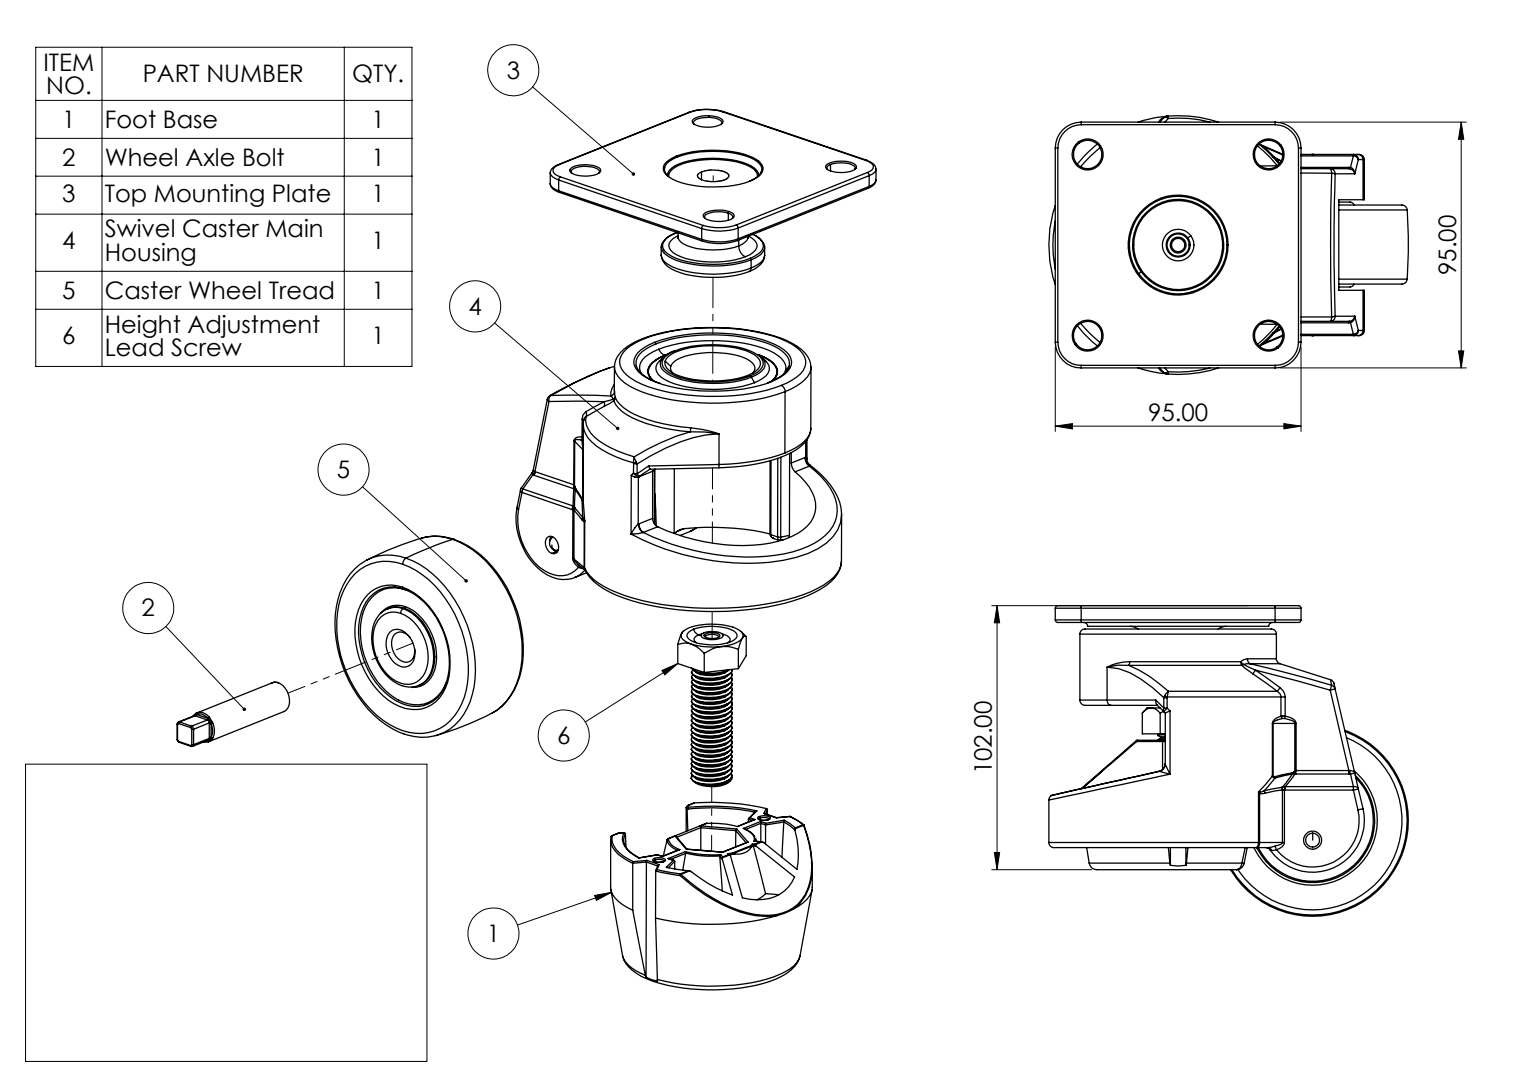
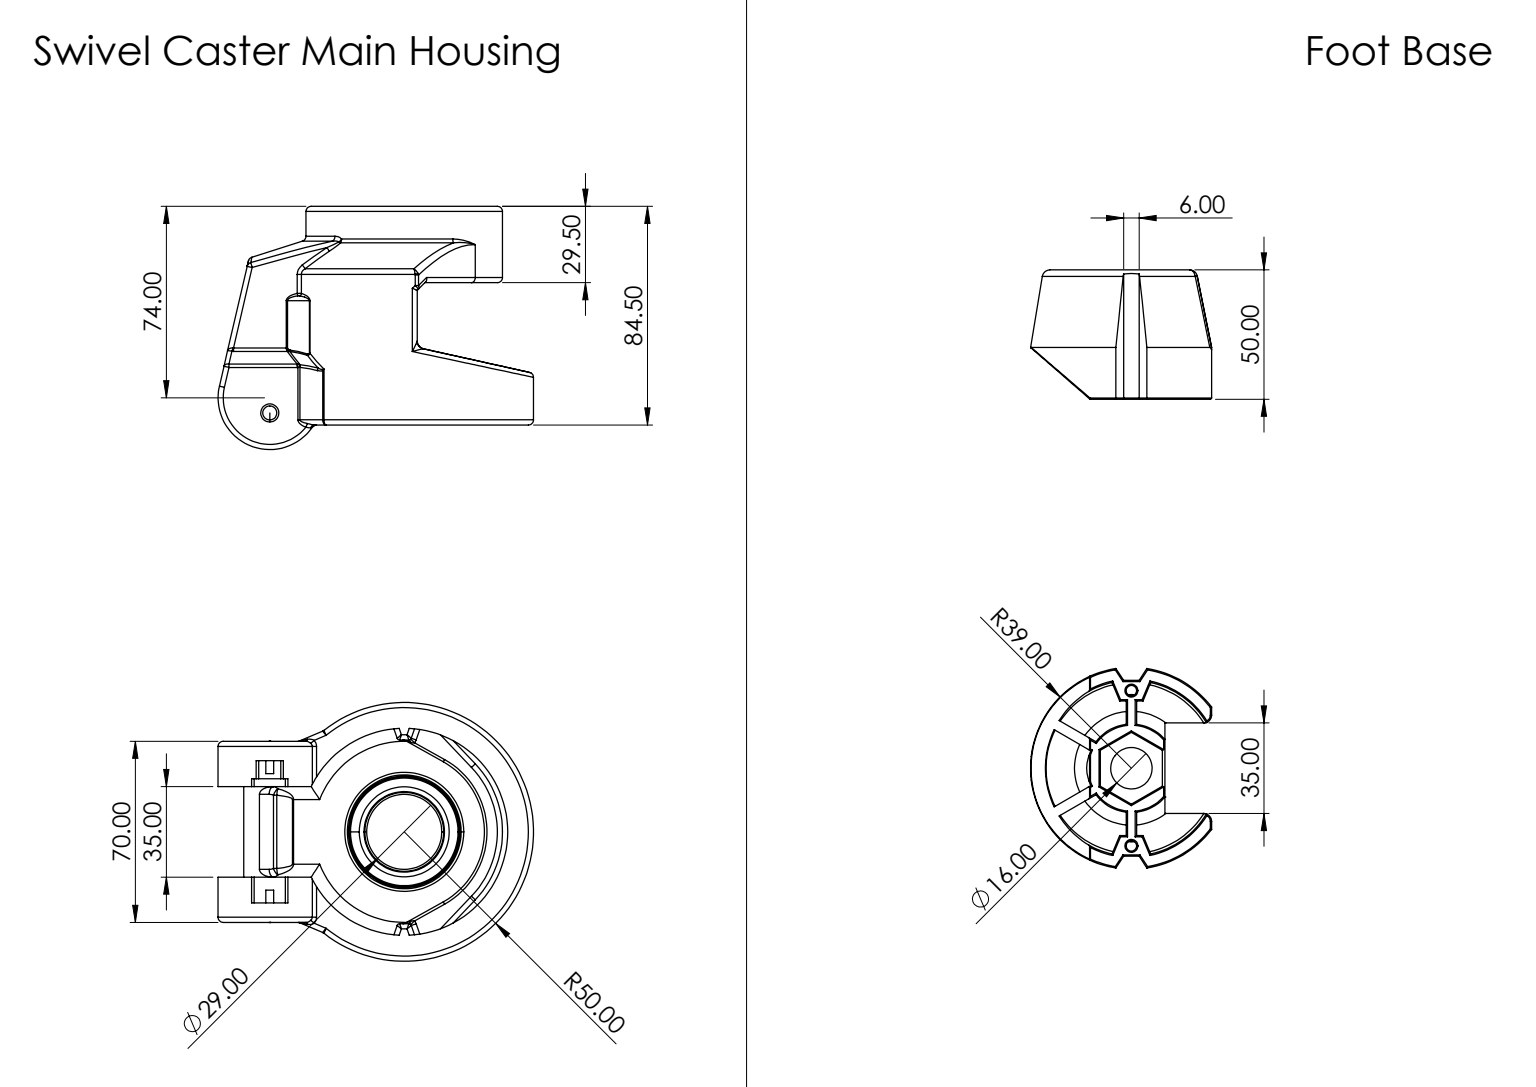
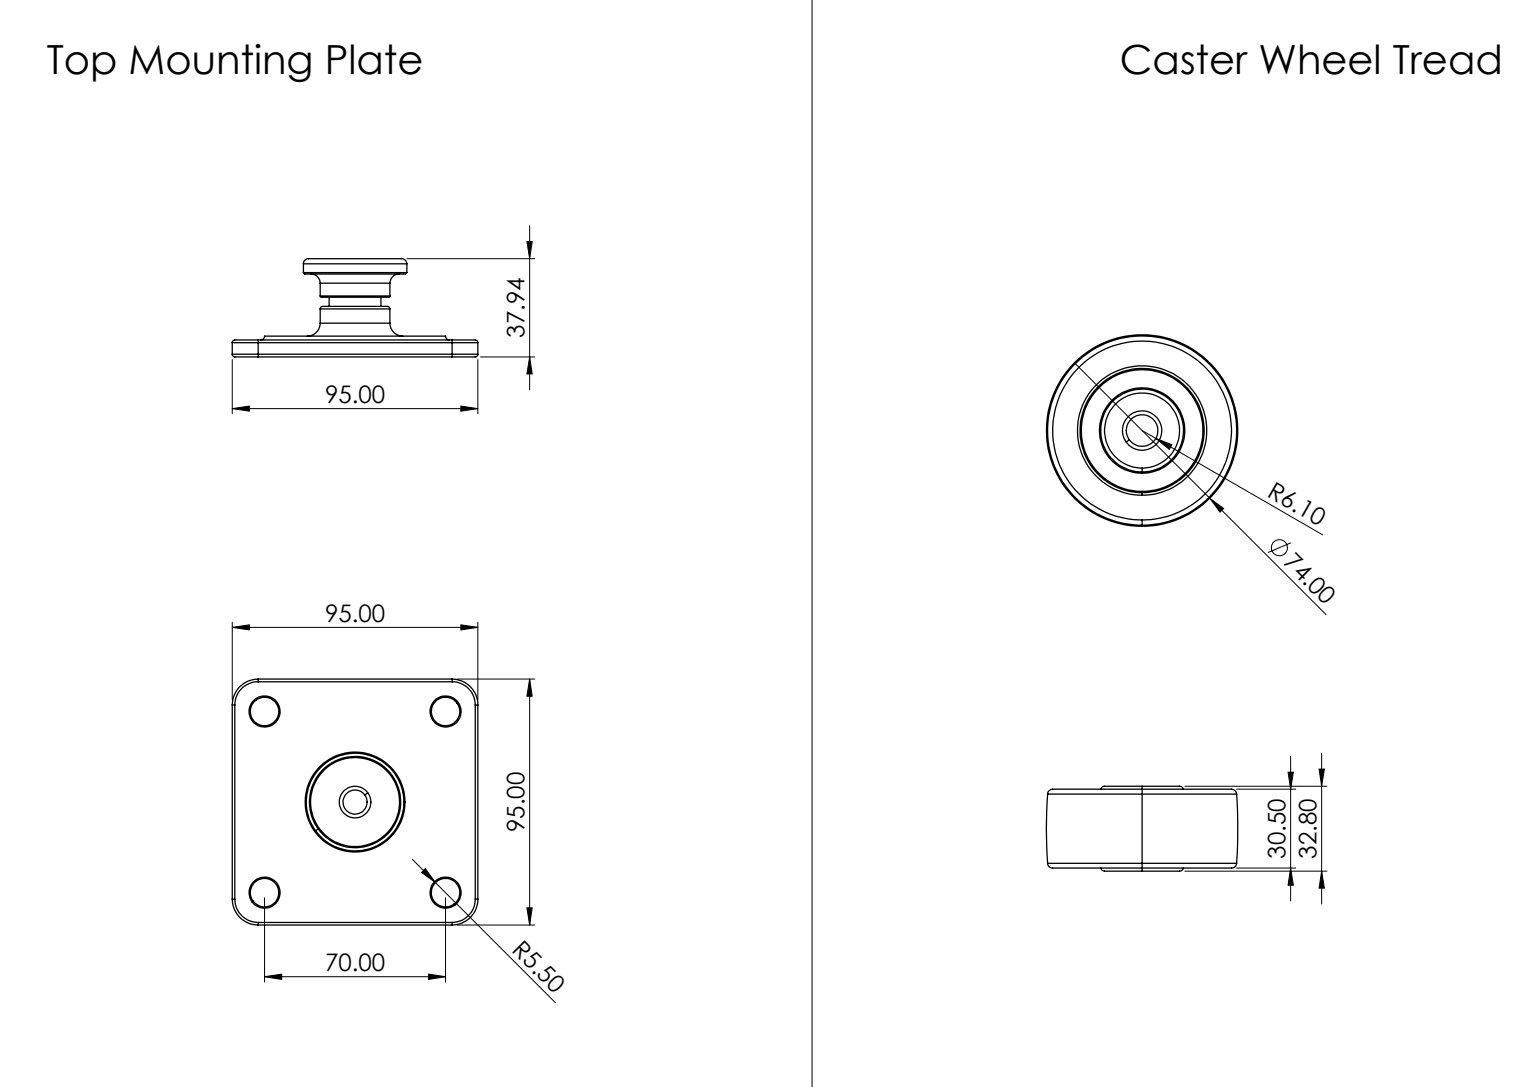
ISO-10303-21;
HEADER;
FILE_DESCRIPTION (('STEP AP214'),
    '1' );
FILE_NAME ('MAS-691',
    '2026-10-09T12:05:53',
    ( '' ),
    ( '' ),
    'SwSTEP 2.0',
    'SolidWorks 2026',
    '' );
FILE_SCHEMA (( 'AUTOMOTIVE_DESIGN' ));
ENDSEC;

DATA;
#1 = CARTESIAN_POINT ( 'NONE',  ( 24.04473007462266310, -15.61618926727986789, -75.50766188105974663 ) ) ;
#2 = CARTESIAN_POINT ( 'NONE',  ( 11.13393739769619906, -63.46281540124650178, -43.92385611378949761 ) ) ;
#3 = CARTESIAN_POINT ( 'NONE',  ( 70.83745409581372598, 17.98087126524719892, -68.79648330188406646 ) ) ;
#4 = ORIENTED_EDGE ( 'NONE', *, *, #7554, .T. ) ;
#5 = CARTESIAN_POINT ( 'NONE',  ( 23.57448381426064188, -48.85252042381474524, -34.86893418027932512 ) ) ;
#6 = CARTESIAN_POINT ( 'NONE',  ( 56.87954270074080654, 19.13328173822429790, -52.82794281668999758 ) ) ;
#7 = DIRECTION ( 'NONE',  ( 0.6933752452815363787, 0.7071067811865472397, -0.1386750490563077587 ) ) ;
#8 = CYLINDRICAL_SURFACE ( 'NONE', #48063, 2.000000000000000000 ) ;
#9 = ORIENTED_EDGE ( 'NONE', *, *, #6010, .T. ) ;
#10 = DIRECTION ( 'NONE',  ( 0.5516667872527539762, 0.8340645993220338061, 0.000000000000000000 ) ) ;
#11 = LINE ( 'NONE', #18878, #28379 ) ;
#12 = CARTESIAN_POINT ( 'NONE',  ( 9.221498779823216196, -11.63191302842313313, -56.67433499279778175 ) ) ;
#13 = CARTESIAN_POINT ( 'NONE',  ( 2.422196078461449797, -25.82482932757800143, -35.02873218748179340 ) ) ;
#14 = EDGE_CURVE ( 'NONE', #41828, #44695, #32317, .T. ) ;
#15 = CARTESIAN_POINT ( 'NONE',  ( 20.62196618598149911, -8.699519395578539260, -73.47554475576539801 ) ) ;
#16 = CYLINDRICAL_SURFACE ( 'NONE', #33863, 6.766999999999998572 ) ;
#17 = CARTESIAN_POINT ( 'NONE',  ( 46.35510799002431526, -38.18910727465775068, -58.54413787839046535 ) ) ;
#18 = SHAPE_DEFINITION_REPRESENTATION ( #45804, #4374 ) ;
#19 = VERTEX_POINT ( 'NONE', #48082 ) ;
#20 = CIRCLE ( 'NONE', #41004, 2.999999999999999112 ) ;
#21 = CIRCLE ( 'NONE', #50217, 3.400000000022779911 ) ;
#22 = CARTESIAN_POINT ( 'NONE',  ( 9.962852259819479528, -19.79044361182920042, -65.04335028194189761 ) ) ;
#23 = AXIS2_PLACEMENT_3D ( 'NONE', #28907, #44909, #49375 ) ;
#24 = CARTESIAN_POINT ( 'NONE',  ( 0.03808610503982521461, -8.381889819517736484, -34.73334895013598356 ) ) ;
#25 = CIRCLE ( 'NONE', #830, 16.00000000000000000 ) ;
#26 = CARTESIAN_POINT ( 'NONE',  ( 9.625247127302518635, -19.52582424083449908, -32.14999999999999858 ) ) ;
#27 = CARTESIAN_POINT ( 'NONE',  ( 47.24444964797500290, 23.22446773931700292, -75.11580175282739447 ) ) ;
#28 = DIRECTION ( 'NONE',  ( 0.000000000000000000, 0.000000000000000000, 1.000000000000000000 ) ) ;
#29 = CARTESIAN_POINT ( 'NONE',  ( 58.45382029077139663, 15.48193787282010092, -47.52511337483110054 ) ) ;
#30 = CARTESIAN_POINT ( 'NONE',  ( 12.20485434016749871, 33.73368687413830003, -16.27613458663830315 ) ) ;
#31 = CARTESIAN_POINT ( 'NONE',  ( 11.75558472888330108, -8.629576846066969509, -76.82947711988130379 ) ) ;
#33 = CARTESIAN_POINT ( 'NONE',  ( 11.13393739769619906, -55.30245861064819479, -43.74348518090240390 ) ) ;
#32 = DIRECTION ( 'NONE',  ( 0.05023550054956202326, 0.000000000000000000, 0.9987374001630934250 ) ) ;
#34 = CARTESIAN_POINT ( 'NONE',  ( 63.30967889250540992, 1.328674444234379859, -68.76626720283900340 ) ) ;
#35 = CARTESIAN_POINT ( 'NONE',  ( 61.45197839950609620, 13.95077426323470071, -46.74199412580669843 ) ) ;
#36 = DIRECTION ( 'NONE',  ( 0.5877852522924696954, 0.8090169943749498938, 0.000000000000000000 ) ) ;
#37 = DIRECTION ( 'NONE',  ( 0.000000000000000000, -0.7071067811865292541, 0.7071067811865656694 ) ) ;
#38 = AXIS2_PLACEMENT_3D ( 'NONE', #21905, #42103, #29767 ) ;
#39 = VERTEX_POINT ( 'NONE', #5102 ) ;
#40 = CARTESIAN_POINT ( 'NONE',  ( 52.81826494772970193, -49.66694110389089900, -48.49938242813500011 ) ) ;
#41 = CARTESIAN_POINT ( 'NONE',  ( 61.28932554653079734, -45.22069038368779559, -27.95515929525059917 ) ) ;
#42 = CARTESIAN_POINT ( 'NONE',  ( 20.99557441488136078, -21.94238693200700041, -72.08401915777523072 ) ) ;
#43 = CARTESIAN_POINT ( 'NONE',  ( 61.24946240356100446, 14.29281268270219840, -47.58806468664730005 ) ) ;
#44 = CARTESIAN_POINT ( 'NONE',  ( 22.19687809394159927, -11.28635708649630054, -78.03525497637551211 ) ) ;
#45 = CARTESIAN_POINT ( 'NONE',  ( 51.50850403090049667, 17.46583278780749993, -76.79363216376158618 ) ) ;
#46 = CARTESIAN_POINT ( 'NONE',  ( 53.43953639093020058, 18.12785922017320317, -48.94167477993919846 ) ) ;
#47 = CARTESIAN_POINT ( 'NONE',  ( 71.33582579397329937, 0.9940695285616559795, -70.71491496446259362 ) ) ;
#48 = CARTESIAN_POINT ( 'NONE',  ( -0.2431464996536397138, -45.41879842705380810, -34.97812159119441588 ) ) ;
#49 = EDGE_CURVE ( 'NONE', #3712, #26115, #46078, .T. ) ;
#50 = ORIENTED_EDGE ( 'NONE', *, *, #39346, .T. ) ;
#51 = CYLINDRICAL_SURFACE ( 'NONE', #25451, 0.9999999999999988898 ) ;
#52 = AXIS2_PLACEMENT_3D ( 'NONE', #15855, #20801, #24196 ) ;
#53 = CARTESIAN_POINT ( 'NONE',  ( 47.61264694707350031, -54.54714935536990339, -55.11842961798419793 ) ) ;
#54 = CARTESIAN_POINT ( 'NONE',  ( 22.50468263344456687, -12.72456034819510151, -68.71118389017816241 ) ) ;
#55 = CONICAL_SURFACE ( 'NONE', #5063, 44.00000000000000000, 0.8066715494215099813 ) ;
#56 = CARTESIAN_POINT ( 'NONE',  ( 10.72262792443331492, -19.77487285394900951, -71.24448753608163543 ) ) ;
#57 = CARTESIAN_POINT ( 'NONE',  ( 60.90067199252950303, -29.96820827507399798, -16.03697021813930235 ) ) ;
#58 = CARTESIAN_POINT ( 'NONE',  ( 71.48394854028050815, 1.096932441169200079, -60.71856768636379797 ) ) ;
#59 = CARTESIAN_POINT ( 'NONE',  ( 14.28038030992539476, 1.245406012443915467, -34.79644291222909658 ) ) ;
#60 = CARTESIAN_POINT ( 'NONE',  ( 72.18036885542301206, 1.274155933524790063, -61.30553710256390332 ) ) ;
#61 = AXIS2_PLACEMENT_3D ( 'NONE', #5299, #13423, #12639 ) ;
#62 = AXIS2_PLACEMENT_3D ( 'NONE', #47458, #35380, #23303 ) ;
#63 = CARTESIAN_POINT ( 'NONE',  ( 22.90087412606865058, -16.66897304226082710, -40.89671642115739303 ) ) ;
#64 = DIRECTION ( 'NONE',  ( 0.8933039976646619529, 0.3805134419105545285, 0.2392017731575520056 ) ) ;
#65 = ORIENTED_EDGE ( 'NONE', *, *, #51526, .T. ) ;
#66 = ORIENTED_EDGE ( 'NONE', *, *, #10007, .T. ) ;
#67 = LINE ( 'NONE', #19711, #13704 ) ;
#68 = CARTESIAN_POINT ( 'NONE',  ( 22.04686178097117732, -19.02415631444728561, -58.61948664697574429 ) ) ;
#69 = ORIENTED_EDGE ( 'NONE', *, *, #51815, .T. ) ;
#70 = CARTESIAN_POINT ( 'NONE',  ( 14.06316349757885042, -7.911113466102105640, -58.92429889998866344 ) ) ;
#71 = CARTESIAN_POINT ( 'NONE',  ( 55.90694558577502704, 19.65285642343416939, -74.84539568267780396 ) ) ;
#72 = ORIENTED_EDGE ( 'NONE', *, *, #36227, .F. ) ;
#73 = CARTESIAN_POINT ( 'NONE',  ( 11.04126890615173195, 33.67834000696034735, -23.14699238744169563 ) ) ;
#74 = CARTESIAN_POINT ( 'NONE',  ( 42.22422596689015251, 6.426959746402536311, -79.19854329468917342 ) ) ;
#75 = CARTESIAN_POINT ( 'NONE',  ( 23.84711268294356046, -17.41670964262949894, -65.58063247732249579 ) ) ;
#76 = EDGE_CURVE ( 'NONE', #45466, #37955, #44145, .T. ) ;
#77 = CARTESIAN_POINT ( 'NONE',  ( 21.74894416331870062, -9.578439440273777805, -43.53078881371720144 ) ) ;
#78 = CARTESIAN_POINT ( 'NONE',  ( 45.17641135619509640, 2.139553668185640412, -34.89907071124209637 ) ) ;
#79 = CARTESIAN_POINT ( 'NONE',  ( 53.63393739769619373, -53.11618894467930119, 16.35000000000000142 ) ) ;
#80 = EDGE_CURVE ( 'NONE', #28603, #19573, #33103, .T. ) ;
#81 = CARTESIAN_POINT ( 'NONE',  ( 63.96520777976849814, -30.70443757047150157, -16.53667252483340278 ) ) ;
#82 = CARTESIAN_POINT ( 'NONE',  ( 9.221484299827681141, -19.60044010530257097, -42.62566474563559638 ) ) ;
#83 = CARTESIAN_POINT ( 'NONE',  ( 9.878977750625089982, -11.56869915257929904, -35.41547006414829468 ) ) ;
#84 = CARTESIAN_POINT ( 'NONE',  ( 41.93136269540350014, 14.16859103147459997, -6.436551634680689915 ) ) ;
#85 = CARTESIAN_POINT ( 'NONE',  ( 15.05440318628110141, 21.88381105532300097, -76.14999999999999147 ) ) ;
#86 = AXIS2_PLACEMENT_3D ( 'NONE', #46178, #31434, #24593 ) ;
#87 = AXIS2_PLACEMENT_3D ( 'NONE', #9634, #13072, #16715 ) ;
#88 = CARTESIAN_POINT ( 'NONE',  ( 83.58549413295790487, -44.91149346033729728, -47.23752224019400359 ) ) ;
#89 = CARTESIAN_POINT ( 'NONE',  ( 9.633937397696209715, -15.61618894467929941, -22.64999999999999858 ) ) ;
#90 = AXIS2_PLACEMENT_3D ( 'NONE', #30342, #50541, #46365 ) ;
#91 = CARTESIAN_POINT ( 'NONE',  ( 8.278517517462621100, -18.12120375785029935, -46.40940759145149741 ) ) ;
#92 = ORIENTED_EDGE ( 'NONE', *, *, #43426, .F. ) ;
#93 = CARTESIAN_POINT ( 'NONE',  ( 54.39552376178149018, -47.99669817431590246, -26.49407277081109768 ) ) ;
#94 = CARTESIAN_POINT ( 'NONE',  ( 13.75381683890189954, -50.28652857585829850, -20.97887788433540024 ) ) ;
#95 = CARTESIAN_POINT ( 'NONE',  ( 19.30039974071021902, -22.89444622034352861, -39.87698757616706757 ) ) ;
#96 = CARTESIAN_POINT ( 'NONE',  ( 63.43393739769620510, 1.883811055320669947, -62.44999999999999574 ) ) ;
#97 = CARTESIAN_POINT ( 'NONE',  ( 22.90093739844393284, -15.61845303799943174, -56.45293168557734020 ) ) ;
#98 = DIRECTION ( 'NONE',  ( 1.681650659181820092E-11, -1.000000000000000000, -2.220771714818679968E-11 ) ) ;
#99 = ORIENTED_EDGE ( 'NONE', *, *, #38277, .T. ) ;
#100 = CARTESIAN_POINT ( 'NONE',  ( -8.352063028131979650, -44.76125978986279819, -5.675626772346689997 ) ) ;
#101 = CARTESIAN_POINT ( 'NONE',  ( 18.20467283260814639, -23.32127324669528434, -38.20900000048465017 ) ) ;
#102 = CARTESIAN_POINT ( 'NONE',  ( 52.13393739769618662, -30.49118894467929763, -65.65000000000000568 ) ) ;
#103 = CARTESIAN_POINT ( 'NONE',  ( 63.10556452593170462, 0.9234936569010840923, -62.37649816534809588 ) ) ;
#104 = CARTESIAN_POINT ( 'NONE',  ( 57.49560449525049677, -50.20980267308190292, -52.71571619239969664 ) ) ;
#105 = CARTESIAN_POINT ( 'NONE',  ( 41.47267182510199746, 13.45740503867699900, -5.287754110957130216 ) ) ;
#106 = CARTESIAN_POINT ( 'NONE',  ( 22.72481333909230017, -17.38742284364922597, -64.53615558299642885 ) ) ;
#107 = DIRECTION ( 'NONE',  ( 0.000000000000000000, 0.000000000000000000, 1.000000000000000000 ) ) ;
#108 = CARTESIAN_POINT ( 'NONE',  ( 53.43679795856239423, -49.34287432940249829, -48.83615822498679648 ) ) ;
#109 = CARTESIAN_POINT ( 'NONE',  ( 9.221334957865163773, -11.63219308205320957, -74.95902792597172493 ) ) ;
#110 = EDGE_CURVE ( 'NONE', #14338, #30215, #34341, .T. ) ;
#111 = CARTESIAN_POINT ( 'NONE',  ( 12.72590726626352975, -21.52907858405782449, -63.11948344771946040 ) ) ;
#112 = CARTESIAN_POINT ( 'NONE',  ( 17.46250221217660226, -52.82751997460400162, -76.12812327221449493 ) ) ;
#113 = LINE ( 'NONE', #8225, #22864 ) ;
#114 = CARTESIAN_POINT ( 'NONE',  ( 63.48718924516480655, 1.369286338574360107, -62.31365646596000119 ) ) ;
#115 = ORIENTED_EDGE ( 'NONE', *, *, #5512, .F. ) ;
#116 = DIRECTION ( 'NONE',  ( -0.2846079131720438693, 0.9586440088791325920, 0.000000000000000000 ) ) ;
#117 = DIRECTION ( 'NONE',  ( 0.000000000000000000, 0.000000000000000000, 1.000000000000000000 ) ) ;
#118 = CARTESIAN_POINT ( 'NONE',  ( 11.66207609259309841, -9.394545466821320190, -81.23899999999999011 ) ) ;
#119 = ORIENTED_EDGE ( 'NONE', *, *, #5990, .F. ) ;
#120 = CARTESIAN_POINT ( 'NONE',  ( 17.35323444535940141, 21.52412519331699770, -76.12563501418100032 ) ) ;
#121 = VERTEX_POINT ( 'NONE', #9296 ) ;
#122 = ORIENTED_EDGE ( 'NONE', *, *, #30558, .T. ) ;
#123 = CARTESIAN_POINT ( 'NONE',  ( 41.13393739769620083, -15.61618894467929941, -76.14999999999999147 ) ) ;
#124 = CARTESIAN_POINT ( 'NONE',  ( 23.50285504017600147, -13.84387210050659966, -81.23899999999999011 ) ) ;
#125 = AXIS2_PLACEMENT_3D ( 'NONE', #16725, #32947, #12811 ) ;
#126 = CARTESIAN_POINT ( 'NONE',  ( 61.67728155832050163, 13.96021777555640142, -46.92123163896760474 ) ) ;
#127 = ORIENTED_EDGE ( 'NONE', *, *, #25238, .T. ) ;
#128 = CARTESIAN_POINT ( 'NONE',  ( 13.00893747662790112, -65.51843693869379592, -23.32157303180050079 ) ) ;
#129 = ORIENTED_EDGE ( 'NONE', *, *, #8832, .T. ) ;
#130 = CARTESIAN_POINT ( 'NONE',  ( 11.13393741218609989, -63.52234717531779751, -24.14942545402350049 ) ) ;
#131 = EDGE_CURVE ( 'NONE', #41228, #12484, #43567, .T. ) ;
#132 = DIRECTION ( 'NONE',  ( 0.000000000000000000, 0.000000000000000000, -1.000000000000000000 ) ) ;
#133 = ORIENTED_EDGE ( 'NONE', *, *, #22274, .F. ) ;
#134 = ORIENTED_EDGE ( 'NONE', *, *, #16581, .T. ) ;
#135 = CARTESIAN_POINT ( 'NONE',  ( 68.13393739769630031, 16.88381105532069881, -71.50000000000000000 ) ) ;
#136 = CARTESIAN_POINT ( 'NONE',  ( 60.78215478534439598, 14.37029503885610104, -47.53399852477849663 ) ) ;
#137 = CARTESIAN_POINT ( 'NONE',  ( 22.18886536826886768, -12.48613193644987263, -40.30080353194567522 ) ) ;
#138 = CARTESIAN_POINT ( 'NONE',  ( 41.55663456559440050, -43.85962873145390262, -3.466044033466880059 ) ) ;
#139 = CARTESIAN_POINT ( 'NONE',  ( -7.981053360220990101, 13.77072044879260027, -5.285160133845220543 ) ) ;
#140 = DIRECTION ( 'NONE',  ( 0.000000000000000000, -1.000000000000000000, 0.000000000000000000 ) ) ;
#141 = DIRECTION ( 'NONE',  ( -1.000000000000000000, -1.007258792502662152E-15, 0.000000000000000000 ) ) ;
#142 = CARTESIAN_POINT ( 'NONE',  ( 23.87684719361660157, -16.89450661858629843, -59.33958724536129381 ) ) ;
#143 = EDGE_LOOP ( 'NONE', ( #42632, #34972, #31733, #32112, #15786, #3340, #43438, #7469 ) ) ;
#144 = CARTESIAN_POINT ( 'NONE',  ( 16.13393739769620083, -15.61618894467929941, -8.050000000000000711 ) ) ;
#145 = CARTESIAN_POINT ( 'NONE',  ( 41.69946260611190070, 14.48490530928729925, -6.580410751903029265 ) ) ;
#146 = CARTESIAN_POINT ( 'NONE',  ( 11.25398292734820060, 32.98847748127889901, -44.13762314110879714 ) ) ;
#147 = CARTESIAN_POINT ( 'NONE',  ( 72.11830705158430987, 1.407740700961940039, -69.90489258341499124 ) ) ;
#148 = CARTESIAN_POINT ( 'NONE',  ( 42.65284985753929448, -39.83221199758776976, -73.17816600590020926 ) ) ;
#149 = AXIS2_PLACEMENT_3D ( 'NONE', #32880, #41030, #5146 ) ;
#150 = AXIS2_PLACEMENT_3D ( 'NONE', #7482, #19780, #50726 ) ;
#151 = DIRECTION ( 'NONE',  ( 0.4646601886423053496, 0.000000000000000000, 0.8854890790353641128 ) ) ;
#152 = CIRCLE ( 'NONE', #47026, 15.56227766016840164 ) ;
#153 = CARTESIAN_POINT ( 'NONE',  ( 13.08915387332580060, 18.89706364897919855, -21.07935023198889724 ) ) ;
#154 = CARTESIAN_POINT ( 'NONE',  ( 47.08254214957229777, 23.29430871593149632, -75.17655545168919673 ) ) ;
#155 = CARTESIAN_POINT ( 'NONE',  ( 48.68907877926229588, -53.99330233976530025, -54.71376368574509996 ) ) ;
#156 = CARTESIAN_POINT ( 'NONE',  ( 51.77632594796870080, -32.59667852913690922, -18.40929238398544854 ) ) ;
#157 = EDGE_CURVE ( 'NONE', #32127, #27118, #5412, .T. ) ;
#158 = DIRECTION ( 'NONE',  ( -9.834501533011740460E-16, -2.054487543405499690E-16, -1.000000000000000000 ) ) ;
#159 = CARTESIAN_POINT ( 'NONE',  ( -14.41646913324137458, -47.38337005707102634, 16.85000000000000142 ) ) ;
#160 = CARTESIAN_POINT ( 'NONE',  ( 20.11809687624943521, -22.52869528883066153, -54.12566693902919468 ) ) ;
#161 = ORIENTED_EDGE ( 'NONE', *, *, #48216, .F. ) ;
#162 = CARTESIAN_POINT ( 'NONE',  ( 8.696784336233250201, -15.17409326420679960, -34.08624212660659936 ) ) ;
#163 = EDGE_CURVE ( 'NONE', #42293, #16351, #20947, .T. ) ;
#164 = CARTESIAN_POINT ( 'NONE',  ( 83.89200044194980421, -48.61618894467930119, -53.92796738110899923 ) ) ;
#165 = ORIENTED_EDGE ( 'NONE', *, *, #23269, .F. ) ;
#166 = CARTESIAN_POINT ( 'NONE',  ( 71.29447239804829906, 1.393731187554809958, -70.25064478522961053 ) ) ;
#167 = CARTESIAN_POINT ( 'NONE',  ( 60.57174147421439869, -45.61905813271650345, -47.32280480079099760 ) ) ;
#168 = CARTESIAN_POINT ( 'NONE',  ( 42.18478254462388577, 8.551920610105096188, -75.43933843070429646 ) ) ;
#169 = EDGE_CURVE ( 'NONE', #3359, #16152, #45412, .T. ) ;
#170 = CARTESIAN_POINT ( 'NONE',  ( 29.13393739769619728, 4.555383930574479656, -84.63196841427449613 ) ) ;
#171 = DIRECTION ( 'NONE',  ( 8.402539340422011355E-12, -1.000000000000000000, -1.365304166073849981E-11 ) ) ;
#172 = ORIENTED_EDGE ( 'NONE', *, *, #12898, .T. ) ;
#173 = CARTESIAN_POINT ( 'NONE',  ( 82.86439673227779679, -45.43596139653639909, -47.48719404937710209 ) ) ;
#174 = ORIENTED_EDGE ( 'NONE', *, *, #31789, .F. ) ;
#175 = ORIENTED_EDGE ( 'NONE', *, *, #21315, .T. ) ;
#176 = ORIENTED_EDGE ( 'NONE', *, *, #14775, .F. ) ;
#177 = LINE ( 'NONE', #11984, #16918 ) ;
#178 = CARTESIAN_POINT ( 'NONE',  ( 12.13393739769500357, -55.41568642894398522, -22.88367089793594999 ) ) ;
#179 = CARTESIAN_POINT ( 'NONE',  ( 76.39443566142985276, -13.50186642808351678, -12.77252636400736918 ) ) ;
#180 = CARTESIAN_POINT ( 'NONE',  ( 53.40601104668340326, -52.07939714610260040, -54.18165646226010068 ) ) ;
#181 = EDGE_LOOP ( 'NONE', ( #10169, #38470, #47423, #39238 ) ) ;
#182 = ORIENTED_EDGE ( 'NONE', *, *, #38895, .T. ) ;
#183 = CARTESIAN_POINT ( 'NONE',  ( 18.20454837585587526, -23.32130853119455693, -55.92427167932272170 ) ) ;
#184 = CARTESIAN_POINT ( 'NONE',  ( 57.10566319413430136, -45.15673104066610222, -25.30628267469290194 ) ) ;
#185 = CARTESIAN_POINT ( 'NONE',  ( 56.36581729833090293, -50.64752597117900024, -53.07181749496119494 ) ) ;
#186 = DIRECTION ( 'NONE',  ( 0.000000000000000000, 1.000000000000000000, 0.000000000000000000 ) ) ;
#187 = CARTESIAN_POINT ( 'NONE',  ( 58.91901068275170417, -2.751350989218700249, -15.64940685286009980 ) ) ;
#188 = EDGE_CURVE ( 'NONE', #6898, #18473, #14502, .T. ) ;
#189 = CARTESIAN_POINT ( 'NONE',  ( 9.367050196127319595, -15.61601677469269944, -55.84717978380999881 ) ) ;
#190 = AXIS2_PLACEMENT_3D ( 'NONE', #21830, #26535, #49643 ) ;
#191 = ORIENTED_EDGE ( 'NONE', *, *, #12053, .T. ) ;
#192 = CARTESIAN_POINT ( 'NONE',  ( 64.43393739769619799, 11.38381105532079829, -62.44999999999999574 ) ) ;
#194 = CARTESIAN_POINT ( 'NONE',  ( 53.11717557676140444, -50.37380613066250135, -77.21703359256949284 ) ) ;
#193 = AXIS2_PLACEMENT_3D ( 'NONE', #44707, #32884, #28448 ) ;
#195 = CARTESIAN_POINT ( 'NONE',  ( 60.26025110216912850, 14.55536647234954906, -47.43140372362420010 ) ) ;
#196 = CARTESIAN_POINT ( 'NONE',  ( 12.16981617636240109, -50.04926268091029584, -21.14999999999999858 ) ) ;
#197 = CARTESIAN_POINT ( 'NONE',  ( 18.24071347613679706, -23.17583458100989802, -56.42598068654729104 ) ) ;
#198 = CARTESIAN_POINT ( 'NONE',  ( 13.05744206701320209, -50.32199602849929931, -21.18087822640150364 ) ) ;
#199 = CARTESIAN_POINT ( 'NONE',  ( 18.48744068327825829, -51.29015062620795362, -15.70679445625363257 ) ) ;
#200 = CARTESIAN_POINT ( 'NONE',  ( 10.91611746120075743, -65.09563545678379626, -18.17421237897874065 ) ) ;
#201 = CARTESIAN_POINT ( 'NONE',  ( 61.22433221214529908, -45.66722181782489542, -47.75777089857670177 ) ) ;
#202 = CARTESIAN_POINT ( 'NONE',  ( 68.13393739769618662, -1.166188944679350081, -90.65000000000000568 ) ) ;
#203 = EDGE_CURVE ( 'NONE', #41459, #2348, #29936, .T. ) ;
#204 = CARTESIAN_POINT ( 'NONE',  ( 12.63580666350229897, -21.74037383255939915, -53.51237412773319591 ) ) ;
#205 = ORIENTED_EDGE ( 'NONE', *, *, #35909, .F. ) ;
#206 = CARTESIAN_POINT ( 'NONE',  ( 14.27557618103930004, -51.11617952483079108, -74.35192203308750436 ) ) ;
#207 = CARTESIAN_POINT ( 'NONE',  ( 47.38398407523909839, -54.66303005604620324, -54.71474001952109489 ) ) ;
#208 = DIRECTION ( 'NONE',  ( 1.000000000000000000, 0.000000000000000000, 0.000000000000000000 ) ) ;
#209 = CARTESIAN_POINT ( 'NONE',  ( 9.807775352051226747, -10.75450683567505550, -36.71600244428209692 ) ) ;
#210 = CARTESIAN_POINT ( 'NONE',  ( 14.48969159609045931, -51.52597369351618539, -75.36997958377637019 ) ) ;
#211 = CARTESIAN_POINT ( 'NONE',  ( 24.04447781939626338, -15.52406317847051120, -55.50396621545129250 ) ) ;
#212 = CARTESIAN_POINT ( 'NONE',  ( 10.72251451727398397, -11.45765055134171284, -75.66113898378057456 ) ) ;
#213 = CARTESIAN_POINT ( 'NONE',  ( 14.63393739769620083, -23.61618894467940066, -35.14999999999999858 ) ) ;
#215 = CARTESIAN_POINT ( 'NONE',  ( 11.13393739769619906, 32.28996931002959769, -24.14942631645369886 ) ) ;
#214 = CARTESIAN_POINT ( 'NONE',  ( 0.5774960717374295616, -8.799493537124943643, -34.81767276520690757 ) ) ;
#216 = DIRECTION ( 'NONE',  ( 1.000000000000000000, 1.435277183835595142E-25, -2.812429781167509836E-09 ) ) ;
#217 = CARTESIAN_POINT ( 'NONE',  ( 48.63544209855220402, 22.87909972998859587, -55.27856191273439634 ) ) ;
#218 = VERTEX_POINT ( 'NONE', #20999 ) ;
#219 = AXIS2_PLACEMENT_3D ( 'NONE', #32252, #16823, #17087 ) ;
#220 = CARTESIAN_POINT ( 'NONE',  ( 53.03258586660929552, -49.57550701127339465, -48.98438927054080239 ) ) ;
#221 = VECTOR ( 'NONE', #20603, 1000.000000000000000 ) ;
#222 = ORIENTED_EDGE ( 'NONE', *, *, #47182, .T. ) ;
#223 = CARTESIAN_POINT ( 'NONE',  ( 45.74232523797041239, 6.648894618224240105, -61.55666661952047036 ) ) ;
#224 = LINE ( 'NONE', #43991, #1797 ) ;
#225 = CARTESIAN_POINT ( 'NONE',  ( 16.13393739769620083, -15.61618894467929941, -10.44999999999999929 ) ) ;
#227 = CARTESIAN_POINT ( 'NONE',  ( 55.09561028961779527, 15.74612775871969994, -25.81326377834329833 ) ) ;
#226 = CARTESIAN_POINT ( 'NONE',  ( 84.44784216359251161, 11.88381105532070059, -47.47585302082339354 ) ) ;
#228 = CARTESIAN_POINT ( 'NONE',  ( 18.41697451332290214, -22.28929168817850126, -66.84789180586540169 ) ) ;
#230 = EDGE_CURVE ( 'NONE', #16151, #14500, #48277, .T. ) ;
#229 = CARTESIAN_POINT ( 'NONE',  ( 52.88388581274700329, 18.44024018630440409, -49.00306432449180249 ) ) ;
#231 = CARTESIAN_POINT ( 'NONE',  ( 57.24436304063220149, -45.12772278369259737, -17.93020339716479938 ) ) ;
#232 = CARTESIAN_POINT ( 'NONE',  ( 15.82997274078853067, -51.11618894467930119, -21.91305730704813115 ) ) ;
#233 = ORIENTED_EDGE ( 'NONE', *, *, #50630, .F. ) ;
#234 = CARTESIAN_POINT ( 'NONE',  ( 15.51400525636760008, -23.43938728828090134, -43.81267675689189645 ) ) ;
#235 = VERTEX_POINT ( 'NONE', #24656 ) ;
#236 = CARTESIAN_POINT ( 'NONE',  ( 11.16919192711069897, -65.09379547448669712, -17.21576935268850050 ) ) ;
#237 = CARTESIAN_POINT ( 'NONE',  ( 12.92951305397479977, 34.28108550583429803, -47.71245015580439741 ) ) ;
#238 = DIRECTION ( 'NONE',  ( 0.000000000000000000, 1.000000000000000000, 0.000000000000000000 ) ) ;
#239 = CARTESIAN_POINT ( 'NONE',  ( 48.15382033460080180, -54.02300406733139937, -53.72956514560460306 ) ) ;
#240 = CARTESIAN_POINT ( 'NONE',  ( 8.799473741179280495, 31.95986279266500318, -46.67015979934819825 ) ) ;
#241 = CARTESIAN_POINT ( 'NONE',  ( -0.007164427059776000244, -10.48291004383190028, -34.77269723891829756 ) ) ;
#242 = EDGE_LOOP ( 'NONE', ( #21413, #44958, #1944, #11021, #47868 ) ) ;
#243 = CARTESIAN_POINT ( 'NONE',  ( 24.04493741881096014, -14.58063984321919015, -75.46599062978197026 ) ) ;
#244 = CARTESIAN_POINT ( 'NONE',  ( -18.86606260230360022, -50.61618894467959962, 17.35000000000000142 ) ) ;
#245 = AXIS2_PLACEMENT_3D ( 'NONE', #20946, #48226, #25130 ) ;
#246 = CARTESIAN_POINT ( 'NONE',  ( 70.83745409581388230, 17.98087126524299606, -74.20351669811765305 ) ) ;
#247 = ORIENTED_EDGE ( 'NONE', *, *, #26711, .F. ) ;
#248 = CARTESIAN_POINT ( 'NONE',  ( 24.04493739085331683, -15.62301657200399418, -43.79259974408412859 ) ) ;
#249 = CARTESIAN_POINT ( 'NONE',  ( 50.13210307247129549, -48.90653279581949420, -76.14999999999999147 ) ) ;
#250 = CARTESIAN_POINT ( 'NONE',  ( 22.88637251419359941, -11.47525136018554370, -49.33255534741104498 ) ) ;
#251 =( BOUNDED_CURVE ( )  B_SPLINE_CURVE ( 3, ( #35430, #43565, #7666, #27816 ),
 .UNSPECIFIED., .F., .T. ) 
 B_SPLINE_CURVE_WITH_KNOTS ( ( 4, 4 ),
 ( 2.356194490192377700, 3.141592653589793116 ),
 .UNSPECIFIED. ) 
 CURVE ( )  GEOMETRIC_REPRESENTATION_ITEM ( )  RATIONAL_B_SPLINE_CURVE ( ( 1.000000000000000000, 0.9492530216741954519, 0.9492530216741954519, 1.000000000000000000 ) ) 
 REPRESENTATION_ITEM ( '' )  );
#252 = ORIENTED_EDGE ( 'NONE', *, *, #43387, .T. ) ;
#253 = CARTESIAN_POINT ( 'NONE',  ( 23.83903514183533190, -17.68687693202930333, -35.59099905439017419 ) ) ;
#254 = LINE ( 'NONE', #44274, #11685 ) ;
#255 = DIRECTION ( 'NONE',  ( 0.000000000000000000, 0.000000000000000000, -1.000000000000000000 ) ) ;
#256 = CARTESIAN_POINT ( 'NONE',  ( 22.51916824768339609, -10.39972011525970075, -71.57429041023848981 ) ) ;
#257 = CARTESIAN_POINT ( 'NONE',  ( 10.37119768687602317, -55.19981235010300935, -21.14999999999890079 ) ) ;
#258 = DIRECTION ( 'NONE',  ( 0.000000000000000000, 0.000000000000000000, -1.000000000000000000 ) ) ;
#259 = SHAPE_DEFINITION_REPRESENTATION ( #50860, #49550 ) ;
#260 = VERTEX_POINT ( 'NONE', #568 ) ;
#261 = VECTOR ( 'NONE', #32679, 1000.000000000000000 ) ;
#262 = CARTESIAN_POINT ( 'NONE',  ( 13.95200227718980024, -8.492576593136959673, -69.63804828363188903 ) ) ;
#263 = AXIS2_PLACEMENT_3D ( 'NONE', #1040, #23378, #35460 ) ;
#264 = CARTESIAN_POINT ( 'NONE',  ( 52.69422391758440227, -49.76824816101610338, -48.79572285777990004 ) ) ;
#265 = EDGE_CURVE ( 'NONE', #15142, #11807, #37468, .T. ) ;
#266 = DIRECTION ( 'NONE',  ( 0.000000000000000000, -1.000000000000000000, 0.000000000000000000 ) ) ;
#267 = DIRECTION ( 'NONE',  ( -0.04332574401194498603, 0.02501412996813599451, 0.9987478026047158508 ) ) ;
#268 = EDGE_CURVE ( 'NONE', #31144, #33328, #44340, .T. ) ;
#269 = CARTESIAN_POINT ( 'NONE',  ( 47.30322462833210295, 23.47865774688779794, -74.36100594765079563 ) ) ;
#270 = CARTESIAN_POINT ( 'NONE',  ( 71.19761362482960010, 1.388189907116970101, -61.01613942410280345 ) ) ;
#271 = EDGE_CURVE ( 'NONE', #20377, #35517, #9367, .T. ) ;
#272 = CARTESIAN_POINT ( 'NONE',  ( 59.65718820948480783, 14.85145970413650041, -47.32570903220330649 ) ) ;
#273 = CARTESIAN_POINT ( 'NONE',  ( 12.23212070002750096, 33.47637228114889751, -15.94047990888659783 ) ) ;
#274 = CARTESIAN_POINT ( 'NONE',  ( 23.75374426366189695, -12.46638513581170038, -69.38289759990109928 ) ) ;
#275 = AXIS2_PLACEMENT_3D ( 'NONE', #225, #8098, #24041 ) ;
#276 = CARTESIAN_POINT ( 'NONE',  ( 54.17120420068020081, -50.61618894747770270, -77.01278694698871163 ) ) ;
#278 = DIRECTION ( 'NONE',  ( 0.000000000000000000, 0.000000000000000000, -1.000000000000000000 ) ) ;
#277 = CARTESIAN_POINT ( 'NONE',  ( 16.13393739769620083, -15.61618894467929941, -28.45282021618999835 ) ) ;
#279 = CARTESIAN_POINT ( 'NONE',  ( 63.07039345372018602, 1.099973129953850215, -68.78515728267289830 ) ) ;
#280 = CARTESIAN_POINT ( 'NONE',  ( 61.31292087637410049, 14.04174110780009954, -47.04181882197700304 ) ) ;
#281 = CARTESIAN_POINT ( 'NONE',  ( 12.14986981628316620, -8.703629658544938863, -78.84100245546133579 ) ) ;
#282 = CARTESIAN_POINT ( 'NONE',  ( 2.558369240368460140, -6.046280207075140467, -34.64999999999999858 ) ) ;
#283 = ORIENTED_EDGE ( 'NONE', *, *, #13602, .F. ) ;
#284 = CARTESIAN_POINT ( 'NONE',  ( 52.85589391196879916, -49.64722623523429945, -48.63421165633150167 ) ) ;
#285 = CARTESIAN_POINT ( 'NONE',  ( 61.33763625571969413, -45.19708596712810333, -27.94521875216469908 ) ) ;
#286 = DIRECTION ( 'NONE',  ( 1.000000000000000000, 0.000000000000000000, -1.224646799147353207E-16 ) ) ;
#287 = CARTESIAN_POINT ( 'NONE',  ( 56.26879455738869495, 14.75277753040210094, -26.06397138246319756 ) ) ;
#288 = CARTESIAN_POINT ( 'NONE',  ( 10.21452801543910027, -20.14026745531459994, -75.02493559595789918 ) ) ;
#289 = CARTESIAN_POINT ( 'NONE',  ( 50.28917926387119763, 18.40713679194410091, -76.14999999999999147 ) ) ;
#291 = EDGE_CURVE ( 'NONE', #43185, #32513, #25957, .T. ) ;
#290 = CARTESIAN_POINT ( 'NONE',  ( 52.72266114154869854, 18.49315592538880182, -48.47378032971769812 ) ) ;
#292 = CARTESIAN_POINT ( 'NONE',  ( 71.23944111523938716, 1.270877794983130027, -70.57718306158270138 ) ) ;
#293 = CARTESIAN_POINT ( 'NONE',  ( 16.13393739769620083, -15.61618894467929941, -34.64999999999999858 ) ) ;
#294 = ORIENTED_EDGE ( 'NONE', *, *, #6376, .T. ) ;
#295 = AXIS2_PLACEMENT_3D ( 'NONE', #26378, #18789, #37943 ) ;
#296 = DIRECTION ( 'NONE',  ( 0.000000000000000000, 0.000000000000000000, 1.000000000000000000 ) ) ;
#297 = AXIS2_PLACEMENT_3D ( 'NONE', #33472, #4412, #32417 ) ;
#298 = CARTESIAN_POINT ( 'NONE',  ( 47.55572014686639903, -54.56393835125380321, -54.83404589176390687 ) ) ;
#299 = CARTESIAN_POINT ( 'NONE',  ( 0.4047412638265869833, -22.38804348994680282, -35.14999999999999858 ) ) ;
#300 = CARTESIAN_POINT ( 'NONE',  ( 33.83393739769619657, -15.61618894467939711, -6.649999999999999467 ) ) ;
#301 = CARTESIAN_POINT ( 'NONE',  ( 59.27112701105020420, 16.84091543466239926, -50.37593205019099685 ) ) ;
#302 = CARTESIAN_POINT ( 'NONE',  ( 71.36299175555980412, 1.264791438333819906, -60.78603624114159487 ) ) ;
#303 = CYLINDRICAL_SURFACE ( 'NONE', #11626, 0.9999999999999988898 ) ;
#304 = AXIS2_PLACEMENT_3D ( 'NONE', #29304, #41620, #1792 ) ;
#305 = CARTESIAN_POINT ( 'NONE',  ( 72.21022460378770802, 1.195685806282509978, -61.28382422308500566 ) ) ;
#306 = LINE ( 'NONE', #33028, #47756 ) ;
#307 = CARTESIAN_POINT ( 'NONE',  ( 64.99878011502339348, 1.099973129953850215, -70.71354394397609155 ) ) ;
#308 = ORIENTED_EDGE ( 'NONE', *, *, #24146, .F. ) ;
#309 = VERTEX_POINT ( 'NONE', #6067 ) ;
#310 = DIRECTION ( 'NONE',  ( 1.224645063448482957E-16, 1.000000000000000000, -1.376914871200490233E-11 ) ) ;
#311 = CARTESIAN_POINT ( 'NONE',  ( 22.90093739248998972, -16.50198092149558349, -58.49448661159359375 ) ) ;
#312 = ORIENTED_EDGE ( 'NONE', *, *, #15491, .T. ) ;
#313 = CARTESIAN_POINT ( 'NONE',  ( 56.04842253378700434, -45.73510956910900660, -25.30965062049470049 ) ) ;
#314 = CARTESIAN_POINT ( 'NONE',  ( 54.83367525942058052, 19.86242937399058306, -75.27593038797637348 ) ) ;
#315 = ORIENTED_EDGE ( 'NONE', *, *, #51572, .T. ) ;
#316 = CYLINDRICAL_SURFACE ( 'NONE', #61, 1.000000000000000888 ) ;
#317 = CARTESIAN_POINT ( 'NONE',  ( 10.20899662427918564, -12.23061640146900686, -71.61833297012245225 ) ) ;
#318 = CARTESIAN_POINT ( 'NONE',  ( 23.83903770539513900, -13.54551362709085538, -35.42433238772350279 ) ) ;
#319 = CARTESIAN_POINT ( 'NONE',  ( 17.19215044318390184, -7.439214858484909598, -47.33329750477089704 ) ) ;
#320 = CIRCLE ( 'NONE', #22077, 7.910999999999997812 ) ;
#321 = CARTESIAN_POINT ( 'NONE',  ( 8.428846698934018278, -17.68690243860981681, -68.42433492461131550 ) ) ;
#322 = CARTESIAN_POINT ( 'NONE',  ( 42.10929425512229329, -37.64097509248548334, -79.77316519949246754 ) ) ;
#323 = SHAPE_REPRESENTATION_RELATIONSHIP ( 'NONE' , 'NONE' ,  #19070, #24050 ) ;
#324 = ORIENTED_EDGE ( 'NONE', *, *, #5080, .T. ) ;
#325 = CARTESIAN_POINT ( 'NONE',  ( 11.84646636965089961, -64.37535564892330342, -24.61798141452300115 ) ) ;
#326 = CARTESIAN_POINT ( 'NONE',  ( 21.51457940895319965, -10.46299709236900100, -33.98952930500309577 ) ) ;
#327 = CARTESIAN_POINT ( 'NONE',  ( 41.50829725104460266, 14.07267842887970133, -6.113795638072149430 ) ) ;
#328 = EDGE_CURVE ( 'NONE', #9603, #32428, #39376, .T. ) ;
#329 = CARTESIAN_POINT ( 'NONE',  ( 14.89540806449589994, 21.53776777092619810, -76.12726769927830617 ) ) ;
#330 = EDGE_CURVE ( 'NONE', #24503, #9584, #50468, .T. ) ;
#331 = VECTOR ( 'NONE', #5456, 1000.000000000000227 ) ;
#332 = CARTESIAN_POINT ( 'NONE',  ( 52.15297977881749603, 18.44951849047100367, -77.15976221510139510 ) ) ;
#333 = CARTESIAN_POINT ( 'NONE',  ( 83.78435757737699419, -44.62302606491700629, -47.11582429421620333 ) ) ;
#334 = DIRECTION ( 'NONE',  ( 1.000000000000000000, 0.000000000000000000, 0.000000000000000000 ) ) ;
#335 = CARTESIAN_POINT ( 'NONE',  ( 8.883252294883678957, -19.54178268943019958, -44.34971538379739542 ) ) ;
#336 = VERTEX_POINT ( 'NONE', #49836 ) ;
#337 = CARTESIAN_POINT ( 'NONE',  ( 53.32987016954000126, -49.16639059516919730, -27.25060986079260061 ) ) ;
#338 = CARTESIAN_POINT ( 'NONE',  ( 12.47078628662380062, -64.90377506766920135, -16.09719858678619886 ) ) ;
#339 = FACE_OUTER_BOUND ( 'NONE', #8165, .T. ) ;
#340 = CARTESIAN_POINT ( 'NONE',  ( 2.633937397696199501, -15.61618894467929763, -1.149999999999999911 ) ) ;
#341 = CARTESIAN_POINT ( 'NONE',  ( 68.13393739769620083, -33.11618894467940066, -65.65000000000000568 ) ) ;
#342 = ORIENTED_EDGE ( 'NONE', *, *, #163, .T. ) ;
#343 = CARTESIAN_POINT ( 'NONE',  ( -5.211271184535770651, -47.35087631705189892, -5.409249467409000367 ) ) ;
#344 = CARTESIAN_POINT ( 'NONE',  ( 47.43699537176610193, 23.38932764359389793, -54.65593435207329520 ) ) ;
#345 = CARTESIAN_POINT ( 'NONE',  ( 21.54530417723247737, -19.77479742635252080, -48.66115513169237516 ) ) ;
#346 = CARTESIAN_POINT ( 'NONE',  ( 63.44018392888030178, 1.383811055320669947, -62.77287342953649585 ) ) ;
#347 = CARTESIAN_POINT ( 'NONE',  ( 12.80406157968140057, 19.41979416798140079, -21.33287590401240053 ) ) ;
#348 = PLANE ( 'NONE',  #1400 ) ;
#349 = CARTESIAN_POINT ( 'NONE',  ( 42.00047115798010111, 12.65453701896299954, -4.514521080317789981 ) ) ;
#350 = DIRECTION ( 'NONE',  ( 1.000000000000000000, 2.460964292799963328E-14, 0.000000000000000000 ) ) ;
#352 = EDGE_CURVE ( 'NONE', #42477, #4597, #41871, .T. ) ;
#351 = CARTESIAN_POINT ( 'NONE',  ( 18.13393739769620083, -41.61618894467930119, -54.64999999999999858 ) ) ;
#353 = CARTESIAN_POINT ( 'NONE',  ( 16.13393739769620083, -15.61618894467929941, -22.14999999999999858 ) ) ;
#354 = CARTESIAN_POINT ( 'NONE',  ( 58.37494088879699206, -46.85178433881189619, -47.96570233379380710 ) ) ;
#355 = CYLINDRICAL_SURFACE ( 'NONE', #16437, 7.910999999999997812 ) ;
#356 = AXIS2_PLACEMENT_3D ( 'NONE', #1615, #5303, #5043 ) ;
#357 = CARTESIAN_POINT ( 'NONE',  ( 65.02936113742819657, 1.390208944942409985, -61.02997314496759884 ) ) ;
#358 = CARTESIAN_POINT ( 'NONE',  ( 17.66259199974900085, -52.33797002293529488, -75.98739629952659413 ) ) ;
#359 = EDGE_CURVE ( 'NONE', #15227, #17198, #33478, .T. ) ;
#360 = CARTESIAN_POINT ( 'NONE',  ( 22.46012642958591599, -10.75454366414201246, -73.29933459694514397 ) ) ;
#361 = CARTESIAN_POINT ( 'NONE',  ( 63.57044994947320760, 1.402336724397559964, -62.38137791222469986 ) ) ;
#362 = VERTEX_POINT ( 'NONE', #30409 ) ;
#363 = FACE_OUTER_BOUND ( 'NONE', #31062, .T. ) ;
#364 = CARTESIAN_POINT ( 'NONE',  ( 8.803701492139829554, 31.98286322187070141, -46.67019247816079286 ) ) ;
#365 = CARTESIAN_POINT ( 'NONE',  ( 22.90093635944459649, -15.62053987609991701, -34.45302314068787553 ) ) ;
#366 = CARTESIAN_POINT ( 'NONE',  ( 11.41959527949359909, -9.607686208987979981, -81.23899999999999011 ) ) ;
#367 = VERTEX_POINT ( 'NONE', #1612 ) ;
#368 = CARTESIAN_POINT ( 'NONE',  ( 18.39143759339100015, 20.51618323985760028, -75.32473453343510528 ) ) ;
#369 = ORIENTED_EDGE ( 'NONE', *, *, #42644, .T. ) ;
#370 = ORIENTED_EDGE ( 'NONE', *, *, #29740, .F. ) ;
#371 = VERTEX_POINT ( 'NONE', #34078 ) ;
#372 = FACE_OUTER_BOUND ( 'NONE', #24038, .T. ) ;
#373 = FACE_OUTER_BOUND ( 'NONE', #2514, .T. ) ;
#374 = CARTESIAN_POINT ( 'NONE',  ( 9.807832152388833435, -10.75443395529458535, -62.71600216802090699 ) ) ;
#375 = CARTESIAN_POINT ( 'NONE',  ( 61.73752130501190294, 13.89709510481169907, -46.60858937970350269 ) ) ;
#376 = ORIENTED_EDGE ( 'NONE', *, *, #2345, .F. ) ;
#377 = CARTESIAN_POINT ( 'NONE',  ( 75.37149648727124429, 8.404366805738446189, -12.88285088340076712 ) ) ;
#378 = CARTESIAN_POINT ( 'NONE',  ( 11.93174526809839975, 34.20691394249479345, -17.93019253464870033 ) ) ;
#379 = ORIENTED_EDGE ( 'NONE', *, *, #9836, .T. ) ;
#380 = CARTESIAN_POINT ( 'NONE',  ( 11.18157709302775693, -63.96091097623292399, -24.11720355368492008 ) ) ;
#381 = LINE ( 'NONE', #40735, #27640 ) ;
#382 = ORIENTED_EDGE ( 'NONE', *, *, #47664, .T. ) ;
#383 = ORIENTED_EDGE ( 'NONE', *, *, #15032, .F. ) ;
#384 = DIRECTION ( 'NONE',  ( 0.000000000000000000, -1.000000000000000000, 0.000000000000000000 ) ) ;
#385 = CYLINDRICAL_SURFACE ( 'NONE', #20080, 0.4999999999999984457 ) ;
#386 = CARTESIAN_POINT ( 'NONE',  ( 60.90370348410529999, 14.44994567453569978, -47.72079593689969812 ) ) ;
#387 = CARTESIAN_POINT ( 'NONE',  ( 50.95711422415039493, 14.35971216196159794, -12.63805038270279901 ) ) ;
#388 = AXIS2_PLACEMENT_3D ( 'NONE', #14443, #6852, #15224 ) ;
#389 = EDGE_CURVE ( 'NONE', #27054, #15604, #37779, .T. ) ;
#390 = CARTESIAN_POINT ( 'NONE',  ( 14.34417029198830029, 20.88381105532299742, -21.14999999999999858 ) ) ;
#391 = CARTESIAN_POINT ( 'NONE',  ( -10.44638207467119884, 11.54816621806459942, -6.014155644910160525 ) ) ;
#392 = CARTESIAN_POINT ( 'NONE',  ( 38.67452568954060155, -15.61618894467929941, -81.65000000000000568 ) ) ;
#393 = CARTESIAN_POINT ( 'NONE',  ( 57.33093049919349937, 14.58258304156659868, -26.26999088063260146 ) ) ;
#394 = CARTESIAN_POINT ( 'NONE',  ( 10.01583490929099973, -20.53102059231009946, -58.07208434834350186 ) ) ;
#395 = ORIENTED_EDGE ( 'NONE', *, *, #27626, .F. ) ;
#396 = DIRECTION ( 'NONE',  ( -0.8090169943749478954, -0.5877852522924724710, 0.000000000000000000 ) ) ;
#397 = VECTOR ( 'NONE', #38374, 1000.000000000000000 ) ;
#398 = CARTESIAN_POINT ( 'NONE',  ( 22.23393739769620225, -15.61618894467929941, -8.849999999999999645 ) ) ;
#399 = CARTESIAN_POINT ( 'NONE',  ( 12.74573753497439910, 34.25580809235049884, -47.28532827175700248 ) ) ;
#400 = CARTESIAN_POINT ( 'NONE',  ( 72.40616118569840864, 1.406831506490830108, -69.61258613051629141 ) ) ;
#401 = CARTESIAN_POINT ( 'NONE',  ( 43.60315030137302728, -39.92105456565624877, -68.58134689406078621 ) ) ;
#402 = CARTESIAN_POINT ( 'NONE',  ( 12.36324357420019915, -64.54680782163349306, -15.76420532458509882 ) ) ;
#403 = CARTESIAN_POINT ( 'NONE',  ( 13.61804211761770134, 18.93546665499809833, -20.94890276653890027 ) ) ;
#404 = CARTESIAN_POINT ( 'NONE',  ( 46.95604843068529988, 23.06042629058710247, -75.52284352240690168 ) ) ;
#405 = CARTESIAN_POINT ( 'NONE',  ( 48.72504344960400147, -54.07331086023980049, -55.30415983355479881 ) ) ;
#406 = DIRECTION ( 'NONE',  ( 0.000000000000000000, 0.000000000000000000, 1.000000000000000000 ) ) ;
#407 = DIRECTION ( 'NONE',  ( 0.5720614028176879140, -0.7071067811865481278, 0.4156269377774475249 ) ) ;
#408 = EDGE_CURVE ( 'NONE', #24575, #50266, #21250, .T. ) ;
#409 = CARTESIAN_POINT ( 'NONE',  ( 16.13393739769620083, -15.61618894467929941, -23.15000000000000213 ) ) ;
#410 = ORIENTED_EDGE ( 'NONE', *, *, #13192, .T. ) ;
#411 = CARTESIAN_POINT ( 'NONE',  ( 19.99250983278150073, -9.242954828350208984, -40.74063233595069988 ) ) ;
#412 = DIRECTION ( 'NONE',  ( 0.6415444970810859626, -0.4854844151940995167, 0.5939070136550161916 ) ) ;
#413 = ORIENTED_EDGE ( 'NONE', *, *, #32309, .F. ) ;
#414 = CARTESIAN_POINT ( 'NONE',  ( 29.13393739769619728, -36.11618894467930119, -81.65000000000000568 ) ) ;
#415 = CARTESIAN_POINT ( 'NONE',  ( 60.63173930441830350, -45.57621591238160619, -47.21435140852850054 ) ) ;
#416 = LINE ( 'NONE', #12475, #13701 ) ;
#417 = CARTESIAN_POINT ( 'NONE',  ( 73.89392149341017557, -43.37877748987173732, -12.94883270627985183 ) ) ;
#419 = LINE ( 'NONE', #4352, #37390 ) ;
#418 = CARTESIAN_POINT ( 'NONE',  ( 42.16784573056604302, 8.550091971082537157, -75.52128294923836904 ) ) ;
#420 = CARTESIAN_POINT ( 'NONE',  ( 87.61621807841599718, 1.883811055320649963, -61.12885639714370001 ) ) ;
#421 = CARTESIAN_POINT ( 'NONE',  ( 68.13393739806078031, -1.166188945131049870, -65.65000000072619457 ) ) ;
#422 = ORIENTED_EDGE ( 'NONE', *, *, #26234, .F. ) ;
#423 = CARTESIAN_POINT ( 'NONE',  ( 84.44784216359251161, -43.11618894467930119, -47.47585302082339354 ) ) ;
#424 = CIRCLE ( 'NONE', #49007, 20.79999999999999716 ) ;
#425 = VERTEX_POINT ( 'NONE', #29383 ) ;
#426 = ORIENTED_EDGE ( 'NONE', *, *, #33634, .T. ) ;
#427 = B_SPLINE_CURVE_WITH_KNOTS ( 'NONE', 3,
 ( #29954, #1422, #45970, #5870, #21837, #29447, #49652, #1939, #10063, #37844, #38104, #33890, #29696, #26023, #9030, #1680, #49901, #42035, #13995, #40993, #6136, #49137, #13234, #22092, #25758, #34143, #2201, #28925, #37572, #13489, #17407, #41510, #24977, #9299, #5107 ),
 .UNSPECIFIED., .F., .F.,
 ( 4, 2, 2, 2, 2, 2, 2, 2, 2, 2, 2, 2, 2, 1, 1, 1, 1, 1, 2, 4 ),
 ( 0.000000000000000000, 0.03125022957391215134, 0.06250045914782430267, 0.09375068872173646095, 0.1250009182956486053, 0.1562511478695607636, 0.1875013774434729219, 0.2500018365912970997, 0.3125022957391213607, 0.3750027548869455107, 0.4375032140347697718, 0.4687534436086817080, 0.4843785583956377039, 0.4921911157891156186, 0.4960973944858545481, 0.4980505338342237631, 0.4990271035084085649, 0.4995153883455007993, 0.4997595307640467777, 0.5000036731825925340 ),
 .UNSPECIFIED. ) ;
#428 = ORIENTED_EDGE ( 'NONE', *, *, #30931, .T. ) ;
#429 = CARTESIAN_POINT ( 'NONE',  ( 61.51108476807580416, -45.14457241600359794, -46.37195364498460037 ) ) ;
#430 = CARTESIAN_POINT ( 'NONE',  ( 8.428856344205472695, -13.54544038257251160, -78.87566503557303577 ) ) ;
#431 = CARTESIAN_POINT ( 'NONE',  ( 76.39418201693595734, -13.59255262052404056, -12.77143339381032838 ) ) ;
#432 = CARTESIAN_POINT ( 'NONE',  ( 53.55397377960559879, -51.73583884506710717, -53.25782589811129242 ) ) ;
#433 = ORIENTED_EDGE ( 'NONE', *, *, #41777, .F. ) ;
#434 = VERTEX_POINT ( 'NONE', #14181 ) ;
#435 = CARTESIAN_POINT ( 'NONE',  ( -0.09557254528323877452, 14.34657913917513383, -34.84921897185084561 ) ) ;
#436 = CARTESIAN_POINT ( 'NONE',  ( 22.14946380439831941, -18.71488146266838370, -32.99858898373786076 ) ) ;
#437 = CARTESIAN_POINT ( 'NONE',  ( 56.50529462384820079, -50.75959910210979587, -53.84464729327209653 ) ) ;
#438 = CARTESIAN_POINT ( 'NONE',  ( 20.29260916630788714, -10.20487065087579026, -36.16115160781710358 ) ) ;
#439 = CARTESIAN_POINT ( 'NONE',  ( 24.04493740220357978, -15.60985432249296423, -59.79207070245149680 ) ) ;
#440 = ORIENTED_EDGE ( 'NONE', *, *, #16005, .F. ) ;
#441 = DIRECTION ( 'NONE',  ( 0.5897727341282541502, 0.3900873262218164661, 0.7071067811865459074 ) ) ;
#442 = CARTESIAN_POINT ( 'NONE',  ( 52.53691734465949992, -50.17408895096939858, -76.99573695420890829 ) ) ;
#443 = CARTESIAN_POINT ( 'NONE',  ( 60.24866557976250192, 14.54998834221814796, -47.36885438232269507 ) ) ;
#444 = CARTESIAN_POINT ( 'NONE',  ( 82.13853704237929776, 15.88381105532069704, -46.37203261889099792 ) ) ;
#445 = CARTESIAN_POINT ( 'NONE',  ( 19.92217479402680169, -8.743343462593710314, -51.67284482273019819 ) ) ;
#446 = FACE_OUTER_BOUND ( 'NONE', #23223, .T. ) ;
#447 = EDGE_CURVE ( 'NONE', #13016, #4886, #50086, .T. ) ;
#448 = CARTESIAN_POINT ( 'NONE',  ( -22.81805345843360655, -13.96957243270927762, -54.73201327936519789 ) ) ;
#449 = DIRECTION ( 'NONE',  ( 0.000000000000000000, 0.000000000000000000, 1.000000000000000000 ) ) ;
#450 = CARTESIAN_POINT ( 'NONE',  ( 70.83393739769717001, -48.11618894467018492, -75.95000000000109708 ) ) ;
#452 = EDGE_CURVE ( 'NONE', #19246, #15767, #46171, .T. ) ;
#451 = FACE_OUTER_BOUND ( 'NONE', #25206, .T. ) ;
#453 = EDGE_CURVE ( 'NONE', #24512, #4326, #17346, .T. ) ;
#454 = DIRECTION ( 'NONE',  ( 0.000000000000000000, 0.000000000000000000, -1.000000000000000000 ) ) ;
#455 = CARTESIAN_POINT ( 'NONE',  ( 9.307192117435908685, -13.84471835421079966, -51.92799550646089557 ) ) ;
#456 = CARTESIAN_POINT ( 'NONE',  ( -11.39236625349560050, -33.81790884424879806, -54.64999999999999858 ) ) ;
#457 = EDGE_CURVE ( 'NONE', #11026, #50723, #11770, .T. ) ;
#458 = EDGE_LOOP ( 'NONE', ( #21605, #10515, #19262, #50340, #19221 ) ) ;
#459 = VECTOR ( 'NONE', #50948, 999.9999999999998863 ) ;
#460 = CARTESIAN_POINT ( 'NONE',  ( 14.53113689391020102, -51.97808261890150305, -75.79330468503940210 ) ) ;
#461 = CARTESIAN_POINT ( 'NONE',  ( 47.30697531817629908, -54.71648428534599873, -54.76104250077580815 ) ) ;
#462 = PRESENTATION_STYLE_ASSIGNMENT (( #44492 ) ) ;
#463 = LINE ( 'NONE', #28751, #28813 ) ;
#464 = CARTESIAN_POINT ( 'NONE',  ( 24.02795760665879854, -15.08725952809635373, -55.48638191674730535 ) ) ;
#465 = DIRECTION ( 'NONE',  ( -0.8660254037844380415, 0.5000000000000012212, -1.387778780781449373E-16 ) ) ;
#466 = CARTESIAN_POINT ( 'NONE',  ( 10.77197593522630115, 33.74263483046039624, -18.02693217510839929 ) ) ;
#468 = CARTESIAN_POINT ( 'NONE',  ( -9.500613363851449833, -43.72129052405930594, -5.962761149281509354 ) ) ;
#467 = CARTESIAN_POINT ( 'NONE',  ( 83.89200044194980421, 17.38381105532069881, -53.92796738110899923 ) ) ;
#469 = DIRECTION ( 'NONE',  ( -1.000000000000000000, 0.000000000000000000, 0.000000000000000000 ) ) ;
#470 = EDGE_CURVE ( 'NONE', #16490, #36140, #45386, .T. ) ;
#471 = CARTESIAN_POINT ( 'NONE',  ( 48.42313109053679909, 22.83113193936399909, -54.61340708730690352 ) ) ;
#472 = ORIENTED_EDGE ( 'NONE', *, *, #37574, .F. ) ;
#473 = CARTESIAN_POINT ( 'NONE',  ( 52.98874192681579842, -49.59627630596699532, -48.96317220553530092 ) ) ;
#474 = ORIENTED_EDGE ( 'NONE', *, *, #40095, .T. ) ;
#475 = CARTESIAN_POINT ( 'NONE',  ( -5.366062602303798279, -15.61618894467929586, -11.05000000000000071 ) ) ;
#476 = LINE ( 'NONE', #31653, #22692 ) ;
#477 = CARTESIAN_POINT ( 'NONE',  ( 57.02861371936400303, -50.62805676435459645, -53.87746547587289569 ) ) ;
#478 = CARTESIAN_POINT ( 'NONE',  ( 84.42999065749789622, 12.06718754213130040, -47.39892822416609874 ) ) ;
#479 = CARTESIAN_POINT ( 'NONE',  ( 22.10083642963680006, -11.85604604323910038, -68.27383256501039455 ) ) ;
#480 = CARTESIAN_POINT ( 'NONE',  ( 52.97768851982059601, 18.39522800273699943, -49.05519422600419688 ) ) ;
#481 = CARTESIAN_POINT ( 'NONE',  ( 56.06159152657470202, -45.29125632613430241, -16.02375003208479853 ) ) ;
#482 = DIRECTION ( 'NONE',  ( 1.000000000000000000, -1.080128361472376380E-29, -1.260570937617230037E-11 ) ) ;
#483 = VERTEX_POINT ( 'NONE', #37512 ) ;
#484 = ORIENTED_EDGE ( 'NONE', *, *, #27774, .F. ) ;
#485 = CARTESIAN_POINT ( 'NONE',  ( 11.50291103294089901, -65.34958077267680210, -17.75618544430749779 ) ) ;
#486 = CARTESIAN_POINT ( 'NONE',  ( 11.18028273825089869, 33.73068083865630484, -46.79252262002829355 ) ) ;
#487 = CARTESIAN_POINT ( 'NONE',  ( -31.36606260230380272, -53.11618894467930119, 11.84999999999999964 ) ) ;
#488 = CARTESIAN_POINT ( 'NONE',  ( 61.75019796695539753, 13.88381105532070059, -28.15000000000000213 ) ) ;
#489 = CARTESIAN_POINT ( 'NONE',  ( 10.63867076987313176, -63.67733169492935730, -23.65473337217691352 ) ) ;
#490 = CARTESIAN_POINT ( 'NONE',  ( 0.1294298976607914931, -10.50415099917325534, -34.68804011290710321 ) ) ;
#491 = ADVANCED_FACE ( 'NONE', ( #29634 ), #45639, .T. ) ;
#492 = AXIS2_PLACEMENT_3D ( 'NONE', #43225, #42968, #30365 ) ;
#493 = ORIENTED_EDGE ( 'NONE', *, *, #30281, .F. ) ;
#494 = CARTESIAN_POINT ( 'NONE',  ( 13.06064429528559323, 19.66369995475592347, -21.55066630772461878 ) ) ;
#495 = TOROIDAL_SURFACE ( 'NONE', #15595, 9.000000000000000000, 1.000000000000000000 ) ;
#496 = CARTESIAN_POINT ( 'NONE',  ( 10.97912920880960108, -63.30540042885840535, -44.74308033447209709 ) ) ;
#497 = CARTESIAN_POINT ( 'NONE',  ( 15.09837707772988225, -23.52718739147557869, -60.04936120705558977 ) ) ;
#498 = CYLINDRICAL_SURFACE ( 'NONE', #18331, 0.4999999999999997224 ) ;
#499 = CARTESIAN_POINT ( 'NONE',  ( 50.39461351434329828, -50.13496434787850120, -76.14999999999999147 ) ) ;
#500 = CARTESIAN_POINT ( 'NONE',  ( 11.93174526809839975, -65.43929183185349530, -17.93019253464870033 ) ) ;
#501 = ORIENTED_EDGE ( 'NONE', *, *, #33687, .T. ) ;
#502 = CARTESIAN_POINT ( 'NONE',  ( 17.07096049057481935, -43.84596607001319768, -60.51477253168923909 ) ) ;
#503 = CARTESIAN_POINT ( 'NONE',  ( 68.13393739806078031, -1.166188944679350081, -41.65000000083975351 ) ) ;
#504 = CARTESIAN_POINT ( 'NONE',  ( 20.63393739769620083, -41.61618894467930119, -35.14999999999999858 ) ) ;
#505 = CARTESIAN_POINT ( 'NONE',  ( 58.35672585773610166, 17.12870549263289988, -50.48250036787379003 ) ) ;
#506 = CARTESIAN_POINT ( 'NONE',  ( 8.766479793714031743, -11.91439363571640087, -70.94053896172950147 ) ) ;
#507 = CARTESIAN_POINT ( 'NONE',  ( -21.36606260230379917, -53.11618894467930119, 10.84999999999999964 ) ) ;
#508 = CARTESIAN_POINT ( 'NONE',  ( 56.46528349507870814, 19.54388576035330161, -74.14939842031650130 ) ) ;
#509 = CONTEXT_DEPENDENT_SHAPE_REPRESENTATION ( #17419, #8056 ) ;
#510 = CARTESIAN_POINT ( 'NONE',  ( 46.98568754098660349, -53.76726209812860446, -75.86283294038038605 ) ) ;
#511 = ORIENTED_EDGE ( 'NONE', *, *, #15909, .F. ) ;
#512 = ADVANCED_FACE ( 'NONE', ( #1871 ), #3388, .F. ) ;
#513 = EDGE_CURVE ( 'NONE', #23355, #5619, #23708, .T. ) ;
#514 = CARTESIAN_POINT ( 'NONE',  ( 23.21317868976809606, -13.29432836881139934, -60.13177655599749727 ) ) ;
#515 = CARTESIAN_POINT ( 'NONE',  ( 53.23879025501499740, -49.52941110961769766, -49.17697456386299848 ) ) ;
#516 = CARTESIAN_POINT ( 'NONE',  ( 14.34417029198830029, 20.88381105532299742, -76.14999999999999147 ) ) ;
#517 = DIRECTION ( 'NONE',  ( 0.000000000000000000, 0.000000000000000000, 1.000000000000000000 ) ) ;
#518 = EDGE_CURVE ( 'NONE', #26843, #25744, #48572, .T. ) ;
#519 = VECTOR ( 'NONE', #18468, 1000.000000000000227 ) ;
#520 = CARTESIAN_POINT ( 'NONE',  ( 47.04991247857869752, 22.88708854419270011, -75.60848552117779775 ) ) ;
#521 = CARTESIAN_POINT ( 'NONE',  ( 19.04590477917927061, -52.29702409155545695, -15.95254375907780364 ) ) ;
#522 = DIRECTION ( 'NONE',  ( 1.000000000000000000, 0.000000000000000000, 0.000000000000000000 ) ) ;
#523 = DIRECTION ( 'NONE',  ( -0.5193766129849238800, 0.000000000000000000, -0.8545454545454611583 ) ) ;
#524 = AXIS2_PLACEMENT_3D ( 'NONE', #10350, #26309, #30759 ) ;
#525 = CARTESIAN_POINT ( 'NONE',  ( 19.12205772217659927, -7.931538163062599622, -71.12571408330079237 ) ) ;
#526 = AXIS2_PLACEMENT_3D ( 'NONE', #41480, #49623, #33347 ) ;
#527 = CARTESIAN_POINT ( 'NONE',  ( 54.55443780522559649, -50.61618894718989736, -76.86024425967369211 ) ) ;
#528 = CARTESIAN_POINT ( 'NONE',  ( 43.79854539025301818, -40.04024745141481390, -67.21557273064806282 ) ) ;
#529 = CARTESIAN_POINT ( 'NONE',  ( 63.47971227208819300, 1.385888765344509999, -68.65207957385619864 ) ) ;
#530 = CARTESIAN_POINT ( 'NONE',  ( 61.25020875759329897, 14.02882808903070000, -46.85262742158650440 ) ) ;
#531 = ADVANCED_FACE ( 'NONE', ( #39580 ), #38821, .T. ) ;
#532 = CARTESIAN_POINT ( 'NONE',  ( -12.80120649412780054, -56.90739261401959936, -52.53814278327499920 ) ) ;
#533 = ORIENTED_EDGE ( 'NONE', *, *, #7118, .T. ) ;
#534 = CARTESIAN_POINT ( 'NONE',  ( 52.87019085405700025, -49.63973566670129856, -48.66536726492419263 ) ) ;
#535 = CARTESIAN_POINT ( 'NONE',  ( 59.27658655098359475, -45.11618906053649880, -25.77369910084199844 ) ) ;
#536 = CARTESIAN_POINT ( 'NONE',  ( 18.13393739769639978, 10.38381105532070059, -35.14999999999999858 ) ) ;
#537 = CARTESIAN_POINT ( 'NONE',  ( 13.68344161607869935, 19.38032502360789877, -21.30676595101419935 ) ) ;
#538 = CARTESIAN_POINT ( 'NONE',  ( 57.00662312664200471, 14.67649396222829949, -26.24686926800940157 ) ) ;
#539 = CARTESIAN_POINT ( 'NONE',  ( 19.49523065122039966, -9.415844892879128736, -36.11094655318100166 ) ) ;
#540 = CARTESIAN_POINT ( 'NONE',  ( 50.91412666205799553, 17.97650990569060170, -76.31682797917909511 ) ) ;
#541 = CARTESIAN_POINT ( 'NONE',  ( 53.03884170327399517, 18.32633884920069889, -48.90887833971159893 ) ) ;
#542 = CARTESIAN_POINT ( 'NONE',  ( 71.19443613848248731, 1.370118064600909902, -70.39245762607309587 ) ) ;
#543 = DIRECTION ( 'NONE',  ( 0.000000000000000000, -1.000000000000000000, 0.000000000000000000 ) ) ;
#544 = CARTESIAN_POINT ( 'NONE',  ( 75.20701160720210510, -44.95918647008760161, -14.39058221657740155 ) ) ;
#545 = ORIENTED_EDGE ( 'NONE', *, *, #34037, .F. ) ;
#546 = CARTESIAN_POINT ( 'NONE',  ( 47.73134908716809832, -54.46630275052049086, -54.83109498023989659 ) ) ;
#547 = CARTESIAN_POINT ( 'NONE',  ( 22.90007318524572000, -14.73211321227309512, -68.80558412982628624 ) ) ;
#548 =( BOUNDED_CURVE ( )  B_SPLINE_CURVE ( 3, ( #24797, #5437, #12517, #44221 ),
 .UNSPECIFIED., .F., .T. ) 
 B_SPLINE_CURVE_WITH_KNOTS ( ( 4, 4 ),
 ( 8.754247816369622087E-15, 0.7853981633974498333 ),
 .UNSPECIFIED. ) 
 CURVE ( )  GEOMETRIC_REPRESENTATION_ITEM ( )  RATIONAL_B_SPLINE_CURVE ( ( 1.000000000000000000, 0.9492530216741921212, 0.9492530216741921212, 1.000000000000000000 ) ) 
 REPRESENTATION_ITEM ( '' )  );
#549 = CARTESIAN_POINT ( 'NONE',  ( 41.27829246776259708, 12.87545685813370078, -3.596739354799320054 ) ) ;
#550 = CARTESIAN_POINT ( 'NONE',  ( 58.09124814586559893, 17.43042520853399679, -50.80790410914660526 ) ) ;
#551 = CARTESIAN_POINT ( 'NONE',  ( 71.17905174416029013, 1.387412027389909985, -61.00994802092580471 ) ) ;
#552 = CARTESIAN_POINT ( 'NONE',  ( 61.75019796695539753, 14.88381105532069881, -28.15000000000000213 ) ) ;
#553 = CARTESIAN_POINT ( 'NONE',  ( 72.06056480500649286, 1.091560265417830022, -61.11985751463939920 ) ) ;
#554 = EDGE_CURVE ( 'NONE', #8993, #16411, #16877, .T. ) ;
#555 = CARTESIAN_POINT ( 'NONE',  ( 9.221329868776839689, -19.60017621584825775, -72.34096665405537863 ) ) ;
#556 = CARTESIAN_POINT ( 'NONE',  ( 65.07343865691001383, 1.370118064600889918, -70.39245762607309587 ) ) ;
#557 = ORIENTED_EDGE ( 'NONE', *, *, #33185, .T. ) ;
#558 = ADVANCED_FACE ( 'NONE', ( #34862 ), #38557, .T. ) ;
#559 = ORIENTED_EDGE ( 'NONE', *, *, #15390, .T. ) ;
#560 = CARTESIAN_POINT ( 'NONE',  ( 14.16335350998109988, -51.13178799506830075, -22.70850810526620123 ) ) ;
#561 = DIRECTION ( 'NONE',  ( -0.05643417272666772372, 0.04100182651872436718, -0.9975640502598241977 ) ) ;
#562 = ORIENTED_EDGE ( 'NONE', *, *, #13602, .T. ) ;
#563 = CARTESIAN_POINT ( 'NONE',  ( 33.77213399851893172, -15.61618894397937929, 14.62639320225000006 ) ) ;
#564 = CARTESIAN_POINT ( 'NONE',  ( 13.00893739761190027, -65.51843714052189682, -47.75434321210310173 ) ) ;
#565 = CARTESIAN_POINT ( 'NONE',  ( 54.70456362050531851, 19.88764045771333500, -75.31516034446933361 ) ) ;
#566 = VERTEX_POINT ( 'NONE', #15220 ) ;
#567 = CARTESIAN_POINT ( 'NONE',  ( 9.366937397696199596, -15.61618894467949836, -28.45282021618999835 ) ) ;
#568 = CARTESIAN_POINT ( 'NONE',  ( 66.72561048563109409, -33.11618894467930829, -20.64999999980150136 ) ) ;
#569 = VECTOR ( 'NONE', #35500, 1000.000000000000114 ) ;
#570 = CARTESIAN_POINT ( 'NONE',  ( 20.11810930412978138, -8.703690030208671047, -35.17433314337063877 ) ) ;
#571 = CARTESIAN_POINT ( 'NONE',  ( 9.848987560566159871, -10.27932417210969973, -47.01642178051639576 ) ) ;
#572 = CARTESIAN_POINT ( 'NONE',  ( 22.46010534431878369, -20.47786315848903271, -67.71599960382185657 ) ) ;
#573 = CARTESIAN_POINT ( 'NONE',  ( 41.62617804670394861, -37.56246594912547465, -82.18879675496150128 ) ) ;
#574 = ORIENTED_EDGE ( 'NONE', *, *, #8895, .T. ) ;
#575 = EDGE_CURVE ( 'NONE', #14719, #11008, #2482, .T. ) ;
#576 = CARTESIAN_POINT ( 'NONE',  ( 18.20469237649928118, -23.32126772162391148, -42.20899783913211678 ) ) ;
#577 = CARTESIAN_POINT ( 'NONE',  ( 9.430654476343230286, -12.36462134097749832, -39.37641661732919829 ) ) ;
#578 = CARTESIAN_POINT ( 'NONE',  ( 40.70149984973559754, 14.09668779090960022, -5.681031432320810204 ) ) ;
#579 = ADVANCED_FACE ( 'NONE', ( #43010 ), #7355, .T. ) ;
#580 = AXIS2_PLACEMENT_3D ( 'NONE', #5691, #33953, #49719 ) ;
#581 = CARTESIAN_POINT ( 'NONE',  ( 14.25117074270229978, 20.49345067490170180, -75.53710645103458887 ) ) ;
#582 = CARTESIAN_POINT ( 'NONE',  ( 52.23705703117550314, 18.52650809402000220, -77.18591267702620939 ) ) ;
#583 = CARTESIAN_POINT ( 'NONE',  ( 33.83216070239956252, -11.80875449455119686, -34.79644660940672907 ) ) ;
#584 = DIRECTION ( 'NONE',  ( -5.226026857244350872E-28, -1.000000000000000000, -1.469246684736110336E-14 ) ) ;
#585 = CARTESIAN_POINT ( 'NONE',  ( 16.51850286063059770, -7.379998677711620658, -41.02252027912539489 ) ) ;
#586 = VERTEX_POINT ( 'NONE', #35117 ) ;
#587 = CARTESIAN_POINT ( 'NONE',  ( 52.82930795109979272, -49.63909307504320623, -27.85263494685039731 ) ) ;
#588 = CARTESIAN_POINT ( 'NONE',  ( 11.66463330127890075, -65.13871550253499265, -16.69890713983809860 ) ) ;
#589 = CARTESIAN_POINT ( 'NONE',  ( 50.37629383861175825, -36.29100334579137410, -76.18004623245177243 ) ) ;
#590 = CARTESIAN_POINT ( 'NONE',  ( 14.06336117282463150, -23.32131560580253193, -64.37566576587414602 ) ) ;
#591 = CARTESIAN_POINT ( 'NONE',  ( 16.13393739769620083, -15.61618894467929941, -6.928362978644219794 ) ) ;
#592 = CARTESIAN_POINT ( 'NONE',  ( 51.83642112035360583, 14.98332062161530054, -13.79430700932419995 ) ) ;
#593 = ORIENTED_EDGE ( 'NONE', *, *, #39989, .T. ) ;
#594 = CARTESIAN_POINT ( 'NONE',  ( -10.40425463635500059, -42.83144259959529165, -6.155050416280118952 ) ) ;
#595 = CARTESIAN_POINT ( 'NONE',  ( 47.39512065225470394, 23.42572006056330025, -54.76405005057330300 ) ) ;
#596 = CIRCLE ( 'NONE', #18187, 2.999999999999999112 ) ;
#597 = LINE ( 'NONE', #27860, #18665 ) ;
#598 = CARTESIAN_POINT ( 'NONE',  ( 63.40852617131290003, 1.383411777981069957, -62.75344103383148564 ) ) ;
#599 = CARTESIAN_POINT ( 'NONE',  ( 54.84969908772705338, 16.62357410610304598, -26.66241143700859695 ) ) ;
#600 = CARTESIAN_POINT ( 'NONE',  ( 43.09344256900070036, 12.72802089279420024, -5.051331041914770559 ) ) ;
#601 = CARTESIAN_POINT ( 'NONE',  ( 11.13393739770729951, 32.24969779483610210, -22.73390400586109905 ) ) ;
#602 = CARTESIAN_POINT ( 'NONE',  ( 20.11808726905815803, -8.703676856905904202, -61.45899610695946791 ) ) ;
#603 = CYLINDRICAL_SURFACE ( 'NONE', #2404, 1.999999999999999556 ) ;
#604 = CARTESIAN_POINT ( 'NONE',  ( 55.64975804555480465, -48.32680575653600386, -48.64277601874709944 ) ) ;
#605 = CARTESIAN_POINT ( 'NONE',  ( 69.22748654599971019, -50.70395984887900909, -74.34354914830332461 ) ) ;
#606 = CARTESIAN_POINT ( 'NONE',  ( 64.89668540611299363, 1.325715844996850024, -60.88145737504000010 ) ) ;
#607 = CARTESIAN_POINT ( 'NONE',  ( 17.33798092487360165, -52.97186080988799972, -76.14999999999999147 ) ) ;
#608 = DIRECTION ( 'NONE',  ( -0.3863301728269261659, -0.9223605572461982538, 0.000000000000000000 ) ) ;
#609 = CARTESIAN_POINT ( 'NONE',  ( 10.26456537522289914, -19.52689034815859870, -81.26573725944388116 ) ) ;
#610 = CARTESIAN_POINT ( 'NONE',  ( 9.366948553292196777, -14.73030905516724509, -47.49448696612870435 ) ) ;
#611 = VERTEX_POINT ( 'NONE', #35648 ) ;
#612 = FACE_BOUND ( 'NONE', #38097, .T. ) ;
#613 = CARTESIAN_POINT ( 'NONE',  ( 9.285737161019211428, 31.96511163084949558, -46.53047815523170527 ) ) ;
#614 = CARTESIAN_POINT ( 'NONE',  ( 11.13393739769619906, -63.48206547090349972, -24.15000000000000213 ) ) ;
#615 = ADVANCED_FACE ( 'NONE', ( #51634 ), #29332, .F. ) ;
#616 = CARTESIAN_POINT ( 'NONE',  ( 13.72573378235179931, -8.165455470583809827, -81.23899999999999011 ) ) ;
#617 = EDGE_LOOP ( 'NONE', ( #818, #18947 ) ) ;
#618 = CARTESIAN_POINT ( 'NONE',  ( 17.87986931031349869, 20.00715776053360173, -74.86150924066380696 ) ) ;
#619 = ORIENTED_EDGE ( 'NONE', *, *, #38375, .T. ) ;
#620 = EDGE_CURVE ( 'NONE', #33379, #44397, #12840, .T. ) ;
#621 = VERTEX_POINT ( 'NONE', #7872 ) ;
#622 = B_SPLINE_CURVE_WITH_KNOTS ( 'NONE', 3,
 ( #47156, #27206, #3638, #27724, #11765, #210, #47411, #27973 ),
 .UNSPECIFIED., .F., .F.,
 ( 4, 2, 2, 4 ),
 ( 0.000000000000000000, 0.1882768039227099566, 0.3749999999997639666, 0.5000003605116074556 ),
 .UNSPECIFIED. ) ;
#623 = ORIENTED_EDGE ( 'NONE', *, *, #20200, .F. ) ;
#624 = CARTESIAN_POINT ( 'NONE',  ( 12.93454037390620037, -65.51377821817899871, -47.66712770179820069 ) ) ;
#625 = CARTESIAN_POINT ( 'NONE',  ( 57.29425095410220337, -45.82021646256149694, -26.26548405410519749 ) ) ;
#626 = CARTESIAN_POINT ( 'NONE',  ( 23.04658433577699839, -17.87353418447250064, -81.23899999999999011 ) ) ;
#627 = EDGE_CURVE ( 'NONE', #14961, #24006, #37678, .T. ) ;
#628 = CARTESIAN_POINT ( 'NONE',  ( 9.221464511544803955, -11.63197161253809675, -62.67433543276930408 ) ) ;
#629 = DIRECTION ( 'NONE',  ( 0.000000000000000000, 0.000000000000000000, -1.000000000000000000 ) ) ;
#630 = VERTEX_POINT ( 'NONE', #47964 ) ;
#631 = DIRECTION ( 'NONE',  ( 0.000000000000000000, -1.000000000000000000, 0.000000000000000000 ) ) ;
#632 = CARTESIAN_POINT ( 'NONE',  ( 9.367521945652839577, -16.18213243797932677, -35.82056437903438706 ) ) ;
#633 = ORIENTED_EDGE ( 'NONE', *, *, #50882, .T. ) ;
#634 = CARTESIAN_POINT ( 'NONE',  ( 11.25474628969880442, -64.20711136671845054, -24.08007506827187427 ) ) ;
#635 = CARTESIAN_POINT ( 'NONE',  ( 14.14309834359610463, -52.38391192218928438, -75.82251645567293963 ) ) ;
#636 = CARTESIAN_POINT ( 'NONE',  ( 51.96094199614199738, 2.175120467137570124, -77.41819485969911341 ) ) ;
#637 = VERTEX_POINT ( 'NONE', #4185 ) ;
#638 = ORIENTED_EDGE ( 'NONE', *, *, #46821, .F. ) ;
#639 = CARTESIAN_POINT ( 'NONE',  ( 66.72561048563099462, 1.883811055320649963, -20.64999999980150136 ) ) ;
#640 = CARTESIAN_POINT ( 'NONE',  ( 61.51122975691190220, 13.91278366405482636, -46.37203261889099792 ) ) ;
#641 = CARTESIAN_POINT ( 'NONE',  ( 70.82480173460169226, 13.72863524801690005, -13.13951160535810025 ) ) ;
#643 = CARTESIAN_POINT ( 'NONE',  ( 53.05450034938409942, -49.59539206943890122, -49.09560404125600286 ) ) ;
#642 = AXIS2_PLACEMENT_3D ( 'NONE', #26175, #25655, #45863 ) ;
#644 = ADVANCED_FACE ( 'NONE', ( #32710 ), #44798, .T. ) ;
#645 = CARTESIAN_POINT ( 'NONE',  ( 45.86983905350170687, 14.32280688279350045, -9.052205324345139914 ) ) ;
#646 = CIRCLE ( 'NONE', #34945, 1.999999999999998446 ) ;
#647 = CARTESIAN_POINT ( 'NONE',  ( -3.175079596678700433, -15.61618894467929941, 17.35000000000000142 ) ) ;
#648 = CARTESIAN_POINT ( 'NONE',  ( -7.106986607165590719, 14.44895595893859941, -4.821389471371529289 ) ) ;
#649 = CARTESIAN_POINT ( 'NONE',  ( 15.67962062535580081, -50.86266781815560023, -15.65622421709140077 ) ) ;
#650 = CARTESIAN_POINT ( 'NONE',  ( 61.35346592530439835, 13.96312120787509947, -28.05093155658810034 ) ) ;
#651 = CARTESIAN_POINT ( 'NONE',  ( 19.27421804432820096, -22.80822521013089954, -59.65646296961579509 ) ) ;
#652 = ORIENTED_EDGE ( 'NONE', *, *, #31324, .T. ) ;
#653 = FACE_OUTER_BOUND ( 'NONE', #143, .T. ) ;
#654 = FACE_OUTER_BOUND ( 'NONE', #22978, .T. ) ;
#655 = CARTESIAN_POINT ( 'NONE',  ( 11.61686812457489992, 33.60076664006019342, -45.15427369068040520 ) ) ;
#656 = CARTESIAN_POINT ( 'NONE',  ( 72.26841818567149289, 1.277726347179370059, -69.91422003724520096 ) ) ;
#657 = CARTESIAN_POINT ( 'NONE',  ( 43.14443873153287967, -39.87986852203775356, -70.80016690477312125 ) ) ;
#658 = CARTESIAN_POINT ( 'NONE',  ( 46.52115624802139848, 22.06631489729150175, -76.11314272684450088 ) ) ;
#659 = CARTESIAN_POINT ( 'NONE',  ( 48.95357505128730224, -53.97596511168260491, -55.27962234102679417 ) ) ;
#660 = DIRECTION ( 'NONE',  ( 0.000000000000000000, 0.000000000000000000, -1.000000000000000000 ) ) ;
#661 = CARTESIAN_POINT ( 'NONE',  ( 9.993740982288887409, -20.62509161583232142, -34.28983011217102472 ) ) ;
#662 = LINE ( 'NONE', #32351, #47229 ) ;
#663 = CARTESIAN_POINT ( 'NONE',  ( 9.367097141674031846, -15.61601956221279863, -71.84717978381000592 ) ) ;
#664 = ORIENTED_EDGE ( 'NONE', *, *, #24146, .T. ) ;
#665 = CARTESIAN_POINT ( 'NONE',  ( 16.48142850091230116, -8.174015587955670625, -40.58219447382339951 ) ) ;
#666 = CARTESIAN_POINT ( 'NONE',  ( 64.29895108830758943, 1.258806274519160162, -61.13074064017239806 ) ) ;
#667 = VERTEX_POINT ( 'NONE', #32194 ) ;
#668 = DIRECTION ( 'NONE',  ( 1.000000000000000000, 0.000000000000000000, 0.000000000000000000 ) ) ;
#669 = CARTESIAN_POINT ( 'NONE',  ( 60.77842532433790268, -45.71912871634670239, -47.73153708891739910 ) ) ;
#670 = FACE_OUTER_BOUND ( 'NONE', #7098, .T. ) ;
#671 = AXIS2_PLACEMENT_3D ( 'NONE', #41968, #6064, #19398 ) ;
#672 = CARTESIAN_POINT ( 'NONE',  ( 12.53549335446709989, 18.74519657356650271, -21.12176656635870131 ) ) ;
#674 = CARTESIAN_POINT ( 'NONE',  ( 8.222928424025267802, -16.65167072501185075, -78.75066471084360842 ) ) ;
#673 = CARTESIAN_POINT ( 'NONE',  ( 41.86108004392503545, 8.517095955210312042, -77.00193962239630707 ) ) ;
#675 = CARTESIAN_POINT ( 'NONE',  ( 52.32303883665399979, -51.41740952823399624, -75.90202711987829787 ) ) ;
#676 = CARTESIAN_POINT ( 'NONE',  ( 11.27226524438746047, -21.94235859059851634, -52.21600097131449303 ) ) ;
#677 = VERTEX_POINT ( 'NONE', #44536 ) ;
#678 = CARTESIAN_POINT ( 'NONE',  ( 84.44066163939218939, -43.31757366620339411, -47.44491107334449964 ) ) ;
#679 = VERTEX_POINT ( 'NONE', #1033 ) ;
#680 = EDGE_CURVE ( 'NONE', #47514, #50462, #13087, .T. ) ;
#681 = ORIENTED_EDGE ( 'NONE', *, *, #42316, .T. ) ;
#682 = ORIENTED_EDGE ( 'NONE', *, *, #11523, .T. ) ;
#683 = CARTESIAN_POINT ( 'NONE',  ( 61.55619681691449330, -45.18291742677050138, -46.87336930385270506 ) ) ;
#684 = CARTESIAN_POINT ( 'NONE',  ( 9.221442382393673753, -11.63200944172679385, -78.95899856290910179 ) ) ;
#685 = CARTESIAN_POINT ( 'NONE',  ( 76.39242090978348187, -14.36197311350646189, -12.76384447145835921 ) ) ;
#686 = CARTESIAN_POINT ( 'NONE',  ( 49.72648160330919609, -53.64673639094019819, -55.11972614036090334 ) ) ;
#687 = ORIENTED_EDGE ( 'NONE', *, *, #17798, .F. ) ;
#688 = ORIENTED_EDGE ( 'NONE', *, *, #39970, .F. ) ;
#689 = CARTESIAN_POINT ( 'NONE',  ( 49.40552051342540096, 22.26542118999089936, -54.15739458345379376 ) ) ;
#690 = CARTESIAN_POINT ( 'NONE',  ( -1.513652225697619480, 19.20845123580577862, -36.54854460006156103 ) ) ;
#691 = CARTESIAN_POINT ( 'NONE',  ( 22.84901343360919768, -14.12476282708878372, -66.77701941837864297 ) ) ;
#692 = CARTESIAN_POINT ( 'NONE',  ( 8.803322232233091071, -63.21315167929310519, -46.67017412665830278 ) ) ;
#693 = DIRECTION ( 'NONE',  ( 0.000000000000000000, 1.000000000000000000, 0.000000000000000000 ) ) ;
#694 = CARTESIAN_POINT ( 'NONE',  ( 51.88873324421900435, -49.34589961264539681, -77.07841372369080091 ) ) ;
#695 =( BOUNDED_CURVE ( )  B_SPLINE_CURVE ( 3, ( #42862, #34451, #14549, #46541 ),
 .UNSPECIFIED., .F., .T. ) 
 B_SPLINE_CURVE_WITH_KNOTS ( ( 4, 4 ),
 ( 5.229612381435808643, 5.497787143782143282 ),
 .UNSPECIFIED. ) 
 CURVE ( )  GEOMETRIC_REPRESENTATION_ITEM ( )  RATIONAL_B_SPLINE_CURVE ( ( 1.000000000000000000, 0.9940158321278117493, 0.9940158321278117493, 1.000000000000000000 ) ) 
 REPRESENTATION_ITEM ( '' )  );
#696 = ORIENTED_EDGE ( 'NONE', *, *, #45315, .F. ) ;
#697 = DIRECTION ( 'NONE',  ( 1.000000000000000000, 1.390415240674919644E-25, -1.562192859871379910E-09 ) ) ;
#698 = DIRECTION ( 'NONE',  ( 0.6888026391158329487, -0.7071067811865494601, 0.1598465650148944150 ) ) ;
#699 = DIRECTION ( 'NONE',  ( -1.000000000000000000, 9.391392475159538137E-33, -1.071169953407190059E-15 ) ) ;
#700 = CARTESIAN_POINT ( 'NONE',  ( 7.492845759203685674, -61.18022026567161475, -20.13893727953967172 ) ) ;
#701 = CARTESIAN_POINT ( 'NONE',  ( 23.59082625508080255, -13.17046693263549884, -59.91161365334649958 ) ) ;
#702 = ADVANCED_FACE ( 'NONE', ( #11811 ), #36152, .F. ) ;
#703 = DIRECTION ( 'NONE',  ( 1.000000000000000000, 0.000000000000000000, 0.000000000000000000 ) ) ;
#704 = EDGE_CURVE ( 'NONE', #47505, #49517, #4236, .T. ) ;
#705 = CARTESIAN_POINT ( 'NONE',  ( 43.17397272625170501, -43.29126248660180210, -4.721727401537160418 ) ) ;
#706 = CARTESIAN_POINT ( 'NONE',  ( 18.29473438519294604, -51.18612221100339355, -15.69049832779063536 ) ) ;
#707 = CARTESIAN_POINT ( 'NONE',  ( 57.41961387009129680, 13.88381105532070059, -17.68493601882729749 ) ) ;
#708 = DIRECTION ( 'NONE',  ( 0.000000000000000000, 0.000000000000000000, 1.000000000000000000 ) ) ;
#709 = CIRCLE ( 'NONE', #8266, 4.000000000000059508 ) ;
#710 = CARTESIAN_POINT ( 'NONE',  ( 63.77506981661740326, 1.028299550205570068, -69.77396888106839867 ) ) ;
#711 = DIRECTION ( 'NONE',  ( 4.486507500526829843E-12, 3.054623595244970244E-12, -1.000000000000000000 ) ) ;
#712 = VECTOR ( 'NONE', #37434, 1000.000000000000114 ) ;
#713 = ORIENTED_EDGE ( 'NONE', *, *, #169, .F. ) ;
#714 = CARTESIAN_POINT ( 'NONE',  ( 14.63221749635400037, -52.02998614742870132, -75.83262351151711300 ) ) ;
#715 = CARTESIAN_POINT ( 'NONE',  ( 47.23936566397109971, -54.76392035971989714, -54.65942029303390370 ) ) ;
#716 = CARTESIAN_POINT ( 'NONE',  ( 14.06325258520262267, -7.911090401242016235, -36.92433639680130142 ) ) ;
#717 = CARTESIAN_POINT ( 'NONE',  ( 56.55522355860080097, -46.21195502513410247, -26.26695352263039851 ) ) ;
#718 = CARTESIAN_POINT ( 'NONE',  ( 9.366937397696199596, -15.61618894467949836, -28.45282021618999835 ) ) ;
#719 = CARTESIAN_POINT ( 'NONE',  ( 23.19722557037290045, -14.28277357378349954, -32.14999999999999858 ) ) ;
#720 = DIRECTION ( 'NONE',  ( 0.000000000000000000, -1.000000000000000000, 0.000000000000000000 ) ) ;
#721 = CARTESIAN_POINT ( 'NONE',  ( 62.09157612670949788, 4.883811055320659733, -65.34607522167520699 ) ) ;
#722 = CARTESIAN_POINT ( 'NONE',  ( 12.16981617636240109, -50.04926268091029584, -21.14999999999999858 ) ) ;
#723 = FACE_OUTER_BOUND ( 'NONE', #48146, .T. ) ;
#724 = CARTESIAN_POINT ( 'NONE',  ( 48.40030353798399432, 22.94693014320370139, -54.96840899516890033 ) ) ;
#725 = EDGE_LOOP ( 'NONE', ( #14856, #9355, #28472, #46085, #1468 ) ) ;
#726 = CARTESIAN_POINT ( 'NONE',  ( 10.90011346693460048, -20.34373019106079994, -67.61334385705760042 ) ) ;
#727 = VERTEX_POINT ( 'NONE', #23818 ) ;
#728 = LINE ( 'NONE', #25080, #19485 ) ;
#729 = DIRECTION ( 'NONE',  ( -1.000000000000000000, 0.000000000000000000, 0.000000000000000000 ) ) ;
#730 = CYLINDRICAL_SURFACE ( 'NONE', #6163, 6.766999999999998572 ) ;
#732 = CARTESIAN_POINT ( 'NONE',  ( 52.87209705597740594, 18.30414775337619915, -27.32974920830639931 ) ) ;
#731 = CARTESIAN_POINT ( 'NONE',  ( 84.16059178761608450, 12.81961614156949913, -47.12825410637790213 ) ) ;
#733 = CARTESIAN_POINT ( 'NONE',  ( 12.44997199531479914, -9.601959350568199270, -61.77788021779369387 ) ) ;
#734 = CARTESIAN_POINT ( 'NONE',  ( 10.87995435926834631, 33.74311107132334087, -17.51161114007551944 ) ) ;
#735 = CARTESIAN_POINT ( 'NONE',  ( 55.85381426216799383, -45.42888099847450434, -16.16583135229329926 ) ) ;
#736 = CARTESIAN_POINT ( 'NONE',  ( 24.04493742152532576, -16.65172855544441788, -79.83400040593491553 ) ) ;
#737 = ORIENTED_EDGE ( 'NONE', *, *, #29270, .F. ) ;
#738 = ADVANCED_FACE ( 'NONE', ( #19903 ), #8902, .F. ) ;
#739 = EDGE_LOOP ( 'NONE', ( #14867, #33257, #22548, #39008 ) ) ;
#740 = CARTESIAN_POINT ( 'NONE',  ( 11.60439326024719975, -64.93477792032190621, -16.46429631545650096 ) ) ;
#741 = CARTESIAN_POINT ( 'NONE',  ( 9.879544118219747872, 32.17924895645339944, -46.22143104348720044 ) ) ;
#742 = CARTESIAN_POINT ( 'NONE',  ( -5.866062602303799167, -15.61618894467929586, -11.65000000000000036 ) ) ;
#743 = CARTESIAN_POINT ( 'NONE',  ( 50.02329611982750635, -52.39131470799049595, -51.61201215204189907 ) ) ;
#744 = CARTESIAN_POINT ( 'NONE',  ( 24.04493742238449627, -16.65172779011892601, -63.54933673588272569 ) ) ;
#745 = AXIS2_PLACEMENT_3D ( 'NONE', #37331, #17418, #21326 ) ;
#746 = CIRCLE ( 'NONE', #22514, 6.099999999999994316 ) ;
#747 = AXIS2_PLACEMENT_3D ( 'NONE', #6843, #22792, #38812 ) ;
#748 = ORIENTED_EDGE ( 'NONE', *, *, #1783, .T. ) ;
#749 = DIRECTION ( 'NONE',  ( -0.000000000000000000, -1.000000000000000000, -0.000000000000000000 ) ) ;
#750 = CARTESIAN_POINT ( 'NONE',  ( 57.21905121524339677, 14.60424898410619932, -26.25836237551570207 ) ) ;
#751 = CARTESIAN_POINT ( 'NONE',  ( 53.64030340482580073, 18.11865384669719603, -49.15850183287659547 ) ) ;
#752 = CARTESIAN_POINT ( 'NONE',  ( 47.40322300430459990, 23.42336669154519768, -54.88279555090589668 ) ) ;
#753 = CARTESIAN_POINT ( 'NONE',  ( 50.61164247096510138, -50.32864445627969729, -76.14999999999999147 ) ) ;
#754 = CARTESIAN_POINT ( 'NONE',  ( 13.39998208309999939, 20.55440457967890211, -74.14999999999999147 ) ) ;
#755 = ORIENTED_EDGE ( 'NONE', *, *, #1133, .T. ) ;
#756 = B_SPLINE_CURVE_WITH_KNOTS ( 'NONE', 3,
 ( #30827, #46855, #26908, #42915, #7013, #22962, #44705, #23982, #31855, #12478, #16146, #48648, #5148, #16938, #51795, #8554, #20320 ),
 .UNSPECIFIED., .F., .F.,
 ( 4, 2, 1, 1, 1, 1, 1, 1, 1, 2, 2, 4 ),
 ( 0.000000000000000000, 0.2499999999999850120, 0.3749999999999775180, 0.4374999999999742428, 0.4687499999999726330, 0.4843749999999718003, 0.4921874999999713562, 0.4960937499999711897, 0.4980468749999710787, 0.4990234374999710232, 0.4999999999999710232, 1.000000000000000000 ),
 .UNSPECIFIED. ) ;
#757 = CARTESIAN_POINT ( 'NONE',  ( 16.13393739769620083, -15.61618894467929941, -10.44999999999999929 ) ) ;
#758 = DIRECTION ( 'NONE',  ( 0.3569024281753349626, 0.000000000000000000, 0.9341416684649872515 ) ) ;
#759 = ORIENTED_EDGE ( 'NONE', *, *, #38571, .T. ) ;
#760 = CARTESIAN_POINT ( 'NONE',  ( 56.46340970796750014, -50.48601309047270291, -52.83593731299979623 ) ) ;
#761 = CARTESIAN_POINT ( 'NONE',  ( 44.13393739769620083, 1.883811055320659955, -54.35294145922169662 ) ) ;
#762 = CARTESIAN_POINT ( 'NONE',  ( 7.893181483431141565, -15.34663001334440047, -76.80273986043728485 ) ) ;
#763 = CARTESIAN_POINT ( 'NONE',  ( 13.75277754671100006, -51.30789837932719877, -22.95878748375140077 ) ) ;
#764 = CARTESIAN_POINT ( 'NONE',  ( 22.90093739769620029, -15.61618894467913243, -28.45282021618999835 ) ) ;
#765 = EDGE_CURVE ( 'NONE', #26981, #3226, #22665, .T. ) ;
#766 = CARTESIAN_POINT ( 'NONE',  ( 47.50309824425850280, -54.59962336152860019, -74.17398805956220542 ) ) ;
#767 = ORIENTED_EDGE ( 'NONE', *, *, #26058, .T. ) ;
#768 = CYLINDRICAL_SURFACE ( 'NONE', #36235, 5.000000000000000000 ) ;
#769 = CARTESIAN_POINT ( 'NONE',  ( 23.36054005697790004, -17.42806857920490060, -66.31085317895978903 ) ) ;
#770 = DIRECTION ( 'NONE',  ( -1.000000000000000000, 0.000000000000000000, 0.000000000000000000 ) ) ;
#771 = CARTESIAN_POINT ( 'NONE',  ( 9.366937397696199596, -15.61618894467949836, -28.45282021618999835 ) ) ;
#772 = CARTESIAN_POINT ( 'NONE',  ( 47.16564561314290671, 23.08780115241070163, -75.35584192875380438 ) ) ;
#773 = CARTESIAN_POINT ( 'NONE',  ( 19.66714325812582942, -54.07769960979511836, -17.19998964887385995 ) ) ;
#774 = CARTESIAN_POINT ( 'NONE',  ( 0.08375394646315241498, 19.63944928676770019, -34.70982966457259522 ) ) ;
#775 = AXIS2_PLACEMENT_3D ( 'NONE', #12372, #28335, #4501 ) ;
#776 = DIRECTION ( 'NONE',  ( 0.8545454545454587159, -1.845195999999999228E-15, -0.5193766129849277657 ) ) ;
#777 = VECTOR ( 'NONE', #14475, 1000.000000000000000 ) ;
#779 = TOROIDAL_SURFACE ( 'NONE', #18371, 23.00000000000000000, 1.000000000000000000 ) ;
#778 = FACE_OUTER_BOUND ( 'NONE', #5985, .T. ) ;
#780 = DIRECTION ( 'NONE',  ( 1.000000000000000000, 2.460964292799963328E-14, 0.000000000000000000 ) ) ;
#782 = CARTESIAN_POINT ( 'NONE',  ( 30.64062214880055635, -35.66006875884785643, -84.61512769226293074 ) ) ;
#781 = CARTESIAN_POINT ( 'NONE',  ( 64.93393739769619799, 1.883811055320669947, -68.84999999999999432 ) ) ;
#783 = AXIS2_PLACEMENT_3D ( 'NONE', #43677, #40000, #12218 ) ;
#784 = CARTESIAN_POINT ( 'NONE',  ( 63.13475262569159696, 0.9955677559369519036, -68.95442834019429768 ) ) ;
#785 = CARTESIAN_POINT ( 'NONE',  ( 61.47583438558680058, 13.93519676881970071, -46.65924605088270027 ) ) ;
#786 = CARTESIAN_POINT ( 'NONE',  ( -29.90810223010410240, -36.12363263534039248, -56.68161292995529976 ) ) ;
#787 = ORIENTED_EDGE ( 'NONE', *, *, #16197, .F. ) ;
#788 = CARTESIAN_POINT ( 'NONE',  ( 53.39264886329749515, -49.37353566164819796, -48.88676049917400235 ) ) ;
#789 = CARTESIAN_POINT ( 'NONE',  ( 52.63393739706710051, -15.61618894417471104, 10.85000000030205669 ) ) ;
#790 = CARTESIAN_POINT ( 'NONE',  ( 24.01815955786813461, -16.28851273216530871, -65.81940510519697796 ) ) ;
#791 = CARTESIAN_POINT ( 'NONE',  ( 57.43883263735640554, 14.20764915532410022, -26.07839150191840005 ) ) ;
#792 = CARTESIAN_POINT ( 'NONE',  ( 13.77087701533600139, -22.26137549781239855, -37.06157372594439181 ) ) ;
#793 = CARTESIAN_POINT ( 'NONE',  ( 50.57709982134520033, 17.50796619428020406, -76.21964822811550277 ) ) ;
#794 = CARTESIAN_POINT ( 'NONE',  ( 52.90392156722190009, 18.39178596602710059, -48.79551525360960085 ) ) ;
#795 = CARTESIAN_POINT ( 'NONE',  ( 71.07527734533519492, 1.384447124000270035, -70.32375107525380997 ) ) ;
#796 = DIRECTION ( 'NONE',  ( 1.000000000000000000, 0.000000000000000000, 0.000000000000000000 ) ) ;
#797 = CARTESIAN_POINT ( 'NONE',  ( 87.61621807841599718, 17.38381105532069881, -61.12885639714370001 ) ) ;
#798 = ORIENTED_EDGE ( 'NONE', *, *, #51697, .F. ) ;
#799 = EDGE_CURVE ( 'NONE', #15443, #35304, #28536, .T. ) ;
#800 = CARTESIAN_POINT ( 'NONE',  ( 22.90090027005575379, -15.64040245347762870, -40.45396332187905131 ) ) ;
#801 = CARTESIAN_POINT ( 'NONE',  ( 10.94036863195580089, -20.95786825121460240, -61.81286799887340067 ) ) ;
#802 = B_SPLINE_CURVE_WITH_KNOTS ( 'NONE', 3,
 ( #21670, #32685, #734, #48979, #33479, #33731, #45550, #45033, #37423, #9645, #1779, #41608, #1267, #49236, #24829, #12816, #13834, #9133 ),
 .UNSPECIFIED., .F., .F.,
 ( 4, 2, 2, 2, 2, 2, 2, 2, 4 ),
 ( 0.000000000000000000, 0.03292105691051003952, 0.2434313698576751894, 0.3750003154496525659, 0.5000002523597224524, 0.5625002208147573679, 0.6625001703428121669, 0.8225000895877013773, 1.000000000000000000 ),
 .UNSPECIFIED. ) ;
#803 = CARTESIAN_POINT ( 'NONE',  ( 72.97593009921529017, 1.263903724274369811, -68.92034810279041324 ) ) ;
#804 = CARTESIAN_POINT ( 'NONE',  ( 47.49204623235880263, -54.60559727471500224, -54.98543878004470287 ) ) ;
#805 = LINE ( 'NONE', #16806, #569 ) ;
#806 = CARTESIAN_POINT ( 'NONE',  ( 18.20779226974428511, -12.71339276770203419, -643.2998782751060389 ) ) ;
#808 = ADVANCED_FACE ( 'NONE', ( #4964 ), #20932, .T. ) ;
#807 = CARTESIAN_POINT ( 'NONE',  ( 71.22849534471220068, 1.384708701328909886, -60.99162623037230446 ) ) ;
#809 = CARTESIAN_POINT ( 'NONE',  ( 71.33393739769628894, 11.23736444591397543, -61.59644660940672622 ) ) ;
#810 = CARTESIAN_POINT ( 'NONE',  ( 71.79351670693411336, 0.9755120847784399807, -60.89440987841059894 ) ) ;
#811 = CARTESIAN_POINT ( 'NONE',  ( 24.04492190258993389, -15.63236072556031075, -71.50832317379786218 ) ) ;
#812 = EDGE_CURVE ( 'NONE', #15276, #40924, #12511, .T. ) ;
#813 = CARTESIAN_POINT ( 'NONE',  ( 64.99546124159368787, 0.9209567800143640959, -70.76376997076650355 ) ) ;
#814 = VERTEX_POINT ( 'NONE', #46105 ) ;
#815 = ORIENTED_EDGE ( 'NONE', *, *, #42486, .F. ) ;
#816 = CARTESIAN_POINT ( 'NONE',  ( 72.33393739769579156, 10.88381105532070059, -62.44999999999859597 ) ) ;
#817 = DIRECTION ( 'NONE',  ( 0.000000000000000000, 0.000000000000000000, -1.000000000000000000 ) ) ;
#818 = ORIENTED_EDGE ( 'NONE', *, *, #24467, .F. ) ;
#819 = CARTESIAN_POINT ( 'NONE',  ( 9.464122031033584292, -13.86995827888586419, -71.92931663830769651 ) ) ;
#820 = DIRECTION ( 'NONE',  ( 0.000000000000000000, -1.000000000000000000, 0.000000000000000000 ) ) ;
#821 = DIRECTION ( 'NONE',  ( 0.000000000000000000, 0.000000000000000000, -1.000000000000000000 ) ) ;
#822 = TOROIDAL_SURFACE ( 'NONE', #30097, 34.47562460986249988, 0.5000000000000000000 ) ;
#823 = CARTESIAN_POINT ( 'NONE',  ( 52.61122371366529649, 19.76723091249260023, -76.13271378951098711 ) ) ;
#824 = VECTOR ( 'NONE', #36277, 1000.000000000000000 ) ;
#825 = EDGE_LOOP ( 'NONE', ( #43165, #3802, #896, #30458 ) ) ;
#826 = DIRECTION ( 'NONE',  ( 1.430038757655089944E-15, 8.684364315601310195E-16, -1.000000000000000000 ) ) ;
#827 = CARTESIAN_POINT ( 'NONE',  ( 42.58169510332613328, 6.482798360464016696, -77.41114634390734750 ) ) ;
#828 = EDGE_CURVE ( 'NONE', #27219, #30000, #4327, .T. ) ;
#829 = CARTESIAN_POINT ( 'NONE',  ( 60.83513156569119928, 14.48683582043410034, -47.74920551991019835 ) ) ;
#830 = AXIS2_PLACEMENT_3D ( 'NONE', #20779, #32822, #5345 ) ;
#831 = B_SPLINE_SURFACE_WITH_KNOTS ( 'NONE', 3, 3, ( 
 ( #44153, #11940, #27897, #43900, #9557, #21322, #5113, #26029, #9814, #13748, #29702, #2205, #49142, #1684, #13999, #42039, #22099, #33895, #49396, #6140, #45194, #24983, #17412, #18182, #14258, #38108 ),
 ( #34148, #37327, #1427, #50161, #9035, #21067, #44935, #33113, #10068, #17924, #33381, #45713, #5630, #25508, #40998, #45456, #25766, #9306, #21579, #37067, #49906, #25253, #41514, #37850, #1165, #17162 ),
 ( #13238, #33641, #13495, #37578, #29189, #29958, #41256, #45976, #29451, #5367, #21843, #17671, #49657, #41773, #5876, #1946, #35195, #27074, #11110, #30997, #11366, #10332, #2981, #39145, #47276, #51198 ),
 ( #3502, #18437, #27329, #3238, #6657, #50934, #42826, #46764, #19471, #30742, #47023, #30483, #6920, #51453, #19213, #46504, #10851, #23131, #46245, #22360, #34675, #18697, #2726, #50675, #43082, #43335 ),
 ( #7427, #31246, #38633, #23376, #7173, #22617, #22873, #15292, #34933, #39400, #35458, #30226, #26293, #42302, #6401, #38364, #18955, #2457, #34414, #50425, #14514, #10595, #26549, #42565, #14773, #26813 ),
 ( #38893, #15030, #8642, #48478, #31505, #4706, #4970, #36663, #9164, #33250, #43588, #37453, #24594, #45062, #45326, #5241, #20674, #49010, #21193, #49266, #1299, #12845, #8908, #36405, #23636, #9431 ),
 ( #13361, #7692, #20415, #28803, #12579, #39652, #20938, #40607, #24858, #44804, #15548, #28544, #11621, #47524, #27584, #29320, #48742, #17032, #25380, #44542, #25119, #16761, #17289, #40866, #766, #32715 ),
 ( #41381, #37200, #36937, #5498, #16499, #4448, #1038, #21454, #510, #32451, #32983, #13115, #29066, #41130, #34543, #30607, #50027, #18566, #6522, #13615, #37711, #50294, #49775, #50546, #37974, #2073 ),
 ( #1552, #38490, #41905, #2326, #26156, #1810, #6005, #17790, #18052, #42166, #17540, #38234, #14637, #22225, #34017, #18300, #10714, #33763, #10459, #21703, #13868, #14120, #34271, #14382, #6266, #30347 ),
 ( #29824, #46371, #22484, #33510, #6787, #2591, #25634, #46628, #26670, #42691, #9930, #45842, #22740, #49524, #41638, #30086, #25892, #29576, #45582, #26413, #42432, #9676, #5747, #21964, #10197, #46111 ) ),
 .UNSPECIFIED., .F., .F., .F.,
 ( 4, 1, 1, 1, 1, 1, 1, 4 ),
 ( 4, 2, 2, 2, 2, 2, 2, 2, 2, 2, 2, 2, 4 ),
 ( 0.000000000000000000, 0.1428571428571430157, 0.2857142857142860315, 0.4285714285714289917, 0.5714285714285709528, 0.7142857142857139685, 0.8571428571428569843, 1.000000000000000000 ),
 ( -6.280768244545899215, -5.577335479905130455, -4.969878459065930620, -4.447679305953560203, -3.925480152841189785, -3.140384122272949607, -2.747836106988829741, -2.273209145326620106, -1.893507575996860037, -1.513806006667089976, -0.9873533102557310315, -0.1450289959975500087, 0.000000000000000000 ),
 .UNSPECIFIED. ) ;
#832 = CARTESIAN_POINT ( 'NONE',  ( 22.58857181005839720, -20.74653149256879914, -44.00610240009889651 ) ) ;
#833 = CARTESIAN_POINT ( 'NONE',  ( 22.82184556707856871, -14.56300605882913324, -56.40312229056203819 ) ) ;
#834 = AXIS2_PLACEMENT_3D ( 'NONE', #41617, #26389, #38468 ) ;
#835 = CARTESIAN_POINT ( 'NONE',  ( 42.48963204042236441, -37.70124347511775653, -77.87149162280671533 ) ) ;
#836 = EDGE_CURVE ( 'NONE', #26710, #12957, #17026, .T. ) ;
#837 = ORIENTED_EDGE ( 'NONE', *, *, #30668, .T. ) ;
#838 = CARTESIAN_POINT ( 'NONE',  ( 11.79202694837120013, -65.42741386353530686, -22.35240830876180240 ) ) ;
#839 = CARTESIAN_POINT ( 'NONE',  ( 23.56125590958530225, -15.03169469483670007, -36.20765937478449814 ) ) ;
#840 = CARTESIAN_POINT ( 'NONE',  ( 41.30042210802800184, 14.36233479846170091, -6.243946835590840294 ) ) ;
#841 = CARTESIAN_POINT ( 'NONE',  ( 14.61074770980889959, 21.25914908875220277, -76.03975947796449475 ) ) ;
#842 = CARTESIAN_POINT ( 'NONE',  ( 24.04470022272198193, -15.61619473591594698, -59.79232576333501470 ) ) ;
#843 = CARTESIAN_POINT ( 'NONE',  ( 84.22920232233470017, -43.79788717120040076, -47.02060905303799387 ) ) ;
#844 = CARTESIAN_POINT ( 'NONE',  ( 11.09249001374801580, 33.92026773320360888, -17.64371731248376918 ) ) ;
#845 = EDGE_CURVE ( 'NONE', #16471, #16095, #2067, .T. ) ;
#846 = CARTESIAN_POINT ( 'NONE',  ( 8.679101862113558497, -12.09366884588789937, -54.64817642206789827 ) ) ;
#847 = ORIENTED_EDGE ( 'NONE', *, *, #20418, .F. ) ;
#848 = CARTESIAN_POINT ( 'NONE',  ( 53.95086563731030083, -48.56598208401319994, -26.86748755849900050 ) ) ;
#849 = CARTESIAN_POINT ( 'NONE',  ( 14.59756433005749976, -51.11618894047399664, -22.39374700643829996 ) ) ;
#850 = CARTESIAN_POINT ( 'NONE',  ( 50.91427647938718337, -35.37289624976227032, -76.35606773506994216 ) ) ;
#851 = CARTESIAN_POINT ( 'NONE',  ( 49.23286883301968686, 12.27403435862436076, -6.320887061515723992 ) ) ;
#852 = CARTESIAN_POINT ( 'NONE',  ( 9.458115080269156039, -13.90150626531904976, -55.92783392174342794 ) ) ;
#853 = CARTESIAN_POINT ( 'NONE',  ( 57.55751162087899786, 17.38381105532069881, -53.92796738110899923 ) ) ;
#854 =( GEOMETRIC_REPRESENTATION_CONTEXT ( 3 ) GLOBAL_UNCERTAINTY_ASSIGNED_CONTEXT ( ( #8008 ) ) GLOBAL_UNIT_ASSIGNED_CONTEXT ( ( #10591, #23128, #47273 ) ) REPRESENTATION_CONTEXT ( 'NONE', 'WORKASPACE' ) );
#855 = ORIENTED_EDGE ( 'NONE', *, *, #20913, .T. ) ;
#856 = AXIS2_PLACEMENT_3D ( 'NONE', #22499, #6022, #38511 ) ;
#857 =( BOUNDED_CURVE ( )  B_SPLINE_CURVE ( 3, ( #37730, #33264, #1828, #49540 ),
 .UNSPECIFIED., .F., .T. ) 
 B_SPLINE_CURVE_WITH_KNOTS ( ( 4, 4 ),
 ( 3.588596993660940093, 3.993185569951394953 ),
 .UNSPECIFIED. ) 
 CURVE ( )  GEOMETRIC_REPRESENTATION_ITEM ( )  RATIONAL_B_SPLINE_CURVE ( ( 1.000000000000000000, 0.9864054627567289124, 0.9864054627567289124, 1.000000000000000000 ) ) 
 REPRESENTATION_ITEM ( '' )  );
#858 = CARTESIAN_POINT ( 'NONE',  ( -10.40801357085099887, -42.82558555462620120, -6.134105759845330574 ) ) ;
#859 = CIRCLE ( 'NONE', #38507, 14.50000000000000178 ) ;
#860 = CARTESIAN_POINT ( 'NONE',  ( 47.36460231065780135, 23.44677451268669799, -54.83710734467110370 ) ) ;
#862 = TOROIDAL_SURFACE ( 'NONE', #18448, 2.500000000000000000, 0.5000000000000000000 ) ;
#861 = DIRECTION ( 'NONE',  ( 0.000000000000000000, 0.000000000000000000, -1.000000000000000000 ) ) ;
#863 = CARTESIAN_POINT ( 'NONE',  ( 63.13551795786779053, 1.096291039689149871, -62.40636042108670267 ) ) ;
#864 = CARTESIAN_POINT ( 'NONE',  ( 13.31438294250619947, 19.11297466560260361, -21.15359004513850039 ) ) ;
#865 = CARTESIAN_POINT ( 'NONE',  ( 68.13393739769790614, -49.95860450174320277, -71.35146707679190570 ) ) ;
#866 = CARTESIAN_POINT ( 'NONE',  ( 42.48652068188589936, 13.02449556106640038, -5.094659062314931042 ) ) ;
#867 = CARTESIAN_POINT ( 'NONE',  ( 45.14832757675640096, -33.29289077328009938, -35.14999999999999858 ) ) ;
#868 = CARTESIAN_POINT ( 'NONE',  ( 24.04493739769619864, -15.61618894467929941, -32.14999999999999858 ) ) ;
#869 = CARTESIAN_POINT ( 'NONE',  ( 25.83723722998072247, -15.61618894467929941, -22.14999999999999858 ) ) ;
#870 = CARTESIAN_POINT ( 'NONE',  ( 57.81670062735999949, -47.19152184943609996, -48.15401930624599913 ) ) ;
#871 = CARTESIAN_POINT ( 'NONE',  ( 14.33494800996290586, -22.21088556678449422, -67.03786065450826470 ) ) ;
#872 = CARTESIAN_POINT ( 'NONE',  ( 64.73967613295080525, 1.000225705806889964, -60.71075825745960231 ) ) ;
#873 = CARTESIAN_POINT ( 'NONE',  ( 17.80031357392610047, -52.43578441516969946, -75.98739629952659413 ) ) ;
#874 = EDGE_CURVE ( 'NONE', #24832, #9203, #1827, .T. ) ;
#875 = CARTESIAN_POINT ( 'NONE',  ( 19.54190971727932791, -21.52911178881554477, -60.78616782307490496 ) ) ;
#876 = CARTESIAN_POINT ( 'NONE',  ( 53.38983091188899266, 13.88381105532070059, -12.71718895241959935 ) ) ;
#877 = ORIENTED_EDGE ( 'NONE', *, *, #49208, .F. ) ;
#878 = DIRECTION ( 'NONE',  ( 0.000000000000000000, 1.000000000000000000, 0.000000000000000000 ) ) ;
#879 = CARTESIAN_POINT ( 'NONE',  ( 9.290087568746971058, 31.99567791594350297, -46.53000049651490144 ) ) ;
#880 = PLANE ( 'NONE',  #44373 ) ;
#881 = DIRECTION ( 'NONE',  ( -1.000000000000000000, 0.000000000000000000, 0.000000000000000000 ) ) ;
#882 = EDGE_CURVE ( 'NONE', #6987, #19003, #21862, .T. ) ;
#883 = EDGE_LOOP ( 'NONE', ( #14827, #681, #23999, #42091, #3747, #27412 ) ) ;
#884 = CARTESIAN_POINT ( 'NONE',  ( 18.01670405268210118, 20.49345067490170180, -75.53710645103458887 ) ) ;
#885 = VERTEX_POINT ( 'NONE', #37447 ) ;
#886 = ORIENTED_EDGE ( 'NONE', *, *, #11704, .T. ) ;
#887 = EDGE_LOOP ( 'NONE', ( #17457, #46801, #27829, #39812, #47372, #27144, #12308, #24981 ) ) ;
#888 = CARTESIAN_POINT ( 'NONE',  ( 10.30800061085760078, -63.35057298049469665, -45.84700176360160384 ) ) ;
#889 = CARTESIAN_POINT ( 'NONE',  ( 63.63393739769619373, 31.88381105532059934, 17.35000000000000142 ) ) ;
#890 = CARTESIAN_POINT ( 'NONE',  ( 20.73418997509670092, -20.86103424430950071, -81.23899999999999011 ) ) ;
#891 = CARTESIAN_POINT ( 'NONE',  ( 14.06331861277063666, -7.911073306414944994, -62.92433584427882209 ) ) ;
#892 = CARTESIAN_POINT ( 'NONE',  ( 61.57064344927020016, 13.99512139804009969, -47.02885309622070054 ) ) ;
#893 = EDGE_LOOP ( 'NONE', ( #27966, #19071, #32570, #8359 ) ) ;
#894 = ORIENTED_EDGE ( 'NONE', *, *, #30363, .F. ) ;
#895 = CARTESIAN_POINT ( 'NONE',  ( -28.43713041416928178, -60.18725675654477669, 17.35000000000000142 ) ) ;
#896 = ORIENTED_EDGE ( 'NONE', *, *, #47691, .T. ) ;
#897 = FACE_OUTER_BOUND ( 'NONE', #2547, .T. ) ;
#898 = CARTESIAN_POINT ( 'NONE',  ( 14.33740833808102266, -52.54004929525823542, -75.96019247807949171 ) ) ;
#899 = DIRECTION ( 'NONE',  ( 1.000000000000000000, 0.000000000000000000, 0.000000000000000000 ) ) ;
#901 = ORIENTED_EDGE ( 'NONE', *, *, #11130, .T. ) ;
#900 = PRODUCT_DEFINITION_FORMATION_WITH_SPECIFIED_SOURCE ( 'ANY', '', #35664, .NOT_KNOWN. ) ;
#902 = CIRCLE ( 'NONE', #46115, 16.50000000000000000 ) ;
#903 = ORIENTED_EDGE ( 'NONE', *, *, #44355, .T. ) ;
#904 = SPHERICAL_SURFACE ( 'NONE', #48457, 3.000000000000000000 ) ;
#905 = CARTESIAN_POINT ( 'NONE',  ( 11.22168610241799058, -65.22927118061893736, -17.68872724077263925 ) ) ;
#906 = AXIS2_PLACEMENT_3D ( 'NONE', #10117, #42084, #27124 ) ;
#907 = CARTESIAN_POINT ( 'NONE',  ( 60.33694438359629686, 14.62750282847430050, -47.70890968787150399 ) ) ;
#908 = CIRCLE ( 'NONE', #9309, 25.00000000000000000 ) ;
#909 = CARTESIAN_POINT ( 'NONE',  ( 51.32664003060159530, 13.97355598320289971, -12.12331377635689833 ) ) ;
#910 = CARTESIAN_POINT ( 'NONE',  ( 9.807807230283941635, -20.47791195640980533, -68.58399767422770310 ) ) ;
#911 = CARTESIAN_POINT ( 'NONE',  ( -2.623662902750090176, 17.43154064403359982, -4.296538304793199536 ) ) ;
#912 = CARTESIAN_POINT ( 'NONE',  ( 59.12150967144670233, 14.27486571672459981, -26.57366796877520088 ) ) ;
#913 = EDGE_CURVE ( 'NONE', #35517, #36938, #13355, .T. ) ;
#914 = CARTESIAN_POINT ( 'NONE',  ( 20.13079160575060200, -22.36984755485060106, -63.61740952279680528 ) ) ;
#915 = ORIENTED_EDGE ( 'NONE', *, *, #39393, .F. ) ;
#917 = EDGE_CURVE ( 'NONE', #26382, #7979, #49518, .T. ) ;
#916 = CARTESIAN_POINT ( 'NONE',  ( 18.11511214869369724, 1.359379830875159900, -35.01387690002259490 ) ) ;
#918 = CARTESIAN_POINT ( 'NONE',  ( -10.84475574424750022, -41.90441115894699919, -5.029302241765080339 ) ) ;
#919 = CARTESIAN_POINT ( 'NONE',  ( 12.39013027391890098, 34.14800971689950160, -46.54379730649250035 ) ) ;
#920 = CARTESIAN_POINT ( 'NONE',  ( 72.29200328562438926, 1.409763019284750118, -69.74012879731020575 ) ) ;
#921 = EDGE_CURVE ( 'NONE', #8004, #33885, #26864, .T. ) ;
#922 = CARTESIAN_POINT ( 'NONE',  ( 41.72973598950768093, -39.73518457503501367, -77.63497562485849812 ) ) ;
#923 = FACE_OUTER_BOUND ( 'NONE', #19528, .T. ) ;
#924 = CARTESIAN_POINT ( 'NONE',  ( 8.389157129729829521, -13.77808729393154685, -64.58170620237746107 ) ) ;
#925 = CARTESIAN_POINT ( 'NONE',  ( 47.20301239504629365, 23.55868320956959749, -74.19770771953690769 ) ) ;
#926 = CARTESIAN_POINT ( 'NONE',  ( 49.02351734455730536, -53.72042385326109581, -54.35736896012630126 ) ) ;
#927 = CARTESIAN_POINT ( 'NONE',  ( 16.13393739769620083, -15.61618894467929941, -11.54999999999999893 ) ) ;
#928 = CARTESIAN_POINT ( 'NONE',  ( 24.04493440204280574, -15.62413989401176373, -33.50798514483673785 ) ) ;
#929 = CARTESIAN_POINT ( 'NONE',  ( -21.36606260230379917, -63.11618894467929408, 16.35000000000000142 ) ) ;
#930 = PLANE ( 'NONE',  #31441 ) ;
#931 = ORIENTED_EDGE ( 'NONE', *, *, #23127, .F. ) ;
#932 = VECTOR ( 'NONE', #14664, 1000.000000000000000 ) ;
#933 = CARTESIAN_POINT ( 'NONE',  ( 12.08985222827440076, -9.359027489130609112, -44.38470316487709511 ) ) ;
#934 = CARTESIAN_POINT ( 'NONE',  ( 64.34567283584411257, 1.332297898506040079, -61.16569568407510360 ) ) ;
#935 = ORIENTED_EDGE ( 'NONE', *, *, #38697, .F. ) ;
#936 = CARTESIAN_POINT ( 'NONE',  ( 55.10455769617425403, -45.21089673182738267, -14.92011165637105918 ) ) ;
#937 = CONICAL_SURFACE ( 'NONE', #46980, 0.7350000000000003197, 0.06981317007977388966 ) ;
#938 = CARTESIAN_POINT ( 'NONE',  ( 60.93213094286049625, -45.54223981210000005, -47.50418379069640196 ) ) ;
#939 = DIRECTION ( 'NONE',  ( 6.938893903907222067E-15, 0.000000000000000000, -1.000000000000000000 ) ) ;
#940 = CARTESIAN_POINT ( 'NONE',  ( 50.93003717695669508, 19.69401293973280076, -76.14999999999999147 ) ) ;
#942 = CARTESIAN_POINT ( 'NONE',  ( 82.13853704237929776, -45.64188066427789892, -47.72348187592560009 ) ) ;
#941 = CARTESIAN_POINT ( 'NONE',  ( 42.56606161249485609, 8.591259806789389941, -73.59713884681082163 ) ) ;
#943 = CARTESIAN_POINT ( 'NONE',  ( 13.39998208309999939, 20.55440457967890211, -23.15000000000000213 ) ) ;
#944 = FACE_OUTER_BOUND ( 'NONE', #51750, .T. ) ;
#945 = EDGE_CURVE ( 'NONE', #47824, #22043, #25991, .T. ) ;
#946 = EDGE_LOOP ( 'NONE', ( #10571, #40119, #3556, #2907 ) ) ;
#947 = CARTESIAN_POINT ( 'NONE',  ( 84.08245047910018855, -44.49819807295929763, -47.41523600659849791 ) ) ;
#948 = ORIENTED_EDGE ( 'NONE', *, *, #16610, .T. ) ;
#949 = ORIENTED_EDGE ( 'NONE', *, *, #24161, .T. ) ;
#950 = ORIENTED_EDGE ( 'NONE', *, *, #33591, .F. ) ;
#951 = CARTESIAN_POINT ( 'NONE',  ( 61.46275447282020110, -45.32732362765139555, -47.26394423894119257 ) ) ;
#952 = CARTESIAN_POINT ( 'NONE',  ( 8.222946371911650232, -14.58057577448233033, -78.83399827190503117 ) ) ;
#953 = CARTESIAN_POINT ( 'NONE',  ( 76.44602326054074126, -6.632694491568091877, -12.99482443176448854 ) ) ;
#954 = CARTESIAN_POINT ( 'NONE',  ( 16.13393739769620083, -15.61618894467929941, -34.64999999999999858 ) ) ;
#955 = ORIENTED_EDGE ( 'NONE', *, *, #18756, .T. ) ;
#956 = ORIENTED_EDGE ( 'NONE', *, *, #9755, .F. ) ;
#957 = CARTESIAN_POINT ( 'NONE',  ( -0.1541415209190244717, 14.27647038466169072, -34.90033495507538674 ) ) ;
#958 = CARTESIAN_POINT ( 'NONE',  ( 22.47159906988888878, -10.82927912022386252, -77.30170387646415975 ) ) ;
#959 = CARTESIAN_POINT ( 'NONE',  ( 43.91475033527959937, -43.54611815821230891, -5.093413304872340674 ) ) ;
#960 = DIRECTION ( 'NONE',  ( 1.000000000000000000, 0.000000000000000000, 0.000000000000000000 ) ) ;
#961 = CARTESIAN_POINT ( 'NONE',  ( 63.88393739769619373, 4.883811055320659733, -61.44999999999999574 ) ) ;
#962 = CARTESIAN_POINT ( 'NONE',  ( 62.11841997430489926, -0.01765245207902430002, -16.72251539323920255 ) ) ;
#963 = CARTESIAN_POINT ( 'NONE',  ( 9.366931398960248956, -14.73043463447693213, -53.49448701394783967 ) ) ;
#964 = ORIENTED_EDGE ( 'NONE', *, *, #11171, .T. ) ;
#965 = CARTESIAN_POINT ( 'NONE',  ( 6.297163323809750857, 27.24491678059309407, -10.85005457635984882 ) ) ;
#966 = CARTESIAN_POINT ( 'NONE',  ( 9.026390854479029002, -47.84168788784550230, -54.64999999999999858 ) ) ;
#967 = CARTESIAN_POINT ( 'NONE',  ( 16.14243133923272566, -22.38318395068864675, -46.95242411700758112 ) ) ;
#968 = FACE_OUTER_BOUND ( 'NONE', #35369, .T. ) ;
#969 = CARTESIAN_POINT ( 'NONE',  ( 8.323089174469110674, -16.37605579175999893, -64.98162524141820029 ) ) ;
#970 = DIRECTION ( 'NONE',  ( 0.000000000000000000, 0.000000000000000000, -1.000000000000000000 ) ) ;
#971 = CARTESIAN_POINT ( 'NONE',  ( 42.86117915456519967, -43.50499890879240183, -4.698036889839340091 ) ) ;
#972 = CARTESIAN_POINT ( 'NONE',  ( 4.133937397696209715, -8.687985714403829718, -47.64999999999999858 ) ) ;
#973 = CARTESIAN_POINT ( 'NONE',  ( 67.04038824939736685, -50.70395984888064334, -74.34354914830332461 ) ) ;
#974 = CARTESIAN_POINT ( 'NONE',  ( 61.05708829393459780, -45.70443442833619940, -47.78546717324650217 ) ) ;
#975 = VECTOR ( 'NONE', #21208, 1000.000000000000000 ) ;
#976 = CARTESIAN_POINT ( 'NONE',  ( 64.23018683434881382, 1.404169013718219894, -69.96877364398430643 ) ) ;
#977 = CARTESIAN_POINT ( 'NONE',  ( 16.13393739769620083, -15.61618894467929941, -17.93019253464870033 ) ) ;
#978 = VECTOR ( 'NONE', #20340, 1000.000000000000114 ) ;
#979 = CARTESIAN_POINT ( 'NONE',  ( 66.61546637871180110, 0.7712952386763189949, -17.88089885441980087 ) ) ;
#980 = ORIENTED_EDGE ( 'NONE', *, *, #37134, .F. ) ;
#982 = ADVANCED_FACE ( 'NONE', ( #7292 ), #46621, .T. ) ;
#981 = CARTESIAN_POINT ( 'NONE',  ( 13.54479388721200017, -51.82694627962620615, -74.93568190819630104 ) ) ;
#983 = CARTESIAN_POINT ( 'NONE',  ( 47.35896996165279660, -54.68274079166319979, -54.83032919328549326 ) ) ;
#984 = EDGE_CURVE ( 'NONE', #15604, #20784, #5928, .T. ) ;
#985 = LINE ( 'NONE', #36352, #4641 ) ;
#986 = CARTESIAN_POINT ( 'NONE',  ( 22.89998285337925310, -16.42400860516817573, -76.88518437983843512 ) ) ;
#987 = CARTESIAN_POINT ( 'NONE',  ( 20.98660220077443839, -9.290834596779705024, -55.21623050661466436 ) ) ;
#988 = CARTESIAN_POINT ( 'NONE',  ( 22.44491825635649818, -19.88650245843829723, -32.14999999999999858 ) ) ;
#989 = FACE_OUTER_BOUND ( 'NONE', #29432, .T. ) ;
#990 = CARTESIAN_POINT ( 'NONE',  ( 47.81771439681010349, -54.40006451610999960, -54.73537641861789638 ) ) ;
#992 = CARTESIAN_POINT ( 'NONE',  ( 9.807852707146459181, -20.47797030866249912, -74.29933501067056056 ) ) ;
#991 = LINE ( 'NONE', #25333, #29805 ) ;
#993 = CARTESIAN_POINT ( 'NONE',  ( 56.40268793340759856, 19.51504490916650170, -53.40073823777059658 ) ) ;
#994 = CARTESIAN_POINT ( 'NONE',  ( 43.27084646106766996, 12.63989574180925324, -5.051381113503446763 ) ) ;
#995 = CARTESIAN_POINT ( 'NONE',  ( 48.58275665155029799, 22.89281328164460305, -55.12556760934580069 ) ) ;
#996 = ORIENTED_EDGE ( 'NONE', *, *, #27776, .F. ) ;
#997 = CARTESIAN_POINT ( 'NONE',  ( 21.69971205180370077, -19.94801438831689921, -59.05769930218669828 ) ) ;
#998 = VERTEX_POINT ( 'NONE', #10970 ) ;
#999 = CARTESIAN_POINT ( 'NONE',  ( 68.13393739769620083, 11.88381105532070059, -73.64407879467491114 ) ) ;
#1000 = CYLINDRICAL_SURFACE ( 'NONE', #37757, 0.4999999999999994449 ) ;
#1001 = CARTESIAN_POINT ( 'NONE',  ( 57.24718408831279959, -50.61618894896510312, -53.91456318529609604 ) ) ;
#1003 = CARTESIAN_POINT ( 'NONE',  ( 53.07092938598290033, 18.14261795147120182, -27.35050432211490090 ) ) ;
#1002 = CARTESIAN_POINT ( 'NONE',  ( 84.37258452300260103, 12.21853262853879940, -47.24504068948059654 ) ) ;
#1004 = CARTESIAN_POINT ( 'NONE',  ( 14.06839928245249993, -8.872591166704909327, -69.85821118628280146 ) ) ;
#1005 = CARTESIAN_POINT ( 'NONE',  ( 58.92073396209919878, -15.61618894467929941, -18.64999999999999858 ) ) ;
#1006 = CARTESIAN_POINT ( 'NONE',  ( 56.21699821026070509, -45.11618894467940066, -15.04108316657150013 ) ) ;
#1007 = EDGE_CURVE ( 'NONE', #9540, #40179, #42785, .T. ) ;
#1008 = CARTESIAN_POINT ( 'NONE',  ( 12.14991563812279907, -22.52877415440609354, -80.45899895091454823 ) ) ;
#1009 = VERTEX_POINT ( 'NONE', #14633 ) ;
#1010 = ADVANCED_FACE ( 'NONE', ( #34536 ), #42685, .T. ) ;
#1011 = ORIENTED_EDGE ( 'NONE', *, *, #6265, .F. ) ;
#1012 = CARTESIAN_POINT ( 'NONE',  ( 11.73339007446299931, -65.00805721967299178, -16.50122832064900180 ) ) ;
#1013 = CARTESIAN_POINT ( 'NONE',  ( 12.68175862228480177, 34.24734278266799947, -47.36921765020689890 ) ) ;
#1014 = CARTESIAN_POINT ( 'NONE',  ( 68.13393739769618662, -29.66618894467940137, -65.65000000000000568 ) ) ;
#1015 = AXIS2_PLACEMENT_3D ( 'NONE', #38013, #45883, #2108 ) ;
#1016 =( BOUNDED_CURVE ( )  B_SPLINE_CURVE ( 3, ( #5150, #1461, #12749, #13532 ),
 .UNSPECIFIED., .F., .T. ) 
 B_SPLINE_CURVE_WITH_KNOTS ( ( 4, 4 ),
 ( 1.570796326794890341, 2.356194490192361712 ),
 .UNSPECIFIED. ) 
 CURVE ( )  GEOMETRIC_REPRESENTATION_ITEM ( )  RATIONAL_B_SPLINE_CURVE ( ( 1.000000000000000000, 0.9492530216741881244, 0.9492530216741881244, 1.000000000000000000 ) ) 
 REPRESENTATION_ITEM ( '' )  );
#1017 = CARTESIAN_POINT ( 'NONE',  ( 48.01951627911569886, -54.26780672149330087, -54.65612569015529942 ) ) ;
#1018 = B_SPLINE_CURVE_WITH_KNOTS ( 'NONE', 3,
 ( #28435, #44435, #8543, #24487 ),
 .UNSPECIFIED., .F., .F.,
 ( 4, 4 ),
 ( 0.000000000000000000, 1.000000000000000000 ),
 .UNSPECIFIED. ) ;
#1019 = DIRECTION ( 'NONE',  ( -1.000000000000000000, -5.367253113454777116E-16, 0.000000000000000000 ) ) ;
#1020 = ORIENTED_EDGE ( 'NONE', *, *, #4336, .F. ) ;
#1021 = CARTESIAN_POINT ( 'NONE',  ( 68.13393739769618662, -28.80002732851770020, -29.09832030244573176 ) ) ;
#1022 = CARTESIAN_POINT ( 'NONE',  ( 52.83862607968303848, 18.42092619350584570, -28.03263386382830191 ) ) ;
#1023 = CARTESIAN_POINT ( 'NONE',  ( 68.13393739769620083, -48.11618894467930119, -76.75000000000000000 ) ) ;
#1024 = CARTESIAN_POINT ( 'NONE',  ( 16.13393739769620083, -15.61618894467929941, 7.530187386896120216 ) ) ;
#1025 = CARTESIAN_POINT ( 'NONE',  ( 72.06663613036050720, 1.456055805561079941, -69.85592311231539497 ) ) ;
#1027 = EDGE_CURVE ( 'NONE', #630, #27600, #34293, .T. ) ;
#1026 = CARTESIAN_POINT ( 'NONE',  ( 50.57758489713300065, -49.85242741362580432, -76.16361833591838604 ) ) ;
#1028 = DIRECTION ( 'NONE',  ( 0.5193766129849327617, -1.517977999999999440E-15, 0.8545454545454557183 ) ) ;
#1029 = ORIENTED_EDGE ( 'NONE', *, *, #45351, .T. ) ;
#1030 = CARTESIAN_POINT ( 'NONE',  ( 22.72481326017360104, -13.84495465653436774, -68.36948467987761546 ) ) ;
#1031 = CARTESIAN_POINT ( 'NONE',  ( 75.13393739769618662, 4.883811055320659733, -84.38499399519520239 ) ) ;
#1032 = ORIENTED_EDGE ( 'NONE', *, *, #49842, .F. ) ;
#1033 = CARTESIAN_POINT ( 'NONE',  ( 87.04559528857578243, -50.03040250705240055, -61.26127762739950811 ) ) ;
#1034 = CARTESIAN_POINT ( 'NONE',  ( 53.39341759735100368, -46.23760979563440543, -14.95068015331019851 ) ) ;
#1035 = CARTESIAN_POINT ( 'NONE',  ( 23.97401567591719740, -15.96280768448609955, -32.02654991895260395 ) ) ;
#1036 = CARTESIAN_POINT ( 'NONE',  ( 13.89448997836719890, -51.22164804421920081, -22.84403551404049892 ) ) ;
#1037 = CARTESIAN_POINT ( 'NONE',  ( 54.78125077669279364, 19.75549256766539941, -75.45543939936278832 ) ) ;
#1038 = CARTESIAN_POINT ( 'NONE',  ( 46.84429319214610388, -53.57519873512780606, -75.98322477344710535 ) ) ;
#1039 = EDGE_LOOP ( 'NONE', ( #45803, #13275, #26617, #7920 ) ) ;
#1040 = CARTESIAN_POINT ( 'NONE',  ( 64.93393739769619799, 11.38381105532070059, -62.44999999999999574 ) ) ;
#1041 = CARTESIAN_POINT ( 'NONE',  ( 57.12444643026329771, -50.61921117834419448, -53.89324253480139504 ) ) ;
#1042 = CARTESIAN_POINT ( 'NONE',  ( 22.90571047178250197, -13.64498330036649953, -32.75701418906499640 ) ) ;
#1043 = FACE_OUTER_BOUND ( 'NONE', #5297, .T. ) ;
#1045 = EDGE_CURVE ( 'NONE', #40975, #16369, #33519, .T. ) ;
#1044 = CARTESIAN_POINT ( 'NONE',  ( 46.79390132917320244, 22.44306139706349867, -75.96020792128800281 ) ) ;
#1046 = CARTESIAN_POINT ( 'NONE',  ( 10.85466640524320070, 33.73459223951330443, -17.55961383757199812 ) ) ;
#1047 = DIRECTION ( 'NONE',  ( 1.000000000000000000, 0.000000000000000000, 0.000000000000000000 ) ) ;
#1048 = VECTOR ( 'NONE', #44595, 1000.000000000000114 ) ;
#1049 = AXIS2_PLACEMENT_3D ( 'NONE', #35049, #51057, #39260 ) ;
#1050 = CYLINDRICAL_SURFACE ( 'NONE', #23550, 0.4999999999999994449 ) ;
#1051 = CARTESIAN_POINT ( 'NONE',  ( 15.88317419833548350, -49.61618860914077089, -83.24417156247753269 ) ) ;
#1052 = DIRECTION ( 'NONE',  ( 1.000000000000000000, 0.000000000000000000, 0.000000000000000000 ) ) ;
#1054 = CARTESIAN_POINT ( 'NONE',  ( 39.92856797414579262, -39.83700212839830357, -84.94016436021760796 ) ) ;
#1053 =( NAMED_UNIT ( * ) PLANE_ANGLE_UNIT ( ) SI_UNIT ( $, .RADIAN. ) );
#1055 = PLANE ( 'NONE',  #5926 ) ;
#1056 = CARTESIAN_POINT ( 'NONE',  ( 6.354289799260980587, -65.11185414427920648, -49.17526497145230735 ) ) ;
#1057 = ORIENTED_EDGE ( 'NONE', *, *, #16426, .F. ) ;
#1058 = CARTESIAN_POINT ( 'NONE',  ( 52.76678904663840086, -49.69688782720479736, -48.54391748749920055 ) ) ;
#1059 = CARTESIAN_POINT ( 'NONE',  ( 58.00948627897130194, -45.11615097667539942, -25.49324546217139797 ) ) ;
#1060 = CARTESIAN_POINT ( 'NONE',  ( 48.95357505128730224, -53.97596511168250544, -55.27962234102679417 ) ) ;
#1061 = CARTESIAN_POINT ( 'NONE',  ( 57.20888602249090127, 14.08682267489909989, -25.90208572559579991 ) ) ;
#1062 = CARTESIAN_POINT ( 'NONE',  ( 15.91222836016400066, -22.66554379454339951, -38.96282807147130001 ) ) ;
#1063 = CARTESIAN_POINT ( 'NONE',  ( 50.57709999312739768, 17.38380754905400138, -76.21964823130210220 ) ) ;
#1064 = CARTESIAN_POINT ( 'NONE',  ( 52.65621920618569618, 18.54360875905199890, -48.47378032971769812 ) ) ;
#1065 = CARTESIAN_POINT ( 'NONE',  ( 71.03049636386479904, 1.383411777981069957, -70.37541122638330648 ) ) ;
#1066 = CARTESIAN_POINT ( 'NONE',  ( 46.90960454922193890, 22.37535576646249424, -75.96332490880217847 ) ) ;
#1067 = ORIENTED_EDGE ( 'NONE', *, *, #20321, .T. ) ;
#1068 = CARTESIAN_POINT ( 'NONE',  ( 9.533333296005068291, -19.07143420819970103, -75.91383772819759201 ) ) ;
#1069 = ORIENTED_EDGE ( 'NONE', *, *, #44169, .F. ) ;
#1070 = EDGE_CURVE ( 'NONE', #22505, #43323, #43724, .T. ) ;
#1071 = CARTESIAN_POINT ( 'NONE',  ( 73.02743803608620965, 1.099344084866040072, -69.05806188122140554 ) ) ;
#1072 = CARTESIAN_POINT ( 'NONE',  ( 47.46325745728530165, -54.62024053978399962, -54.87604833503670676 ) ) ;
#1073 = CYLINDRICAL_SURFACE ( 'NONE', #49651, 16.00000000000000000 ) ;
#1074 = CARTESIAN_POINT ( 'NONE',  ( 73.00373354607030763, 1.334812829108570131, -62.63859554625260273 ) ) ;
#1075 = CARTESIAN_POINT ( 'NONE',  ( 4.133937397696209715, -8.687985714403829718, -47.64999999999999858 ) ) ;
#1076 = CARTESIAN_POINT ( 'NONE',  ( 52.87018954733399312, 18.40735846197139836, -48.66536493865070412 ) ) ;
#1077 = DIRECTION ( 'NONE',  ( 0.000000000000000000, 1.000000000000000000, 0.000000000000000000 ) ) ;
#1078 = CARTESIAN_POINT ( 'NONE',  ( 72.23968433060379368, 1.026088617261680103, -61.27424404961239901 ) ) ;
#1079 = CARTESIAN_POINT ( 'NONE',  ( -13.39236625349559873, -30.35380722911099838, -54.64999999999999858 ) ) ;
#1080 = CARTESIAN_POINT ( 'NONE',  ( 65.07863563811220331, 1.331842543267529821, -70.50106597067950531 ) ) ;
#1081 = VERTEX_POINT ( 'NONE', #51317 ) ;
#1082 = VERTEX_POINT ( 'NONE', #15414 ) ;
#1083 = CARTESIAN_POINT ( 'NONE',  ( 8.796734227443069543, -63.17759121671350186, -46.67028841929619887 ) ) ;
#1084 = DIRECTION ( 'NONE',  ( 1.000000000000000000, 0.000000000000000000, 0.000000000000000000 ) ) ;
#1085 = EDGE_LOOP ( 'NONE', ( #33468, #22180, #43746, #6700 ) ) ;
#1086 = CARTESIAN_POINT ( 'NONE',  ( 22.27312146484720046, -12.14444901143390076, -72.68335544512909507 ) ) ;
#1087 = DIRECTION ( 'NONE',  ( 0.000000000000000000, 0.000000000000000000, 1.000000000000000000 ) ) ;
#1088 = CARTESIAN_POINT ( 'NONE',  ( 14.04940779400430984, -9.151428043508968102, -49.85362723947532970 ) ) ;
#1089 = CARTESIAN_POINT ( 'NONE',  ( 52.53869629129660268, 19.33658919202579796, -76.53474691679770103 ) ) ;
#1090 = CIRCLE ( 'NONE', #16995, 23.50000000000000000 ) ;
#1091 = ORIENTED_EDGE ( 'NONE', *, *, #23754, .F. ) ;
#1092 = AXIS2_PLACEMENT_3D ( 'NONE', #37068, #29452, #29190 ) ;
#1093 = DIRECTION ( 'NONE',  ( 1.000000000000000000, 0.000000000000000000, 0.000000000000000000 ) ) ;
#1094 = CARTESIAN_POINT ( 'NONE',  ( 17.98749448546718455, 1.245406012443906807, -34.79644291222912500 ) ) ;
#1095 = DIRECTION ( 'NONE',  ( 1.000000000000000000, 0.000000000000000000, 0.000000000000000000 ) ) ;
#1096 = CARTESIAN_POINT ( 'NONE',  ( 13.31717580901180042, -23.36529045443169750, -52.40330909284259775 ) ) ;
#1097 = CARTESIAN_POINT ( 'NONE',  ( 22.90039887029312737, -15.52396765975452908, -56.44848823407438232 ) ) ;
#1098 = CARTESIAN_POINT ( 'NONE',  ( 42.99289099728417085, -37.77664616342443082, -75.35523169207313288 ) ) ;
#1099 = ORIENTED_EDGE ( 'NONE', *, *, #24455, .T. ) ;
#1100 = CARTESIAN_POINT ( 'NONE',  ( 11.38296080374989927, -63.50148532158249282, -24.39902340605380004 ) ) ;
#1101 = CARTESIAN_POINT ( 'NONE',  ( 22.83083802998899969, -12.35110237284849966, -32.08827495947629416 ) ) ;
#1102 = CARTESIAN_POINT ( 'NONE',  ( 16.13393739769620083, -15.61618894467929941, -9.721247897589949005 ) ) ;
#1103 = AXIS2_PLACEMENT_3D ( 'NONE', #43812, #16805, #7910 ) ;
#1104 = EDGE_CURVE ( 'NONE', #41238, #12186, #39011, .T. ) ;
#1105 = CARTESIAN_POINT ( 'NONE',  ( 14.35648533949829897, 20.67521890232639947, -75.71427953954510315 ) ) ;
#1106 = EDGE_CURVE ( 'NONE', #14173, #483, #41913, .T. ) ;
#1107 = CARTESIAN_POINT ( 'NONE',  ( 23.97380802304540737, -16.70946919957393106, -59.83642518982571090 ) ) ;
#1108 = ADVANCED_FACE ( 'NONE', ( #35047, #10710 ), #26663, .T. ) ;
#1109 = CARTESIAN_POINT ( 'NONE',  ( 83.45566905280610115, -44.67438416926519551, -46.48561260377719861 ) ) ;
#1110 = EDGE_CURVE ( 'NONE', #11008, #14401, #41834, .T. ) ;
#1111 = CARTESIAN_POINT ( 'NONE',  ( 9.466508518632270608, -10.76561033469889850, -56.70786862972200026 ) ) ;
#1112 = ORIENTED_EDGE ( 'NONE', *, *, #13564, .T. ) ;
#1113 = CARTESIAN_POINT ( 'NONE',  ( 53.29233422487229888, -49.24065040618290112, -27.36763233434339782 ) ) ;
#1114 = CARTESIAN_POINT ( 'NONE',  ( 16.65429250103910164, -51.11618894347319753, -20.30769847209390022 ) ) ;
#1115 = DIRECTION ( 'NONE',  ( 1.000000000000000000, 0.000000000000000000, 0.000000000000000000 ) ) ;
#1116 = CARTESIAN_POINT ( 'NONE',  ( 9.852065557373178351, -12.47056568813226107, -69.99514707462319052 ) ) ;
#1117 = CARTESIAN_POINT ( 'NONE',  ( 83.89200044194980421, 17.38381105532069881, -53.92796738110899923 ) ) ;
#1118 = AXIS2_PLACEMENT_3D ( 'NONE', #6228, #14083, #30044 ) ;
#1119 = ORIENTED_EDGE ( 'NONE', *, *, #22600, .T. ) ;
#1120 = CARTESIAN_POINT ( 'NONE',  ( -3.322299359250789674, -48.33316442662350454, -4.794339771350640156 ) ) ;
#1121 = AXIS2_PLACEMENT_3D ( 'NONE', #26654, #30332, #31102 ) ;
#1122 = CARTESIAN_POINT ( 'NONE',  ( 47.25269221664989772, 23.52078290745969724, -54.62328044731309973 ) ) ;
#1123 = PLANE ( 'NONE',  #43774 ) ;
#1124 = CARTESIAN_POINT ( 'NONE',  ( 63.50390619396998915, 1.388715606738730068, -62.57493595107060713 ) ) ;
#1125 = DIRECTION ( 'NONE',  ( 0.000000000000000000, 0.000000000000000000, 1.000000000000000000 ) ) ;
#1126 = CARTESIAN_POINT ( 'NONE',  ( 10.86720897088950011, 33.73900725339469631, -17.53558621447849930 ) ) ;
#1127 = DIRECTION ( 'NONE',  ( -0.3863301728269291635, 0.9223605572461970326, 0.000000000000000000 ) ) ;
#1128 = CARTESIAN_POINT ( 'NONE',  ( 53.63393739769619373, -62.11618894467930119, 11.84999999999999964 ) ) ;
#1129 = CARTESIAN_POINT ( 'NONE',  ( 71.83998266832981017, 1.442158793902750036, -61.28605443723469648 ) ) ;
#1130 = CARTESIAN_POINT ( 'NONE',  ( 56.66108174125150043, -47.79774483192920087, -48.40197048052689865 ) ) ;
#1131 = CARTESIAN_POINT ( 'NONE',  ( 52.82976730393809817, 18.42853680774779690, -28.15002497595520126 ) ) ;
#1132 = CARTESIAN_POINT ( 'NONE',  ( 52.73680207265829978, 20.85125113597840141, -53.40499982253649591 ) ) ;
#1133 = EDGE_CURVE ( 'NONE', #17335, #39508, #35624, .T. ) ;
#1134 = CARTESIAN_POINT ( 'NONE',  ( 22.90093737924810569, -16.50198979217266171, -60.49448455657499579 ) ) ;
#1135 = CARTESIAN_POINT ( 'NONE',  ( 21.54529342003797154, -11.45756571115651745, -48.24448846502571087 ) ) ;
#1136 = VERTEX_POINT ( 'NONE', #44213 ) ;
#1137 = CARTESIAN_POINT ( 'NONE',  ( -0.2550193211043536579, -10.79508889112895176, -34.98823006203678432 ) ) ;
#1138 = CARTESIAN_POINT ( 'NONE',  ( 10.14269527681349992, 32.00387675655870368, -45.99343597682049989 ) ) ;
#1139 = DIRECTION ( 'NONE',  ( -1.000000000000000000, 0.000000000000000000, 0.000000000000000000 ) ) ;
#1140 = CARTESIAN_POINT ( 'NONE',  ( 67.02524171442360057, -29.91412924832570042, -17.24420288053820016 ) ) ;
#1141 = ORIENTED_EDGE ( 'NONE', *, *, #24172, .F. ) ;
#1142 = CARTESIAN_POINT ( 'NONE',  ( 17.94181465708570045, 20.01251569944690090, -74.87640169473949925 ) ) ;
#1143 = ORIENTED_EDGE ( 'NONE', *, *, #5904, .T. ) ;
#1144 = EDGE_LOOP ( 'NONE', ( #12960, #15336, #21444, #25660, #40732 ) ) ;
#1145 = CARTESIAN_POINT ( 'NONE',  ( 47.68999173674550462, 23.28182553471719984, -55.17369749140770097 ) ) ;
#1146 = VERTEX_POINT ( 'NONE', #43704 ) ;
#1147 = CARTESIAN_POINT ( 'NONE',  ( 10.51296283413299903, -64.44909923135459451, -46.46298057769340062 ) ) ;
#1148 = CARTESIAN_POINT ( 'NONE',  ( 57.12778779988809674, -45.34015298987380049, -25.89881448804210251 ) ) ;
#1149 = CARTESIAN_POINT ( 'NONE',  ( 19.95187633256550086, -21.36878654213050055, -81.23899999999999011 ) ) ;
#1150 = CARTESIAN_POINT ( 'NONE',  ( 61.57131126144769695, 13.93819913114500153, -46.80234620618990249 ) ) ;
#1151 = CARTESIAN_POINT ( 'NONE',  ( 64.83819905826869956, 1.404650034021960092, -61.09597217184949614 ) ) ;
#1152 = ORIENTED_EDGE ( 'NONE', *, *, #30983, .T. ) ;
#1153 = EDGE_CURVE ( 'NONE', #21674, #36323, #43957, .T. ) ;
#1154 = DIRECTION ( 'NONE',  ( 0.000000000000000000, -1.000000000000000000, 0.000000000000000000 ) ) ;
#1155 = DIRECTION ( 'NONE',  ( -1.000000000000000000, 0.000000000000000000, 0.000000000000000000 ) ) ;
#1156 = ORIENTED_EDGE ( 'NONE', *, *, #45674, .T. ) ;
#1157 = CARTESIAN_POINT ( 'NONE',  ( 51.67634973896889505, -45.99404415929730305, -13.53858448670719916 ) ) ;
#1158 = LINE ( 'NONE', #41768, #48093 ) ;
#1159 = AXIS2_PLACEMENT_3D ( 'NONE', #40714, #49114, #17132 ) ;
#1160 = DIRECTION ( 'NONE',  ( -2.217154000000000151E-17, -9.040936000000000316E-17, 1.000000000000000000 ) ) ;
#1161 = ORIENTED_EDGE ( 'NONE', *, *, #38814, .F. ) ;
#1162 = VERTEX_POINT ( 'NONE', #4379 ) ;
#1163 = DIRECTION ( 'NONE',  ( 0.000000000000000000, 0.000000000000000000, -1.000000000000000000 ) ) ;
#1165 = CARTESIAN_POINT ( 'NONE',  ( 47.20319696544930110, -54.79145866998830172, -74.17413012813480577 ) ) ;
#1164 = CIRCLE ( 'NONE', #51377, 1.999999999999999556 ) ;
#1166 = CARTESIAN_POINT ( 'NONE',  ( 73.28401566534610367, 12.46528443789909879, -12.81730577991920050 ) ) ;
#1167 = CARTESIAN_POINT ( 'NONE',  ( 53.12059660037449760, -49.56856005606769600, -49.12440250185819934 ) ) ;
#1168 = B_SPLINE_CURVE_WITH_KNOTS ( 'NONE', 3,
 ( #28138, #20529, #8502, #4559 ),
 .UNSPECIFIED., .F., .F.,
 ( 4, 4 ),
 ( 0.000000000000000000, 1.000000000000000000 ),
 .UNSPECIFIED. ) ;
#1169 = CARTESIAN_POINT ( 'NONE',  ( 22.90080846266944548, -15.61618871746016879, -44.84718732428002852 ) ) ;
#1170 = CARTESIAN_POINT ( 'NONE',  ( 23.04646694808121410, -19.60030851528551210, -67.95899617219959055 ) ) ;
#1171 = CARTESIAN_POINT ( 'NONE',  ( -6.895251857565479980, 14.63674971373709965, -5.069369356803940185 ) ) ;
#1172 = CARTESIAN_POINT ( 'NONE',  ( 22.90117443638819239, -15.61618876209028528, -62.84717844892357164 ) ) ;
#1173 = CARTESIAN_POINT ( 'NONE',  ( 61.34394966329610099, 13.89927047214030154, -27.35702754952210114 ) ) ;
#1174 = EDGE_CURVE ( 'NONE', #7868, #5274, #3430, .T. ) ;
#1175 = CARTESIAN_POINT ( 'NONE',  ( 10.99779310440810143, -21.54971824701760497, -72.01461621554039993 ) ) ;
#1176 = ORIENTED_EDGE ( 'NONE', *, *, #35132, .T. ) ;
#1177 = CARTESIAN_POINT ( 'NONE',  ( 53.43679795862760074, 18.11049644000969749, -48.83615822496579995 ) ) ;
#1178 = CIRCLE ( 'NONE', #11219, 5.999999999999998224 ) ;
#1179 = CARTESIAN_POINT ( 'NONE',  ( -9.920770761350539146, -43.31452625206590312, -5.970037222519819942 ) ) ;
#1180 = FACE_OUTER_BOUND ( 'NONE', #24859, .T. ) ;
#1181 = CARTESIAN_POINT ( 'NONE',  ( 72.54418616719020463, 1.434949534324099885, -69.27291511353429598 ) ) ;
#1182 = FACE_OUTER_BOUND ( 'NONE', #28159, .T. ) ;
#1183 = ADVANCED_FACE ( 'NONE', ( #23758 ), #7621, .F. ) ;
#1184 = FACE_OUTER_BOUND ( 'NONE', #22076, .T. ) ;
#1185 = CARTESIAN_POINT ( 'NONE',  ( 47.06490539288780184, 23.30732543520909772, -75.17786433282310554 ) ) ;
#1186 = CARTESIAN_POINT ( 'NONE',  ( 49.02675822138120054, -53.86209816185859722, -54.70857181914429646 ) ) ;
#1187 = CARTESIAN_POINT ( 'NONE',  ( 41.93138893772210452, -44.52284172065920131, -5.197898045262170363 ) ) ;
#1188 = AXIS2_PLACEMENT_3D ( 'NONE', #30496, #50437, #50946 ) ;
#1189 = CARTESIAN_POINT ( 'NONE',  ( 23.98466744169371978, -16.62257527342094576, -33.54825124114566393 ) ) ;
#1190 = DIRECTION ( 'NONE',  ( 0.000000000000000000, 0.000000000000000000, -1.000000000000000000 ) ) ;
#1192 = EDGE_CURVE ( 'NONE', #36035, #22605, #51866, .T. ) ;
#1191 = CARTESIAN_POINT ( 'NONE',  ( 22.90068744318051586, -15.61618870719606278, -70.84718393407784731 ) ) ;
#1193 = ORIENTED_EDGE ( 'NONE', *, *, #2776, .F. ) ;
#1194 = CARTESIAN_POINT ( 'NONE',  ( 20.37871476403569915, -21.73897911326690036, -41.37438378445959586 ) ) ;
#1195 = CARTESIAN_POINT ( 'NONE',  ( 64.45537117179310371, 1.245299373075330118, -61.01735943755249991 ) ) ;
#1196 = VERTEX_POINT ( 'NONE', #34146 ) ;
#1197 = CARTESIAN_POINT ( 'NONE',  ( 85.66799001034409855, 19.38381105532069881, -61.58097075742929860 ) ) ;
#1198 = CARTESIAN_POINT ( 'NONE',  ( 60.82911148122739320, -45.58366361498899977, -47.52550039496580325 ) ) ;
#1199 = CARTESIAN_POINT ( 'NONE',  ( 56.93701001016370356, 19.40825549114710213, -53.86363390760720193 ) ) ;
#1200 = CARTESIAN_POINT ( 'NONE',  ( 12.69621344236849936, 18.74918026471999966, -21.09935757923890165 ) ) ;
#1202 = FACE_OUTER_BOUND ( 'NONE', #23308, .T. ) ;
#1201 = CARTESIAN_POINT ( 'NONE',  ( 44.85572791398350745, 8.787869211225075361, -62.51294508393674931 ) ) ;
#1203 = CARTESIAN_POINT ( 'NONE',  ( 52.03944403422909915, -51.37790098174010467, -75.97489327030881157 ) ) ;
#1204 = FACE_OUTER_BOUND ( 'NONE', #46556, .T. ) ;
#1205 = ORIENTED_EDGE ( 'NONE', *, *, #18866, .T. ) ;
#1206 = CARTESIAN_POINT ( 'NONE',  ( 84.25371145582080601, -44.18318432820999675, -47.43624648648039965 ) ) ;
#1207 = ORIENTED_EDGE ( 'NONE', *, *, #7215, .T. ) ;
#1208 = ORIENTED_EDGE ( 'NONE', *, *, #16789, .F. ) ;
#1209 = VERTEX_POINT ( 'NONE', #46762 ) ;
#1210 = CARTESIAN_POINT ( 'NONE',  ( 61.50405222244170034, -45.37411808438429262, -47.35446793284499734 ) ) ;
#1211 = CARTESIAN_POINT ( 'NONE',  ( 52.74431155066509547, -49.74087895501130419, -48.86925626324400440 ) ) ;
#1212 = CARTESIAN_POINT ( 'NONE',  ( 61.26174344272975958, 14.35308087949198708, -47.65928943619329061 ) ) ;
#1213 = DIRECTION ( 'NONE',  ( -1.451784999999999966E-10, 6.183944999999999577E-11, 1.000000000000000000 ) ) ;
#1214 = ORIENTED_EDGE ( 'NONE', *, *, #2608, .T. ) ;
#1215 = EDGE_CURVE ( 'NONE', #43941, #37382, #5116, .T. ) ;
#1216 = VERTEX_POINT ( 'NONE', #13042 ) ;
#1217 = DIRECTION ( 'NONE',  ( -0.8090169943749487835, -0.5877852522924713607, 0.000000000000000000 ) ) ;
#1218 = ORIENTED_EDGE ( 'NONE', *, *, #7596, .F. ) ;
#1219 = CARTESIAN_POINT ( 'NONE',  ( 56.74347695815399817, 19.18629571232069964, -52.86071028956509821 ) ) ;
#1220 = CARTESIAN_POINT ( 'NONE',  ( 20.63393739769620083, -41.61618894467930119, -34.64999999999999858 ) ) ;
#1221 = EDGE_CURVE ( 'NONE', #4288, #13029, #8048, .T. ) ;
#1222 = CARTESIAN_POINT ( 'NONE',  ( 14.16187783161290170, -50.35113599914600258, -20.85710678118659800 ) ) ;
#1223 = VECTOR ( 'NONE', #46761, 1000.000000000000000 ) ;
#1224 = CARTESIAN_POINT ( 'NONE',  ( 17.92370450339619836, 19.88381105532299742, -74.14999999999999147 ) ) ;
#1225 = LINE ( 'NONE', #20861, #8389 ) ;
#1226 = EDGE_LOOP ( 'NONE', ( #51735, #40981, #47829, #33821, #877, #37585, #23815, #23897, #32974, #29371 ) ) ;
#1227 = CARTESIAN_POINT ( 'NONE',  ( 57.49008833992955658, -50.10650853560072449, -52.59398466008588002 ) ) ;
#1228 = CARTESIAN_POINT ( 'NONE',  ( 51.81517742741720411, -50.18339821138420120, -76.50774528515320583 ) ) ;
#1229 = CARTESIAN_POINT ( 'NONE',  ( 22.90086341797264780, -15.61618933298137790, -46.45282805145726002 ) ) ;
#1230 = CARTESIAN_POINT ( 'NONE',  ( 14.19338055721680014, -32.55558437065590027, -34.90839531524139971 ) ) ;
#1231 = CARTESIAN_POINT ( 'NONE',  ( 17.24545617948280096, -23.38479715910980161, -68.46725820821738751 ) ) ;
#1232 = FACE_OUTER_BOUND ( 'NONE', #36716, .T. ) ;
#1233 = CARTESIAN_POINT ( 'NONE',  ( 45.06709565917970650, 13.92152238313070178, -7.502891261494740505 ) ) ;
#1234 = CIRCLE ( 'NONE', #12959, 9.768249999999998323 ) ;
#1235 = CARTESIAN_POINT ( 'NONE',  ( 41.93138893772210452, -44.52284172065920131, -5.197898045262170363 ) ) ;
#1236 = CARTESIAN_POINT ( 'NONE',  ( 72.31745269033760337, 1.031856533264720266, -61.34884692546020091 ) ) ;
#1237 = DIRECTION ( 'NONE',  ( -1.000000000000000000, 0.000000000000000000, 0.000000000000000000 ) ) ;
#1238 = AXIS2_PLACEMENT_3D ( 'NONE', #41872, #6756, #3080 ) ;
#1239 = ADVANCED_FACE ( 'NONE', ( #41062 ), #34410, .T. ) ;
#1240 = CARTESIAN_POINT ( 'NONE',  ( 64.07670260090860381, 1.019777262794749895, -70.07076857027371375 ) ) ;
#1241 = CARTESIAN_POINT ( 'NONE',  ( -23.86606260230380272, -15.61618894467908092, -53.92777777777782688 ) ) ;
#1242 = CARTESIAN_POINT ( 'NONE',  ( 65.61836598397030684, 0.5117851582676719024, -17.32554831824890229 ) ) ;
#1243 = ADVANCED_FACE ( 'NONE', ( #14771 ), #24019, .T. ) ;
#1244 = ORIENTED_EDGE ( 'NONE', *, *, #6440, .F. ) ;
#1245 = CARTESIAN_POINT ( 'NONE',  ( 13.87305293863050082, -51.45286096150079658, -74.99552951438440118 ) ) ;
#1246 = CARTESIAN_POINT ( 'NONE',  ( 57.28958349610260115, 19.33036382309920143, -53.44848231829909935 ) ) ;
#1247 = FACE_OUTER_BOUND ( 'NONE', #46803, .T. ) ;
#1248 = CARTESIAN_POINT ( 'NONE',  ( 83.71507592998568725, 13.22434697382143298, -46.59591546942163376 ) ) ;
#1249 = CARTESIAN_POINT ( 'NONE',  ( 24.04482276282174169, -15.57017577287801124, -55.50582115160575825 ) ) ;
#1250 = CARTESIAN_POINT ( 'NONE',  ( 22.52893251407120090, -12.64281036005729852, -32.14999999999999858 ) ) ;
#1251 = CARTESIAN_POINT ( 'NONE',  ( 57.35132949813925762, 14.51266520188007902, -26.25078878154161188 ) ) ;
#1252 = CARTESIAN_POINT ( 'NONE',  ( 47.69530821581999902, -54.51124612977650230, -55.10855014336240032 ) ) ;
#1253 = VECTOR ( 'NONE', #27515, 1000.000000000000114 ) ;
#1255 = CARTESIAN_POINT ( 'NONE',  ( 9.366602974803960535, -15.61605382581650048, -49.84717978381009118 ) ) ;
#1254 = CARTESIAN_POINT ( 'NONE',  ( 38.13393739769620083, -15.61618894467929941, -13.15000000000000036 ) ) ;
#1256 = CARTESIAN_POINT ( 'NONE',  ( 56.38979760733869995, 19.45007144631160045, -53.17790575662699837 ) ) ;
#1257 = CARTESIAN_POINT ( 'NONE',  ( 48.76650864246020234, 22.82327037976499895, -55.26805329862090588 ) ) ;
#1258 = ORIENTED_EDGE ( 'NONE', *, *, #24321, .T. ) ;
#1259 = CARTESIAN_POINT ( 'NONE',  ( 9.908454316688080965, -18.93069035251320287, -59.69145075069559425 ) ) ;
#1260 = ORIENTED_EDGE ( 'NONE', *, *, #31950, .T. ) ;
#1261 = CARTESIAN_POINT ( 'NONE',  ( 2.528703657258680515, -5.910750250813970652, -34.65800258959620095 ) ) ;
#1262 = CARTESIAN_POINT ( 'NONE',  ( 65.07026117056290104, 1.388189907116970101, -61.01613942410280345 ) ) ;
#1263 = FACE_OUTER_BOUND ( 'NONE', #41665, .T. ) ;
#1265 = CARTESIAN_POINT ( 'NONE',  ( 54.74050131502779948, 16.39029591686540144, -26.36129443285850016 ) ) ;
#1264 = CARTESIAN_POINT ( 'NONE',  ( 83.43488124258610128, 13.92192429134099996, -47.39353206303620425 ) ) ;
#1266 = CARTESIAN_POINT ( 'NONE',  ( 11.13117135703519978, -20.58759625438899832, -63.20382097693880041 ) ) ;
#1267 = CARTESIAN_POINT ( 'NONE',  ( 11.74347662707552153, 33.65273995683249808, -16.31133514116600125 ) ) ;
#1268 = CARTESIAN_POINT ( 'NONE',  ( 72.72759757326660690, 1.395196698723390138, -68.83033655198650536 ) ) ;
#1269 = B_SPLINE_SURFACE_WITH_KNOTS ( 'NONE', 3, 3, ( 
 ( #40469, #20277, #44928, #28659, #44663, #8767, #16363, #12972, #40733, #12436, #24717, #4831, #16894, #9029, #10325, #14249 ),
 ( #38103, #13487, #6394, #30219, #1157, #33375, #49135, #17153, #13233, #34142, #33633, #1936, #46238, #49391, #29953, #1679 ),
 ( #9807, #29446, #45451, #1420, #26022, #5869, #9552, #2199, #13994, #25756, #33889, #22090, #42034, #9298, #17666, #21836 ),
 ( #13742, #25503, #26286, #37843, #45706, #41767, #41250, #18175, #6133, #41508, #21575, #5620, #50154, #42294, #22354, #33106 ),
 ( #17918, #21318, #29184, #17406, #37571, #49899, #45968, #10061, #45185, #49650, #25248, #29695, #5362, #37319, #14506, #22863 ),
 ( #34404, #15286, #30476, #26543, #38884, #42558, #2717, #35188, #43329, #11356, #47269, #39139, #6649, #7168, #51192, #31240 ) ),
 .UNSPECIFIED., .F., .F., .F.,
 ( 4, 1, 1, 4 ),
 ( 4, 2, 2, 2, 2, 2, 2, 4 ),
 ( -7.901482146000000741E-06, 0.3333333333333329818, 0.6666666666666670737, 1.000000000266519917 ),
 ( -7.901482146000000741E-06, 2.041349754395100025, 4.374320902275219858, 5.832427869700300249, 6.561481353412840001, 7.727966927352889925, 9.594343845656990055, 11.66486364088270022 ),
 .UNSPECIFIED. ) ;
#1270 = DIRECTION ( 'NONE',  ( 1.000000000000000000, 0.000000000000000000, 0.000000000000000000 ) ) ;
#1271 = ORIENTED_EDGE ( 'NONE', *, *, #30459, .T. ) ;
#1272 = ORIENTED_EDGE ( 'NONE', *, *, #3205, .F. ) ;
#1273 = CARTESIAN_POINT ( 'NONE',  ( 12.08205748224309950, -65.27925620804988682, -16.92411159753779870 ) ) ;
#1274 = CARTESIAN_POINT ( 'NONE',  ( 12.89154239176200001, 34.27648701824740129, -47.61655765160880094 ) ) ;
#1275 = DIRECTION ( 'NONE',  ( -0.5720614028176828070, 0.4156269377774549079, -0.7071067811865477948 ) ) ;
#1276 = FACE_OUTER_BOUND ( 'NONE', #37122, .T. ) ;
#1277 = CARTESIAN_POINT ( 'NONE',  ( 51.45476138140149658, 3.156784108801740985, -76.74519123628812167 ) ) ;
#1278 = ORIENTED_EDGE ( 'NONE', *, *, #26962, .F. ) ;
#1279 = CARTESIAN_POINT ( 'NONE',  ( -18.95254157709769771, -32.86309081617850580, -51.24642923610910117 ) ) ;
#1280 = CARTESIAN_POINT ( 'NONE',  ( 59.49262858449159808, -50.48013859002959691, -53.20292136905285929 ) ) ;
#1281 = EDGE_CURVE ( 'NONE', #4886, #6632, #5540, .T. ) ;
#1282 = CARTESIAN_POINT ( 'NONE',  ( 13.55699286802090420, 20.68057025407604499, -75.01676221294341929 ) ) ;
#1283 = CARTESIAN_POINT ( 'NONE',  ( 14.13393739769649571, 3.536827985081051562, -43.67210484879171872 ) ) ;
#1284 = CYLINDRICAL_SURFACE ( 'NONE', #28414, 0.4999999999999983347 ) ;
#1285 = EDGE_CURVE ( 'NONE', #4176, #35594, #17330, .T. ) ;
#1286 = CARTESIAN_POINT ( 'NONE',  ( 22.37268434111649995, -53.60841447722789610, -34.64999999999999858 ) ) ;
#1287 = VERTEX_POINT ( 'NONE', #25162 ) ;
#1288 = CARTESIAN_POINT ( 'NONE',  ( 54.75911359420939561, -47.36916784795560176, -25.73144026446449928 ) ) ;
#1289 = CARTESIAN_POINT ( 'NONE',  ( 10.07017945894041944, 22.77497238916370748, -34.80997524099235818 ) ) ;
#1290 = VERTEX_POINT ( 'NONE', #1075 ) ;
#1291 = CARTESIAN_POINT ( 'NONE',  ( 9.807746736123759135, -10.75454355271028639, -53.00066549702621899 ) ) ;
#1292 = FACE_OUTER_BOUND ( 'NONE', #38022, .T. ) ;
#1293 = AXIS2_PLACEMENT_3D ( 'NONE', #39345, #27526, #11829 ) ;
#1294 = CARTESIAN_POINT ( 'NONE',  ( 17.58945275769320205, -7.904624730565840807, -37.57187509340590026 ) ) ;
#1295 = CARTESIAN_POINT ( 'NONE',  ( 52.88663104391009995, -49.66786150580319514, -48.99336411538499902 ) ) ;
#1296 = AXIS2_PLACEMENT_3D ( 'NONE', #24869, #13128, #25137 ) ;
#1297 = CARTESIAN_POINT ( 'NONE',  ( 60.34379259250669492, 14.63564649040839960, -47.72732609510669732 ) ) ;
#1298 = CARTESIAN_POINT ( 'NONE',  ( 54.70440021269280351, 19.88794248854869906, -75.31486140208340885 ) ) ;
#1299 = CARTESIAN_POINT ( 'NONE',  ( 47.39174436423379433, -54.56554572047070195, -74.72285389774751252 ) ) ;
#1300 = ORIENTED_EDGE ( 'NONE', *, *, #10372, .T. ) ;
#1301 = CARTESIAN_POINT ( 'NONE',  ( 55.96902517572589630, 14.60256971682040117, -17.77637908280700429 ) ) ;
#1302 = CARTESIAN_POINT ( 'NONE',  ( 57.00264675662779723, -50.63106778522559637, -53.72993499349190216 ) ) ;
#1303 = CARTESIAN_POINT ( 'NONE',  ( 52.56369620065810011, -49.86341771588610072, -48.47378032971909789 ) ) ;
#1304 = CARTESIAN_POINT ( 'NONE',  ( 21.99623050575979732, -19.53742327708049942, -37.03483646650040129 ) ) ;
#1305 = LINE ( 'NONE', #771, #12830 ) ;
#1306 = ADVANCED_FACE ( 'NONE', ( #5017 ), #28656, .T. ) ;
#1307 = AXIS2_PLACEMENT_3D ( 'NONE', #50998, #30544, #15617 ) ;
#1308 = VERTEX_POINT ( 'NONE', #21495 ) ;
#1309 = CARTESIAN_POINT ( 'NONE',  ( 46.71512400210709615, 22.30641209017640136, -76.02645024177060407 ) ) ;
#1310 = CARTESIAN_POINT ( 'NONE',  ( 65.07261215712630076, 1.274277262446069869, -60.70118609097839624 ) ) ;
#1311 = CARTESIAN_POINT ( 'NONE',  ( 41.38327847047529673, -45.62082798267930173, -6.314269469673459589 ) ) ;
#1312 = CARTESIAN_POINT ( 'NONE',  ( 12.32961272724990032, 33.41202109490849637, -15.85993007184249848 ) ) ;
#1313 = CARTESIAN_POINT ( 'NONE',  ( 8.058121637015549510, -13.95368465620019904, -78.57229360328089740 ) ) ;
#1314 = CARTESIAN_POINT ( 'NONE',  ( 60.31639983754979539, -45.83544975381219189, -47.65366050515983432 ) ) ;
#1316 = CARTESIAN_POINT ( 'NONE',  ( 16.13393739769620083, -15.61618894467929941, -28.45282021618999835 ) ) ;
#1315 = CARTESIAN_POINT ( 'NONE',  ( 24.04462826173309153, -15.61618628916268392, -33.50766512250601181 ) ) ;
#1317 = DIRECTION ( 'NONE',  ( 0.000000000000000000, 0.000000000000000000, -1.000000000000000000 ) ) ;
#1318 = CARTESIAN_POINT ( 'NONE',  ( 8.428832403331353973, -13.54552742703515911, -68.59100208448060698 ) ) ;
#1319 = CARTESIAN_POINT ( 'NONE',  ( -26.90058206776739880, -41.85481090454489816, -56.03720707547429924 ) ) ;
#1320 = ORIENTED_EDGE ( 'NONE', *, *, #330, .T. ) ;
#1321 =( BOUNDED_CURVE ( )  B_SPLINE_CURVE ( 3, ( #30585, #50783, #14615, #35565 ),
 .UNSPECIFIED., .F., .T. ) 
 B_SPLINE_CURVE_WITH_KNOTS ( ( 4, 4 ),
 ( 5.497787143782143282, 5.746835782486941824 ),
 .UNSPECIFIED. ) 
 CURVE ( )  GEOMETRIC_REPRESENTATION_ITEM ( )  RATIONAL_B_SPLINE_CURVE ( ( 1.000000000000000000, 0.9948379068877977183, 0.9948379068877977183, 1.000000000000000000 ) ) 
 REPRESENTATION_ITEM ( '' )  );
#1322 = CARTESIAN_POINT ( 'NONE',  ( 52.78519993256289666, -49.68938364784359152, -48.68758331618039392 ) ) ;
#1323 = CARTESIAN_POINT ( 'NONE',  ( 59.21978530496789972, -45.12527060529160394, -25.93003219259560055 ) ) ;
#1324 = CIRCLE ( 'NONE', #34746, 2.000000000000000000 ) ;
#1325 = CARTESIAN_POINT ( 'NONE',  ( 48.72504344960389489, -54.07331086023990707, -55.30415983355479881 ) ) ;
#1326 = CARTESIAN_POINT ( 'NONE',  ( 56.88551911260069716, 14.51619878703609956, -26.16768187466989559 ) ) ;
#1327 = CARTESIAN_POINT ( 'NONE',  ( 14.81228562542739979, -8.688288820165540827, -33.89281648339969166 ) ) ;
#1328 = CARTESIAN_POINT ( 'NONE',  ( 50.13210307260710152, 17.67415490553439739, -76.14999999999999147 ) ) ;
#1329 = CARTESIAN_POINT ( 'NONE',  ( 52.66273062025209839, 18.53842598467419833, -48.50781030805210037 ) ) ;
#1330 = CARTESIAN_POINT ( 'NONE',  ( 71.41555540048999262, 0.9948723650351710690, -70.66407068423170301 ) ) ;
#1331 = CARTESIAN_POINT ( 'NONE',  ( -0.03447620312152044342, -8.421650097910747590, -34.79644660940672196 ) ) ;
#1332 = CARTESIAN_POINT ( 'NONE',  ( 46.52565834994577898, 21.89345249407521621, -76.13734531344884715 ) ) ;
#1333 = TOROIDAL_SURFACE ( 'NONE', #50715, 1.499999999742110068, 0.4999999999874650269 ) ;
#1334 = EDGE_LOOP ( 'NONE', ( #1354, #15466, #17577, #13098, #33374 ) ) ;
#1335 = CARTESIAN_POINT ( 'NONE',  ( 10.29322140962580079, -20.24141662394440289, -73.85414552054359660 ) ) ;
#1336 = CARTESIAN_POINT ( 'NONE',  ( 73.05279713336409486, 1.186856010528209993, -68.92285061280580294 ) ) ;
#1337 = CARTESIAN_POINT ( 'NONE',  ( 47.40218600936929505, -54.65618228108590415, -54.84992837070570459 ) ) ;
#1338 = CARTESIAN_POINT ( 'NONE',  ( 14.81467456660999993, -7.815966731016759539, -81.23899999999999011 ) ) ;
#1339 = CARTESIAN_POINT ( 'NONE',  ( 68.13393739769618662, -1.166188944679350081, -40.64999999999999858 ) ) ;
#1340 = CARTESIAN_POINT ( 'NONE',  ( 60.25958433222680100, 14.85042903512990087, -48.01680402935890157 ) ) ;
#1341 = CARTESIAN_POINT ( 'NONE',  ( -31.86606260230380627, -15.61618894467930474, -76.14999999999999147 ) ) ;
#1342 = FACE_OUTER_BOUND ( 'NONE', #34261, .T. ) ;
#1343 = CARTESIAN_POINT ( 'NONE',  ( 71.81752115780599866, 1.390572245144489960, -61.18038351632199578 ) ) ;
#1344 = CARTESIAN_POINT ( 'NONE',  ( 14.13393739769619906, -45.61618894467940066, -49.33749999999999858 ) ) ;
#1345 = CARTESIAN_POINT ( 'NONE',  ( 64.95336252238109864, 1.097895768572089814, -70.68669971647908312 ) ) ;
#1346 = EDGE_LOOP ( 'NONE', ( #33772, #30629, #30206, #50001 ) ) ;
#1347 = CARTESIAN_POINT ( 'NONE',  ( 9.293307013010640105, -63.25115262801180194, -46.52992041538980317 ) ) ;
#1348 = ADVANCED_FACE ( 'NONE', ( #6049 ), #12789, .T. ) ;
#1349 = DIRECTION ( 'NONE',  ( 1.000000000000000000, 0.000000000000000000, 0.000000000000000000 ) ) ;
#1350 = VERTEX_POINT ( 'NONE', #10501 ) ;
#1351 = CARTESIAN_POINT ( 'NONE',  ( 14.36265541187617956, -9.025324658394913158, -69.86948818930653715 ) ) ;
#1352 = DIRECTION ( 'NONE',  ( 0.000000000000000000, 0.000000000000000000, 1.000000000000000000 ) ) ;
#1353 = CARTESIAN_POINT ( 'NONE',  ( 53.91131433573680454, 19.51725069840180282, -76.32773059538270388 ) ) ;
#1354 = ORIENTED_EDGE ( 'NONE', *, *, #2281, .F. ) ;
#1355 = CARTESIAN_POINT ( 'NONE',  ( 10.47406283454438203, 31.88305279702909800, -45.62066736167659542 ) ) ;
#1357 = CARTESIAN_POINT ( 'NONE',  ( 28.13393739769619728, -8.687985714403851034, -47.64999999999999858 ) ) ;
#1356 = AXIS2_PLACEMENT_3D ( 'NONE', #51549, #3598, #31601 ) ;
#1358 = CARTESIAN_POINT ( 'NONE',  ( 23.04645231909379888, -11.63204132127529888, -43.62568514326029856 ) ) ;
#1359 = CARTESIAN_POINT ( 'NONE',  ( 8.099657082704819544, -17.46904076716189991, -52.72018481709709903 ) ) ;
#1360 = CARTESIAN_POINT ( 'NONE',  ( 0.07463975747371710823, -20.73676263863309899, -34.71188928912349780 ) ) ;
#1361 = CARTESIAN_POINT ( 'NONE',  ( 42.35187137306987637, -37.67955064941986620, -78.56033206297207983 ) ) ;
#1362 = EDGE_LOOP ( 'NONE', ( #37307, #7671, #15273, #21352 ) ) ;
#1363 = CARTESIAN_POINT ( 'NONE',  ( 59.11315108609827007, -47.49289742320240038, -49.51859781974984998 ) ) ;
#1364 = CARTESIAN_POINT ( 'NONE',  ( 23.58352022967059725, -15.51416230748120029, -42.22829813561959611 ) ) ;
#1365 = CARTESIAN_POINT ( 'NONE',  ( 52.62851868536470334, -49.80923738442960769, -48.67162951074860189 ) ) ;
#1366 = CIRCLE ( 'NONE', #21432, 1.999999999999999778 ) ;
#1367 = CARTESIAN_POINT ( 'NONE',  ( 11.01954162827919959, -11.00411938779079968, -32.14999999999999858 ) ) ;
#1368 = EDGE_CURVE ( 'NONE', #36393, #16544, #23804, .T. ) ;
#1369 = AXIS2_PLACEMENT_3D ( 'NONE', #35812, #18788, #43171 ) ;
#1370 = EDGE_CURVE ( 'NONE', #38406, #50553, #31003, .T. ) ;
#1371 = CARTESIAN_POINT ( 'NONE',  ( 13.98848244166460120, 20.97417580057960151, -75.67041253543310120 ) ) ;
#1372 = CARTESIAN_POINT ( 'NONE',  ( 51.68229386154369820, 17.53316009977629975, -77.01557736631420426 ) ) ;
#1373 = LINE ( 'NONE', #13441, #5556 ) ;
#1374 = CARTESIAN_POINT ( 'NONE',  ( 17.58032879468959919, -7.498881962947089974, -53.06379780079550557 ) ) ;
#1375 = ORIENTED_EDGE ( 'NONE', *, *, #48401, .F. ) ;
#1376 = CARTESIAN_POINT ( 'NONE',  ( 55.61276803169860017, -46.45957139663980229, -25.89158459899769582 ) ) ;
#1377 = CARTESIAN_POINT ( 'NONE',  ( 14.04279605691000121, -50.94365768270629502, -21.72007173761920029 ) ) ;
#1378 = CARTESIAN_POINT ( 'NONE',  ( 11.93454077925219892, 32.88420340368310235, -15.38530629706399999 ) ) ;
#1379 = DIRECTION ( 'NONE',  ( 0.7071067811865475727, 0.000000000000000000, 0.7071067811865475727 ) ) ;
#1380 = CARTESIAN_POINT ( 'NONE',  ( -11.00461184790416524, -51.23639054309960983, -51.06967761013345353 ) ) ;
#1381 = EDGE_LOOP ( 'NONE', ( #21922, #21116, #28793, #39356 ) ) ;
#1382 = CARTESIAN_POINT ( 'NONE',  ( -8.382319638490058011, -44.65444820222590039, -5.282248192611979754 ) ) ;
#1383 = CARTESIAN_POINT ( 'NONE',  ( 47.23442391913490468, 23.53533408100059887, -54.66895834688099853 ) ) ;
#1384 = AXIS2_PLACEMENT_3D ( 'NONE', #341, #51214, #43856 ) ;
#1385 = CARTESIAN_POINT ( 'NONE',  ( 56.48539520774843226, -50.76770210929910832, -53.84780620286824160 ) ) ;
#1386 = CARTESIAN_POINT ( 'NONE',  ( 63.23977555071240175, 1.186515949276300219, -62.33540229050490211 ) ) ;
#1387 = CARTESIAN_POINT ( 'NONE',  ( 74.17629866868290378, -33.11618894467940066, -65.34607522167520699 ) ) ;
#1388 = CARTESIAN_POINT ( 'NONE',  ( 11.82896774831129960, 34.18482258325850154, -17.62577553875959779 ) ) ;
#1389 = CARTESIAN_POINT ( 'NONE',  ( -28.43713041416927467, 28.95487886718607129, 16.35000000000000142 ) ) ;
#1390 = CARTESIAN_POINT ( 'NONE',  ( 53.05372063824089679, 18.31120138125479713, -48.79446872373849686 ) ) ;
#1391 = CARTESIAN_POINT ( 'NONE',  ( 72.04429487089811346, 1.454949836291180132, -61.42720652002459758 ) ) ;
#1392 = CARTESIAN_POINT ( 'NONE',  ( 57.22322293371580315, -47.50141109488779989, -48.27531557238859961 ) ) ;
#1393 = CARTESIAN_POINT ( 'NONE',  ( 53.20717401374850652, 18.10213357476860097, -27.47939579088139794 ) ) ;
#1394 = CARTESIAN_POINT ( 'NONE',  ( 52.21238886552460201, 21.07428037441609803, -53.50655909053360659 ) ) ;
#1395 = CARTESIAN_POINT ( 'NONE',  ( 63.33722961565180043, 1.138495159512730170, -69.18058936015049198 ) ) ;
#1396 = CARTESIAN_POINT ( 'NONE',  ( 52.88720174365979432, 13.88381105532070059, -12.35033059909330078 ) ) ;
#1397 = ORIENTED_EDGE ( 'NONE', *, *, #19551, .F. ) ;
#1398 = FACE_OUTER_BOUND ( 'NONE', #43122, .T. ) ;
#1399 = CARTESIAN_POINT ( 'NONE',  ( 9.731815933137479391, 31.93091152407239619, -46.29980776193180247 ) ) ;
#1400 = AXIS2_PLACEMENT_3D ( 'NONE', #16334, #9264, #32287 ) ;
#1401 = CARTESIAN_POINT ( 'NONE',  ( 14.47161711077219870, -7.905140794172798024, -81.23899999999999011 ) ) ;
#1402 = ORIENTED_EDGE ( 'NONE', *, *, #47573, .T. ) ;
#1403 = CARTESIAN_POINT ( 'NONE',  ( 17.96427685920679806, 20.25300558755819935, -75.29799846200430125 ) ) ;
#1404 = CIRCLE ( 'NONE', #14796, 13.50000000000000178 ) ;
#1405 = ORIENTED_EDGE ( 'NONE', *, *, #32872, .F. ) ;
#1406 = VERTEX_POINT ( 'NONE', #6830 ) ;
#1407 = CARTESIAN_POINT ( 'NONE',  ( 9.807871516326736483, -20.47799444578012285, -80.29933555240771170 ) ) ;
#1408 = EDGE_CURVE ( 'NONE', #8663, #31302, #31927, .T. ) ;
#1409 = VERTEX_POINT ( 'NONE', #22781 ) ;
#1410 = CARTESIAN_POINT ( 'NONE',  ( 11.17576989425459999, -64.81915578497500974, -46.44971693985230132 ) ) ;
#1411 = CARTESIAN_POINT ( 'NONE',  ( 57.41360129382550070, -45.61097492619999372, -26.20065532981040235 ) ) ;
#1412 = CARTESIAN_POINT ( 'NONE',  ( 19.28358208762359993, -21.69091679252559857, -81.23899999999999011 ) ) ;
#1413 = DIRECTION ( 'NONE',  ( 0.000000000000000000, 0.000000000000000000, 1.000000000000000000 ) ) ;
#1414 = ADVANCED_FACE ( 'NONE', ( #19383 ), #47187, .T. ) ;
#1415 = CARTESIAN_POINT ( 'NONE',  ( 61.71045229757179840, 13.90353478476480120, -46.65737748138349872 ) ) ;
#1416 = DIRECTION ( 'NONE',  ( 0.000000000000000000, 0.000000000000000000, 1.000000000000000000 ) ) ;
#1417 = ORIENTED_EDGE ( 'NONE', *, *, #33330, .T. ) ;
#1418 = CARTESIAN_POINT ( 'NONE',  ( 75.20566382767655966, 0.9154195451593050148, -12.07278360623682190 ) ) ;
#1419 = ORIENTED_EDGE ( 'NONE', *, *, #15135, .F. ) ;
#1420 = CARTESIAN_POINT ( 'NONE',  ( 52.47575601967660219, -45.60254204323580041, -13.75339527049669996 ) ) ;
#1421 = AXIS2_PLACEMENT_3D ( 'NONE', #4906, #5181, #37141 ) ;
#1422 = CARTESIAN_POINT ( 'NONE',  ( 8.222921933280828100, -16.32121750950448558, -34.76395294823650772 ) ) ;
#1423 = DIRECTION ( 'NONE',  ( -0.7288689868556610385, 0.6846531968814593139, 0.000000000000000000 ) ) ;
#1424 = ORIENTED_EDGE ( 'NONE', *, *, #38832, .F. ) ;
#1425 = B_SPLINE_CURVE_WITH_KNOTS ( 'NONE', 3,
 ( #31340, #10683, #43425, #42654, #2821, #23216, #31596, #30572, #47366, #46594 ),
 .UNSPECIFIED., .F., .F.,
 ( 4, 2, 2, 2, 4 ),
 ( -0.1857717838168330138, -0.1853436703574470046, -0.1652145016249799980, -0.1459149143056970022, -0.1350635247393814631 ),
 .UNSPECIFIED. ) ;
#1426 = CARTESIAN_POINT ( 'NONE',  ( 73.23379646625190276, 0.8840451408750739093, -68.81103260973570457 ) ) ;
#1427 = CARTESIAN_POINT ( 'NONE',  ( 46.45131131807830371, -53.13009906462109910, -76.13977852870850427 ) ) ;
#1428 = CARTESIAN_POINT ( 'NONE',  ( 75.20081098849910006, 13.72681413341010170, -14.38878604297190122 ) ) ;
#1429 = ADVANCED_FACE ( 'NONE', ( #23547 ), #3670, .T. ) ;
#1430 = CARTESIAN_POINT ( 'NONE',  ( 45.31002628895360118, 14.31856235321039961, -8.676032249097868743 ) ) ;
#1431 = EDGE_CURVE ( 'NONE', #22850, #15006, #38801, .T. ) ;
#1432 = CARTESIAN_POINT ( 'NONE',  ( 38.67452568954060155, -37.56081407618430035, -84.65000000000000568 ) ) ;
#1433 = LINE ( 'NONE', #34877, #17322 ) ;
#1434 = PRODUCT_DEFINITION_SHAPE ( 'NONE', 'NONE',  #51878 ) ;
#1435 = CARTESIAN_POINT ( 'NONE',  ( 11.12431739752382320, 24.06965717816936845, -21.40301502515332999 ) ) ;
#1436 = CIRCLE ( 'NONE', #12283, 2.000000000000000000 ) ;
#1437 = CARTESIAN_POINT ( 'NONE',  ( 58.35547055286580331, 14.14095518617109981, -26.20742642234660025 ) ) ;
#1438 = CARTESIAN_POINT ( 'NONE',  ( 9.431647741891751480, -19.69859773764449784, -70.11336187001349174 ) ) ;
#1439 = ORIENTED_EDGE ( 'NONE', *, *, #19864, .T. ) ;
#1440 = CARTESIAN_POINT ( 'NONE',  ( 22.90066504558609850, -15.61618132107965984, -48.84717678326153845 ) ) ;
#1441 = CARTESIAN_POINT ( 'NONE',  ( 73.04443511092439678, 0.9036513197889539661, -62.20214363597960272 ) ) ;
#1442 = CARTESIAN_POINT ( 'NONE',  ( 63.43393739769620510, 1.883811055320669947, -62.44999999999999574 ) ) ;
#1443 = CARTESIAN_POINT ( 'NONE',  ( 72.83009333885370040, 0.9561296872639739597, -69.38553930450309792 ) ) ;
#1444 = CARTESIAN_POINT ( 'NONE',  ( 11.47551314106880049, -64.97235711416220738, -16.61573023122599935 ) ) ;
#1445 = CARTESIAN_POINT ( 'NONE',  ( 24.04493700328880479, -15.41104471036569024, -65.49941472047517266 ) ) ;
#1446 = DIRECTION ( 'NONE',  ( 1.000000000000000000, 0.000000000000000000, 0.000000000000000000 ) ) ;
#1447 = CARTESIAN_POINT ( 'NONE',  ( 49.25252623552799491, -53.65403535679590163, -54.36973269069940073 ) ) ;
#1448 = CARTESIAN_POINT ( 'NONE',  ( 9.221332323800828235, -19.60018030228138741, -56.62567467500329599 ) ) ;
#1449 = CARTESIAN_POINT ( 'NONE',  ( 8.222936770565050679, -15.65019028997524586, -34.50629429565288575 ) ) ;
#1450 = DIRECTION ( 'NONE',  ( 0.000000000000000000, 0.000000000000000000, -1.000000000000000000 ) ) ;
#1451 = ORIENTED_EDGE ( 'NONE', *, *, #25769, .T. ) ;
#1452 = CARTESIAN_POINT ( 'NONE',  ( 22.05896741169510022, -11.09947402434689856, -44.86001675125889676 ) ) ;
#1453 = CARTESIAN_POINT ( 'NONE',  ( 64.52993238696269884, 1.239065815390639980, -60.96725493808969532 ) ) ;
#1454 = ORIENTED_EDGE ( 'NONE', *, *, #12920, .T. ) ;
#1455 = CARTESIAN_POINT ( 'NONE',  ( 83.67474313643315043, -44.49425646638592724, -46.57587831639807519 ) ) ;
#1456 = CARTESIAN_POINT ( 'NONE',  ( 60.85786081670519820, -45.57206638213919803, -47.51990102095140145 ) ) ;
#1457 = CARTESIAN_POINT ( 'NONE',  ( 9.366426063424411197, -15.61626247110940113, -71.45282021618990598 ) ) ;
#1458 = CARTESIAN_POINT ( 'NONE',  ( 13.50362950008909912, 18.90074601879630123, -20.96762847675789843 ) ) ;
#1460 = FACE_OUTER_BOUND ( 'NONE', #45509, .T. ) ;
#1459 = CARTESIAN_POINT ( 'NONE',  ( 42.97465247888425210, 8.631328837227204787, -71.62199823571720003 ) ) ;
#1461 = CARTESIAN_POINT ( 'NONE',  ( 11.87719327230665023, -41.98180839364705008, -34.64999999999999858 ) ) ;
#1462 = CARTESIAN_POINT ( 'NONE',  ( 60.40024892680336421, -45.69452726455055114, -47.21879065637983075 ) ) ;
#1463 = ORIENTED_EDGE ( 'NONE', *, *, #6459, .F. ) ;
#1464 = B_SPLINE_CURVE_WITH_KNOTS ( 'NONE', 3,
 ( #15475, #31173, #253, #44023, #23301, #47202, #11808, #31426, #47962, #4440, #32192, #51119, #7870, #19653, #39578, #27770, #20407, #47455 ),
 .UNSPECIFIED., .F., .F.,
 ( 4, 2, 2, 2, 2, 2, 2, 2, 4 ),
 ( 0.4999984887057566940, 0.5624986776175371350, 0.6249988665293175760, 0.6874990554410981280, 0.7499992443528785691, 0.8124994332646588990, 0.8749996221764393400, 0.9374998110882196700, 1.000000000000000000 ),
 .UNSPECIFIED. ) ;
#1465 = ORIENTED_EDGE ( 'NONE', *, *, #26717, .T. ) ;
#1466 = ORIENTED_EDGE ( 'NONE', *, *, #48803, .T. ) ;
#1467 = EDGE_CURVE ( 'NONE', #7417, #30849, #38039, .T. ) ;
#1468 = ORIENTED_EDGE ( 'NONE', *, *, #29771, .T. ) ;
#1469 = CARTESIAN_POINT ( 'NONE',  ( 61.73009793398990297, -45.11618193111070241, -46.50780714789189574 ) ) ;
#1470 = CARTESIAN_POINT ( 'NONE',  ( 47.65701684106380043, -54.43194395141289732, -54.14467735021966632 ) ) ;
#1471 = ADVANCED_FACE ( 'NONE', ( #50845 ), #29523, .T. ) ;
#1472 = CARTESIAN_POINT ( 'NONE',  ( 53.63393739769619373, 31.59091783650714547, 11.14289321881345174 ) ) ;
#1473 = EDGE_CURVE ( 'NONE', #38811, #24770, #23474, .T. ) ;
#1474 = AXIS2_PLACEMENT_3D ( 'NONE', #20240, #40428, #9254 ) ;
#1475 = ORIENTED_EDGE ( 'NONE', *, *, #32075, .T. ) ;
#1476 = VERTEX_POINT ( 'NONE', #488 ) ;
#1477 = EDGE_CURVE ( 'NONE', #34084, #28709, #47785, .T. ) ;
#1478 = ORIENTED_EDGE ( 'NONE', *, *, #24385, .T. ) ;
#1479 = CARTESIAN_POINT ( 'NONE',  ( 17.90512215027165155, -22.20707991068925935, -72.86943705533576576 ) ) ;
#1480 = CARTESIAN_POINT ( 'NONE',  ( -8.439161468533404431, 14.66851012883797267, -42.49231428658828236 ) ) ;
#1481 = DIRECTION ( 'NONE',  ( 0.000000000000000000, 0.000000000000000000, 1.000000000000000000 ) ) ;
#1483 = CARTESIAN_POINT ( 'NONE',  ( 22.90093737893454318, -16.50198540115231083, -52.49448440678582273 ) ) ;
#1482 = AXIS2_PLACEMENT_3D ( 'NONE', #21995, #42200, #6298 ) ;
#1484 = CARTESIAN_POINT ( 'NONE',  ( 29.13393739769619728, 2.762490711761015572, -83.77132034355965118 ) ) ;
#1485 = ORIENTED_EDGE ( 'NONE', *, *, #20741, .F. ) ;
#1486 = DIRECTION ( 'NONE',  ( 0.9222478369447116853, 7.578800512648213833E-13, 0.3865991816478668297 ) ) ;
#1487 = CARTESIAN_POINT ( 'NONE',  ( 52.51047230659040110, -50.98242248866299775, -76.15156771093519694 ) ) ;
#1488 = DIRECTION ( 'NONE',  ( -1.000000000000000000, -0.000000000000000000, -0.000000000000000000 ) ) ;
#1489 = CARTESIAN_POINT ( 'NONE',  ( 83.87141997220982148, -44.85900116921240510, -47.47133103328876302 ) ) ;
#1490 = EDGE_CURVE ( 'NONE', #28355, #28663, #908, .T. ) ;
#1491 = CARTESIAN_POINT ( 'NONE',  ( 19.15004480972399747, -22.86117643056869753, -60.38692723972829413 ) ) ;
#1492 = DIRECTION ( 'NONE',  ( 0.000000000000000000, -3.858025010473989332E-12, -1.000000000000000000 ) ) ;
#1493 = CARTESIAN_POINT ( 'NONE',  ( 43.82162984104279957, 13.85296797899130006, -6.692196338156839452 ) ) ;
#1494 = ADVANCED_FACE ( 'NONE', ( #1276 ), #17267, .F. ) ;
#1495 = CARTESIAN_POINT ( 'NONE',  ( 42.16203264904510206, -44.19296810100679807, -4.955231405260050792 ) ) ;
#1496 = CARTESIAN_POINT ( 'NONE',  ( 72.97999464611700660, 0.9170823515334789455, -62.11176382508629956 ) ) ;
#1497 = CARTESIAN_POINT ( 'NONE',  ( 56.61650758228095270, 14.09311236904805575, -25.29355102104276298 ) ) ;
#1498 = CARTESIAN_POINT ( 'NONE',  ( 63.95618934260088650, 1.116860928049330015, -69.95003379205579108 ) ) ;
#1499 = CARTESIAN_POINT ( 'NONE',  ( 8.633937397696200833, -15.61618894467929941, -81.65000000000000568 ) ) ;
#1500 = CARTESIAN_POINT ( 'NONE',  ( 65.88923117608129587, 0.1772000611986560004, -17.14611195593310100 ) ) ;
#1501 = ORIENTED_EDGE ( 'NONE', *, *, #1027, .F. ) ;
#1502 = CARTESIAN_POINT ( 'NONE',  ( 13.51893541109899921, -51.88241111310259868, -74.91994212301230505 ) ) ;
#1503 = CARTESIAN_POINT ( 'NONE',  ( 47.20789789792050328, -54.78773433559100425, -54.64276886469819772 ) ) ;
#1504 = DIRECTION ( 'NONE',  ( -0.9752630547974272535, -0.2208726750153868490, 0.008788366101716807433 ) ) ;
#1505 = CARTESIAN_POINT ( 'NONE',  ( 15.67962062493570130, 19.63028992856250099, -20.15000000000000213 ) ) ;
#1506 = CIRCLE ( 'NONE', #35809, 7.599999999999996092 ) ;
#1508 = ADVANCED_FACE ( 'NONE', ( #18029 ), #5983, .T. ) ;
#1507 = CARTESIAN_POINT ( 'NONE',  ( 23.29272054552549776, -14.67821866136879905, -32.14999999999999858 ) ) ;
#1509 = CARTESIAN_POINT ( 'NONE',  ( 47.79491795492819506, -54.42065591789820189, -54.76904050234069388 ) ) ;
#1511 = CARTESIAN_POINT ( 'NONE',  ( 10.17382535698764912, -11.84529732105606570, -50.02674116095206358 ) ) ;
#1510 = CARTESIAN_POINT ( 'NONE',  ( 14.25134537629159937, 19.88704348313540393, -22.60288543027370167 ) ) ;
#1512 = CARTESIAN_POINT ( 'NONE',  ( 23.24148394091340109, -47.84168788784550230, -54.64999999999999858 ) ) ;
#1513 = CARTESIAN_POINT ( 'NONE',  ( 48.02894741700589520, 23.13744333908370265, -55.28037973459740329 ) ) ;
#1514 = ORIENTED_EDGE ( 'NONE', *, *, #8021, .T. ) ;
#1515 = CARTESIAN_POINT ( 'NONE',  ( 11.21742354769409999, -20.67291226489259870, -61.59270509622239587 ) ) ;
#1516 = VERTEX_POINT ( 'NONE', #10173 ) ;
#1517 = LINE ( 'NONE', #475, #34553 ) ;
#1518 = CARTESIAN_POINT ( 'NONE',  ( 65.08882305123219680, 1.387412027389909985, -61.00994802092580471 ) ) ;
#1519 = CARTESIAN_POINT ( 'NONE',  ( 9.366956123961729830, -16.50212425713979414, -43.41115352553956086 ) ) ;
#1521 = CARTESIAN_POINT ( 'NONE',  ( 54.52192486798780635, 16.42131495964800436, -25.85211914981980286 ) ) ;
#1520 = CARTESIAN_POINT ( 'NONE',  ( 82.76927220787719364, 14.00476221583219960, -47.14638044783710313 ) ) ;
#1522 = CARTESIAN_POINT ( 'NONE',  ( 22.84952155313539990, -17.77106438141320055, -72.55165484244589891 ) ) ;
#1523 = CARTESIAN_POINT ( 'NONE',  ( 2.458146360389407370, -5.580163940743402051, -34.79644291222906105 ) ) ;
#1524 = CARTESIAN_POINT ( 'NONE',  ( 57.38548500607319625, -45.11618894467940066, -16.91114573195289950 ) ) ;
#1525 = CARTESIAN_POINT ( 'NONE',  ( 68.13393739769620083, -29.61618894467929763, -65.65000000000000568 ) ) ;
#1526 = VERTEX_POINT ( 'NONE', #9411 ) ;
#1527 = VERTEX_POINT ( 'NONE', #42145 ) ;
#1528 = CARTESIAN_POINT ( 'NONE',  ( 11.77474680306579913, -65.05674245715520954, -16.56178175561650079 ) ) ;
#1529 = CARTESIAN_POINT ( 'NONE',  ( 11.95619557619699869, 33.96145947778699536, -46.48573944864449459 ) ) ;
#1530 = PLANE ( 'NONE',  #33213 ) ;
#1531 = ADVANCED_FACE ( 'NONE', ( #37690 ), #21940, .T. ) ;
#1532 = CARTESIAN_POINT ( 'NONE',  ( 11.97534989113796478, -21.02757240557042806, -55.16115446716158033 ) ) ;
#1533 = CARTESIAN_POINT ( 'NONE',  ( 11.19961559249191474, -65.24734874261105233, -46.39999999999999858 ) ) ;
#1534 = ORIENTED_EDGE ( 'NONE', *, *, #47452, .T. ) ;
#1535 = EDGE_CURVE ( 'NONE', #21630, #5671, #42400, .T. ) ;
#1536 = CARTESIAN_POINT ( 'NONE',  ( -22.52006847887419738, -21.48129748781419934, -54.44818321674360106 ) ) ;
#1537 = CARTESIAN_POINT ( 'NONE',  ( 54.10074222690910517, 17.30990981831594766, -26.94461139255280457 ) ) ;
#1538 = CYLINDRICAL_SURFACE ( 'NONE', #19772, 0.4999999999999985012 ) ;
#1539 = CARTESIAN_POINT ( 'NONE',  ( 48.53787819235320455, 22.50666767116170064, -53.55604134326550536 ) ) ;
#1540 = CARTESIAN_POINT ( 'NONE',  ( 63.10112488574510792, -1.418970404380659911, -16.22863366573779587 ) ) ;
#1541 = CARTESIAN_POINT ( 'NONE',  ( 50.83757470097779674, -48.72856112802359263, -76.31330844465840357 ) ) ;
#1542 = CARTESIAN_POINT ( 'NONE',  ( 23.04646112206593145, -19.60031942610110178, -43.67434694693088915 ) ) ;
#1543 = EDGE_LOOP ( 'NONE', ( #23972, #20280, #24064, #34922 ) ) ;
#1544 = CARTESIAN_POINT ( 'NONE',  ( 62.63393739769619373, -53.11618894467930119, 16.35000000000000142 ) ) ;
#1545 = VERTEX_POINT ( 'NONE', #9657 ) ;
#1546 = CARTESIAN_POINT ( 'NONE',  ( 24.04493741605278956, -14.58064998728431583, -57.46600087271308865 ) ) ;
#1547 = CIRCLE ( 'NONE', #33326, 10.00000000000000355 ) ;
#1548 = CARTESIAN_POINT ( 'NONE',  ( 16.13393739769620083, -15.61618894467929941, -76.14999999999999147 ) ) ;
#1549 = CARTESIAN_POINT ( 'NONE',  ( 9.272314511663010350, -20.18801675654929895, -80.60524855149100176 ) ) ;
#1550 = CARTESIAN_POINT ( 'NONE',  ( 14.25092085129799990, -51.11945063234009723, -22.60339916836199947 ) ) ;
#1551 = CARTESIAN_POINT ( 'NONE',  ( 56.79308212940160416, 19.43544009391369798, -74.33926175450910989 ) ) ;
#1552 = CARTESIAN_POINT ( 'NONE',  ( 46.35275103504449845, -52.90993241930539881, -76.14999999999999147 ) ) ;
#1553 = ORIENTED_EDGE ( 'NONE', *, *, #3853, .T. ) ;
#1554 = CARTESIAN_POINT ( 'NONE',  ( 55.83827540872459849, 14.63062675802740031, -17.19948835330949777 ) ) ;
#1555 = CARTESIAN_POINT ( 'NONE',  ( 57.16059588472099762, -50.58286358578039454, -53.44447636780149935 ) ) ;
#1556 = CARTESIAN_POINT ( 'NONE',  ( 52.69370164499209608, -49.76876103374040383, -48.79614663361950022 ) ) ;
#1557 = CARTESIAN_POINT ( 'NONE',  ( 68.13393739769618662, -30.49118894467929763, -65.65000000000000568 ) ) ;
#1558 = CARTESIAN_POINT ( 'NONE',  ( 61.28293951594075395, 14.37135162400847577, -47.68063998569994055 ) ) ;
#1559 = ORIENTED_EDGE ( 'NONE', *, *, #50815, .T. ) ;
#1560 = CARTESIAN_POINT ( 'NONE',  ( 47.14495913819140327, 22.93959528134109860, -75.51614565245159838 ) ) ;
#1561 = CARTESIAN_POINT ( 'NONE',  ( 65.16938214696820353, 1.384887413063060180, -60.98363600610959878 ) ) ;
#1562 = B_SPLINE_CURVE_WITH_KNOTS ( 'NONE', 3,
 ( #6945, #42060, #38659, #2747, #49929, #33912, #2483, #22119, #18464, #34437, #14020 ),
 .UNSPECIFIED., .F., .F.,
 ( 4, 2, 1, 2, 2, 4 ),
 ( 0.5057982913668825908, 0.5366858981564543996, 0.5675735049460263193, 0.6293487185251679383, 0.7528991456834492890, 1.000000000000000000 ),
 .UNSPECIFIED. ) ;
#1563 = CARTESIAN_POINT ( 'NONE',  ( 60.83524288460374407, -45.71913028275803725, -47.74946701498301138 ) ) ;
#1564 = LINE ( 'NONE', #6280, #30665 ) ;
#1565 = EDGE_CURVE ( 'NONE', #48357, #10825, #38099, .T. ) ;
#1566 = CARTESIAN_POINT ( 'NONE',  ( 24.15168607019749913, -17.53938432383520052, -81.58261298369829717 ) ) ;
#1568 = EDGE_CURVE ( 'NONE', #38311, #20782, #37722, .T. ) ;
#1567 = CARTESIAN_POINT ( 'NONE',  ( 82.45640976213999807, 13.86031052324960022, -46.38984575855459980 ) ) ;
#1569 = CARTESIAN_POINT ( 'NONE',  ( 22.90114886013774864, -15.61618877916400017, -48.45281860778688809 ) ) ;
#1570 = CARTESIAN_POINT ( 'NONE',  ( 41.04642893364459866, -37.84180074923700232, -85.09326562515050796 ) ) ;
#1571 = CARTESIAN_POINT ( 'NONE',  ( 61.26297983503680200, 14.01014034993499990, -46.58707769322979431 ) ) ;
#1572 = CARTESIAN_POINT ( 'NONE',  ( 15.09837409447361978, -7.705190857215417743, -68.96600325170983581 ) ) ;
#1573 = CARTESIAN_POINT ( 'NONE',  ( 6.156981251802729815, -64.53629940273539489, -47.78905844757039745 ) ) ;
#1574 = ADVANCED_FACE ( 'NONE', ( #45821 ), #21805, .T. ) ;
#1575 = ORIENTED_EDGE ( 'NONE', *, *, #48319, .F. ) ;
#1576 = CARTESIAN_POINT ( 'NONE',  ( 52.85276835010299834, -49.64923573467969931, -48.69281397809770340 ) ) ;
#1577 = VERTEX_POINT ( 'NONE', #25868 ) ;
#1578 = CIRCLE ( 'NONE', #34180, 2.000000000000001776 ) ;
#1579 = CARTESIAN_POINT ( 'NONE',  ( 57.69121261463050132, -45.19183260204550834, -25.76919019428369850 ) ) ;
#1580 = CARTESIAN_POINT ( 'NONE',  ( 24.04483683623963941, -15.65738770392476020, -65.79398883384345709 ) ) ;
#1581 = CARTESIAN_POINT ( 'NONE',  ( 57.24727847454269636, 13.89208492953430074, -25.38222954899870132 ) ) ;
#1582 = CARTESIAN_POINT ( 'NONE',  ( 11.85511828107729926, -21.22281588510560013, -35.16031938041760441 ) ) ;
#1584 = CARTESIAN_POINT ( 'NONE',  ( 50.03007040746729928, 17.38380685021119731, -76.14999999999999147 ) ) ;
#1583 = VECTOR ( 'NONE', #1605, 1000.000000000000114 ) ;
#1585 = CARTESIAN_POINT ( 'NONE',  ( 52.79729137842230102, 18.45889402858979977, -48.80671571307529888 ) ) ;
#1586 = CARTESIAN_POINT ( 'NONE',  ( 60.23362534523650424, -45.78182602740779572, -47.26357634580359246 ) ) ;
#1587 = CARTESIAN_POINT ( 'NONE',  ( 67.05761679591040547, -45.11618894467940066, -12.74175955172660046 ) ) ;
#1588 = ORIENTED_EDGE ( 'NONE', *, *, #14854, .F. ) ;
#1589 = CIRCLE ( 'NONE', #30859, 0.5000000000000000000 ) ;
#1590 = CARTESIAN_POINT ( 'NONE',  ( 9.160088560685300862, -18.23766309806380193, -71.95289117501670262 ) ) ;
#1591 = CARTESIAN_POINT ( 'NONE',  ( 73.04558532727548936, 1.003508719580009867, -69.08444824154609876 ) ) ;
#1592 = CARTESIAN_POINT ( 'NONE',  ( 47.43684003301049756, -54.63141987875069816, -54.76595269979989666 ) ) ;
#1593 = CARTESIAN_POINT ( 'NONE',  ( 18.02367597830500756, -7.913804971115164122, -49.36890451167464278 ) ) ;
#1594 = CARTESIAN_POINT ( 'NONE',  ( 73.13312216970089708, 0.9955677559369568996, -62.34557165980569948 ) ) ;
#1595 = CARTESIAN_POINT ( 'NONE',  ( 10.74148174179099868, -64.95262810519260199, -18.12706498543029809 ) ) ;
#1596 = CARTESIAN_POINT ( 'NONE',  ( 53.05372063824079731, 18.31120138125489660, -48.79446872373860344 ) ) ;
#1597 = CARTESIAN_POINT ( 'NONE',  ( 20.09906114624694951, -22.53978528867605036, -76.12648450854941018 ) ) ;
#1598 = CARTESIAN_POINT ( 'NONE',  ( 22.67257700126428333, -13.83859173790965258, -62.36835213070619233 ) ) ;
#1599 = CARTESIAN_POINT ( 'NONE',  ( 13.79739187203479744, -23.21386632249247839, -46.10279150706872997 ) ) ;
#1600 = EDGE_CURVE ( 'NONE', #13869, #21630, #35583, .T. ) ;
#1601 = CARTESIAN_POINT ( 'NONE',  ( 65.06933737855379718, 1.383922910988889976, -70.31893907080630868 ) ) ;
#1602 = ORIENTED_EDGE ( 'NONE', *, *, #36920, .F. ) ;
#1603 = CARTESIAN_POINT ( 'NONE',  ( 9.284331854864920075, -63.18779374651679603, -46.53073416084929903 ) ) ;
#1604 = ORIENTED_EDGE ( 'NONE', *, *, #15882, .T. ) ;
#1605 = DIRECTION ( 'NONE',  ( -0.4156269377774524099, -0.5720614028176843613, -0.7071067811865480168 ) ) ;
#1606 = CARTESIAN_POINT ( 'NONE',  ( 85.17508943611196059, 18.35477988570885444, -52.74015335379900904 ) ) ;
#1607 = CARTESIAN_POINT ( 'NONE',  ( 10.13629284140139930, -19.32709435317449831, -53.67081198986049628 ) ) ;
#1608 = CARTESIAN_POINT ( 'NONE',  ( 52.02578739311559985, 19.35467404128699798, -76.37778590630358622 ) ) ;
#1610 = VERTEX_POINT ( 'NONE', #10955 ) ;
#1609 = B_SPLINE_CURVE_WITH_KNOTS ( 'NONE', 3,
 ( #39533, #4135, #51838, #51330, #51583 ),
 .UNSPECIFIED., .F., .F.,
 ( 4, 1, 4 ),
 ( 0.4999950733969018013, 0.6666633822707539458, 1.000000000000000000 ),
 .UNSPECIFIED. ) ;
#1611 = CARTESIAN_POINT ( 'NONE',  ( -11.32734370190460105, 10.64934056395049922, -19.14999999999999858 ) ) ;
#1612 = CARTESIAN_POINT ( 'NONE',  ( 9.366560669795820360, -15.61606439180730099, -33.84717978380999881 ) ) ;
#1613 = CARTESIAN_POINT ( 'NONE',  ( 8.313605784523671716, -16.98482869512226401, -66.45256872909452284 ) ) ;
#1614 = CARTESIAN_POINT ( 'NONE',  ( 15.81717235992440074, -23.85526534721260106, -54.30456343836939936 ) ) ;
#1615 = CARTESIAN_POINT ( 'NONE',  ( 8.133937397696209715, 8.337936262032100032, -43.74348518090240390 ) ) ;
#1616 = CARTESIAN_POINT ( 'NONE',  ( 43.33544367895569849, -37.82612097586055455, -73.64240385444296066 ) ) ;
#1617 = ORIENTED_EDGE ( 'NONE', *, *, #45206, .F. ) ;
#1618 = CIRCLE ( 'NONE', #33396, 18.00000000000000355 ) ;
#1619 = CARTESIAN_POINT ( 'NONE',  ( 57.20752091846340193, -45.84035874391049958, -26.25769493244969865 ) ) ;
#1620 = CARTESIAN_POINT ( 'NONE',  ( 11.79648058786079901, -9.558700832602001540, -39.53485447945649867 ) ) ;
#1622 = CARTESIAN_POINT ( 'NONE',  ( 53.50485636675099954, -49.42567878242080326, -49.20411384802949328 ) ) ;
#1621 = VECTOR ( 'NONE', #13500, 1000.000000000000000 ) ;
#1623 = CARTESIAN_POINT ( 'NONE',  ( 8.222919265141586109, -14.58077434080222545, -32.54933488526609153 ) ) ;
#1624 = CIRCLE ( 'NONE', #10003, 1.000000000000000888 ) ;
#1625 = CARTESIAN_POINT ( 'NONE',  ( 13.52746909241120044, 20.57970132932399920, -74.87640169473949925 ) ) ;
#1626 = DIRECTION ( 'NONE',  ( 1.000000000000000000, 0.000000000000000000, 0.000000000000000000 ) ) ;
#1627 =( BOUNDED_CURVE ( )  B_SPLINE_CURVE ( 3, ( #43430, #27168, #23222, #43177 ),
 .UNSPECIFIED., .F., .T. ) 
 B_SPLINE_CURVE_WITH_KNOTS ( ( 4, 4 ),
 ( 5.122516320926171041, 5.907914484323606885 ),
 .UNSPECIFIED. ) 
 CURVE ( )  GEOMETRIC_REPRESENTATION_ITEM ( )  RATIONAL_B_SPLINE_CURVE ( ( 1.000000000000000000, 0.9492530216741927873, 0.9492530216741927873, 1.000000000000000000 ) ) 
 REPRESENTATION_ITEM ( '' )  );
#1628 = CARTESIAN_POINT ( 'NONE',  ( 41.24056053114340159, -44.83149236909930124, -5.438981521421270671 ) ) ;
#1629 = CARTESIAN_POINT ( 'NONE',  ( 83.70899958829811283, -44.46275198668180195, -46.59258846095890050 ) ) ;
#1630 = CARTESIAN_POINT ( 'NONE',  ( 18.48369898198360062, -23.51943772008690203, -55.91567931908580391 ) ) ;
#1631 = ORIENTED_EDGE ( 'NONE', *, *, #47061, .F. ) ;
#1632 = CARTESIAN_POINT ( 'NONE',  ( 52.92338564704119364, -49.48118464961610385, -27.26198717260970028 ) ) ;
#1633 = EDGE_CURVE ( 'NONE', #1136, #48851, #35566, .T. ) ;
#1634 = CARTESIAN_POINT ( 'NONE',  ( 55.47560955148180284, -50.96964303883889613, -75.04526988654890829 ) ) ;
#1635 = CARTESIAN_POINT ( 'NONE',  ( 12.98154199631053274, -22.91985500418327248, -40.13723907971733951 ) ) ;
#1636 = CARTESIAN_POINT ( 'NONE',  ( 2.204417066470079956, 24.53158638618599952, -10.01932650448550000 ) ) ;
#1637 = CARTESIAN_POINT ( 'NONE',  ( 12.00938018391108919, -9.895123749747092745, -70.14834965109328380 ) ) ;
#1638 = CARTESIAN_POINT ( 'NONE',  ( -23.86606260230380272, -15.61618894467908092, -53.92777777777782688 ) ) ;
#1639 = EDGE_CURVE ( 'NONE', #21944, #32127, #11212, .T. ) ;
#1640 = ORIENTED_EDGE ( 'NONE', *, *, #24705, .T. ) ;
#1641 = CARTESIAN_POINT ( 'NONE',  ( -9.106445543791931385, -44.03001587129549677, -5.504031293643000033 ) ) ;
#1642 = CARTESIAN_POINT ( 'NONE',  ( 47.46194251081040250, 23.38593605885670001, -54.80975913085070061 ) ) ;
#1643 = DIRECTION ( 'NONE',  ( 1.000000000000000000, 0.000000000000000000, 5.637851296925361431E-15 ) ) ;
#1644 = CARTESIAN_POINT ( 'NONE',  ( 63.18291598250529262, 1.096305581841160004, -62.33061120451039727 ) ) ;
#1645 = CARTESIAN_POINT ( 'NONE',  ( 60.98478001766370227, 14.15589715924580005, -46.95039023230899744 ) ) ;
#1646 = CARTESIAN_POINT ( 'NONE',  ( 11.11465748640249984, 33.92433621588410375, -17.59315317980379945 ) ) ;
#1647 = DIRECTION ( 'NONE',  ( -1.000000000000000000, -8.935017999999999834E-14, 2.044407999999999825E-12 ) ) ;
#1648 = CARTESIAN_POINT ( 'NONE',  ( 52.86023839377149613, 18.41257215013510162, -48.64479331233690829 ) ) ;
#1649 = CARTESIAN_POINT ( 'NONE',  ( 18.06932202639800167, 24.33696219936669891, -76.14999999999999147 ) ) ;
#1650 = DIRECTION ( 'NONE',  ( 0.000000000000000000, 0.000000000000000000, -1.000000000000000000 ) ) ;
#1651 = CARTESIAN_POINT ( 'NONE',  ( 53.50528692585089630, 17.84081850706130012, -27.26091398553390022 ) ) ;
#1652 = CARTESIAN_POINT ( 'NONE',  ( 52.25041881653689302, 21.33925748481399864, -54.52050471625830141 ) ) ;
#1653 = CARTESIAN_POINT ( 'NONE',  ( 63.69560517452909920, 1.394111633877010092, -69.38462823658350942 ) ) ;
#1654 = AXIS2_PLACEMENT_3D ( 'NONE', #2847, #31113, #42939 ) ;
#1655 = CARTESIAN_POINT ( 'NONE',  ( 51.23808412292059700, 13.88381105532070059, -11.16296171957920080 ) ) ;
#1656 = ORIENTED_EDGE ( 'NONE', *, *, #8046, .F. ) ;
#1657 = DIRECTION ( 'NONE',  ( -0.5516667872527389882, -0.8340645993220435761, 8.326672684688666658E-17 ) ) ;
#1658 = CARTESIAN_POINT ( 'NONE',  ( 10.77213051274009992, 32.03892353611769295, -45.20477560231249470 ) ) ;
#1659 = DIRECTION ( 'NONE',  ( 0.000000000000000000, 0.000000000000000000, -1.000000000000000000 ) ) ;
#1660 = AXIS2_PLACEMENT_3D ( 'NONE', #44288, #32994, #47977 ) ;
#1661 = CARTESIAN_POINT ( 'NONE',  ( 14.81467456660999993, -7.815966731016759539, -81.23899999999999011 ) ) ;
#1662 = EDGE_CURVE ( 'NONE', #48498, #12296, #21120, .T. ) ;
#1663 = CARTESIAN_POINT ( 'NONE',  ( 11.55666008087221641, -9.119572623996059946, -80.81238995496710231 ) ) ;
#1664 = VERTEX_POINT ( 'NONE', #23228 ) ;
#1665 = VERTEX_POINT ( 'NONE', #31350 ) ;
#1666 = B_SPLINE_CURVE_WITH_KNOTS ( 'NONE', 3,
 ( #722, #24294, #12533, #16713, #40309, #4144, #35859, #13070, #24815, #12275 ),
 .UNSPECIFIED., .F., .F.,
 ( 4, 2, 2, 2, 4 ),
 ( 0.000000000000000000, 0.2500000000000000000, 0.5000000000000000000, 0.7500000000000000000, 1.000000000000000000 ),
 .UNSPECIFIED. ) ;
#1667 = CARTESIAN_POINT ( 'NONE',  ( 63.93393739769619089, 1.883811055320669947, -62.44999999999999574 ) ) ;
#1668 = EDGE_CURVE ( 'NONE', #28134, #25290, #15167, .T. ) ;
#1669 = ORIENTED_EDGE ( 'NONE', *, *, #47982, .T. ) ;
#1670 = CARTESIAN_POINT ( 'NONE',  ( 10.24662431634200033, -64.14781499658329267, -46.34409721753970501 ) ) ;
#1671 = CARTESIAN_POINT ( 'NONE',  ( 56.60481287756580571, -45.54075046089940315, -25.88701370651539690 ) ) ;
#1672 = CARTESIAN_POINT ( 'NONE',  ( 23.99259192901511284, -16.66193452127228625, -77.54972237907269061 ) ) ;
#1673 = CARTESIAN_POINT ( 'NONE',  ( 0.1457841021255935343, -4.451138319363987073, -34.68167779225149161 ) ) ;
#1674 = CARTESIAN_POINT ( 'NONE',  ( 61.37880515396449965, 14.09585059423469922, -47.24540677760579399 ) ) ;
#1675 = CARTESIAN_POINT ( 'NONE',  ( 63.55847417696450208, 1.399433130755639798, -62.41600958228519858 ) ) ;
#1676 = ORIENTED_EDGE ( 'NONE', *, *, #48105, .F. ) ;
#1677 = CARTESIAN_POINT ( 'NONE',  ( 46.92881658497164210, 7.010978364822217479, -55.67557228759626042 ) ) ;
#1678 = ORIENTED_EDGE ( 'NONE', *, *, #32314, .F. ) ;
#1679 = CARTESIAN_POINT ( 'NONE',  ( 45.14275739423920442, -45.91162181551540300, -8.929573315219988316 ) ) ;
#1680 = CARTESIAN_POINT ( 'NONE',  ( 19.34678433693689215, -22.91919624005971556, -34.16012075487866895 ) ) ;
#1681 = CARTESIAN_POINT ( 'NONE',  ( 22.90092006877790709, -15.63200709851992443, -50.45356305415408826 ) ) ;
#1682 = ORIENTED_EDGE ( 'NONE', *, *, #4769, .F. ) ;
#1683 = DIRECTION ( 'NONE',  ( 0.3863301728269245006, -0.9223605572461989199, -3.608224830031755305E-16 ) ) ;
#1684 = CARTESIAN_POINT ( 'NONE',  ( 47.01289497786039817, -54.42182676496869931, -75.36291177546809195 ) ) ;
#1685 = CARTESIAN_POINT ( 'NONE',  ( 75.47257744440361193, 12.45848636096840067, -13.44587694045140047 ) ) ;
#1686 = CARTESIAN_POINT ( 'NONE',  ( 51.04010994546690227, 13.88381105532070059, -11.02192607414670000 ) ) ;
#1687 = CARTESIAN_POINT ( 'NONE',  ( 50.22323044735963293, 21.91892061222964472, -53.94765380580868452 ) ) ;
#1688 = AXIS2_PLACEMENT_3D ( 'NONE', #46753, #26537, #38878 ) ;
#1689 = VECTOR ( 'NONE', #33658, 1000.000000000000000 ) ;
#1690 = AXIS2_PLACEMENT_3D ( 'NONE', #39632, #7917, #51683 ) ;
#1691 = CARTESIAN_POINT ( 'NONE',  ( 22.90147442980407888, -15.70852189567019330, -62.85151964813176306 ) ) ;
#1692 = CARTESIAN_POINT ( 'NONE',  ( 60.46851295127660109, 13.88923079682050066, -26.48073026131960006 ) ) ;
#1693 = CIRCLE ( 'NONE', #14232, 2.000000000000000000 ) ;
#1694 = CLOSED_SHELL ( 'NONE', ( #12356, #8471, #31755, #13954, #36652, #22567, #45074, #30523, #7885, #702, #2912, #45252, #37723, #9003, #46743, #8402, #4460, #20099, #15266, #34124, #28345, #49575, #27791, #22214, #15863, #26295, #9008, #37449, #17898, #38741, #43411, #42881, #8802, #12110, #8183, #36287, #47763, #3443, #45280, #22229, #29551, #19431, #12834, #5292, #24576, #26528, #15723, #18699, #6950, #13357, #2129, #42108, #44657, #24258, #4602, #2828, #26312, #45212, #9753, #26551 ) ) ;
#1695 = CARTESIAN_POINT ( 'NONE',  ( 21.65169865715700226, -21.19660639024510118, -71.53930262915869775 ) ) ;
#1696 = B_SPLINE_SURFACE_WITH_KNOTS ( 'NONE', 3, 3, ( 
 ( #23166, #39695, #31802, #15839, #35236, #50972, #20011, #11927, #7471 ),
 ( #11664, #12172, #47821, #24185, #36003, #18992, #4047, #23422, #19771 ),
 ( #3280, #39443, #19254, #19513, #7735, #34973, #3801, #120, #35760 ),
 ( #51743, #28131, #51243, #27878, #39183, #15335, #35504, #43881, #7978 ),
 ( #23930, #44137, #16094, #47063, #31287, #31548, #47319, #43121, #23678 ),
 ( #27627, #47566, #15069, #11409, #31037, #39952, #11147, #27370, #32052 ),
 ( #48074, #51493, #15594, #8233, #43632, #40206, #43376, #27117, #7212 ),
 ( #44912, #24702, #49120, #21301, #32306, #25488, #48591, #33089, #33358 ),
 ( #44647, #37045, #9282, #37305, #41236, #884, #48850, #24442, #12424 ),
 ( #8753, #13473, #20521, #9016, #25229, #36258, #9538, #5347, #28388 ),
 ( #32825, #4294, #36516, #368, #20266, #16349, #1403, #36775, #5089 ),
 ( #21043, #24960, #40976, #29429, #8495, #12955, #17392, #49376, #45436 ),
 ( #40720, #48328, #4550, #44394, #4816, #40456, #16878, #1142, #618 ),
 ( #16603, #32560, #12692, #28646, #28909, #13219, #20783, #17138, #29169 ),
 ( #45170, #26270, #49886, #22594, #2431, #13980, #46221, #22074, #14749 ),
 ( #6119, #42277, #38610, #17901, #50401, #14489, #25743, #45692, #30204 ) ),
 .UNSPECIFIED., .F., .F., .F.,
 ( 4, 2, 2, 2, 2, 2, 2, 4 ),
 ( 4, 1, 1, 1, 1, 1, 4 ),
 ( -1.570796326794899889, -1.295906969605790104, -0.9817477042468120141, -0.7853981633974489451, -0.6872233929727680213, -0.5301437602932779214, -0.2788163480060950050, 2.850064269800000171E-05 ),
 ( -2.850064267999999931E-05, 0.1666666666666670182, 0.3333333333333329818, 0.5000000000000000000, 0.6666666666666670737, 0.8333333333333330373, 1.000028500642689888 ),
 .UNSPECIFIED. ) ;
#1697 = EDGE_LOOP ( 'NONE', ( #38223, #35096, #38212, #11603 ) ) ;
#1698 = CARTESIAN_POINT ( 'NONE',  ( 18.21162691092218111, -8.876325039443173637, -48.44236253966248995 ) ) ;
#1699 = ADVANCED_FACE ( 'NONE', ( #47625 ), #46868, .F. ) ;
#1700 = CARTESIAN_POINT ( 'NONE',  ( -10.41252972610489991, -41.50076126836940205, -4.265331396025359822 ) ) ;
#1701 = CARTESIAN_POINT ( 'NONE',  ( 76.79000011994270380, -42.06488460674430030, -14.47554790092480026 ) ) ;
#1702 = CARTESIAN_POINT ( 'NONE',  ( 72.98949351566140820, 0.9150552061895700362, -69.17495778280340346 ) ) ;
#1703 = DIRECTION ( 'NONE',  ( -0.9223605572461961444, -0.3863301728269312174, 0.000000000000000000 ) ) ;
#1704 = CARTESIAN_POINT ( 'NONE',  ( -24.36606260230359666, -50.61618894467959962, 11.34999999999999964 ) ) ;
#1705 = B_SPLINE_CURVE_WITH_KNOTS ( 'NONE', 3,
 ( #16444, #24018, #44486, #33190, #48953, #32398, #40042, #32143, #41073, #48419 ),
 .UNSPECIFIED., .F., .F.,
 ( 4, 2, 2, 2, 4 ),
 ( 0.5000003605016758446, 0.5624999999907476234, 0.6624999999928627981, 0.8224999999962434583, 1.000000000000000000 ),
 .UNSPECIFIED. ) ;
#1706 = CARTESIAN_POINT ( 'NONE',  ( 64.97340239734430156, 1.393731187554809958, -70.25064478522961053 ) ) ;
#1707 = CARTESIAN_POINT ( 'NONE',  ( 49.05945480412340487, -53.75841287389920353, -54.45983108200709921 ) ) ;
#1708 = CARTESIAN_POINT ( 'NONE',  ( 43.09344256554030750, -43.96039878386999789, -5.051331041927119792 ) ) ;
#1709 = FACE_OUTER_BOUND ( 'NONE', #41195, .T. ) ;
#1710 = CARTESIAN_POINT ( 'NONE',  ( 55.52075019247980237, -50.89749466248539989, -52.96229217805840506 ) ) ;
#1711 = AXIS2_PLACEMENT_3D ( 'NONE', #40553, #24278, #48686 ) ;
#1712 = ORIENTED_EDGE ( 'NONE', *, *, #3770, .F. ) ;
#1713 = CARTESIAN_POINT ( 'NONE',  ( 11.29738606970870052, -21.28315158705520105, -55.79222923803829559 ) ) ;
#1714 = CARTESIAN_POINT ( 'NONE',  ( 64.34763627307550848, 1.432916438945960103, -61.30477097020899890 ) ) ;
#1715 = ORIENTED_EDGE ( 'NONE', *, *, #43152, .T. ) ;
#1716 = CARTESIAN_POINT ( 'NONE',  ( 10.14762331803407669, -11.88703313963010189, -34.02451708608307968 ) ) ;
#1717 = CARTESIAN_POINT ( 'NONE',  ( 61.19107041010649795, -45.55858923584479925, -47.61997709501220299 ) ) ;
#1718 = DIRECTION ( 'NONE',  ( 0.3281607301299678814, 0.6263469766835031427, 0.7071067811865485719 ) ) ;
#1719 = CARTESIAN_POINT ( 'NONE',  ( 14.19855276898620033, -55.56934008872499930, -76.14999999999999147 ) ) ;
#1721 = CARTESIAN_POINT ( 'NONE',  ( 52.26504646883520167, -49.78354544620959388, -77.19463087837650050 ) ) ;
#1720 = CARTESIAN_POINT ( 'NONE',  ( 44.14631460519247952, 8.734076427534667175, -65.95149200678194745 ) ) ;
#1722 = CARTESIAN_POINT ( 'NONE',  ( 51.84413677266599763, -51.33743803777170456, -76.02231597519390505 ) ) ;
#1723 = CARTESIAN_POINT ( 'NONE',  ( 10.12953414448040057, -54.14192202099170004, -35.04035092416999220 ) ) ;
#1724 = EDGE_LOOP ( 'NONE', ( #5035, #39103, #10123, #27654 ) ) ;
#1725 = ORIENTED_EDGE ( 'NONE', *, *, #8148, .T. ) ;
#1726 = EDGE_LOOP ( 'NONE', ( #15779, #17354, #33318, #39302 ) ) ;
#1727 = EDGE_CURVE ( 'NONE', #36299, #14841, #11730, .T. ) ;
#1728 = ORIENTED_EDGE ( 'NONE', *, *, #9218, .F. ) ;
#1729 = CARTESIAN_POINT ( 'NONE',  ( 61.28609324400200364, -45.23040860746230152, -46.44124428239370417 ) ) ;
#1730 = AXIS2_PLACEMENT_3D ( 'NONE', #22923, #38944, #3034 ) ;
#1731 = CARTESIAN_POINT ( 'NONE',  ( 14.16187783161720048, 19.11875810978959933, -20.85710678118659800 ) ) ;
#1732 = FACE_OUTER_BOUND ( 'NONE', #40043, .T. ) ;
#1733 = CONICAL_SURFACE ( 'NONE', #5065, 1.154999999999999361, 0.08090409915523018303 ) ;
#1734 = EDGE_LOOP ( 'NONE', ( #45147, #20798, #48731, #3768 ) ) ;
#1735 = VECTOR ( 'NONE', #35100, 1000.000000000000000 ) ;
#1736 = ORIENTED_EDGE ( 'NONE', *, *, #35169, .F. ) ;
#1737 = DIRECTION ( 'NONE',  ( -3.489701575733883348E-12, -0.02843704686102061993, -0.9995955854073307334 ) ) ;
#1738 = CARTESIAN_POINT ( 'NONE',  ( 64.93393739769619799, 1.383811055320669947, -62.44999999999999574 ) ) ;
#1739 = CARTESIAN_POINT ( 'NONE',  ( 45.34397758664299971, -33.92854118026809829, -34.64999999999999858 ) ) ;
#1740 = ORIENTED_EDGE ( 'NONE', *, *, #20357, .T. ) ;
#1741 = CARTESIAN_POINT ( 'NONE',  ( 44.12711257345860361, 1.883811055320659955, -54.38706558040959749 ) ) ;
#1742 = CARTESIAN_POINT ( 'NONE',  ( 52.66575370896529762, -50.80825905356590511, -76.31205015067719444 ) ) ;
#1743 = CARTESIAN_POINT ( 'NONE',  ( 15.32497155414790058, -23.42210476894710425, -60.54536510185550213 ) ) ;
#1744 = CARTESIAN_POINT ( 'NONE',  ( 2.446837772604975925, -5.526216967578156947, -34.84133294386909085 ) ) ;
#1745 = CARTESIAN_POINT ( 'NONE',  ( 45.73978377946800578, 13.90695855600979947, -7.826106078158160173 ) ) ;
#1746 = CARTESIAN_POINT ( 'NONE',  ( 41.62693577203659601, -43.81499318205119664, -3.742293455806500191 ) ) ;
#1747 = CARTESIAN_POINT ( 'NONE',  ( 67.04038824939742369, -50.70395984888145335, -73.25000000000218847 ) ) ;
#1748 = CARTESIAN_POINT ( 'NONE',  ( 16.13393739769620083, -15.61618894467929941, -32.14999999999999858 ) ) ;
#1749 = CARTESIAN_POINT ( 'NONE',  ( 64.08748592165750324, 1.274156885185230070, -69.99444499429958455 ) ) ;
#1750 = CARTESIAN_POINT ( 'NONE',  ( 68.13393739769620083, -20.61618894467929763, -65.65000000000000568 ) ) ;
#1751 = CARTESIAN_POINT ( 'NONE',  ( 17.71568204744891517, -51.70197554413384466, -75.56421372420066973 ) ) ;
#1752 = ORIENTED_EDGE ( 'NONE', *, *, #10725, .F. ) ;
#1753 = CARTESIAN_POINT ( 'NONE',  ( 14.90551652343050115, -52.98917440366089693, -76.14999999999999147 ) ) ;
#1754 = ADVANCED_FACE ( 'NONE', ( #18798 ), #34777, .T. ) ;
#1755 = CARTESIAN_POINT ( 'NONE',  ( -13.36606260230359844, -50.61618894467959962, 14.21249999999999858 ) ) ;
#1756 = FACE_OUTER_BOUND ( 'NONE', #35636, .T. ) ;
#1757 = EDGE_CURVE ( 'NONE', #20534, #18008, #24256, .T. ) ;
#1758 = CARTESIAN_POINT ( 'NONE',  ( 11.55608217430013873, 33.52247355198553436, -44.82755758702938920 ) ) ;
#1759 = ADVANCED_FACE ( 'NONE', ( #34130 ), #26032, .F. ) ;
#1760 = AXIS2_PLACEMENT_3D ( 'NONE', #42868, #3025, #27121 ) ;
#1761 = CARTESIAN_POINT ( 'NONE',  ( 23.40110066171819980, -15.35420991546000025, -32.14999999999999858 ) ) ;
#1762 = AXIS2_PLACEMENT_3D ( 'NONE', #1024, #49251, #36919 ) ;
#1763 = EDGE_CURVE ( 'NONE', #40179, #42937, #47476, .T. ) ;
#1764 = CARTESIAN_POINT ( 'NONE',  ( 63.48611918674540533, 1.385702546077159925, -68.77407799673838440 ) ) ;
#1765 = DIRECTION ( 'NONE',  ( 0.000000000000000000, 1.000000000000000000, 0.000000000000000000 ) ) ;
#1766 = CARTESIAN_POINT ( 'NONE',  ( 13.22040357262759791, -8.188698541349817006, -44.88848981900320467 ) ) ;
#1767 = CARTESIAN_POINT ( 'NONE',  ( 23.62413055734869971, -48.75525398023999912, -35.14999999999999858 ) ) ;
#1768 = CARTESIAN_POINT ( 'NONE',  ( 15.09833599464489140, -23.52718242961558914, -46.33404756934790214 ) ) ;
#1769 = CARTESIAN_POINT ( 'NONE',  ( 48.25528797735780273, 23.04103089059060139, -55.30957496453530098 ) ) ;
#1770 = ORIENTED_EDGE ( 'NONE', *, *, #27594, .T. ) ;
#1771 = CARTESIAN_POINT ( 'NONE',  ( 13.52272076457530048, -9.064539772954379515, -62.22645654473139842 ) ) ;
#1772 = ORIENTED_EDGE ( 'NONE', *, *, #29438, .T. ) ;
#1773 = DIRECTION ( 'NONE',  ( 0.000000000000000000, 0.000000000000000000, -1.000000000000000000 ) ) ;
#1774 = CARTESIAN_POINT ( 'NONE',  ( 53.59007319635684041, -49.40623578145638106, -49.22505640097209323 ) ) ;
#1775 = CARTESIAN_POINT ( 'NONE',  ( 21.54530064538955614, -19.77480226385806716, -42.66115309383150134 ) ) ;
#1777 = CARTESIAN_POINT ( 'NONE',  ( 55.88720985982159561, 14.71003042163810015, -25.33276895956559827 ) ) ;
#1776 = CARTESIAN_POINT ( 'NONE',  ( 83.77685426296399385, 13.49366907108930036, -47.23654203728539613 ) ) ;
#1778 = CARTESIAN_POINT ( 'NONE',  ( 11.42698330956450015, -20.86853526883250254, -73.18540629095488725 ) ) ;
#1779 = CARTESIAN_POINT ( 'NONE',  ( 11.60439326025533013, 33.70240003096060377, -16.46429631544720351 ) ) ;
#1780 = CARTESIAN_POINT ( 'NONE',  ( 57.48392867679269358, -45.11618894467940066, -17.43413672685039728 ) ) ;
#1781 = CARTESIAN_POINT ( 'NONE',  ( 8.693390981131763340, -48.85252042381475235, -34.86893418027933933 ) ) ;
#1782 = VERTEX_POINT ( 'NONE', #3484 ) ;
#1783 = EDGE_CURVE ( 'NONE', #20901, #45666, #28073, .T. ) ;
#1784 = ORIENTED_EDGE ( 'NONE', *, *, #12856, .F. ) ;
#1785 = CARTESIAN_POINT ( 'NONE',  ( 12.29766918195309877, -64.63049967510049498, -15.84900139482509829 ) ) ;
#1786 = CARTESIAN_POINT ( 'NONE',  ( 10.93111994017589872, 32.28751451308780673, -44.89712406839979764 ) ) ;
#1787 = CARTESIAN_POINT ( 'NONE',  ( 24.04493700143699186, -15.61325609016573779, -39.50755344202253383 ) ) ;
#1788 = CARTESIAN_POINT ( 'NONE',  ( -0.3347231778593094398, 32.07101016863870768, -50.60099389661314007 ) ) ;
#1789 = CARTESIAN_POINT ( 'NONE',  ( 17.06835202619926406, -16.29508091107710754, 36.77166666666649775 ) ) ;
#1790 = ORIENTED_EDGE ( 'NONE', *, *, #1281, .T. ) ;
#1791 = CARTESIAN_POINT ( 'NONE',  ( -19.04335822585570170, -33.05973225684409300, -51.59769406952909776 ) ) ;
#1792 = DIRECTION ( 'NONE',  ( -1.000000000000000000, 0.000000000000000000, 0.000000000000000000 ) ) ;
#1793 = CARTESIAN_POINT ( 'NONE',  ( 51.39286536822110207, 19.84796399938319666, -49.98540144959209641 ) ) ;
#1794 = CARTESIAN_POINT ( 'NONE',  ( 62.41274088580539825, -1.258673626276660018, -16.17370678346230051 ) ) ;
#1795 = CARTESIAN_POINT ( 'NONE',  ( 50.87835763800730149, -49.82993816064299608, -76.22533641326209874 ) ) ;
#1796 = CARTESIAN_POINT ( 'NONE',  ( 60.67850367109549836, -46.09186595282459820, -48.19625756050770349 ) ) ;
#1797 = VECTOR ( 'NONE', #24040, 1000.000000000000000 ) ;
#1798 = EDGE_LOOP ( 'NONE', ( #30055, #3306, #45630, #43946 ) ) ;
#1799 = CARTESIAN_POINT ( 'NONE',  ( 10.90918837189948754, -9.627391034007024118, -33.06390794336576988 ) ) ;
#1801 = DIRECTION ( 'NONE',  ( 0.000000000000000000, -1.000000000000000000, 0.000000000000000000 ) ) ;
#1800 = AXIS2_PLACEMENT_3D ( 'NONE', #28318, #47246, #4229 ) ;
#1802 = VERTEX_POINT ( 'NONE', #15531 ) ;
#1803 = CARTESIAN_POINT ( 'NONE',  ( 20.11812543827117494, -8.703699676690527909, -57.17433449590220107 ) ) ;
#1804 = DIRECTION ( 'NONE',  ( 1.000000000000000000, 0.000000000000000000, 0.000000000000000000 ) ) ;
#1805 = EDGE_CURVE ( 'NONE', #20360, #49314, #10568, .T. ) ;
#1806 = VECTOR ( 'NONE', #48834, 1000.000000000000000 ) ;
#1807 = CARTESIAN_POINT ( 'NONE',  ( 8.558321896845489718, -13.56758030102569990, -37.09656150702419808 ) ) ;
#1808 = CARTESIAN_POINT ( 'NONE',  ( 9.813195994592092575, -18.65377965825830486, -65.70430698158793348 ) ) ;
#1809 = CARTESIAN_POINT ( 'NONE',  ( 53.91121292163150258, 19.51725716617239925, -76.32774465143938869 ) ) ;
#1810 = CARTESIAN_POINT ( 'NONE',  ( 46.81166088778630296, -53.49946929133769657, -76.01705645362530106 ) ) ;
#1811 = VERTEX_POINT ( 'NONE', #23357 ) ;
#1812 = CARTESIAN_POINT ( 'NONE',  ( 55.62561308564289675, 14.67649059877530071, -16.78101652394359888 ) ) ;
#1813 = CARTESIAN_POINT ( 'NONE',  ( 9.366947176629301097, -14.73031912718973047, -77.49448675212997273 ) ) ;
#1814 = CARTESIAN_POINT ( 'NONE',  ( 57.32356178811300396, -50.41450853367899754, -53.00097362968700310 ) ) ;
#1815 = CARTESIAN_POINT ( 'NONE',  ( 14.69332040448139942, -8.712069350285601033, -32.28170060268329422 ) ) ;
#1816 = CARTESIAN_POINT ( 'NONE',  ( 13.13393739769619906, -49.61618894467939356, -35.14999999999999858 ) ) ;
#1817 = ORIENTED_EDGE ( 'NONE', *, *, #5322, .F. ) ;
#1818 = B_SPLINE_CURVE_WITH_KNOTS ( 'NONE', 3,
 ( #24431, #48580, #12681, #44636, #18852, #6300, #19112, #7331, #14671 ),
 .UNSPECIFIED., .F., .F.,
 ( 4, 1, 1, 1, 1, 1, 4 ),
 ( 0.000000000000000000, 0.08931995506724747791, 0.2031549606839579136, 0.3169899663004408508, 0.4308249719171447500, 0.5446599775336212756, 0.6416644417609895790 ),
 .UNSPECIFIED. ) ;
#1819 = CARTESIAN_POINT ( 'NONE',  ( 47.45533712166319873, 23.17465650934340360, -75.00623913050900171 ) ) ;
#1820 = CARTESIAN_POINT ( 'NONE',  ( 65.14310169846920928, 1.336371993404959824, -60.77157093307350522 ) ) ;
#1821 = CARTESIAN_POINT ( 'NONE',  ( 53.41693480158270546, -49.35328119387190071, -48.75416851881869462 ) ) ;
#1822 = CARTESIAN_POINT ( 'NONE',  ( 68.13393739769658453, -28.80002732851960445, -29.09832030244560741 ) ) ;
#1823 = TOROIDAL_SURFACE ( 'NONE', #37700, 15.56227766038949945, 0.9999999999568489617 ) ;
#1824 = DIRECTION ( 'NONE',  ( 0.8090169943749525583, 0.5877852522924661427, 0.000000000000000000 ) ) ;
#1825 = CARTESIAN_POINT ( 'NONE',  ( 18.67273062756910207, -7.771648177471909946, -81.10729939731677973 ) ) ;
#1826 = ADVANCED_FACE ( 'NONE', ( #11605 ), #6835, .T. ) ;
#1827 = B_SPLINE_CURVE_WITH_KNOTS ( 'NONE', 3,
 ( #13861, #32978, #9158, #41124, #45055, #37194, #29818, #25886, #41900, #18043, #5999 ),
 .UNSPECIFIED., .F., .F.,
 ( 4, 2, 1, 2, 2, 4 ),
 ( 0.5057982913667791181, 0.5366858981563504827, 0.5675735049459218473, 0.6293487185250745686, 0.7528991456833793450, 1.000000000000000000 ),
 .UNSPECIFIED. ) ;
#1828 = CARTESIAN_POINT ( 'NONE',  ( 60.60297408742504643, 14.35593598357043099, -47.14360528713132936 ) ) ;
#1829 = CARTESIAN_POINT ( 'NONE',  ( -5.143445851551899928, 17.08457437255530209, -39.23905930810909126 ) ) ;
#1831 = CARTESIAN_POINT ( 'NONE',  ( 41.86067813338569721, -38.82080758994548830, -81.03536039894463272 ) ) ;
#1830 = CARTESIAN_POINT ( 'NONE',  ( 16.13393739769620083, -15.61618894467929941, -19.14999999999999858 ) ) ;
#1832 = FACE_OUTER_BOUND ( 'NONE', #18083, .T. ) ;
#1833 = CARTESIAN_POINT ( 'NONE',  ( -18.46117119614969937, 21.06649955959539966, -53.76231701354929982 ) ) ;
#1834 = ORIENTED_EDGE ( 'NONE', *, *, #24084, .T. ) ;
#1835 = VECTOR ( 'NONE', #3592, 1000.000000000000000 ) ;
#1836 = CARTESIAN_POINT ( 'NONE',  ( 52.80366530508379697, -49.67681281767760026, -48.66066742733800510 ) ) ;
#1837 = CIRCLE ( 'NONE', #34479, 19.56371635397779940 ) ;
#1838 = ORIENTED_EDGE ( 'NONE', *, *, #5333, .T. ) ;
#1839 = CARTESIAN_POINT ( 'NONE',  ( 41.49481243519896623, 8.512502644196153767, -78.61658674046471162 ) ) ;
#1840 = CARTESIAN_POINT ( 'NONE',  ( 48.59292341170780105, -54.12958895873340026, -55.31326040662610666 ) ) ;
#1841 = CARTESIAN_POINT ( 'NONE',  ( 56.72616477557319570, 14.12792985703750048, -25.70465367030369919 ) ) ;
#1842 = CARTESIAN_POINT ( 'NONE',  ( 22.37652147218269860, -18.89836852075259799, -42.60689890039769523 ) ) ;
#1843 = CARTESIAN_POINT ( 'NONE',  ( 29.10094820555050177, -26.72778965252999939, -34.97139175453740023 ) ) ;
#1844 = CARTESIAN_POINT ( 'NONE',  ( 53.33276493848160271, 18.22256187676000039, -49.10545657411340414 ) ) ;
#1845 = CARTESIAN_POINT ( 'NONE',  ( 64.86358929490590697, 1.263903724274369811, -60.80800729848100161 ) ) ;
#1846 = CARTESIAN_POINT ( 'NONE',  ( 60.32811079037119839, -45.73232245539999496, -47.24891709412590046 ) ) ;
#1847 = CARTESIAN_POINT ( 'NONE',  ( 16.13393739769620083, -15.61618894467929941, -74.14999999999999147 ) ) ;
#1848 = VERTEX_POINT ( 'NONE', #47764 ) ;
#1849 = CARTESIAN_POINT ( 'NONE',  ( 20.48230527184779959, -9.566528533608519069, -78.76571924648798984 ) ) ;
#1850 = ADVANCED_FACE ( 'NONE', ( #16293, #39130, #3994 ), #48017, .T. ) ;
#1851 = CARTESIAN_POINT ( 'NONE',  ( 72.85248830348810145, 1.369535599030039963, -68.77214795431979155 ) ) ;
#1852 = CARTESIAN_POINT ( 'NONE',  ( 47.50772827459159942, -54.57838557763199816, -54.69148953378340394 ) ) ;
#1853 = CARTESIAN_POINT ( 'NONE',  ( 10.13549572879737148, -10.40084719372432254, -49.02025583064260417 ) ) ;
#1854 = CARTESIAN_POINT ( 'NONE',  ( 72.85976395805219852, 1.369613126987639928, -62.54642937019949755 ) ) ;
#1855 = CARTESIAN_POINT ( 'NONE',  ( 11.73919149117240046, -65.42291996908740259, -18.11861173573770145 ) ) ;
#1856 = CARTESIAN_POINT ( 'NONE',  ( 71.61023385683570552, 1.007912009470880221, -60.76768544528139415 ) ) ;
#1857 = CARTESIAN_POINT ( 'NONE',  ( 39.88393739769619373, 31.59091783650714547, 17.05710678118654755 ) ) ;
#1858 = CARTESIAN_POINT ( 'NONE',  ( 22.89447552609475878, -15.29690831320359656, -62.43780689980356868 ) ) ;
#1859 = CARTESIAN_POINT ( 'NONE',  ( 9.367163129351689932, -15.61602587752549809, -57.45282021618999835 ) ) ;
#1860 = CARTESIAN_POINT ( 'NONE',  ( 64.81454860220668479, 1.096305581841150012, -70.60102141519101338 ) ) ;
#1861 = ORIENTED_EDGE ( 'NONE', *, *, #23152, .F. ) ;
#1862 = CARTESIAN_POINT ( 'NONE',  ( 8.970405606519269881, -63.23339553274689706, -46.63272187348500353 ) ) ;
#1863 = CARTESIAN_POINT ( 'NONE',  ( 17.16953043169627691, -7.705195452461492067, -47.33399925743757564 ) ) ;
#1864 = ORIENTED_EDGE ( 'NONE', *, *, #31561, .F. ) ;
#1865 = DIRECTION ( 'NONE',  ( 0.000000000000000000, 1.000000000000000000, 0.000000000000000000 ) ) ;
#1866 = DIRECTION ( 'NONE',  ( 1.000000000000000000, 0.000000000000000000, 0.000000000000000000 ) ) ;
#1867 = CARTESIAN_POINT ( 'NONE',  ( 57.09195614716849576, 16.19545665448480065, -46.39999999999999858 ) ) ;
#1868 = CARTESIAN_POINT ( 'NONE',  ( 52.68970887852299967, 19.39006498537879963, -76.51771730001300398 ) ) ;
#1869 = ORIENTED_EDGE ( 'NONE', *, *, #28540, .F. ) ;
#1870 = LINE ( 'NONE', #21514, #15867 ) ;
#1871 = FACE_OUTER_BOUND ( 'NONE', #2040, .T. ) ;
#1872 = DIRECTION ( 'NONE',  ( 0.000000000000000000, 0.000000000000000000, -1.000000000000000000 ) ) ;
#1873 = EDGE_CURVE ( 'NONE', #49018, #13116, #51763, .T. ) ;
#1874 = CARTESIAN_POINT ( 'NONE',  ( 7.979399327260850328, -14.39707905883819983, -56.83956923240529591 ) ) ;
#1875 = EDGE_CURVE ( 'NONE', #6515, #29501, #26789, .T. ) ;
#1876 = CARTESIAN_POINT ( 'NONE',  ( 18.14582764655064651, -9.096175230596063699, -56.04792584441368319 ) ) ;
#1877 = CARTESIAN_POINT ( 'NONE',  ( 43.77103348427062457, -37.88684466609633006, -71.46451074123150704 ) ) ;
#1878 = ADVANCED_FACE ( 'NONE', ( #29375 ), #17083, .T. ) ;
#1879 = EDGE_LOOP ( 'NONE', ( #23046, #50505, #48861, #755 ) ) ;
#1880 = VECTOR ( 'NONE', #40014, 1000.000000000000000 ) ;
#1881 = CARTESIAN_POINT ( 'NONE',  ( 57.03837479396619869, -45.89653934241670186, -26.24811324117309752 ) ) ;
#1882 = CARTESIAN_POINT ( 'NONE',  ( 21.35513134223840126, -20.93086933004790140, -40.48548165221990303 ) ) ;
#1883 = AXIS2_PLACEMENT_3D ( 'NONE', #9159, #9670, #1804 ) ;
#1884 = CARTESIAN_POINT ( 'NONE',  ( 52.77399506770059645, -49.72485891806019964, -48.90117834109280182 ) ) ;
#1885 = CARTESIAN_POINT ( 'NONE',  ( 9.706165438393730582, -12.70257730181489997, -32.14999999999999858 ) ) ;
#1886 = CARTESIAN_POINT ( 'NONE',  ( 14.40819075579249997, 20.22256044820920096, -75.26885115310530239 ) ) ;
#1887 = CYLINDRICAL_SURFACE ( 'NONE', #44089, 1.000000000000003775 ) ;
#1888 = EDGE_CURVE ( 'NONE', #28919, #42024, #42043, .T. ) ;
#1889 = CARTESIAN_POINT ( 'NONE',  ( 41.74197467272710327, -45.06540362037719660, -5.934314133911740008 ) ) ;
#1890 = CYLINDRICAL_SURFACE ( 'NONE', #7233, 6.766999999999998572 ) ;
#1891 = CARTESIAN_POINT ( 'NONE',  ( 19.91591662378250049, -22.94280848184829935, -53.85598711143169481 ) ) ;
#1892 = ADVANCED_FACE ( 'NONE', ( #33035 ), #8441, .F. ) ;
#1893 = ORIENTED_EDGE ( 'NONE', *, *, #28364, .T. ) ;
#1894 = CARTESIAN_POINT ( 'NONE',  ( 52.64678251747500326, -49.77729224470360236, -27.84346069079800401 ) ) ;
#1895 = CARTESIAN_POINT ( 'NONE',  ( 16.36414204281640039, -51.09682298092410235, -20.27640028196719868 ) ) ;
#1897 = CARTESIAN_POINT ( 'NONE',  ( 41.51381057164023503, -39.71056979448638202, -78.67767418718656813 ) ) ;
#1896 = CARTESIAN_POINT ( 'NONE',  ( 10.97326672351239907, 33.19570593983480222, -16.07944711293080076 ) ) ;
#1898 = CARTESIAN_POINT ( 'NONE',  ( 22.49413451099558614, -12.69308235403424590, -52.70970122521629975 ) ) ;
#1899 = CARTESIAN_POINT ( 'NONE',  ( 68.13393739769618662, -1.166188944679350081, -65.65000000000000568 ) ) ;
#1900 = VERTEX_POINT ( 'NONE', #21242 ) ;
#1901 = CARTESIAN_POINT ( 'NONE',  ( -2.700142689170709875, -48.79866302901520214, -5.083883930088719971 ) ) ;
#1902 = CARTESIAN_POINT ( 'NONE',  ( 47.48638238263849587, 23.36238434565460054, -54.71109617728680519 ) ) ;
#1903 = SPHERICAL_SURFACE ( 'NONE', #11986, 1.999999999999739764 ) ;
#1904 = CARTESIAN_POINT ( 'NONE',  ( 63.16328864814500577, 1.096044978595160035, -62.36169201816110075 ) ) ;
#1905 = DIRECTION ( 'NONE',  ( -1.000000000000000000, 0.000000000000000000, 0.000000000000000000 ) ) ;
#1906 = CARTESIAN_POINT ( 'NONE',  ( 11.50001307144090035, 33.75586786865649458, -16.62227806133670072 ) ) ;
#1907 = CARTESIAN_POINT ( 'NONE',  ( 51.88873276978809912, 18.11352090822219907, -77.07841357864730014 ) ) ;
#1908 = DIRECTION ( 'NONE',  ( 0.000000000000000000, 0.000000000000000000, 1.000000000000000000 ) ) ;
#1909 = CARTESIAN_POINT ( 'NONE',  ( 19.44911581942429635, 24.24611119365071588, -75.64152464225232109 ) ) ;
#1910 = CARTESIAN_POINT ( 'NONE',  ( 56.66172278421190356, -47.79833722945330265, -48.40341972513039792 ) ) ;
#1911 = DIRECTION ( 'NONE',  ( -0.000000000000000000, 1.000000000000000000, 0.000000000000000000 ) ) ;
#1912 = CARTESIAN_POINT ( 'NONE',  ( 51.97963026116360652, 21.17322201635790080, -53.55374510773989982 ) ) ;
#1913 = CARTESIAN_POINT ( 'NONE',  ( 63.64962603492929816, 1.332297187113020032, -69.43825451126340909 ) ) ;
#1914 = CARTESIAN_POINT ( 'NONE',  ( 12.08205748224309950, -65.27925620804988682, -16.92411159753779870 ) ) ;
#1915 = CARTESIAN_POINT ( 'NONE',  ( 50.03007040746459921, -48.61618894467930119, -76.14999999999999147 ) ) ;
#1916 = ORIENTED_EDGE ( 'NONE', *, *, #17794, .T. ) ;
#1917 = DIRECTION ( 'NONE',  ( 0.000000000000000000, 0.000000000000000000, 1.000000000000000000 ) ) ;
#1918 = CARTESIAN_POINT ( 'NONE',  ( 10.77081499238640028, 31.97176150883899837, -45.20487661762840048 ) ) ;
#1919 = AXIS2_PLACEMENT_3D ( 'NONE', #24596, #39654, #51201 ) ;
#1920 = CARTESIAN_POINT ( 'NONE',  ( 72.71580530985501412, 1.395841836299609895, -62.33173032533499480 ) ) ;
#1921 = CARTESIAN_POINT ( 'NONE',  ( 67.09948588395030811, -33.06559114426190149, -20.09058981816900058 ) ) ;
#1922 = EDGE_LOOP ( 'NONE', ( #50683, #28575, #11412, #1656 ) ) ;
#1923 = LINE ( 'NONE', #49635, #18443 ) ;
#1924 = ORIENTED_EDGE ( 'NONE', *, *, #31100, .T. ) ;
#1925 = ORIENTED_EDGE ( 'NONE', *, *, #42229, .F. ) ;
#1926 = CARTESIAN_POINT ( 'NONE',  ( 11.13393739769619906, -15.61618894467929941, -46.14999999999999858 ) ) ;
#1927 = ORIENTED_EDGE ( 'NONE', *, *, #5665, .T. ) ;
#1928 = CARTESIAN_POINT ( 'NONE',  ( 11.08968279120479927, -64.22844165307741093, -45.26598027972680427 ) ) ;
#1929 = CARTESIAN_POINT ( 'NONE',  ( 57.39717139072750030, -45.73959026386049942, -26.25633027675440090 ) ) ;
#1930 = B_SPLINE_CURVE_WITH_KNOTS ( 'NONE', 3,
 ( #2424, #22588, #34384, #26519, #46216, #38605, #10302, #50396, #10562, #47044, #23150, #3783, #6944, #50954, #31019, #28115, #11132, #27610, #19752 ),
 .UNSPECIFIED., .F., .F.,
 ( 4, 3, 3, 3, 3, 3, 4 ),
 ( 8.130128712166969862, 8.744224101849910724, 18.73762479188560093, 24.98350022315790397, 28.10643793879390273, 33.10313828381179491, 38.04558972261919791 ),
 .UNSPECIFIED. ) ;
#1931 = CARTESIAN_POINT ( 'NONE',  ( 22.72480972994501869, -17.38744065826488239, -44.53615520578274101 ) ) ;
#1932 = DIRECTION ( 'NONE',  ( 0.9750030843324432039, -0.2182216942497586243, -0.04181241084878352388 ) ) ;
#1933 = ORIENTED_EDGE ( 'NONE', *, *, #37546, .T. ) ;
#1934 = CARTESIAN_POINT ( 'NONE',  ( 45.71458171117632219, 6.890963836120773678, -61.74677868268134517 ) ) ;
#1935 = ORIENTED_EDGE ( 'NONE', *, *, #9755, .T. ) ;
#1936 = CARTESIAN_POINT ( 'NONE',  ( 47.84831528495369213, -45.94688046902010115, -10.78657639741869900 ) ) ;
#1937 = EDGE_CURVE ( 'NONE', #13386, #49388, #40659, .T. ) ;
#1938 = AXIS2_PLACEMENT_3D ( 'NONE', #45067, #36160, #20420 ) ;
#1939 = CARTESIAN_POINT ( 'NONE',  ( 10.85063640367556204, -21.53850039894781432, -34.52410773689097567 ) ) ;
#1940 = CARTESIAN_POINT ( 'NONE',  ( 15.78755803686370029, 19.77187500835140099, -20.74412215666090020 ) ) ;
#1941 = CARTESIAN_POINT ( 'NONE',  ( 22.90093740079596429, -15.61855648616878689, -50.45293054938055377 ) ) ;
#1942 = EDGE_CURVE ( 'NONE', #30218, #26995, #5027, .T. ) ;
#1944 = ORIENTED_EDGE ( 'NONE', *, *, #30435, .F. ) ;
#1943 =( BOUNDED_SURFACE ( )  B_SPLINE_SURFACE ( 2, 2, ( 
 ( #3885, #44220, #36094, #24014, #36341, #450, #35840, #12006, #31885 ),
 ( #12259, #51577, #27961, #32394, #8844, #32653, #39527, #8322, #20104 ),
 ( #35589, #43964, #40037, #4128, #16179, #13554, #33187, #17479, #48950 ),
 ( #37647, #20880, #1747, #973, #13051, #25318, #29004, #41070, #21640 ),
 ( #49718, #33701, #25573, #45002, #45522, #17731, #13806, #5180, #4905 ) ),
 .UNSPECIFIED., .F., .T., .T. ) 
 B_SPLINE_SURFACE_WITH_KNOTS ( ( 3, 2, 3 ),
 ( 3, 2, 2, 2, 3 ),
 ( -0.003205554299145560102, 0.8238407534178779912, 1.650887061134900025 ),
 ( -3.141592653589790007, -1.570796326794899889, 0.000000000000000000, 1.570796326794899889, 3.141592653589790007 ),
 .UNSPECIFIED. ) 
 GEOMETRIC_REPRESENTATION_ITEM ( )  RATIONAL_B_SPLINE_SURFACE ( (
 ( 1.000000000000000000, 0.7071067811865480168, 1.000000000000000000, 0.7071067811865480168, 1.000000000000000000, 0.7071067811865480168, 1.000000000000000000, 0.7071067811865480168, 1.000000000000000000),
 ( 0.9157107718028779653, 0.6475052963473819645, 0.9157107718028779653, 0.6475052963473819645, 0.9157107718028779653, 0.6475052963473819645, 0.9157107718028779653, 0.6475052963473819645, 0.9157107718028779653),
 ( 1.000000000000000000, 0.7071067811865480168, 1.000000000000000000, 0.7071067811865480168, 1.000000000000000000, 0.7071067811865480168, 1.000000000000000000, 0.7071067811865480168, 1.000000000000000000),
 ( 0.9157107718028449916, 0.6475052963473589829, 0.9157107718028449916, 0.6475052963473589829, 0.9157107718028449916, 0.6475052963473589829, 0.9157107718028449916, 0.6475052963473589829, 0.9157107718028449916),
 ( 1.000000000000000000, 0.7071067811865480168, 1.000000000000000000, 0.7071067811865480168, 1.000000000000000000, 0.7071067811865480168, 1.000000000000000000, 0.7071067811865480168, 1.000000000000000000) ) ) 
 REPRESENTATION_ITEM ( '' )  SURFACE ( )  );
#1945 = CARTESIAN_POINT ( 'NONE',  ( 73.01385068780759013, 0.9098571636355720083, -69.14090909090960224 ) ) ;
#1946 = CARTESIAN_POINT ( 'NONE',  ( 47.11818671551210258, -54.50110806056969892, -75.17436503908771783 ) ) ;
#1947 = CARTESIAN_POINT ( 'NONE',  ( 64.87946167155979538, 12.49593138203690046, -10.46016357390099927 ) ) ;
#1948 = CARTESIAN_POINT ( 'NONE',  ( 50.20000625561069540, -49.66915949483620096, -76.14999999999999147 ) ) ;
#1949 = CARTESIAN_POINT ( 'NONE',  ( 54.69511575210409404, 20.01728140309300130, -53.07518616905519337 ) ) ;
#1950 = VECTOR ( 'NONE', #6293, 1000.000000000000227 ) ;
#1951 = CIRCLE ( 'NONE', #27081, 16.60961179679778610 ) ;
#1952 = CARTESIAN_POINT ( 'NONE',  ( 52.57481508192889663, 20.19967092288990074, -75.83555757118479335 ) ) ;
#1953 = CARTESIAN_POINT ( 'NONE',  ( 61.66984244049909591, 13.88595911880170064, -28.15148628585509982 ) ) ;
#1954 = CARTESIAN_POINT ( 'NONE',  ( 23.86772648130780183, -16.94857574789820021, -75.34181132021238625 ) ) ;
#1955 = ADVANCED_FACE ( 'NONE', ( #37251 ), #40400, .T. ) ;
#1956 = VERTEX_POINT ( 'NONE', #37504 ) ;
#1957 = CARTESIAN_POINT ( 'NONE',  ( 24.04461175216078317, -15.61617380819018663, -65.50766589912049653 ) ) ;
#1958 = CARTESIAN_POINT ( 'NONE',  ( 73.07318775143939149, 0.8986939045430389905, -62.24348040161350326 ) ) ;
#1959 = DIRECTION ( 'NONE',  ( 0.000000000000000000, 1.000000000000000000, 0.000000000000000000 ) ) ;
#1960 = EDGE_CURVE ( 'NONE', #39247, #15377, #38368, .T. ) ;
#1961 = CARTESIAN_POINT ( 'NONE',  ( 72.65863549626330098, 1.000506532484680022, -69.59146369456030357 ) ) ;
#1962 = CARTESIAN_POINT ( 'NONE',  ( 71.58179376171669617, 0.9036513197889510796, -60.73950228677190211 ) ) ;
#1963 = CARTESIAN_POINT ( 'NONE',  ( 24.04508668034977248, -15.61618904219531778, -35.79233368253564862 ) ) ;
#1964 = CARTESIAN_POINT ( 'NONE',  ( 15.09831437461540915, -7.705198071712128005, -42.96596090275411939 ) ) ;
#1965 = CARTESIAN_POINT ( 'NONE',  ( 65.19259745005730622, 1.384447124000270035, -70.32375107525380997 ) ) ;
#1966 = CARTESIAN_POINT ( 'NONE',  ( 9.976573729570910487, -53.79438198982419550, -34.67842804303189297 ) ) ;
#1967 = CARTESIAN_POINT ( 'NONE',  ( 42.70036219403750266, -44.15320494937070350, -5.071714815372149410 ) ) ;
#1968 = AXIS2_PLACEMENT_3D ( 'NONE', #43740, #16464, #32166 ) ;
#1969 = PLANE ( 'NONE',  #11684 ) ;
#1970 = CARTESIAN_POINT ( 'NONE',  ( 68.13393739769618662, -30.66618894467940137, -40.64999999999999858 ) ) ;
#1971 = EDGE_LOOP ( 'NONE', ( #47071, #17443, #38687, #7155, #20399 ) ) ;
#1972 = CARTESIAN_POINT ( 'NONE',  ( 17.44088820494859959, -8.281437829217798807, -52.62347199549359544 ) ) ;
#1973 = CARTESIAN_POINT ( 'NONE',  ( 63.71089178726140290, 1.048861872235970161, -61.59523540267399966 ) ) ;
#1974 = ORIENTED_EDGE ( 'NONE', *, *, #4701, .T. ) ;
#1975 = CARTESIAN_POINT ( 'NONE',  ( 9.944902970854920810, 32.89001708672019930, -17.55158127909980337 ) ) ;
#1976 = CARTESIAN_POINT ( 'NONE',  ( 38.67452568954050207, -36.11618894467930119, -81.65000000000000568 ) ) ;
#1977 = DIRECTION ( 'NONE',  ( 0.000000000000000000, 0.000000000000000000, 1.000000000000000000 ) ) ;
#1978 = CARTESIAN_POINT ( 'NONE',  ( 47.81335647231750130, -54.39749252970050009, -54.71582838609450050 ) ) ;
#1980 = CARTESIAN_POINT ( 'NONE',  ( 11.96950732185187327, -9.924082013335068453, -54.14612557624229794 ) ) ;
#1979 = CARTESIAN_POINT ( 'NONE',  ( 45.05458756453126767, 8.801970288391714803, -61.54777943354527281 ) ) ;
#1981 = CARTESIAN_POINT ( 'NONE',  ( 19.21265657477716005, 18.23736444591407135, -34.79644660940672907 ) ) ;
#1982 = CARTESIAN_POINT ( 'NONE',  ( 20.13393739769620083, -2.337132753317949785, -62.14999999999999858 ) ) ;
#1983 = ORIENTED_EDGE ( 'NONE', *, *, #32786, .F. ) ;
#1984 = EDGE_LOOP ( 'NONE', ( #32187, #27398, #36832, #18906 ) ) ;
#1985 = EDGE_LOOP ( 'NONE', ( #14919, #4355, #20268, #30721, #27509 ) ) ;
#1986 = VERTEX_POINT ( 'NONE', #33563 ) ;
#1987 = CARTESIAN_POINT ( 'NONE',  ( 61.14293679174719642, -45.32076580385039932, -46.99585847235690039 ) ) ;
#1988 = CARTESIAN_POINT ( 'NONE',  ( 51.35032894455923014, -51.12106501579054907, -50.03594749790474339 ) ) ;
#1989 = CIRCLE ( 'NONE', #1118, 5.499999999999998224 ) ;
#1990 = CYLINDRICAL_SURFACE ( 'NONE', #16811, 0.4999999999999980571 ) ;
#1991 = AXIS2_PLACEMENT_3D ( 'NONE', #23507, #35591, #51834 ) ;
#1992 = ORIENTED_EDGE ( 'NONE', *, *, #50752, .F. ) ;
#1993 = ORIENTED_EDGE ( 'NONE', *, *, #16301, .F. ) ;
#1994 = CARTESIAN_POINT ( 'NONE',  ( 24.04484245248367458, -15.57431735484160384, -77.50599178999226524 ) ) ;
#1995 = EDGE_CURVE ( 'NONE', #17152, #14356, #25174, .T. ) ;
#1996 = CARTESIAN_POINT ( 'NONE',  ( 68.13393739769618662, -29.66618894467940137, -65.65000000000000568 ) ) ;
#1997 = ORIENTED_EDGE ( 'NONE', *, *, #26711, .T. ) ;
#1998 = CARTESIAN_POINT ( 'NONE',  ( 23.90266814002770346, -17.16108999061242102, -49.57014705178468716 ) ) ;
#1999 = CARTESIAN_POINT ( 'NONE',  ( 53.50362398765149408, -50.77013085338330001, -76.38491628186639559 ) ) ;
#2000 = CARTESIAN_POINT ( 'NONE',  ( 60.68849784050689777, 14.37619509097770099, -47.46714534019130127 ) ) ;
#2001 = CARTESIAN_POINT ( 'NONE',  ( 23.98165953727020039, -15.61838248587350009, -74.01258338267071224 ) ) ;
#2002 = FACE_OUTER_BOUND ( 'NONE', #11935, .T. ) ;
#2003 = CONICAL_SURFACE ( 'NONE', #23749, 3.567506086244481622, 0.04995839572194331335 ) ;
#2004 = CARTESIAN_POINT ( 'NONE',  ( 41.35124225329579417, 13.74788993297780060, -5.668943192347540183 ) ) ;
#2005 = CARTESIAN_POINT ( 'NONE',  ( 42.25542674110280217, -43.34247267206160359, -3.898748443015970011 ) ) ;
#2006 = CARTESIAN_POINT ( 'NONE',  ( 72.23968433060379368, 1.026088617261680103, -61.27424404961239901 ) ) ;
#2007 = CARTESIAN_POINT ( 'NONE',  ( -7.099872940393900045, 14.68218975379929958, -5.638321079196820129 ) ) ;
#2008 = CARTESIAN_POINT ( 'NONE',  ( 64.75240447675760436, 1.412311545208970065, -70.17188921921470524 ) ) ;
#2009 = LINE ( 'NONE', #1499, #42841 ) ;
#2010 = CARTESIAN_POINT ( 'NONE',  ( 66.56329404978689013, -1.021671608844639811, -16.96526467878980071 ) ) ;
#2011 = EDGE_CURVE ( 'NONE', #27433, #50743, #51160, .T. ) ;
#2012 = ORIENTED_EDGE ( 'NONE', *, *, #5435, .T. ) ;
#2013 = CARTESIAN_POINT ( 'NONE',  ( 14.40115328186280053, -52.48721817738829287, -75.97756937697440094 ) ) ;
#2014 = CIRCLE ( 'NONE', #20434, 14.50000000000000178 ) ;
#2015 = CARTESIAN_POINT ( 'NONE',  ( 47.18324198357289845, -54.80726809202429450, -54.61058319554170026 ) ) ;
#2016 = EDGE_CURVE ( 'NONE', #11224, #26299, #45114, .T. ) ;
#2017 = B_SPLINE_CURVE_WITH_KNOTS ( 'NONE', 3,
 ( #45735, #26048, #1706, #14019, #17942, #41275, #10352, #2481, #49928, #29978, #46001, #5649, #1965, #9831, #22380, #26311 ),
 .UNSPECIFIED., .F., .F.,
 ( 4, 2, 2, 2, 2, 2, 2, 4 ),
 ( 0.000000000000000000, 0.07319275283554199651, 0.1391693187718069935, 0.1804046724819720060, 0.2061767685508260062, 0.2577209606885330073, 0.3401916681088649752, 0.4123535371016520124 ),
 .UNSPECIFIED. ) ;
#2018 = LINE ( 'NONE', #25062, #33928 ) ;
#2019 = AXIS2_PLACEMENT_3D ( 'NONE', #13002, #23970, #47863 ) ;
#2020 = DIRECTION ( 'NONE',  ( 0.5193766129849389790, 0.000000000000000000, -0.8545454545454520545 ) ) ;
#2021 = B_SPLINE_CURVE_WITH_KNOTS ( 'NONE', 3,
 ( #25618, #40850, #4951, #5226, #1537, #17524, #25364, #33493, #13851, #17775, #48726, #24841, #33233, #1022, #44788, #21688 ),
 .UNSPECIFIED., .F., .F.,
 ( 4, 2, 2, 2, 2, 2, 2, 4 ),
 ( 0.000000000000000000, 0.08300154222485658928, 0.3122511566686436146, 0.4625707003009139617, 0.6128902439331841423, 0.7672452152475061071, 0.9236669617927576459, 1.000000000000000000 ),
 .UNSPECIFIED. ) ;
#2022 = CARTESIAN_POINT ( 'NONE',  ( 46.57724752952230318, -53.42760099267549379, -76.07728942632040514 ) ) ;
#2023 = CARTESIAN_POINT ( 'NONE',  ( 63.26014808640670140, 1.265401080857980087, -68.86031185997930493 ) ) ;
#2024 = CARTESIAN_POINT ( 'NONE',  ( 48.08549546625859961, -54.25909977946169960, -54.72858777524749740 ) ) ;
#2025 = CARTESIAN_POINT ( 'NONE',  ( 8.222262383277058717, -15.61618471288229948, -44.50766849176299900 ) ) ;
#2026 = CARTESIAN_POINT ( 'NONE',  ( 56.50306386193680908, 19.52810639402949988, -53.80671218419070101 ) ) ;
#2027 = CARTESIAN_POINT ( 'NONE',  ( 47.96924620030790010, 23.16287378102880012, -55.24392577788600533 ) ) ;
#2028 = ORIENTED_EDGE ( 'NONE', *, *, #12361, .F. ) ;
#2029 = CARTESIAN_POINT ( 'NONE',  ( 22.73929038217119825, -18.08840882263159955, -76.96117772256469891 ) ) ;
#2030 = ORIENTED_EDGE ( 'NONE', *, *, #39129, .T. ) ;
#2031 = DIRECTION ( 'NONE',  ( 1.000000000000000000, 0.000000000000000000, 0.000000000000000000 ) ) ;
#2032 = DIRECTION ( 'NONE',  ( 0.8090169943749472292, -0.5877852522924734702, 0.000000000000000000 ) ) ;
#2033 = CARTESIAN_POINT ( 'NONE',  ( 12.14992638744813824, -8.703597654584235954, -40.84100140184820305 ) ) ;
#2035 = CARTESIAN_POINT ( 'NONE',  ( 52.58045726257309838, 18.61320901487979995, -28.15003661640620081 ) ) ;
#2034 = CARTESIAN_POINT ( 'NONE',  ( 84.44784216359251161, 11.88381105532070059, -47.47585302082339354 ) ) ;
#2036 = CARTESIAN_POINT ( 'NONE',  ( 20.66515000696679749, -21.02087866656289705, -78.73073146540821199 ) ) ;
#2037 = CARTESIAN_POINT ( 'NONE',  ( 19.40270147970599979, -49.11618894467930829, -34.64999999999999858 ) ) ;
#2038 = CARTESIAN_POINT ( 'NONE',  ( 55.87821755845719451, -45.11618894467940066, -14.71204629713069956 ) ) ;
#2039 = CARTESIAN_POINT ( 'NONE',  ( 16.13393739769620083, -15.61618894467929941, 7.849999999999999645 ) ) ;
#2040 = EDGE_LOOP ( 'NONE', ( #5607, #38553, #13786, #44927, #10429 ) ) ;
#2041 = CARTESIAN_POINT ( 'NONE',  ( 8.664097273252890474, -48.79579064807929711, -34.96018206680729890 ) ) ;
#2042 = AXIS2_PLACEMENT_3D ( 'NONE', #26480, #34345, #26221 ) ;
#2043 = ORIENTED_EDGE ( 'NONE', *, *, #23955, .F. ) ;
#2044 = ORIENTED_EDGE ( 'NONE', *, *, #20741, .T. ) ;
#2045 = CARTESIAN_POINT ( 'NONE',  ( 12.31509292276649958, -64.63808111159269743, -15.85496248754649962 ) ) ;
#2046 = DIRECTION ( 'NONE',  ( 0.8660254037844351549, -0.5000000000000061062, 0.000000000000000000 ) ) ;
#2047 = CARTESIAN_POINT ( 'NONE',  ( 22.90093381512099668, -15.61618921778096336, -54.45281771551935890 ) ) ;
#2048 = CARTESIAN_POINT ( 'NONE',  ( 11.71633469864940125, -65.33094175685840810, -47.42091646943509886 ) ) ;
#2049 = ORIENTED_EDGE ( 'NONE', *, *, #271, .F. ) ;
#2050 = TOROIDAL_SURFACE ( 'NONE', #31315, 14.50000000000000000, 1.500000000000000000 ) ;
#2051 = ORIENTED_EDGE ( 'NONE', *, *, #31232, .F. ) ;
#2052 = CARTESIAN_POINT ( 'NONE',  ( -20.73632584900919795, -28.65688283608509934, -52.79758657238259900 ) ) ;
#2053 = CARTESIAN_POINT ( 'NONE',  ( 56.96266348647149869, 14.69613425542049967, -26.24590930288369961 ) ) ;
#2054 = CARTESIAN_POINT ( 'NONE',  ( 53.52648000331849687, -49.40009412630509900, -49.17036629546220183 ) ) ;
#2055 = EDGE_CURVE ( 'NONE', #8993, #4830, #49318, .T. ) ;
#2056 = VECTOR ( 'NONE', #41210, 1000.000000000000114 ) ;
#2057 = CARTESIAN_POINT ( 'NONE',  ( 53.13593891953769344, 18.17654723902450087, -48.71694933965890328 ) ) ;
#2058 = CARTESIAN_POINT ( 'NONE',  ( 64.95030386029479530, -1.381558580551719873, -16.48070782218119845 ) ) ;
#2059 = CARTESIAN_POINT ( 'NONE',  ( 50.88311850207449538, -49.08192913539919289, -76.31540042335409169 ) ) ;
#2060 = EDGE_CURVE ( 'NONE', #2815, #12686, #24904, .T. ) ;
#2061 = CARTESIAN_POINT ( 'NONE',  ( 56.76964376401279821, -50.36013064195670097, -52.79151955495370174 ) ) ;
#2062 = EDGE_LOOP ( 'NONE', ( #45987, #51744 ) ) ;
#2063 = EDGE_CURVE ( 'NONE', #25175, #45766, #2640, .T. ) ;
#2064 = CARTESIAN_POINT ( 'NONE',  ( 20.97397396333849784, -9.337171417351125768, -33.50141378971362371 ) ) ;
#2065 = CARTESIAN_POINT ( 'NONE',  ( 65.43042069958039519, 17.98087126524892909, -71.50000000000090949 ) ) ;
#2066 = ORIENTED_EDGE ( 'NONE', *, *, #44781, .T. ) ;
#2067 = LINE ( 'NONE', #9425, #28497 ) ;
#2068 = CARTESIAN_POINT ( 'NONE',  ( 46.20926621405610035, -46.13066349458740234, -9.791022513314830533 ) ) ;
#2069 = EDGE_CURVE ( 'NONE', #34462, #31947, #12409, .T. ) ;
#2070 = CARTESIAN_POINT ( 'NONE',  ( 14.22007994406810027, -8.005413869907048507, -43.43407599211369075 ) ) ;
#2071 = CARTESIAN_POINT ( 'NONE',  ( 13.58337773622180045, -50.81123558615350078, -21.57342365037870024 ) ) ;
#2072 = CARTESIAN_POINT ( 'NONE',  ( 54.26191342777159576, 19.70404036202970133, -75.79539126991741682 ) ) ;
#2073 = CARTESIAN_POINT ( 'NONE',  ( 47.57154850773469690, -54.56571258662719970, -74.14999999999999147 ) ) ;
#2074 = ORIENTED_EDGE ( 'NONE', *, *, #40283, .T. ) ;
#2075 = CARTESIAN_POINT ( 'NONE',  ( 56.06575504548730038, 14.47328901277619906, -17.60699513660309989 ) ) ;
#2076 = CARTESIAN_POINT ( 'NONE',  ( 11.97534233955078165, -10.20481119701443262, -77.74448596776977638 ) ) ;
#2077 = CARTESIAN_POINT ( 'NONE',  ( 57.05931830690970230, -50.59304237665070048, -53.44572518174189923 ) ) ;
#2078 = CARTESIAN_POINT ( 'NONE',  ( 15.59821405493169877, -8.583724250529140676, -44.32297812435340489 ) ) ;
#2079 = PLANE ( 'NONE',  #31097 ) ;
#2080 = CARTESIAN_POINT ( 'NONE',  ( 47.64116069630630790, 23.30216092776590031, -74.19778950654200855 ) ) ;
#2081 = CARTESIAN_POINT ( 'NONE',  ( 65.04142308672740569, 1.102581332775300016, -60.56179621591489592 ) ) ;
#2082 = ADVANCED_FACE ( 'NONE', ( #21505 ), #11019, .F. ) ;
#2083 = CARTESIAN_POINT ( 'NONE',  ( 60.68789125469645995, -45.76122483410996011, -47.75606074947312152 ) ) ;
#2084 = CARTESIAN_POINT ( 'NONE',  ( 15.09849320450292431, -7.705176464883582099, -57.25066471183642136 ) ) ;
#2085 = FACE_OUTER_BOUND ( 'NONE', #46082, .T. ) ;
#2086 = DIRECTION ( 'NONE',  ( 0.000000000000000000, -1.000000000000000000, 0.000000000000000000 ) ) ;
#2087 = VECTOR ( 'NONE', #47340, 1000.000000000000000 ) ;
#2088 = CARTESIAN_POINT ( 'NONE',  ( 52.68908936341578908, 18.51792035577400242, -38.31189016485890875 ) ) ;
#2090 = CARTESIAN_POINT ( 'NONE',  ( 42.09738834484929271, -37.61273901578999812, -79.83211318711599347 ) ) ;
#2089 = CARTESIAN_POINT ( 'NONE',  ( 51.13393739769620083, 19.38381105532069881, 11.34999999999999964 ) ) ;
#2091 = AXIS2_PLACEMENT_3D ( 'NONE', #3053, #19287, #46833 ) ;
#2092 = LINE ( 'NONE', #8930, #22623 ) ;
#2093 = CARTESIAN_POINT ( 'NONE',  ( 8.222845792583640900, -15.61638830267690103, -48.79233150823699816 ) ) ;
#2094 = CARTESIAN_POINT ( 'NONE',  ( 6.354289799265040450, 33.87947625492100201, -49.17526497145149733 ) ) ;
#2095 = ORIENTED_EDGE ( 'NONE', *, *, #33459, .F. ) ;
#2096 = CARTESIAN_POINT ( 'NONE',  ( 52.75373701181550246, -49.71023522919640669, -48.68700931713409830 ) ) ;
#2097 = ORIENTED_EDGE ( 'NONE', *, *, #15032, .T. ) ;
#2098 = EDGE_CURVE ( 'NONE', #46021, #12521, #13664, .T. ) ;
#2099 = AXIS2_PLACEMENT_3D ( 'NONE', #41942, #26976, #21999 ) ;
#2100 = DIRECTION ( 'NONE',  ( 0.6888026391158399431, 0.7071067811865427988, 0.1598465650148944706 ) ) ;
#2101 = CARTESIAN_POINT ( 'NONE',  ( 57.05854516459380221, 13.92570298991769917, -25.37276671555040153 ) ) ;
#2102 = CARTESIAN_POINT ( 'NONE',  ( 17.88832476977960084, -8.785033577883739397, -44.03283965954289414 ) ) ;
#2103 = CARTESIAN_POINT ( 'NONE',  ( 29.10811623682189975, -26.73044074004180004, -34.99013415954840411 ) ) ;
#2104 = CARTESIAN_POINT ( 'NONE',  ( 52.92824256686530049, 18.39304521719179775, -48.92669088499940244 ) ) ;
#2105 = DIRECTION ( 'NONE',  ( 0.000000000000000000, 0.000000000000000000, 1.000000000000000000 ) ) ;
#2106 = ORIENTED_EDGE ( 'NONE', *, *, #45125, .F. ) ;
#2107 = CARTESIAN_POINT ( 'NONE',  ( 19.88348325370240133, -22.05417008143080082, -79.39947069499689292 ) ) ;
#2108 = DIRECTION ( 'NONE',  ( 1.000000000000000000, 0.000000000000000000, 0.000000000000000000 ) ) ;
#2109 = FACE_OUTER_BOUND ( 'NONE', #17396, .T. ) ;
#2110 = CARTESIAN_POINT ( 'NONE',  ( 73.01149271009099095, 1.265664290790580182, -62.44691083073610116 ) ) ;
#2111 = CARTESIAN_POINT ( 'NONE',  ( 10.78192289011060012, -64.93864051461240194, -17.70651626566360193 ) ) ;
#2112 = CARTESIAN_POINT ( 'NONE',  ( 71.56253747416560884, 1.100585178972000033, -60.77016257896750062 ) ) ;
#2113 = DIRECTION ( 'NONE',  ( 0.000000000000000000, -1.000000000000000000, 0.000000000000000000 ) ) ;
#2114 = CARTESIAN_POINT ( 'NONE',  ( 22.90083777812701982, -15.57647135431740004, -62.45096014559136677 ) ) ;
#2115 = CARTESIAN_POINT ( 'NONE',  ( 21.32685934670647043, -21.60664595198382898, -45.78044139066837204 ) ) ;
#2116 = ORIENTED_EDGE ( 'NONE', *, *, #30735, .T. ) ;
#2117 = CARTESIAN_POINT ( 'NONE',  ( 64.91481325068460251, 1.325839985408290067, -70.42711907493250578 ) ) ;
#2118 = VERTEX_POINT ( 'NONE', #10768 ) ;
#2119 = CARTESIAN_POINT ( 'NONE',  ( 9.279764201640460897, -63.15676077487329820, -46.53183983118100286 ) ) ;
#2120 = CARTESIAN_POINT ( 'NONE',  ( 16.13393739769620083, -15.61618894467929941, -1.149999999999999911 ) ) ;
#2121 = EDGE_LOOP ( 'NONE', ( #28707, #38998 ) ) ;
#2122 = CARTESIAN_POINT ( 'NONE',  ( 23.13393739769620083, -2.337132753317950229, -84.65000000000000568 ) ) ;
#2124 = B_SPLINE_CURVE_WITH_KNOTS ( 'NONE', 3,
 ( #27180, #35570, #39509, #50530, #38743, #3096, #2837, #14621, #47130, #14878, #35036, #51044, #42411, #18803, #2575, #6506 ),
 .UNSPECIFIED., .F., .F.,
 ( 4, 2, 2, 2, 2, 2, 2, 4 ),
 ( 0.1345846079508339899, 1.324410793755629978, 2.838023129476340056, 3.784030839301789850, 4.257034694214520520, 5.013840862074870230, 6.224730730651439892, 7.568061678603579701 ),
 .UNSPECIFIED. ) ;
#2123 = CARTESIAN_POINT ( 'NONE',  ( 56.92789888016839939, 19.40969084676650169, -53.72375501523509911 ) ) ;
#2125 = CARTESIAN_POINT ( 'NONE',  ( 20.99564533579582104, -21.94233031744103002, -69.79933736319598836 ) ) ;
#2126 = CARTESIAN_POINT ( 'NONE',  ( 52.63691515807389720, 19.18298782300839989, -76.75103203969149490 ) ) ;
#2127 = B_SPLINE_CURVE_WITH_KNOTS ( 'NONE', 3,
 ( #26876, #19016, #22933, #10653, #26611, #50229, #2266, #50992, #2528, #15095 ),
 .UNSPECIFIED., .F., .F.,
 ( 4, 1, 1, 1, 1, 1, 1, 4 ),
 ( 0.000000000000000000, 0.1428610187999453662, 0.2857180173656790334, 0.4285750159314126728, 0.5714320144971452020, 0.7142890130628789525, 0.8571460116286125919, 1.000000000000000000 ),
 .UNSPECIFIED. ) ;
#2128 = ORIENTED_EDGE ( 'NONE', *, *, #41690, .F. ) ;
#2129 = ADVANCED_FACE ( 'NONE', ( #18871 ), #34593, .T. ) ;
#2130 = DIRECTION ( 'NONE',  ( 1.377466541413789929E-11, -1.000000000000000000, 3.637457002807960330E-11 ) ) ;
#2131 = FACE_BOUND ( 'NONE', #44388, .T. ) ;
#2132 = CARTESIAN_POINT ( 'NONE',  ( 22.90071998467804804, -15.61618839864605057, -72.45282571548244732 ) ) ;
#2133 = CARTESIAN_POINT ( 'NONE',  ( 64.93393739769619799, 1.383811055320669947, -68.84999999999999432 ) ) ;
#2134 = EDGE_CURVE ( 'NONE', #41237, #2815, #48649, .T. ) ;
#2135 = CARTESIAN_POINT ( 'NONE',  ( 23.78551980429849877, -12.54438056346319996, -53.67081198986049628 ) ) ;
#2136 = CYLINDRICAL_SURFACE ( 'NONE', #31309, 1.000000000000001332 ) ;
#2137 = CARTESIAN_POINT ( 'NONE',  ( 45.55117721137337128, -38.10517850036617205, -62.56376302709497139 ) ) ;
#2138 = EDGE_LOOP ( 'NONE', ( #696, #20214, #8362, #43316 ) ) ;
#2139 = DIRECTION ( 'NONE',  ( -1.000000000000000000, 0.000000000000000000, 0.000000000000000000 ) ) ;
#2140 = CARTESIAN_POINT ( 'NONE',  ( 16.33068269661450245, -23.06387214769610239, -48.72425048283629678 ) ) ;
#2141 = EDGE_CURVE ( 'NONE', #8577, #47254, #46985, .T. ) ;
#2142 = CARTESIAN_POINT ( 'NONE',  ( 9.524248426565812053, -13.05564950212349906, -32.14999999999999858 ) ) ;
#2143 = CARTESIAN_POINT ( 'NONE',  ( 13.76101809979590129, 20.06273926763419979, -74.14993629405250886 ) ) ;
#2144 = EDGE_CURVE ( 'NONE', #28912, #14719, #3039, .T. ) ;
#2145 = CARTESIAN_POINT ( 'NONE',  ( 17.27947978972579079, -52.93031137935258812, -76.14999999999999147 ) ) ;
#2146 = CARTESIAN_POINT ( 'NONE',  ( 45.55527100000080054, -45.23107034338350019, -8.104338965901980885 ) ) ;
#2147 = CARTESIAN_POINT ( 'NONE',  ( 23.57883367829501609, -12.85227554272108463, -61.39446357243666341 ) ) ;
#2148 = CIRCLE ( 'NONE', #28920, 38.00000000000000000 ) ;
#2149 = CARTESIAN_POINT ( 'NONE',  ( 18.93672734906450117, -23.37035487000509804, -65.89726463310188365 ) ) ;
#2150 = EDGE_LOOP ( 'NONE', ( #3023, #42729, #51132, #1559, #13182 ) ) ;
#2151 = CARTESIAN_POINT ( 'NONE',  ( 52.66971685105150414, -49.76276386869629675, -28.00590812673040020 ) ) ;
#2152 = VECTOR ( 'NONE', #27858, 1000.000000000000000 ) ;
#2153 = CARTESIAN_POINT ( 'NONE',  ( 55.05458601726860479, -50.70842107373549368, -75.94395387307670831 ) ) ;
#2155 = CARTESIAN_POINT ( 'NONE',  ( 41.51536462713278297, -39.71075051493620123, -78.67016534560366381 ) ) ;
#2154 = CARTESIAN_POINT ( 'NONE',  ( 2.889165181869819854, 24.41604209844609841, -9.165974378419068813 ) ) ;
#2156 = CARTESIAN_POINT ( 'NONE',  ( 47.77491216306469823, -54.41753965447119867, -54.70980729587230229 ) ) ;
#2157 = CARTESIAN_POINT ( 'NONE',  ( 16.13393739769620083, -15.61618894467929941, -21.14999999999999858 ) ) ;
#2158 = ORIENTED_EDGE ( 'NONE', *, *, #34472, .F. ) ;
#2159 = CARTESIAN_POINT ( 'NONE',  ( -9.084335010050759607, -44.06577152659710350, -5.655813564461040777 ) ) ;
#2160 = CARTESIAN_POINT ( 'NONE',  ( 47.45221640967909593, 23.39300712745730237, -54.83348072773369353 ) ) ;
#2161 = ADVANCED_FACE ( 'NONE', ( #14430 ), #6573, .T. ) ;
#2162 = DIRECTION ( 'NONE',  ( 0.9987374001630935361, 0.000000000000000000, -0.05023550054956103100 ) ) ;
#2163 = CARTESIAN_POINT ( 'NONE',  ( 63.21464875163319874, 1.097545367735379918, -62.28124518314879765 ) ) ;
#2164 = CARTESIAN_POINT ( 'NONE',  ( 16.13393739769620083, -15.61618894467929941, -12.13039854958090125 ) ) ;
#2165 = CARTESIAN_POINT ( 'NONE',  ( 11.98643056009569996, 34.18553739082079801, -17.50083518280339945 ) ) ;
#2166 = CARTESIAN_POINT ( 'NONE',  ( 51.85719454310479648, 18.05925402898169807, -77.06877199832730696 ) ) ;
#2167 = CARTESIAN_POINT ( 'NONE',  ( 53.20761889774500020, 18.23056977116550215, -48.79936051936330443 ) ) ;
#2168 = DIRECTION ( 'NONE',  ( 0.000000000000000000, 0.000000000000000000, -1.000000000000000000 ) ) ;
#2169 = CARTESIAN_POINT ( 'NONE',  ( 72.33393739769618946, 1.883811055320669947, -68.84999999999999432 ) ) ;
#2170 = CARTESIAN_POINT ( 'NONE',  ( 53.42450764587109546, 17.84354127545960012, -27.17986344697500201 ) ) ;
#2171 = EDGE_CURVE ( 'NONE', #34516, #48296, #25943, .T. ) ;
#2172 = CARTESIAN_POINT ( 'NONE',  ( 54.91646384901309830, 20.20362395552430002, -54.04939823774950014 ) ) ;
#2173 = CARTESIAN_POINT ( 'NONE',  ( 63.25101889642220954, 0.9479899806831150189, -69.13670813078400101 ) ) ;
#2174 = DIRECTION ( 'NONE',  ( -1.000000000000000000, 0.000000000000000000, 0.000000000000000000 ) ) ;
#2175 = CARTESIAN_POINT ( 'NONE',  ( 9.807752066895531584, -20.47784117495694645, -76.29935098731050402 ) ) ;
#2176 = CARTESIAN_POINT ( 'NONE',  ( 53.91121044660913242, 19.99510753048234335, -75.56421356237309794 ) ) ;
#2177 = CARTESIAN_POINT ( 'NONE',  ( 11.10554433198240076, 32.07361188791999496, -44.25245290781410290 ) ) ;
#2178 = CARTESIAN_POINT ( 'NONE',  ( 16.65420337942459739, 19.88381105532299742, -15.67544741556190324 ) ) ;
#2179 = CARTESIAN_POINT ( 'NONE',  ( 66.61544058241169353, -32.00365722899270082, -17.88087248512020011 ) ) ;
#2180 = AXIS2_PLACEMENT_3D ( 'NONE', #11320, #51407, #3711 ) ;
#2181 = CARTESIAN_POINT ( 'NONE',  ( 12.13393739769649926, 24.18330853958550364, -74.14999999999999147 ) ) ;
#2182 = VERTEX_POINT ( 'NONE', #41961 ) ;
#2183 = EDGE_LOOP ( 'NONE', ( #39248, #38356, #16893, #27058, #13122, #35973, #29171, #24670, #19454, #46637 ) ) ;
#2184 = CARTESIAN_POINT ( 'NONE',  ( 86.75761129539395711, -50.03040250705240055, -60.02031173921621132 ) ) ;
#2185 = CARTESIAN_POINT ( 'NONE',  ( 76.49544124310347115, -3.188935732503785925, -13.20777387361363964 ) ) ;
#2186 = ORIENTED_EDGE ( 'NONE', *, *, #29324, .F. ) ;
#2187 = CARTESIAN_POINT ( 'NONE',  ( 12.13443654887529988, -65.25725380275149234, -46.16574950220010010 ) ) ;
#2188 = CARTESIAN_POINT ( 'NONE',  ( 56.44903381556829913, -45.81280302780699998, -26.04903467481380019 ) ) ;
#2189 = DIRECTION ( 'NONE',  ( 0.8660254037844387076, 0.4999999999999998890, 0.000000000000000000 ) ) ;
#2190 = CARTESIAN_POINT ( 'NONE',  ( 20.11810193263714552, -8.703685627498805033, -63.17433625578833301 ) ) ;
#2191 = EDGE_CURVE ( 'NONE', #48341, #7094, #21775, .T. ) ;
#2192 = LINE ( 'NONE', #13737, #42701 ) ;
#2193 = EDGE_LOOP ( 'NONE', ( #5154, #18273, #39175, #11087 ) ) ;
#2194 = DIRECTION ( 'NONE',  ( 0.000000000000000000, 0.000000000000000000, -1.000000000000000000 ) ) ;
#2195 = DIRECTION ( 'NONE',  ( 0.000000000000000000, -1.000000000000000000, 0.000000000000000000 ) ) ;
#2196 = AXIS2_PLACEMENT_3D ( 'NONE', #50565, #2611, #14655 ) ;
#2197 = EDGE_CURVE ( 'NONE', #1545, #19377, #26208, .T. ) ;
#2198 = ORIENTED_EDGE ( 'NONE', *, *, #35446, .T. ) ;
#2199 = CARTESIAN_POINT ( 'NONE',  ( 49.86167560267210064, -45.58438661543760162, -11.84535681539230012 ) ) ;
#2200 = AXIS2_PLACEMENT_3D ( 'NONE', #41223, #45423, #17890 ) ;
#2201 = CARTESIAN_POINT ( 'NONE',  ( 24.04034479754921705, -15.90769644645291159, -33.80405724268722167 ) ) ;
#2202 = CARTESIAN_POINT ( 'NONE',  ( 14.50346589897350036, 19.73949337933519743, -21.59847332898520023 ) ) ;
#2203 = CARTESIAN_POINT ( 'NONE',  ( 21.43993832425762847, -20.26257607252427206, -49.07611398817140724 ) ) ;
#2204 = CARTESIAN_POINT ( 'NONE',  ( 29.99034385824719706, -15.61618894467929941, -24.14999999999999858 ) ) ;
#2205 = CARTESIAN_POINT ( 'NONE',  ( 46.95605112289660354, -54.29280230291429632, -75.52284329973289800 ) ) ;
#2206 = CARTESIAN_POINT ( 'NONE',  ( 64.89208931730020424, 12.18390113865149971, -10.41451813566090046 ) ) ;
#2207 = CARTESIAN_POINT ( 'NONE',  ( 47.03372200559340399, 13.88381105525409964, -8.530834882583718581 ) ) ;
#2208 = DIRECTION ( 'NONE',  ( 1.000000000000000000, 0.000000000000000000, 0.000000000000000000 ) ) ;
#2210 = AXIS2_PLACEMENT_3D ( 'NONE', #29549, #18022, #14093 ) ;
#2209 = CARTESIAN_POINT ( 'NONE',  ( 53.64468172387730505, 20.03465317324409867, -75.63087525020739577 ) ) ;
#2211 = CARTESIAN_POINT ( 'NONE',  ( 61.43364056055730060, 13.93410018439400133, -28.15121868926310000 ) ) ;
#2212 = CARTESIAN_POINT ( 'NONE',  ( 15.98404599893290090, -7.372388041690080662, -35.00188151829029692 ) ) ;
#2213 = VERTEX_POINT ( 'NONE', #37770 ) ;
#2214 = AXIS2_PLACEMENT_3D ( 'NONE', #10095, #29476, #45221 ) ;
#2215 = LINE ( 'NONE', #21588, #48947 ) ;
#2216 = CARTESIAN_POINT ( 'NONE',  ( 5.980931312570809233, -59.92332712615679924, -13.42879642680019892 ) ) ;
#2217 = LINE ( 'NONE', #50174, #35402 ) ;
#2218 = CARTESIAN_POINT ( 'NONE',  ( 72.78068555023349973, 1.369286338573830086, -68.98634353402660224 ) ) ;
#2219 = CARTESIAN_POINT ( 'NONE',  ( 19.57495879260927296, -55.46790799353475165, -75.52237511312991103 ) ) ;
#2220 = CARTESIAN_POINT ( 'NONE',  ( 3.633937397696210159, -22.83306730954970121, -34.64999999999999858 ) ) ;
#2221 = CONICAL_SURFACE ( 'NONE', #31492, 0.6299999999999942313, 0.7853981633974476129 ) ;
#2222 = ADVANCED_FACE ( 'NONE', ( #17842 ), #6318, .T. ) ;
#2223 = LINE ( 'NONE', #18200, #30963 ) ;
#2224 = CARTESIAN_POINT ( 'NONE',  ( 40.73531902818009343, 13.41031014730079995, -4.523453215150309958 ) ) ;
#2225 = CARTESIAN_POINT ( 'NONE',  ( 47.32200660942530845, -54.12888409431639758, -75.47293010958831871 ) ) ;
#2226 = CARTESIAN_POINT ( 'NONE',  ( 34.13393739769620083, -15.61618894467929941, -18.58999999999999986 ) ) ;
#2227 = AXIS2_PLACEMENT_3D ( 'NONE', #6594, #22558, #33324 ) ;
#2228 = DIRECTION ( 'NONE',  ( 0.000000000000000000, 0.000000000000000000, -1.000000000000000000 ) ) ;
#2229 = ADVANCED_FACE ( 'NONE', ( #2374 ), #25329, .F. ) ;
#2230 = CARTESIAN_POINT ( 'NONE',  ( 22.81411437884488791, -16.71916889329374811, -62.50490964971036334 ) ) ;
#2231 = FACE_OUTER_BOUND ( 'NONE', #31489, .T. ) ;
#2232 = ADVANCED_FACE ( 'NONE', ( #27242 ), #15719, .T. ) ;
#2233 = VERTEX_POINT ( 'NONE', #23556 ) ;
#2234 = CARTESIAN_POINT ( 'NONE',  ( 18.78540261209650097, -8.653687486498709447, -54.68316420314759796 ) ) ;
#2235 = CARTESIAN_POINT ( 'NONE',  ( 63.66985334848389044, 1.334524132314560019, -61.83332299293069667 ) ) ;
#2236 = ORIENTED_EDGE ( 'NONE', *, *, #23575, .T. ) ;
#2237 = CARTESIAN_POINT ( 'NONE',  ( 19.54194422072443516, -21.52909115720838429, -68.78615194735675686 ) ) ;
#2238 = FACE_OUTER_BOUND ( 'NONE', #30126, .T. ) ;
#2239 = DIRECTION ( 'NONE',  ( 0.000000000000000000, 0.000000000000000000, -1.000000000000000000 ) ) ;
#2240 = CARTESIAN_POINT ( 'NONE',  ( 16.14559401701608365, -23.52718254156647149, -62.00720200095474155 ) ) ;
#2242 = CARTESIAN_POINT ( 'NONE',  ( 11.27235727644277929, -9.289949671220924188, -35.08399737537874330 ) ) ;
#2241 = CARTESIAN_POINT ( 'NONE',  ( 43.63810915241377586, 8.691766788974046420, -68.41189615741917862 ) ) ;
#2243 = DIRECTION ( 'NONE',  ( -0.6047562208151069374, 0.7964106436917012255, 0.000000000000000000 ) ) ;
#2244 = DIRECTION ( 'NONE',  ( 0.000000000000000000, 1.000000000000000000, 0.000000000000000000 ) ) ;
#2245 = ORIENTED_EDGE ( 'NONE', *, *, #26707, .F. ) ;
#2246 = ORIENTED_EDGE ( 'NONE', *, *, #46970, .F. ) ;
#2247 = ORIENTED_EDGE ( 'NONE', *, *, #18614, .F. ) ;
#2248 = CARTESIAN_POINT ( 'NONE',  ( 61.28608632866890105, -45.23041223059910010, -46.37198050166980323 ) ) ;
#2249 =( BOUNDED_CURVE ( )  B_SPLINE_CURVE ( 3, ( #25269, #28685, #37085, #12995 ),
 .UNSPECIFIED., .F., .T. ) 
 B_SPLINE_CURVE_WITH_KNOTS ( ( 4, 4 ),
 ( 1.570796326794895226, 2.356194490192482505 ),
 .UNSPECIFIED. ) 
 CURVE ( )  GEOMETRIC_REPRESENTATION_ITEM ( )  RATIONAL_B_SPLINE_CURVE ( ( 1.000000000000000000, 0.9492530216741734694, 0.9492530216741734694, 1.000000000000000000 ) ) 
 REPRESENTATION_ITEM ( '' )  );
#2250 = FACE_OUTER_BOUND ( 'NONE', #33222, .T. ) ;
#2251 = AXIS2_PLACEMENT_3D ( 'NONE', #50041, #37466, #29839 ) ;
#2252 = EDGE_LOOP ( 'NONE', ( #37375, #21111 ) ) ;
#2253 = ADVANCED_FACE ( 'NONE', ( #43259 ), #39316, .T. ) ;
#2254 = ORIENTED_EDGE ( 'NONE', *, *, #29257, .T. ) ;
#2255 = CARTESIAN_POINT ( 'NONE',  ( -0.4410626023037880206, -27.49517073325580085, -35.14999999999999858 ) ) ;
#2256 = CARTESIAN_POINT ( 'NONE',  ( 58.92073396209919878, -28.11618894467929763, -15.65000000000000036 ) ) ;
#2257 = ORIENTED_EDGE ( 'NONE', *, *, #7986, .F. ) ;
#2258 = DIRECTION ( 'NONE',  ( 0.000000000000000000, 0.000000000000000000, -1.000000000000000000 ) ) ;
#2259 = CARTESIAN_POINT ( 'NONE',  ( 52.69947344156820179, -50.44413467004440577, -76.74590226450008856 ) ) ;
#2260 = CARTESIAN_POINT ( 'NONE',  ( 61.00673202071669721, 14.19811893154319904, -47.28177263109790118 ) ) ;
#2261 = AXIS2_PLACEMENT_3D ( 'NONE', #7012, #10682, #35290 ) ;
#2262 = CARTESIAN_POINT ( 'NONE',  ( 22.20860492341360271, -20.58460539698850056, -76.23071345245209329 ) ) ;
#2263 = LINE ( 'NONE', #25822, #41461 ) ;
#2264 = CARTESIAN_POINT ( 'NONE',  ( 41.54742305948139602, 13.60457115157169916, -5.527274669639810512 ) ) ;
#2265 = CARTESIAN_POINT ( 'NONE',  ( 41.89087153576700473, -43.57633437332699344, -3.657595758776970296 ) ) ;
#2266 = CARTESIAN_POINT ( 'NONE',  ( 65.36617373303984380, -0.6361151674937697287, -16.64867384814720808 ) ) ;
#2267 = CARTESIAN_POINT ( 'NONE',  ( 65.70575104159891566, 1.626048249155310099, -18.95023426183129800 ) ) ;
#2268 = CARTESIAN_POINT ( 'NONE',  ( 64.49087712817019735, 1.421946872762799963, -70.08110891980980739 ) ) ;
#2269 = CARTESIAN_POINT ( 'NONE',  ( 47.10914403122639982, 8.080609220371670176, -53.83103343289329956 ) ) ;
#2270 = CARTESIAN_POINT ( 'NONE',  ( 54.17308945005400034, -50.61618894467930119, -77.01198594373980200 ) ) ;
#2271 = ORIENTED_EDGE ( 'NONE', *, *, #43902, .T. ) ;
#2272 = CARTESIAN_POINT ( 'NONE',  ( 14.92239907274469957, -52.74444847917729362, -76.12391999848780699 ) ) ;
#2273 = AXIS2_PLACEMENT_3D ( 'NONE', #10654, #41579, #30021 ) ;
#2274 = CARTESIAN_POINT ( 'NONE',  ( 47.18324198357289845, -54.80726809202429450, -54.61058319554170026 ) ) ;
#2275 = CARTESIAN_POINT ( 'NONE',  ( 14.28038400710302724, 10.53025766472732450, -34.79644660940672907 ) ) ;
#2276 = CARTESIAN_POINT ( 'NONE',  ( 16.13393739769620083, -15.61618894467929941, -32.14999999999999858 ) ) ;
#2277 = DIRECTION ( 'NONE',  ( 0.000000000000000000, -1.000000000000000000, 0.000000000000000000 ) ) ;
#2278 = CARTESIAN_POINT ( 'NONE',  ( 63.50390619396989678, 1.388715606738730068, -68.72506404892941134 ) ) ;
#2279 = CARTESIAN_POINT ( 'NONE',  ( 48.21851895114659925, -54.27397483391509780, -55.06726167884789902 ) ) ;
#2280 = CARTESIAN_POINT ( 'NONE',  ( 22.00814659180725386, -11.71282814676025730, -50.66049260946093824 ) ) ;
#2281 = EDGE_CURVE ( 'NONE', #1516, #43574, #3420, .T. ) ;
#2282 = CARTESIAN_POINT ( 'NONE',  ( -10.89209614962082995, -42.33678087180149419, -6.195842417289838089 ) ) ;
#2283 = CARTESIAN_POINT ( 'NONE',  ( 12.14974942666175828, -22.52868013065419461, -46.45904183493432527 ) ) ;
#2284 = CARTESIAN_POINT ( 'NONE',  ( 47.83780165944460094, 23.21886414354259998, -55.23279884646720461 ) ) ;
#2285 = ORIENTED_EDGE ( 'NONE', *, *, #1888, .F. ) ;
#2286 = CARTESIAN_POINT ( 'NONE',  ( 9.148329271428000453, -14.64467554761950119, -71.89116613449289162 ) ) ;
#2287 = ORIENTED_EDGE ( 'NONE', *, *, #49546, .F. ) ;
#2288 = CARTESIAN_POINT ( 'NONE',  ( 71.42224537953511287, 1.096044978595170027, -70.62064874955129312 ) ) ;
#2289 = CARTESIAN_POINT ( 'NONE',  ( 0.3209249304026170480, -50.71887597443840434, -35.14999999999999858 ) ) ;
#2290 = CIRCLE ( 'NONE', #19013, 0.5000000000000000000 ) ;
#2291 = CARTESIAN_POINT ( 'NONE',  ( 83.69028012310354825, 13.83793465666272482, -47.49659995924119471 ) ) ;
#2292 = CARTESIAN_POINT ( 'NONE',  ( 18.20470697638991808, -7.911114290554745132, -41.09100108441210608 ) ) ;
#2294 = CARTESIAN_POINT ( 'NONE',  ( 55.86629951729040044, 14.73742367376410023, -25.42247174273690291 ) ) ;
#2293 = CARTESIAN_POINT ( 'NONE',  ( 84.43354761919439966, 12.07319023258030022, -47.41425570151039892 ) ) ;
#2295 = CARTESIAN_POINT ( 'NONE',  ( 9.350953455536869185, -17.54846419477570052, -79.36448291391718612 ) ) ;
#2296 = DIRECTION ( 'NONE',  ( 1.062456999999999985E-16, -7.719205000000000365E-17, 1.000000000000000000 ) ) ;
#2297 = CARTESIAN_POINT ( 'NONE',  ( 17.16957190133613054, -7.705201370156754770, -67.33399687314600612 ) ) ;
#2298 = DIRECTION ( 'NONE',  ( 0.000000000000000000, 0.000000000000000000, -1.000000000000000000 ) ) ;
#2299 = VERTEX_POINT ( 'NONE', #47448 ) ;
#2300 = CARTESIAN_POINT ( 'NONE',  ( 8.644451877215889368, -48.75768716228870403, -35.10565360069929852 ) ) ;
#2301 = ORIENTED_EDGE ( 'NONE', *, *, #34873, .F. ) ;
#2302 = ORIENTED_EDGE ( 'NONE', *, *, #11741, .T. ) ;
#2303 = CARTESIAN_POINT ( 'NONE',  ( 12.32961272725700219, -64.64439898424720354, -15.85993007182080028 ) ) ;
#2304 = CARTESIAN_POINT ( 'NONE',  ( 8.602773590722975428, -13.11400814803269732, -38.60984802764800605 ) ) ;
#2305 = CARTESIAN_POINT ( 'NONE',  ( 11.67619942398430055, 33.65927571709689659, -45.08494251881550241 ) ) ;
#2306 = FACE_OUTER_BOUND ( 'NONE', #27368, .T. ) ;
#2307 = ORIENTED_EDGE ( 'NONE', *, *, #27466, .F. ) ;
#2308 = ORIENTED_EDGE ( 'NONE', *, *, #15977, .F. ) ;
#2309 = EDGE_CURVE ( 'NONE', #34738, #45666, #19276, .T. ) ;
#2310 = CARTESIAN_POINT ( 'NONE',  ( -13.76835980061299836, -41.17840569159340447, -47.00285061395300090 ) ) ;
#2311 = CARTESIAN_POINT ( 'NONE',  ( 63.93393739769684458, 10.88381105532090487, -69.84999999999980957 ) ) ;
#2312 = CARTESIAN_POINT ( 'NONE',  ( 51.76793811538249912, 19.62547313263230109, -50.48796164790370256 ) ) ;
#2313 = EDGE_CURVE ( 'NONE', #8182, #45770, #41955, .T. ) ;
#2314 = CARTESIAN_POINT ( 'NONE',  ( 60.33936747781210386, -2.295495892611130184, -15.82216635100610169 ) ) ;
#2315 = CARTESIAN_POINT ( 'NONE',  ( 50.57709982134520033, -48.74034408314059874, -76.21964822811550277 ) ) ;
#2316 = CARTESIAN_POINT ( 'NONE',  ( 57.03554082408360415, -49.83830780016760542, -52.10329396591820483 ) ) ;
#2317 = ORIENTED_EDGE ( 'NONE', *, *, #20342, .F. ) ;
#2318 = CARTESIAN_POINT ( 'NONE',  ( 24.02155121257710846, -14.98319770599232470, -33.76684429329586123 ) ) ;
#2319 = CARTESIAN_POINT ( 'NONE',  ( 70.03247032090601465, 18.72622661238470343, -69.60146707679315625 ) ) ;
#2320 = EDGE_LOOP ( 'NONE', ( #40995, #36084, #19829, #17081 ) ) ;
#2321 = DIRECTION ( 'NONE',  ( 0.000000000000000000, -1.000000000000000000, 0.000000000000000000 ) ) ;
#2322 = CARTESIAN_POINT ( 'NONE',  ( 57.81609062655950027, -47.19091213400450613, -48.15256270216469403 ) ) ;
#2323 = CARTESIAN_POINT ( 'NONE',  ( 8.452546488159928373, -14.00902333825419888, -47.07814682104019255 ) ) ;
#2324 = CARTESIAN_POINT ( 'NONE',  ( 13.87200042841950065, -51.20037006225030751, -22.54888207536149736 ) ) ;
#2325 = CARTESIAN_POINT ( 'NONE',  ( 53.85265205760590135, 19.88976859782529871, -75.70177109258371217 ) ) ;
#2326 = CARTESIAN_POINT ( 'NONE',  ( 46.63703890305789912, -53.27462879060840351, -76.10201724918678678 ) ) ;
#2327 = CARTESIAN_POINT ( 'NONE',  ( 56.70268528983609713, 13.88381105532070059, -15.64847180727820053 ) ) ;
#2328 = CARTESIAN_POINT ( 'NONE',  ( 11.13393739769619906, 32.27621211514449584, -43.92731420739779225 ) ) ;
#2329 = CARTESIAN_POINT ( 'NONE',  ( 56.84210777396779690, -50.65785230063129774, -53.85131221196560602 ) ) ;
#2330 = AXIS2_PLACEMENT_3D ( 'NONE', #28657, #28400, #20275 ) ;
#2331 = CARTESIAN_POINT ( 'NONE',  ( 9.414480144562521247, -17.75895664038510091, -45.74891888349859670 ) ) ;
#2332 = PLANE ( 'NONE',  #17724 ) ;
#2333 = ORIENTED_EDGE ( 'NONE', *, *, #13311, .T. ) ;
#2334 = CARTESIAN_POINT ( 'NONE',  ( 47.61403878904570064, 23.30730827445200148, -74.36225195369628693 ) ) ;
#2335 = AXIS2_PLACEMENT_3D ( 'NONE', #23663, #107, #48060 ) ;
#2336 = CARTESIAN_POINT ( 'NONE',  ( 20.10261140139872182, -55.32589573411479478, -19.54203465799566430 ) ) ;
#2337 = CARTESIAN_POINT ( 'NONE',  ( 60.34379258661509482, -45.86802437805019395, -47.72732609191810127 ) ) ;
#2338 = CARTESIAN_POINT ( 'NONE',  ( 53.63393739769619373, -63.11618894467929408, 16.35000000000000142 ) ) ;
#2339 = CARTESIAN_POINT ( 'NONE',  ( 51.50424210664085223, -51.12586965113519710, 11.97999999999999865 ) ) ;
#2340 = DIRECTION ( 'NONE',  ( 1.000000000000000000, -4.005157696510369650E-32, -3.556943099846429769E-14 ) ) ;
#2341 = LINE ( 'NONE', #34817, #50999 ) ;
#2342 = CARTESIAN_POINT ( 'NONE',  ( -0.1635911377674279799, 19.81675348476660048, -35.29985221058469591 ) ) ;
#2344 = CARTESIAN_POINT ( 'NONE',  ( 42.32416139106639008, -38.87540147440780913, -78.75518257947804557 ) ) ;
#2343 = DIRECTION ( 'NONE',  ( 0.000000000000000000, 0.000000000000000000, 1.000000000000000000 ) ) ;
#2345 = EDGE_CURVE ( 'NONE', #17152, #35735, #24333, .T. ) ;
#2346 = FACE_OUTER_BOUND ( 'NONE', #6063, .T. ) ;
#2347 = CARTESIAN_POINT ( 'NONE',  ( 6.312816564084299920, 31.89199177866499468, -47.22137548220790393 ) ) ;
#2348 = VERTEX_POINT ( 'NONE', #48204 ) ;
#2349 = CARTESIAN_POINT ( 'NONE',  ( 52.69435697169009813, -49.74608733290399698, -48.50602906872329356 ) ) ;
#2350 = ORIENTED_EDGE ( 'NONE', *, *, #46645, .F. ) ;
#2351 = DIRECTION ( 'NONE',  ( 0.000000000000000000, 0.000000000000000000, -1.000000000000000000 ) ) ;
#2352 = CARTESIAN_POINT ( 'NONE',  ( 12.72604580451289813, -9.703220991147921026, -41.78615335765307037 ) ) ;
#2353 = CARTESIAN_POINT ( 'NONE',  ( 14.21330390444039971, 19.89053608221549752, -22.50776184251580148 ) ) ;
#2354 = CARTESIAN_POINT ( 'NONE',  ( 51.13393739769620083, 19.38381105532069881, 11.97999999999999865 ) ) ;
#2355 = CARTESIAN_POINT ( 'NONE',  ( 15.45594426927969955, -22.63636586655560023, -44.98346683230629850 ) ) ;
#2356 = DIRECTION ( 'NONE',  ( 0.000000000000000000, 0.000000000000000000, 1.000000000000000000 ) ) ;
#2357 = CARTESIAN_POINT ( 'NONE',  ( 52.80437707413480553, 18.46123689847469862, -48.85649626243960597 ) ) ;
#2358 = CARTESIAN_POINT ( 'NONE',  ( 55.34109141907249807, -45.97060569714729894, -16.40367016765270236 ) ) ;
#2359 = DIRECTION ( 'NONE',  ( 0.000000000000000000, -1.000000000000000000, 0.000000000000000000 ) ) ;
#2360 = VERTEX_POINT ( 'NONE', #13102 ) ;
#2361 = CARTESIAN_POINT ( 'NONE',  ( 18.42797611233919852, -8.527907785417399467, -80.66697359201479856 ) ) ;
#2362 = CYLINDRICAL_SURFACE ( 'NONE', #1015, 40.00000000000000711 ) ;
#2363 = CARTESIAN_POINT ( 'NONE',  ( 9.002245878291878611, 32.05387020899590311, -46.62846274566239657 ) ) ;
#2364 = CARTESIAN_POINT ( 'NONE',  ( 72.83834671619840151, 1.382830464309369844, -62.68920552647019662 ) ) ;
#2365 = CARTESIAN_POINT ( 'NONE',  ( 11.17220089305429909, -65.21595029614879024, -17.67193522364469871 ) ) ;
#2366 = CARTESIAN_POINT ( 'NONE',  ( 53.12218299101002117, -49.57312743959001722, -49.13784299743716133 ) ) ;
#2367 = CARTESIAN_POINT ( 'NONE',  ( 24.04521450903870061, -15.61618868716203501, -63.50766715510244609 ) ) ;
#2368 = CARTESIAN_POINT ( 'NONE',  ( 22.86433249997304884, -14.89035933162552539, -62.41863209491601339 ) ) ;
#2369 = CIRCLE ( 'NONE', #18252, 1.999999999999997113 ) ;
#2370 = CARTESIAN_POINT ( 'NONE',  ( 16.13393739769620083, -15.61618894467929941, -32.14999999999999858 ) ) ;
#2371 = CARTESIAN_POINT ( 'NONE',  ( 64.86108678489050305, 1.186856010528209993, -70.56885973566789971 ) ) ;
#2372 = ORIENTED_EDGE ( 'NONE', *, *, #12854, .F. ) ;
#2373 = CARTESIAN_POINT ( 'NONE',  ( 10.13886454369750112, -63.17879643090980579, -45.99496747666990615 ) ) ;
#2374 = FACE_OUTER_BOUND ( 'NONE', #43123, .T. ) ;
#2375 = ORIENTED_EDGE ( 'NONE', *, *, #11059, .T. ) ;
#2376 = ADVANCED_FACE ( 'NONE', ( #40851 ), #12307, .T. ) ;
#2377 = CARTESIAN_POINT ( 'NONE',  ( 22.60607335269574492, -20.31847096301905609, -47.64999999999999858 ) ) ;
#2378 = CARTESIAN_POINT ( 'NONE',  ( 56.93466172174790074, 19.03186587073140146, -52.70269903729370498 ) ) ;
#2379 = CARTESIAN_POINT ( 'NONE',  ( 53.03699914620550260, 19.13327433011199830, -77.13749948101029474 ) ) ;
#2380 = ORIENTED_EDGE ( 'NONE', *, *, #19648, .F. ) ;
#2381 = DIRECTION ( 'NONE',  ( 0.000000000000000000, 0.000000000000000000, -1.000000000000000000 ) ) ;
#2382 = DIRECTION ( 'NONE',  ( 0.000000000000000000, 0.000000000000000000, 1.000000000000000000 ) ) ;
#2383 = DIRECTION ( 'NONE',  ( -9.816708849317168638E-16, 1.000000000000000000, 0.000000000000000000 ) ) ;
#2384 = DIRECTION ( 'NONE',  ( 0.000000000000000000, -9.718338800990680596E-16, 1.000000000000000000 ) ) ;
#2385 = CARTESIAN_POINT ( 'NONE',  ( 20.16438269627179736, -8.423259725569389289, -67.45490599493020056 ) ) ;
#2386 = DIRECTION ( 'NONE',  ( 1.000000000000000000, 0.000000000000000000, 0.000000000000000000 ) ) ;
#2387 = CARTESIAN_POINT ( 'NONE',  ( 43.88839816904001623, -37.90263197162346387, -70.87765394619944459 ) ) ;
#2388 = ORIENTED_EDGE ( 'NONE', *, *, #27241, .F. ) ;
#2389 = CARTESIAN_POINT ( 'NONE',  ( 56.77148119808899907, -46.03634836625910509, -26.24810600973490082 ) ) ;
#2390 = CARTESIAN_POINT ( 'NONE',  ( 15.41773806569820060, -23.03196620144690243, -44.76330392965540028 ) ) ;
#2391 = DIRECTION ( 'NONE',  ( -0.000000000000000000, -1.000000000000000000, -0.000000000000000000 ) ) ;
#2392 = CARTESIAN_POINT ( 'NONE',  ( 13.50200499130249909, 20.63642445556759952, -74.86150924066380696 ) ) ;
#2393 = CARTESIAN_POINT ( 'NONE',  ( 8.222961267541252894, -14.58046671945546002, -50.83399806724860071 ) ) ;
#2394 = CARTESIAN_POINT ( 'NONE',  ( 42.70541728070560339, -45.00675845543869968, -6.147241989062049328 ) ) ;
#2395 = CARTESIAN_POINT ( 'NONE',  ( 24.04493710079389146, -15.61360612403737314, -61.50757231037331962 ) ) ;
#2396 = AXIS2_PLACEMENT_3D ( 'NONE', #6919, #2980, #7172 ) ;
#2397 = CARTESIAN_POINT ( 'NONE',  ( 19.43325479052089833, -23.17245954930830010, -59.87662587226670041 ) ) ;
#2398 = ORIENTED_EDGE ( 'NONE', *, *, #32972, .F. ) ;
#2399 = CARTESIAN_POINT ( 'NONE',  ( 53.27340400499669926, -49.09268838209659691, -26.76986176472670209 ) ) ;
#2400 = CARTESIAN_POINT ( 'NONE',  ( 55.46462020123170333, -50.75003295001909720, -75.55576601992819974 ) ) ;
#2402 = CARTESIAN_POINT ( 'NONE',  ( 46.98749101202549383, -39.23094825485602399, -34.79644638567071269 ) ) ;
#2401 = CARTESIAN_POINT ( 'NONE',  ( 11.43906257866700038, 33.09497493101680021, -15.68575602140459857 ) ) ;
#2403 = EDGE_CURVE ( 'NONE', #5979, #8568, #16842, .T. ) ;
#2404 = AXIS2_PLACEMENT_3D ( 'NONE', #33345, #24688, #49361 ) ;
#2405 = CARTESIAN_POINT ( 'NONE',  ( 47.35501076093819961, -54.67813530284840340, -54.64069690081250030 ) ) ;
#2406 = CYLINDRICAL_SURFACE ( 'NONE', #28182, 7.910999999999997812 ) ;
#2407 = VERTEX_POINT ( 'NONE', #44789 ) ;
#2408 = FACE_OUTER_BOUND ( 'NONE', #1734, .T. ) ;
#2409 = EDGE_CURVE ( 'NONE', #30947, #24819, #31893, .T. ) ;
#2410 = CARTESIAN_POINT ( 'NONE',  ( 47.55449607009450119, 23.31128263483790164, -54.66330429744959218 ) ) ;
#2411 = CARTESIAN_POINT ( 'NONE',  ( 11.65531868176484487, -9.064193434896999690, -65.10144457859644262 ) ) ;
#2412 = DIRECTION ( 'NONE',  ( -1.000000000000000000, 0.000000000000000000, 0.000000000000000000 ) ) ;
#2413 = DIRECTION ( 'NONE',  ( 0.4156269377774536866, -0.5720614028176834731, 0.7071067811865480168 ) ) ;
#2414 = CARTESIAN_POINT ( 'NONE',  ( 11.31571024077640075, 33.79537190493880416, -16.86897517425000004 ) ) ;
#2415 = ADVANCED_FACE ( 'NONE', ( #8373 ), #5482, .T. ) ;
#2416 = CARTESIAN_POINT ( 'NONE',  ( 51.67588099511389998, 17.45826125070719925, -77.01364301606231777 ) ) ;
#2417 = CARTESIAN_POINT ( 'NONE',  ( 53.27426930170610575, 18.19673474085740139, -48.84492426196599979 ) ) ;
#2418 = DIRECTION ( 'NONE',  ( 0.000000000000000000, -1.000000000000000000, 0.000000000000000000 ) ) ;
#2419 = CARTESIAN_POINT ( 'NONE',  ( 58.40646430935630207, -46.88458887768990735, -48.04310473389099911 ) ) ;
#2420 = CARTESIAN_POINT ( 'NONE',  ( 54.16532707871409968, 17.12274662488560040, -26.76512942855410060 ) ) ;
#2421 = DIRECTION ( 'NONE',  ( 0.000000000000000000, 1.000000000000000000, 0.000000000000000000 ) ) ;
#2422 = CARTESIAN_POINT ( 'NONE',  ( 63.53378487636381067, 1.392489938374319891, -68.91992234782470916 ) ) ;
#2423 = CARTESIAN_POINT ( 'NONE',  ( 53.36465014982429977, 18.25085194934079880, -49.20420490330940311 ) ) ;
#2424 = CARTESIAN_POINT ( 'NONE',  ( 46.03121886948380137, -45.11618894467940066, -7.582877905987319700 ) ) ;
#2425 = CARTESIAN_POINT ( 'NONE',  ( 9.367299438200719308, -15.61632798465739924, -73.84717978381010539 ) ) ;
#2426 = CARTESIAN_POINT ( 'NONE',  ( 10.76899899952330131, 31.88305279702909800, -45.20723331625340791 ) ) ;
#2427 = CARTESIAN_POINT ( 'NONE',  ( 72.85979347688879670, 0.9828917932958439740, -61.95210570009940199 ) ) ;
#2428 = EDGE_CURVE ( 'NONE', #32624, #4643, #25526, .T. ) ;
#2429 = DIRECTION ( 'NONE',  ( 0.6676418852214537347, -0.2329255526947816568, 0.7071067811863875896 ) ) ;
#2430 = EDGE_LOOP ( 'NONE', ( #48923, #24938, #29146, #19387 ) ) ;
#2431 = CARTESIAN_POINT ( 'NONE',  ( 18.50686101264880179, 20.06273318926150040, -74.35769860268439402 ) ) ;
#2432 = VERTEX_POINT ( 'NONE', #21179 ) ;
#2433 = ORIENTED_EDGE ( 'NONE', *, *, #28309, .F. ) ;
#2434 = CARTESIAN_POINT ( 'NONE',  ( 41.50224533218029421, 12.67611161623769966, -3.489448898335199889 ) ) ;
#2435 = CARTESIAN_POINT ( 'NONE',  ( 49.41913868843145252, -2.245867004874552819, -15.72629724680255414 ) ) ;
#2436 = ORIENTED_EDGE ( 'NONE', *, *, #33166, .T. ) ;
#2437 = ADVANCED_FACE ( 'NONE', ( #20661 ), #21573, .T. ) ;
#2438 = CARTESIAN_POINT ( 'NONE',  ( 11.15230508032369805, -64.00960885307659964, -44.57032717116720022 ) ) ;
#2439 = CARTESIAN_POINT ( 'NONE',  ( 56.21080665499489726, -45.60151275163879347, -25.51026796885810199 ) ) ;
#2440 = CARTESIAN_POINT ( 'NONE',  ( 23.61408947799745661, -18.30540000354351449, -77.61739823543270234 ) ) ;
#2441 = CARTESIAN_POINT ( 'NONE',  ( 16.13393739769620083, -15.61618894467929941, -23.15000000000000213 ) ) ;
#2442 = ORIENTED_EDGE ( 'NONE', *, *, #1408, .T. ) ;
#2443 = CARTESIAN_POINT ( 'NONE',  ( -31.36606260230380272, -63.11618894467929408, 10.84999999999999964 ) ) ;
#2444 = TOROIDAL_SURFACE ( 'NONE', #24181, 17.07000000028409659, 3.569999999987189643 ) ;
#2445 = CARTESIAN_POINT ( 'NONE',  ( 47.09446252081839646, 7.025840437962705742, -54.84737438438714463 ) ) ;
#2446 = CARTESIAN_POINT ( 'NONE',  ( 16.13393739769620083, -27.61618894467930474, -22.14999999999999858 ) ) ;
#2447 = CIRCLE ( 'NONE', #9145, 5.500000000000005329 ) ;
#2448 = CIRCLE ( 'NONE', #15836, 10.00000000000000711 ) ;
#2449 = ORIENTED_EDGE ( 'NONE', *, *, #15158, .T. ) ;
#2450 = CARTESIAN_POINT ( 'NONE',  ( 8.174661525294158793, -13.46383032146310121, -36.87639860437320038 ) ) ;
#2451 = DIRECTION ( 'NONE',  ( 0.000000000000000000, 0.000000000000000000, 1.000000000000000000 ) ) ;
#2452 = AXIS2_PLACEMENT_3D ( 'NONE', #39112, #35156, #43556 ) ;
#2453 = CARTESIAN_POINT ( 'NONE',  ( 16.22101879095299992, 19.83813843325669879, -20.26096174765840274 ) ) ;
#2454 = CARTESIAN_POINT ( 'NONE',  ( 16.59010301012261834, -22.43865132935006201, -50.93120400185586050 ) ) ;
#2455 = CARTESIAN_POINT ( 'NONE',  ( 14.36263005250068758, -22.20704640813376685, -47.03613900106096679 ) ) ;
#2456 = DIRECTION ( 'NONE',  ( -0.3918900565005491998, 0.9200120562340454722, 0.000000000000000000 ) ) ;
#2457 = CARTESIAN_POINT ( 'NONE',  ( 47.27368826427839821, -54.50755326446490301, -75.00321679105040573 ) ) ;
#2458 = CARTESIAN_POINT ( 'NONE',  ( 43.23251398108950383, 13.74603371045659905, -6.010618268419490207 ) ) ;
#2459 = EDGE_CURVE ( 'NONE', #50858, #4288, #18686, .T. ) ;
#2460 = FACE_OUTER_BOUND ( 'NONE', #41298, .T. ) ;
#2461 = CARTESIAN_POINT ( 'NONE',  ( 53.35839899967449895, 20.15050419475459975, -75.63635010498570921 ) ) ;
#2462 = CARTESIAN_POINT ( 'NONE',  ( 61.75043778037309750, 13.88381108430640154, -28.15157759350370270 ) ) ;
#2463 = CARTESIAN_POINT ( 'NONE',  ( 8.447399571967670440, -14.03382222439730143, -78.35213070062989971 ) ) ;
#2464 = ORIENTED_EDGE ( 'NONE', *, *, #10308, .F. ) ;
#2465 = DIRECTION ( 'NONE',  ( -0.5516667872527503125, 0.8340645993220362486, -1.942890293094025918E-16 ) ) ;
#2466 = CARTESIAN_POINT ( 'NONE',  ( 5.641888144657690063, -58.94988526653390437, -11.71462473494669965 ) ) ;
#2467 = CARTESIAN_POINT ( 'NONE',  ( 75.05098508634559096, -12.48077121835190084, -11.32537598484450037 ) ) ;
#2468 = DIRECTION ( 'NONE',  ( 0.000000000000000000, 0.000000000000000000, -1.000000000000000000 ) ) ;
#2469 = DIRECTION ( 'NONE',  ( 0.8529218806139627906, -0.5196445842661518988, -0.04993767728678798895 ) ) ;
#2470 = AXIS2_PLACEMENT_3D ( 'NONE', #45539, #29780, #32673 ) ;
#2471 = AXIS2_PLACEMENT_3D ( 'NONE', #48276, #29123, #1093 ) ;
#2472 = PLANE ( 'NONE',  #49858 ) ;
#2473 = AXIS2_PLACEMENT_3D ( 'NONE', #9175, #28, #16252 ) ;
#2474 = CARTESIAN_POINT ( 'NONE',  ( 8.633937397695980565, 17.54628985290149856, -34.64999999999999858 ) ) ;
#2475 = AXIS2_PLACEMENT_3D ( 'NONE', #37544, #6618, #10030 ) ;
#2476 = CARTESIAN_POINT ( 'NONE',  ( 82.50625024752521597, -45.42892848413679729, -47.45620293274949830 ) ) ;
#2477 = CARTESIAN_POINT ( 'NONE',  ( 13.65323342483580049, 20.15922856511949846, -23.15000000000000213 ) ) ;
#2478 = CONICAL_SURFACE ( 'NONE', #31749, 0.7350000000000010969, 0.06981317007977388966 ) ;
#2479 = CARTESIAN_POINT ( 'NONE',  ( 41.88234443671479568, 12.44058544459540094, -3.969549609002189783 ) ) ;
#2480 = EDGE_CURVE ( 'NONE', #40057, #16152, #2840, .T. ) ;
#2481 = CARTESIAN_POINT ( 'NONE',  ( 65.08882305123219680, 1.387412027389909985, -70.29005197907430613 ) ) ;
#2482 = B_SPLINE_CURVE_WITH_KNOTS ( 'NONE', 3,
 ( #11034, #2910, #6581, #27512, #11291, #31174, #27252, #3686, #14696, #3168, #31428, #46949, #43266, #43514, #14955, #7618, #46690, #42492 ),
 .UNSPECIFIED., .F., .F.,
 ( 4, 2, 2, 2, 2, 2, 2, 2, 4 ),
 ( 0.3486532883837264452, 0.4300716273357606534, 0.5114899662877948616, 0.5929083052398289588, 0.6743266441918631671, 0.7557449831438973753, 0.8371633220959315835, 0.9185816610479657918, 1.000000000000000000 ),
 .UNSPECIFIED. ) ;
#2483 = CARTESIAN_POINT ( 'NONE',  ( 19.86710128871024850, 24.20909934830549659, -75.14570525072024054 ) ) ;
#2484 = CARTESIAN_POINT ( 'NONE',  ( 66.23540447448814916, -49.95860450174190248, -75.14853292321149070 ) ) ;
#2485 = CIRCLE ( 'NONE', #25876, 3.000000000000003997 ) ;
#2486 = CARTESIAN_POINT ( 'NONE',  ( 22.55531972313694666, -17.79662447378222367, -62.55699137843335933 ) ) ;
#2487 = CARTESIAN_POINT ( 'NONE',  ( 18.50685669541299916, -51.29511715723860732, -74.14992839339309683 ) ) ;
#2488 = B_SPLINE_CURVE_WITH_KNOTS ( 'NONE', 3,
 ( #34929, #47272, #15026, #30993, #11106, #28086, #51450, #19723, #39649, #19965, #43331, #44091, #43836, #35963, #39141, #47520, #11359, #7937, #3755, #7424, #8192, #27070, #43076, #24135, #23373, #40160, #31754, #39395, #11616, #27581, #43584, #35715, #51699, #15792, #47774, #11880, #8974 ),
 .UNSPECIFIED., .F., .F.,
 ( 4, 2, 2, 2, 2, 2, 2, 2, 2, 2, 2, 2, 2, 2, 1, 1, 1, 1, 1, 2, 4 ),
 ( 0.000000000000000000, 0.03125019491472925265, 0.06250038982945850530, 0.09375058474418775101, 0.1250007796589170106, 0.1562509745736462563, 0.1875011694883755020, 0.2187513644031047477, 0.2500015593178340212, 0.3125019491472925681, 0.3750023389767511151, 0.4375027288062096620, 0.4687529237209391297, 0.4843780211783040301, 0.4921905699069865081, 0.4960968442713278859, 0.4980499814534985470, 0.4990265500445839053, 0.4995148343401266122, 0.4997589764878979657, 0.5000031186356694857 ),
 .UNSPECIFIED. ) ;
#2489 = LINE ( 'NONE', #9580, #519 ) ;
#2490 = VERTEX_POINT ( 'NONE', #19838 ) ;
#2491 = CARTESIAN_POINT ( 'NONE',  ( 12.43868033672440099, -22.08548331050309699, -53.73253703038420070 ) ) ;
#2492 = CARTESIAN_POINT ( 'NONE',  ( 63.47413392627220219, 1.313759828079400060, -62.14118152289400143 ) ) ;
#2493 = VERTEX_POINT ( 'NONE', #3868 ) ;
#2494 = CARTESIAN_POINT ( 'NONE',  ( -10.41130465719239950, 11.60708275212090079, -6.431269174833519564 ) ) ;
#2495 = DIRECTION ( 'NONE',  ( 0.000000000000000000, 0.000000000000000000, 1.000000000000000000 ) ) ;
#2496 = CARTESIAN_POINT ( 'NONE',  ( 16.13393739769620083, -15.61618894467929941, -47.64999999999999858 ) ) ;
#2497 = CARTESIAN_POINT ( 'NONE',  ( 23.78344371453452410, -17.69876028378456922, -61.59227590569546607 ) ) ;
#2498 = CARTESIAN_POINT ( 'NONE',  ( 46.06102096816690050, 8.864772444052823275, -56.66258995241773277 ) ) ;
#2499 = CARTESIAN_POINT ( 'NONE',  ( 9.788743069423331278, -18.35763646220170031, -81.23899999999999011 ) ) ;
#2500 = CARTESIAN_POINT ( 'NONE',  ( 16.13393739769609780, -15.61618894467929941, 8.449999999999999289 ) ) ;
#2501 = ORIENTED_EDGE ( 'NONE', *, *, #42022, .T. ) ;
#2502 = ORIENTED_EDGE ( 'NONE', *, *, #43172, .T. ) ;
#2503 = ORIENTED_EDGE ( 'NONE', *, *, #16917, .T. ) ;
#2504 = CARTESIAN_POINT ( 'NONE',  ( 26.13393739769619728, -28.89524513604070322, -39.64999999999999858 ) ) ;
#2505 = CARTESIAN_POINT ( 'NONE',  ( 61.18213688343650603, -45.28487339755239560, -46.74705100057859397 ) ) ;
#2506 = CARTESIAN_POINT ( 'NONE',  ( 53.51474650799030286, -49.43356839336680508, -49.22562654179730401 ) ) ;
#2507 = CARTESIAN_POINT ( 'NONE',  ( 82.68190288415928535, -45.40220004952831800, -47.42733033421982469 ) ) ;
#2508 = ORIENTED_EDGE ( 'NONE', *, *, #9627, .T. ) ;
#2509 = ORIENTED_EDGE ( 'NONE', *, *, #26912, .F. ) ;
#2510 = CYLINDRICAL_SURFACE ( 'NONE', #20187, 5.499999999999998224 ) ;
#2511 = CARTESIAN_POINT ( 'NONE',  ( 19.54191378771778531, -9.703268531717034406, -54.11948898031546662 ) ) ;
#2512 = AXIS2_PLACEMENT_3D ( 'NONE', #34984, #39708, #23432 ) ;
#2513 = CIRCLE ( 'NONE', #38504, 12.00000000000000000 ) ;
#2514 = EDGE_LOOP ( 'NONE', ( #23570, #6495, #48068, #50962 ) ) ;
#2515 = CARTESIAN_POINT ( 'NONE',  ( 16.79377243150814536, -23.56734767625158256, -49.98149220073255350 ) ) ;
#2516 = CARTESIAN_POINT ( 'NONE',  ( 51.93948718480190507, -51.08957512830220082, -76.10418645920529457 ) ) ;
#2517 = VECTOR ( 'NONE', #47503, 1000.000000000000227 ) ;
#2518 = CARTESIAN_POINT ( 'NONE',  ( 60.40971711783320330, 14.45930241792809845, -47.28043267387079851 ) ) ;
#2519 = EDGE_CURVE ( 'NONE', #19450, #14121, #45321, .T. ) ;
#2520 = VECTOR ( 'NONE', #19835, 1000.000000000000114 ) ;
#2521 = CARTESIAN_POINT ( 'NONE',  ( 22.21138144903229872, -10.65116916682739934, -71.79445331288948751 ) ) ;
#2522 = ITEM_DEFINED_TRANSFORMATION ( 'NONE', 'NONE', #86,  #20940 ) ;
#2523 = EDGE_CURVE ( 'NONE', #26915, #43399, #47386, .T. ) ;
#2524 = CARTESIAN_POINT ( 'NONE',  ( 23.13393739769620083, -15.61618894467929941, -82.15000000000000568 ) ) ;
#2525 = CARTESIAN_POINT ( 'NONE',  ( 45.08955516288700238, 14.59038207675800081, -8.804749820302610885 ) ) ;
#2526 = CARTESIAN_POINT ( 'NONE',  ( 40.47914112739019998, -44.80448066467319990, -4.470311448230490647 ) ) ;
#2527 = EDGE_CURVE ( 'NONE', #6481, #19827, #11887, .T. ) ;
#2528 = CARTESIAN_POINT ( 'NONE',  ( 65.44700751694060159, -1.324274634346296775, -16.55186757724361968 ) ) ;
#2529 = CARTESIAN_POINT ( 'NONE',  ( 66.50380103983820845, 1.883526056381209512, -20.28031759223009445 ) ) ;
#2530 = LINE ( 'NONE', #22936, #6989 ) ;
#2531 = CARTESIAN_POINT ( 'NONE',  ( 46.84271081672680026, 8.424848343090520331, -54.36135291155100191 ) ) ;
#2532 = CARTESIAN_POINT ( 'NONE',  ( 74.93037295002230280, 11.88381105532070059, -15.31098073120859837 ) ) ;
#2533 = CARTESIAN_POINT ( 'NONE',  ( 13.65479182716389950, -8.170345444894159925, -52.68519703601729987 ) ) ;
#2534 = ORIENTED_EDGE ( 'NONE', *, *, #34724, .T. ) ;
#2535 = CARTESIAN_POINT ( 'NONE',  ( 57.55751162087899786, 19.14609342572249773, -52.97747665988080001 ) ) ;
#2536 = CARTESIAN_POINT ( 'NONE',  ( 71.62240088300148955, 1.377110276564099900, -70.22675574799650633 ) ) ;
#2537 = CARTESIAN_POINT ( 'NONE',  ( 44.36443571826935539, -39.98382968829412221, -64.89400308598267486 ) ) ;
#2538 = DIRECTION ( 'NONE',  ( 1.000000000000000000, 0.000000000000000000, 0.000000000000000000 ) ) ;
#2539 = CARTESIAN_POINT ( 'NONE',  ( 21.88969301003089996, -11.69594164191370034, -32.14999999999999858 ) ) ;
#2540 = EDGE_CURVE ( 'NONE', #50841, #24756, #18562, .T. ) ;
#2541 = CARTESIAN_POINT ( 'NONE',  ( 63.51391054266390768, 1.390208944942409985, -68.75457626026799574 ) ) ;
#2542 = CARTESIAN_POINT ( 'NONE',  ( 48.03324057931929758, -54.36799250499229430, -55.25634970046999683 ) ) ;
#2543 = DIRECTION ( 'NONE',  ( 1.000000000000000000, 0.000000000000000000, 0.000000000000000000 ) ) ;
#2544 = CARTESIAN_POINT ( 'NONE',  ( 56.40159749620720220, 19.40038761406519896, -53.06856178888660480 ) ) ;
#2545 = CARTESIAN_POINT ( 'NONE',  ( 47.83059346947020174, 23.21195136793840064, -55.02665008976270400 ) ) ;
#2546 = AXIS2_PLACEMENT_3D ( 'NONE', #48343, #132, #24721 ) ;
#2547 = EDGE_LOOP ( 'NONE', ( #23653, #6453, #1676 ) ) ;
#2548 = AXIS2_PLACEMENT_3D ( 'NONE', #19188, #3737, #3990 ) ;
#2549 = CARTESIAN_POINT ( 'NONE',  ( 23.17868282713410011, -15.95400683938519926, -78.86243206809150763 ) ) ;
#2550 =( BOUNDED_CURVE ( )  B_SPLINE_CURVE ( 3, ( #20735, #5036, #45385, #20471 ),
 .UNSPECIFIED., .F., .T. ) 
 B_SPLINE_CURVE_WITH_KNOTS ( ( 4, 4 ),
 ( 5.769749740152300355, 6.283185307179586232 ),
 .UNSPECIFIED. ) 
 CURVE ( )  GEOMETRIC_REPRESENTATION_ITEM ( )  RATIONAL_B_SPLINE_CURVE ( ( 1.000000000000000000, 0.9781523768112219130, 0.9781523768112219130, 1.000000000000000000 ) ) 
 REPRESENTATION_ITEM ( '' )  );
#2551 = ORIENTED_EDGE ( 'NONE', *, *, #25464, .F. ) ;
#2552 = CARTESIAN_POINT ( 'NONE',  ( 71.32344782937069283, 1.326324093417220240, -70.44093178352299844 ) ) ;
#2553 = AXIS2_PLACEMENT_3D ( 'NONE', #20985, #36982, #21499 ) ;
#2554 = CARTESIAN_POINT ( 'NONE',  ( 82.64649737942757213, 14.08998960694586344, -47.29316709580923117 ) ) ;
#2555 = DIRECTION ( 'NONE',  ( 0.000000000000000000, 0.000000000000000000, 1.000000000000000000 ) ) ;
#2556 = CARTESIAN_POINT ( 'NONE',  ( 20.99563651348813664, -9.290040531262853563, -77.50066261921593025 ) ) ;
#2558 = CARTESIAN_POINT ( 'NONE',  ( 53.46882080935260007, 17.64232885596709721, -26.54419876889340202 ) ) ;
#2557 = CARTESIAN_POINT ( 'NONE',  ( 61.75019796695539753, 13.88381105532070059, -28.15000000000000213 ) ) ;
#2559 = CARTESIAN_POINT ( 'NONE',  ( 21.87115360135859987, -19.71825049090939785, -70.65040049691899071 ) ) ;
#2560 = AXIS2_PLACEMENT_3D ( 'NONE', #21515, #41440, #41189 ) ;
#2561 = CARTESIAN_POINT ( 'NONE',  ( 19.21265657477752598, -49.46974233527256359, -34.79644660940672907 ) ) ;
#2562 = CARTESIAN_POINT ( 'NONE',  ( 24.04493737600856207, -16.65173076576985878, -41.54933394159128568 ) ) ;
#2563 = CARTESIAN_POINT ( 'NONE',  ( 20.29254098389584726, -21.02756184446683463, -40.74443803683676890 ) ) ;
#2564 = B_SPLINE_SURFACE_WITH_KNOTS ( 'NONE', 3, 3, ( 
 ( #16198, #32154, #43470, #12531, #35337, #44235 ),
 ( #8337, #39792, #40052, #31902, #24547, #48429 ),
 ( #24292, #51338, #11771, #4401, #20370, #19612 ),
 ( #4142, #19865, #27976, #7577, #36358, #15436 ),
 ( #35856, #466, #31388, #27729, #43979, #47417 ),
 ( #11510, #27468, #39540, #3642, #15689, #31643 ),
 ( #8084, #47663, #51845, #47922, #32670, #4922 ),
 ( #13316, #13818, #17493, #25841, #37660, #20629 ),
 ( #9117, #21406, #45277, #37155, #37408, #17746 ),
 ( #29532, #45536, #20893, #24813, #9387, #29021 ) ),
 .UNSPECIFIED., .F., .F., .F.,
 ( 4, 2, 2, 2, 4 ),
 ( 4, 1, 1, 4 ),
 ( -0.2468266944438050059, -0.2159733576383290055, -0.1666080187495679876, -0.08762347652754901017, 1.941358000000000020E-15 ),
 ( 0.000000000000000000, 0.3333333333333329818, 0.6666666666666670737, 1.000000000000000000 ),
 .UNSPECIFIED. ) ;
#2565 = VERTEX_POINT ( 'NONE', #35828 ) ;
#2566 = CARTESIAN_POINT ( 'NONE',  ( 18.44107633810049762, 5.527441888613518373, -34.79644660940672907 ) ) ;
#2567 = ORIENTED_EDGE ( 'NONE', *, *, #6462, .T. ) ;
#2568 = EDGE_LOOP ( 'NONE', ( #17814, #45757, #35941, #44641, #4819 ) ) ;
#2569 = CARTESIAN_POINT ( 'NONE',  ( 11.98449920101150035, -64.78734946337890221, -16.08642242878890016 ) ) ;
#2570 = CARTESIAN_POINT ( 'NONE',  ( 19.60730040409203667, -8.442301474033923725, -39.15105660710381130 ) ) ;
#2571 = CARTESIAN_POINT ( 'NONE',  ( 12.72599916435775214, -21.52913051451223225, -55.11948793158605753 ) ) ;
#2572 = CARTESIAN_POINT ( 'NONE',  ( 9.886195853582540494, -64.20534592295300058, -46.62515117760860051 ) ) ;
#2573 = ORIENTED_EDGE ( 'NONE', *, *, #14370, .F. ) ;
#2574 = ORIENTED_EDGE ( 'NONE', *, *, #40111, .F. ) ;
#2575 = CARTESIAN_POINT ( 'NONE',  ( 50.12648257197400170, 22.24397334070430077, -55.01261709213260076 ) ) ;
#2576 = CARTESIAN_POINT ( 'NONE',  ( 57.50723795381379944, -45.11618894467940066, -25.33268388717609909 ) ) ;
#2577 = CARTESIAN_POINT ( 'NONE',  ( 50.12452099567399699, 21.34276116794150369, -52.77544220100040206 ) ) ;
#2578 = CARTESIAN_POINT ( 'NONE',  ( 63.13518000424760146, -1.636848992617379928, -16.22147126600509637 ) ) ;
#2579 = CARTESIAN_POINT ( 'NONE',  ( 50.97631566918259693, -50.00474991773980094, -76.22722522842570925 ) ) ;
#2580 = CARTESIAN_POINT ( 'NONE',  ( 56.64011576333900422, -50.33902915376989995, -52.69731447354050147 ) ) ;
#2581 = ORIENTED_EDGE ( 'NONE', *, *, #30396, .F. ) ;
#2582 = CARTESIAN_POINT ( 'NONE',  ( 16.13393739769620083, -15.61618894467929941, -28.45282021618999835 ) ) ;
#2583 = CARTESIAN_POINT ( 'NONE',  ( 68.13393739769814772, 19.38381105532029736, -71.50000000000200373 ) ) ;
#2584 = EDGE_LOOP ( 'NONE', ( #41859, #16154, #11938, #44412, #38669 ) ) ;
#2585 = CARTESIAN_POINT ( 'NONE',  ( 17.01980719008272658, -8.849199162639587612, -51.99448548333836584 ) ) ;
#2586 = CARTESIAN_POINT ( 'NONE',  ( 47.18077425662879421, -45.11618894467940066, -8.347046103084750257 ) ) ;
#2587 = CARTESIAN_POINT ( 'NONE',  ( 12.83474630336350053, -8.495649237981627522, -41.37438378445959586 ) ) ;
#2588 = EDGE_CURVE ( 'NONE', #12971, #36729, #32664, .T. ) ;
#2589 = CARTESIAN_POINT ( 'NONE',  ( 13.56095021366290077, -51.24259045802140378, -22.27874983821260102 ) ) ;
#2590 = CARTESIAN_POINT ( 'NONE',  ( 56.10489411446869212, 19.52080739473450066, -75.03274246618039456 ) ) ;
#2591 = CARTESIAN_POINT ( 'NONE',  ( 46.81978912889830013, -53.49478526707780190, -76.01748491306379663 ) ) ;
#2592 = EDGE_CURVE ( 'NONE', #37038, #10379, #2670, .T. ) ;
#2593 = CARTESIAN_POINT ( 'NONE',  ( 57.24436304061489977, 13.89534489433389908, -17.93020804353299980 ) ) ;
#2594 = LINE ( 'NONE', #26415, #14815 ) ;
#2595 = CARTESIAN_POINT ( 'NONE',  ( 13.63393739769619906, -45.61618894467940066, -35.14999999999999858 ) ) ;
#2596 = CIRCLE ( 'NONE', #45274, 2.999999999999999112 ) ;
#2597 = CARTESIAN_POINT ( 'NONE',  ( 9.202753043728490567, -16.92050586389959932, -41.78797233031760072 ) ) ;
#2598 = CYLINDRICAL_SURFACE ( 'NONE', #20103, 1.999999999999996225 ) ;
#2599 = AXIS2_PLACEMENT_3D ( 'NONE', #19074, #18560, #30600 ) ;
#2600 = ORIENTED_EDGE ( 'NONE', *, *, #46888, .F. ) ;
#2601 = CARTESIAN_POINT ( 'NONE',  ( 47.63737930067980386, 23.29734254719310016, -74.36261479959799203 ) ) ;
#2602 = CARTESIAN_POINT ( 'NONE',  ( 65.05077035654539941, 1.384378348444520013, -60.98758765055369935 ) ) ;
#2603 = PLANE ( 'NONE',  #15551 ) ;
#2604 = CARTESIAN_POINT ( 'NONE',  ( 30.68460988201149675, -15.41618894468000356, -65.65000000000004832 ) ) ;
#2605 = CARTESIAN_POINT ( 'NONE',  ( 45.82851118213719843, -45.11588810659969795, -7.494127385217890236 ) ) ;
#2606 = CARTESIAN_POINT ( 'NONE',  ( 63.43393739769620510, 1.383811055320669947, -62.79342862858290886 ) ) ;
#2607 = DIRECTION ( 'NONE',  ( 1.000000000000000000, -1.080128361472376380E-29, -1.260570937617230037E-11 ) ) ;
#2608 = EDGE_CURVE ( 'NONE', #50703, #22911, #42457, .T. ) ;
#2609 = CARTESIAN_POINT ( 'NONE',  ( 82.53030587998239298, 14.28927347135980064, -47.58595373936260842 ) ) ;
#2610 = CARTESIAN_POINT ( 'NONE',  ( -0.2420090942845939952, 19.37547203512649929, -34.97694517729849650 ) ) ;
#2612 = CARTESIAN_POINT ( 'NONE',  ( 45.89884848434977016, -40.22868796843931705, -56.88510789556015368 ) ) ;
#2611 = DIRECTION ( 'NONE',  ( 4.718060457820110146E-11, -8.281540456132319756E-12, 1.000000000000000000 ) ) ;
#2613 = EDGE_CURVE ( 'NONE', #6636, #14944, #35275, .T. ) ;
#2614 = CARTESIAN_POINT ( 'NONE',  ( 56.61928439928507828, -45.32411236664518839, -17.93019253464870033 ) ) ;
#2615 = CARTESIAN_POINT ( 'NONE',  ( 24.04493739244504624, -14.58064021191867887, -69.46600480801545530 ) ) ;
#2616 = CARTESIAN_POINT ( 'NONE',  ( -29.55684472351650172, 4.629324287396400450, -55.62305524083090091 ) ) ;
#2617 = ORIENTED_EDGE ( 'NONE', *, *, #37878, .F. ) ;
#2618 = CARTESIAN_POINT ( 'NONE',  ( 52.69140955423309691, -49.74818585651569691, -48.48983962412659565 ) ) ;
#2619 = ORIENTED_EDGE ( 'NONE', *, *, #42232, .F. ) ;
#2620 = CARTESIAN_POINT ( 'NONE',  ( 45.69008980065965631, 8.960831227535303256, -57.99265491320560528 ) ) ;
#2621 = LINE ( 'NONE', #42719, #20185 ) ;
#2622 = CARTESIAN_POINT ( 'NONE',  ( 13.65323342448890109, 20.15922856535879859, -23.15000001653130113 ) ) ;
#2623 = CARTESIAN_POINT ( 'NONE',  ( 83.84453551654050329, 13.09585956956080111, -46.66649649553750123 ) ) ;
#2624 = CARTESIAN_POINT ( 'NONE',  ( 16.77661224428939590, -22.63968719969309973, -42.92377462465219651 ) ) ;
#2625 = CARTESIAN_POINT ( 'NONE',  ( 28.63499203762230394, -26.55409882356909890, -34.64999999999999858 ) ) ;
#2626 = CARTESIAN_POINT ( 'NONE',  ( 52.83551389523529451, 18.45330133924599991, -48.92570522021940604 ) ) ;
#2627 = CARTESIAN_POINT ( 'NONE',  ( 55.95161226490260020, -45.83867278594010486, -17.62594177103509807 ) ) ;
#2628 = CARTESIAN_POINT ( 'NONE',  ( 13.20770907579910158, -46.26637462015160196, -23.15000000000000213 ) ) ;
#2629 = ORIENTED_EDGE ( 'NONE', *, *, #51660, .T. ) ;
#2630 = CARTESIAN_POINT ( 'NONE',  ( 18.51684932252259941, -22.35565481394259990, -81.45916290265100201 ) ) ;
#2631 = CARTESIAN_POINT ( 'NONE',  ( 10.89208540626859900, -65.00086834622119625, -17.57297890437749999 ) ) ;
#2632 = CARTESIAN_POINT ( 'NONE',  ( 9.618181907774909334, 33.17626444807680031, -46.87734673202830038 ) ) ;
#2633 = CARTESIAN_POINT ( 'NONE',  ( 73.08075677931830683, 1.188042061556800144, -62.42534911081870064 ) ) ;
#2634 = CIRCLE ( 'NONE', #10144, 2.000000000000001776 ) ;
#2635 = CARTESIAN_POINT ( 'NONE',  ( 10.98984918190470061, -65.15326276073609790, -18.13296861429880380 ) ) ;
#2636 = DIRECTION ( 'NONE',  ( 0.000000000000000000, 0.000000000000000000, 1.000000000000000000 ) ) ;
#2637 = CARTESIAN_POINT ( 'NONE',  ( 23.79010008140480892, -17.67459298788599398, -75.87594074650500886 ) ) ;
#2638 = CARTESIAN_POINT ( 'NONE',  ( 24.04493738655059687, -14.58064352360674043, -45.75066538883495326 ) ) ;
#2639 = VECTOR ( 'NONE', #19715, 1000.000000000000000 ) ;
#2640 = CIRCLE ( 'NONE', #5149, 6.000000000000005329 ) ;
#2641 = CARTESIAN_POINT ( 'NONE',  ( 9.653816277033588023, -20.24304174429426340, -46.31047858425840502 ) ) ;
#2642 = ORIENTED_EDGE ( 'NONE', *, *, #20677, .F. ) ;
#2643 = CARTESIAN_POINT ( 'NONE',  ( 64.73967613295090473, 1.000225705806889964, -70.58924174254049433 ) ) ;
#2644 = ORIENTED_EDGE ( 'NONE', *, *, #14707, .F. ) ;
#2645 = CARTESIAN_POINT ( 'NONE',  ( 10.97982788474749860, -63.40303658660428709, -44.74674020368789940 ) ) ;
#2646 = CARTESIAN_POINT ( 'NONE',  ( 21.28881342178227243, -11.15893607458650294, -32.22570542542457162 ) ) ;
#2647 = VERTEX_POINT ( 'NONE', #48142 ) ;
#2648 = CARTESIAN_POINT ( 'NONE',  ( 3.987490788289478783, -8.603434725040944642, -34.79644660940672907 ) ) ;
#2649 = CARTESIAN_POINT ( 'NONE',  ( 57.07954899399199888, 19.06789840296940142, -52.78599243482480574 ) ) ;
#2650 = CARTESIAN_POINT ( 'NONE',  ( 52.47683853037149504, 18.72915222723299777, -77.24560337738110150 ) ) ;
#2651 = VERTEX_POINT ( 'NONE', #16166 ) ;
#2652 = CARTESIAN_POINT ( 'NONE',  ( 9.127478424014915603, -63.94375969568785933, -46.75102854448083889 ) ) ;
#2653 = LINE ( 'NONE', #41698, #21680 ) ;
#2654 = CARTESIAN_POINT ( 'NONE',  ( 16.13393739769620083, -15.61618894467929941, -41.53556505950739819 ) ) ;
#2655 = LINE ( 'NONE', #14440, #44553 ) ;
#2656 = CARTESIAN_POINT ( 'NONE',  ( 8.562943635882170668, -18.88157919922900163, -66.66271668429418185 ) ) ;
#2657 = EDGE_CURVE ( 'NONE', #18765, #29187, #24260, .T. ) ;
#2658 = CARTESIAN_POINT ( 'NONE',  ( 22.90068744318051586, -15.61618870719606278, -70.84718393407784731 ) ) ;
#2659 = CARTESIAN_POINT ( 'NONE',  ( 45.04398199156845095, -38.04764848494028229, -65.09977662695574452 ) ) ;
#2660 = ORIENTED_EDGE ( 'NONE', *, *, #42944, .F. ) ;
#2661 = CARTESIAN_POINT ( 'NONE',  ( 61.55415490858686667, -1.843864237299252862, -15.99574535869863823 ) ) ;
#2662 = CARTESIAN_POINT ( 'NONE',  ( 8.689358087320488977, -15.90762109230819910, -55.22020283005320351 ) ) ;
#2663 = CARTESIAN_POINT ( 'NONE',  ( 9.375062053639432236, -18.97670595503450031, -32.14999999999999858 ) ) ;
#2664 = CARTESIAN_POINT ( 'NONE',  ( 10.13166960481762757, -12.43500837955161309, -61.60803830279134274 ) ) ;
#2665 = DIRECTION ( 'NONE',  ( 1.224647809895004774E-16, 1.000000000000000000, -3.858400438143726299E-12 ) ) ;
#2666 = CARTESIAN_POINT ( 'NONE',  ( 68.13393739769745139, -49.21324915460109395, -75.95351669811962836 ) ) ;
#2667 = CARTESIAN_POINT ( 'NONE',  ( 41.37000474207589917, -45.26882832540889723, -6.004987957165030643 ) ) ;
#2668 = CIRCLE ( 'NONE', #5183, 4.649999999999999467 ) ;
#2669 = CARTESIAN_POINT ( 'NONE',  ( 8.974883818595877472, -12.14812015699499526, -60.65116565854415143 ) ) ;
#2670 = CIRCLE ( 'NONE', #39480, 2.000000000000000000 ) ;
#2671 = CARTESIAN_POINT ( 'NONE',  ( 24.35155753959719860, -14.94280947335750120, -67.48164325437410582 ) ) ;
#2672 = ORIENTED_EDGE ( 'NONE', *, *, #13327, .F. ) ;
#2673 = CARTESIAN_POINT ( 'NONE',  ( 20.61518557697189991, -22.02660557262029783, -32.14999999999999858 ) ) ;
#2674 = CARTESIAN_POINT ( 'NONE',  ( 56.18572637789630164, -50.74534604707739760, -74.96558747352590046 ) ) ;
#2676 = CARTESIAN_POINT ( 'NONE',  ( 40.99639966443897521, -39.64985368671198529, -81.17215446963993486 ) ) ;
#2675 = CARTESIAN_POINT ( 'NONE',  ( -2.285077198058380166, 18.61977639420179642, -5.969580375927669991 ) ) ;
#2678 = EDGE_CURVE ( 'NONE', #19040, #5062, #8304, .T. ) ;
#2677 = CARTESIAN_POINT ( 'NONE',  ( 20.39068152308554716, 10.74943050428834823, -34.64999999999999858 ) ) ;
#2679 = CARTESIAN_POINT ( 'NONE',  ( 87.61621807841599718, -15.61618894467929941, -61.12885639714370001 ) ) ;
#2680 = ORIENTED_EDGE ( 'NONE', *, *, #33098, .F. ) ;
#2681 = CARTESIAN_POINT ( 'NONE',  ( 15.05440318628110141, 21.88381105532300097, -76.14999999999999147 ) ) ;
#2682 = CARTESIAN_POINT ( 'NONE',  ( 47.41723297365239631, 23.41216560487029952, -54.77931948513369775 ) ) ;
#2683 = CARTESIAN_POINT ( 'NONE',  ( 68.13393739769618662, -29.16618894467940137, -65.65000000000000568 ) ) ;
#2684 = DIRECTION ( 'NONE',  ( -0.8660254037844381525, 0.5000000000000007772, 0.000000000000000000 ) ) ;
#2685 = CARTESIAN_POINT ( 'NONE',  ( -23.72016456855330091, -54.14290045843440424, 17.35000000000000142 ) ) ;
#2686 = CARTESIAN_POINT ( 'NONE',  ( 11.99376942192360040, 34.12659637466200024, -17.21195695013489768 ) ) ;
#2687 = CARTESIAN_POINT ( 'NONE',  ( 13.41159479355771467, -22.12244823249002224, -57.47332068091731827 ) ) ;
#2688 = CARTESIAN_POINT ( 'NONE',  ( 53.13650386459389807, 18.26782892954070192, -48.81774254411430292 ) ) ;
#2689 = FACE_OUTER_BOUND ( 'NONE', #26055, .T. ) ;
#2690 = CARTESIAN_POINT ( 'NONE',  ( 60.34488827473360573, -45.86932735725469712, -47.73027270518679899 ) ) ;
#2691 = CARTESIAN_POINT ( 'NONE',  ( 52.82924303383909859, 18.40678474754740179, -27.83106633233370175 ) ) ;
#2692 = CARTESIAN_POINT ( 'NONE',  ( 20.13393739496619972, 24.18330852864180258, -20.65000000000000213 ) ) ;
#2693 = CARTESIAN_POINT ( 'NONE',  ( 52.85423108789519375, -49.63991540118476564, -27.95802159601835157 ) ) ;
#2694 = PLANE ( 'NONE',  #47024 ) ;
#2695 = CARTESIAN_POINT ( 'NONE',  ( 11.27223392903683497, -21.94233489862524067, -76.21602140441011386 ) ) ;
#2696 = CARTESIAN_POINT ( 'NONE',  ( 71.33582579397329937, 0.9940695285616559795, -60.58508503553749591 ) ) ;
#2697 = CARTESIAN_POINT ( 'NONE',  ( 10.77261237629559965, 32.06410662680400492, -45.20506416186449883 ) ) ;
#2698 = CARTESIAN_POINT ( 'NONE',  ( 72.81668245960399588, 1.239065815390979930, -62.04599498926259571 ) ) ;
#2699 = CARTESIAN_POINT ( 'NONE',  ( 68.13393739769618662, -1.666188944679350081, -65.65000000000000568 ) ) ;
#2700 = CARTESIAN_POINT ( 'NONE',  ( 12.73007005307443329, 24.23871925420958462, -75.55954122747003510 ) ) ;
#2701 = EDGE_LOOP ( 'NONE', ( #4927, #24902, #44543, #10126 ) ) ;
#2702 = VERTEX_POINT ( 'NONE', #5168 ) ;
#2703 = LINE ( 'NONE', #11345, #48828 ) ;
#2704 = CARTESIAN_POINT ( 'NONE',  ( 48.82567944589380460, -3.116188925162400203, -15.64999999106299988 ) ) ;
#2705 = EDGE_LOOP ( 'NONE', ( #35832, #27499, #29235, #30784, #22657, #33958 ) ) ;
#2706 = CARTESIAN_POINT ( 'NONE',  ( 11.66108919451019865, -64.87818593170879922, -45.24345066936370330 ) ) ;
#2707 = CARTESIAN_POINT ( 'NONE',  ( 55.89127853695700310, -45.96104820497279775, -25.54022091618979928 ) ) ;
#2708 = CARTESIAN_POINT ( 'NONE',  ( 11.19961949155312908, -65.24734059375452944, -18.17421237899869979 ) ) ;
#2709 = CARTESIAN_POINT ( 'NONE',  ( 64.93393739769619799, 10.88381105532070059, -69.84999999999999432 ) ) ;
#2710 =( BOUNDED_CURVE ( )  B_SPLINE_CURVE ( 3, ( #40308, #40054, #12274, #8338 ),
 .UNSPECIFIED., .F., .T. ) 
 B_SPLINE_CURVE_WITH_KNOTS ( ( 4, 4 ),
 ( 5.578367201137250042, 5.769749740152300355 ),
 .UNSPECIFIED. ) 
 CURVE ( )  GEOMETRIC_REPRESENTATION_ITEM ( )  RATIONAL_B_SPLINE_CURVE ( ( 1.000000000000000000, 0.9969500553618734218, 0.9969500553618734218, 1.000000000000000000 ) ) 
 REPRESENTATION_ITEM ( '' )  );
#2711 = DIRECTION ( 'NONE',  ( 0.000000000000000000, 0.000000000000000000, -1.000000000000000000 ) ) ;
#2712 = ORIENTED_EDGE ( 'NONE', *, *, #10147, .F. ) ;
#2713 = CARTESIAN_POINT ( 'NONE',  ( 11.63574103177584185, 34.14703465354016032, -22.51277960591899685 ) ) ;
#2714 = CARTESIAN_POINT ( 'NONE',  ( 43.08803616482992993, 6.558594096496958237, -74.87949594534148900 ) ) ;
#2715 = CARTESIAN_POINT ( 'NONE',  ( 12.16706694049450022, 34.22772821235970042, -22.71320579729880151 ) ) ;
#2716 = ORIENTED_EDGE ( 'NONE', *, *, #46821, .T. ) ;
#2717 = CARTESIAN_POINT ( 'NONE',  ( 51.23833940013359722, -45.11618894467940066, -11.16259862780779955 ) ) ;
#2718 = EDGE_CURVE ( 'NONE', #33931, #51003, #24364, .T. ) ;
#2719 = LINE ( 'NONE', #39394, #13757 ) ;
#2720 = CYLINDRICAL_SURFACE ( 'NONE', #29707, 0.4999999999999994449 ) ;
#2721 = CARTESIAN_POINT ( 'NONE',  ( 12.23243695589036761, -21.17135045914907820, -51.14773272228742940 ) ) ;
#2722 = EDGE_CURVE ( 'NONE', #1545, #28603, #44726, .T. ) ;
#2723 = DIRECTION ( 'NONE',  ( 0.000000000000000000, -1.000000000000000000, 0.000000000000000000 ) ) ;
#2724 = EDGE_CURVE ( 'NONE', #13650, #27748, #30261, .T. ) ;
#2725 = CARTESIAN_POINT ( 'NONE',  ( 10.22105554918047865, -12.20814692505701160, -63.61948725257905579 ) ) ;
#2726 = CARTESIAN_POINT ( 'NONE',  ( 47.30318258422299493, -54.71095611916120305, -74.36173831268348522 ) ) ;
#2727 = CARTESIAN_POINT ( 'NONE',  ( 66.82519403554060489, 13.09192299164059925, -11.25137922129169965 ) ) ;
#2728 = EDGE_CURVE ( 'NONE', #6692, #43986, #46190, .T. ) ;
#2729 = DIRECTION ( 'NONE',  ( -0.6918010270571961495, 0.3994115091971370823, -0.6015661104845201335 ) ) ;
#2730 = CARTESIAN_POINT ( 'NONE',  ( 52.75030376661270282, 20.12775360152859960, -75.83477265320939864 ) ) ;
#2731 = LINE ( 'NONE', #38642, #41516 ) ;
#2732 = CARTESIAN_POINT ( 'NONE',  ( 9.135602731787439978, -11.25659805155929938, -34.68500579403580275 ) ) ;
#2733 = EDGE_LOOP ( 'NONE', ( #29216, #33986, #12183, #24840, #4810 ) ) ;
#2734 = CARTESIAN_POINT ( 'NONE',  ( 53.91527575946920336, -48.70888914390349811, -27.03219125244680043 ) ) ;
#2735 = CARTESIAN_POINT ( 'NONE',  ( 10.35404411787279955, -63.79155264719249629, -15.51648447543499998 ) ) ;
#2736 = CARTESIAN_POINT ( 'NONE',  ( 76.39184943767510561, -18.71884955068060208, -12.76139016365400103 ) ) ;
#2738 = EDGE_CURVE ( 'NONE', #26146, #23479, #4370, .T. ) ;
#2737 = CARTESIAN_POINT ( 'NONE',  ( 75.29474438729376118, 13.39011681956304045, -14.04674746638269767 ) ) ;
#2739 = CARTESIAN_POINT ( 'NONE',  ( 61.10787018228941037, -45.48724546724425721, -47.48172069074966828 ) ) ;
#2740 = CARTESIAN_POINT ( 'NONE',  ( 14.17038268164670001, 1.343694785579800044, -34.95504743437649608 ) ) ;
#2741 = AXIS2_PLACEMENT_3D ( 'NONE', #9925, #33245, #25887 ) ;
#2742 = DIRECTION ( 'NONE',  ( -0.06672502100504953959, -0.04847856544221940817, 0.9965929962951476373 ) ) ;
#2743 = CARTESIAN_POINT ( 'NONE',  ( 82.43660516933499594, -45.21753288021749739, -47.02797074234310060 ) ) ;
#2744 = LINE ( 'NONE', #42582, #14789 ) ;
#2745 = CARTESIAN_POINT ( 'NONE',  ( 41.54582584773770293, 12.73228223202879938, -4.072799719962560516 ) ) ;
#2746 = CARTESIAN_POINT ( 'NONE',  ( 61.43325308111587901, -45.44830257304832344, -47.47808681911117645 ) ) ;
#2747 = CARTESIAN_POINT ( 'NONE',  ( 19.62692545003119449, 24.23099720707456584, -75.46694760810223102 ) ) ;
#2748 = CARTESIAN_POINT ( 'NONE',  ( 65.43042069957888884, -49.21324915460513694, -73.25000000000119371 ) ) ;
#2749 = CARTESIAN_POINT ( 'NONE',  ( 20.29256185465771267, -21.02754514162187860, -62.74448681189702626 ) ) ;
#2750 = CARTESIAN_POINT ( 'NONE',  ( 18.05183576353649855, -51.93578155835659516, -75.67800190747080080 ) ) ;
#2751 = CARTESIAN_POINT ( 'NONE',  ( 41.51083608087070331, -44.40732572871969808, -4.911476834593860197 ) ) ;
#2752 = ORIENTED_EDGE ( 'NONE', *, *, #32037, .F. ) ;
#2753 = CARTESIAN_POINT ( 'NONE',  ( 17.36723456227180051, -22.96368324152579987, -51.51440696060289781 ) ) ;
#2754 = CARTESIAN_POINT ( 'NONE',  ( 63.63571284094848579, 1.261444690199680085, -61.78778606023939091 ) ) ;
#2755 = EDGE_LOOP ( 'NONE', ( #50519, #36386, #18610, #21044 ) ) ;
#2756 = CARTESIAN_POINT ( 'NONE',  ( 2.633937397696199945, -15.61618894467930119, 17.35000000000000142 ) ) ;
#2757 = CARTESIAN_POINT ( 'NONE',  ( 61.09252571675989429, -45.64957244923589741, -47.71760867771700276 ) ) ;
#2758 = CARTESIAN_POINT ( 'NONE',  ( 73.18782247527531126, 0.8859637708054489691, -68.88406027352149863 ) ) ;
#2759 = CARTESIAN_POINT ( 'NONE',  ( 45.71596276813887272, 8.844597340974925004, -58.33858004979597922 ) ) ;
#2760 = ADVANCED_FACE ( 'NONE', ( #37126 ), #36964, .F. ) ;
#2761 = CARTESIAN_POINT ( 'NONE',  ( 9.042768892828480176, -16.06693453323889997, -81.23899999999999011 ) ) ;
#2762 = CARTESIAN_POINT ( 'NONE',  ( 40.79813849721050190, -45.21264691650740275, -5.648537283802860465 ) ) ;
#2763 = ORIENTED_EDGE ( 'NONE', *, *, #5622, .F. ) ;
#2764 = VERTEX_POINT ( 'NONE', #16958 ) ;
#2765 = VECTOR ( 'NONE', #44428, 1000.000000000000000 ) ;
#2766 = ORIENTED_EDGE ( 'NONE', *, *, #812, .F. ) ;
#2767 = FACE_OUTER_BOUND ( 'NONE', #41206, .T. ) ;
#2768 = CARTESIAN_POINT ( 'NONE',  ( 61.13177402460449628, -45.31381189176509849, -46.88387570683920558 ) ) ;
#2769 = DIRECTION ( 'NONE',  ( 0.000000000000000000, 1.000000000000000000, 0.000000000000000000 ) ) ;
#2770 = ORIENTED_EDGE ( 'NONE', *, *, #28864, .T. ) ;
#2771 = CARTESIAN_POINT ( 'NONE',  ( 16.13393739769620083, -51.11618894467930119, -15.65000000000000036 ) ) ;
#2772 = ORIENTED_EDGE ( 'NONE', *, *, #6864, .T. ) ;
#2773 = CARTESIAN_POINT ( 'NONE',  ( 14.06329792164433101, -7.911078663674788736, -63.20899909920748883 ) ) ;
#2774 = B_SPLINE_CURVE_WITH_KNOTS ( 'NONE', 3,
 ( #43181, #7274, #26647, #20331, #20849, #15908, #25028, #43944, #32372 ),
 .UNSPECIFIED., .F., .F.,
 ( 4, 1, 1, 1, 1, 1, 4 ),
 ( 0.000000000000000000, 0.1666583021584449043, 0.3333266417267553017, 0.4999949812950666983, 0.6666633208633782059, 0.8333316604316886034, 1.000000000000000000 ),
 .UNSPECIFIED. ) ;
#2775 = CARTESIAN_POINT ( 'NONE',  ( 45.16555009513719199, -33.34057249083589625, -34.94897920698430482 ) ) ;
#2776 = EDGE_CURVE ( 'NONE', #13640, #25200, #38652, .T. ) ;
#2777 = AXIS2_PLACEMENT_3D ( 'NONE', #23907, #15815, #31780 ) ;
#2778 = ORIENTED_EDGE ( 'NONE', *, *, #17160, .F. ) ;
#2779 = CARTESIAN_POINT ( 'NONE',  ( 10.83684432477319959, -19.82762902495380075, -81.23899999999999011 ) ) ;
#2781 = CARTESIAN_POINT ( 'NONE',  ( 52.03834266725660740, -51.29072892105509851, -76.00976796454538942 ) ) ;
#2780 = CIRCLE ( 'NONE', #6974, 0.5000000000000004441 ) ;
#2782 = CARTESIAN_POINT ( 'NONE',  ( 60.86852778604830405, 14.26338112473730035, -47.33036891254590728 ) ) ;
#2783 = CIRCLE ( 'NONE', #36236, 2.000000000000002220 ) ;
#2784 = ADVANCED_FACE ( 'NONE', ( #48666 ), #28568, .T. ) ;
#2785 = DIRECTION ( 'NONE',  ( 0.7071067811865475727, 0.000000000000000000, -0.7071067811865475727 ) ) ;
#2786 = CARTESIAN_POINT ( 'NONE',  ( 40.74969953824990654, -44.70763297598060149, -4.809312831994500215 ) ) ;
#2787 = CARTESIAN_POINT ( 'NONE',  ( 5.133937397696200833, -15.61618894467929763, -20.58999999999999986 ) ) ;
#2788 = CARTESIAN_POINT ( 'NONE',  ( -7.615929272822939744, 14.09493422113850158, -5.327442894417729669 ) ) ;
#2789 = CARTESIAN_POINT ( 'NONE',  ( 1.058369240368409958, -22.58802147093010149, -34.64999999999999858 ) ) ;
#2790 = CARTESIAN_POINT ( 'NONE',  ( 72.38393739769620083, 4.883811055320659733, -61.44999999999999574 ) ) ;
#2791 = CARTESIAN_POINT ( 'NONE',  ( 87.61621807841599718, -48.61618894467930119, -61.12885639714370001 ) ) ;
#2792 = CARTESIAN_POINT ( 'NONE',  ( 23.66220021668120310, -17.83249377738399843, -55.37864069218029073 ) ) ;
#2793 = ORIENTED_EDGE ( 'NONE', *, *, #38533, .T. ) ;
#2794 = CARTESIAN_POINT ( 'NONE',  ( 14.33739625361640080, -52.54005950962240235, -75.96018872839380265 ) ) ;
#2795 = CIRCLE ( 'NONE', #51356, 20.00000000000000000 ) ;
#2796 = CARTESIAN_POINT ( 'NONE',  ( 57.55751162087899786, 19.27819942682179999, -53.27961218320869818 ) ) ;
#2797 = UNCERTAINTY_MEASURE_WITH_UNIT (LENGTH_MEASURE( 1.000000000000000082E-05 ), #44346, 'distance_accuracy_value', 'NONE');
#2799 = EDGE_CURVE ( 'NONE', #7053, #39784, #13043, .T. ) ;
#2798 = CARTESIAN_POINT ( 'NONE',  ( 71.62484648860579739, 0.9098571636355720083, -70.52991329011129551 ) ) ;
#2800 = CARTESIAN_POINT ( 'NONE',  ( 45.34134074967911943, -40.05352858297872132, -60.15667676233234573 ) ) ;
#2801 = CARTESIAN_POINT ( 'NONE',  ( 15.80832228677579643, 19.69806892893299732, -20.21644471496479767 ) ) ;
#2802 = CARTESIAN_POINT ( 'NONE',  ( 18.86789271228509790, -51.78678246903520233, -74.14999999999999147 ) ) ;
#2803 = CARTESIAN_POINT ( 'NONE',  ( 8.222911085862994796, -16.64130829724042115, -40.46641358909141672 ) ) ;
#2804 = CARTESIAN_POINT ( 'NONE',  ( 63.47112272702528912, 1.372372808637209785, -68.90857576278490626 ) ) ;
#2805 = CARTESIAN_POINT ( 'NONE',  ( 47.87139909866390752, -54.42646853815559638, -55.03639171593840018 ) ) ;
#2806 = CARTESIAN_POINT ( 'NONE',  ( 6.293131413228051585, -65.09536678314599101, -49.18705164837409427 ) ) ;
#2807 = AXIS2_PLACEMENT_3D ( 'NONE', #1005, #37170, #45292 ) ;
#2808 = CARTESIAN_POINT ( 'NONE',  ( 20.49757756391890240, -10.07532225487519284, -36.55952288011872042 ) ) ;
#2809 = CARTESIAN_POINT ( 'NONE',  ( 22.46008945880927499, -20.47788497429293031, -46.00070147826757250 ) ) ;
#2810 = LINE ( 'NONE', #19037, #40669 ) ;
#2811 = VERTEX_POINT ( 'NONE', #41824 ) ;
#2812 = VECTOR ( 'NONE', #44702, 1000.000000000000000 ) ;
#2813 = CARTESIAN_POINT ( 'NONE',  ( 20.07088694243709881, -21.46793974735500043, -73.15866903151078304 ) ) ;
#2814 = TOROIDAL_SURFACE ( 'NONE', #6147, 16.60961179679779676, 0.5000000000000000000 ) ;
#2815 = VERTEX_POINT ( 'NONE', #2256 ) ;
#2816 = CARTESIAN_POINT ( 'NONE',  ( 71.44853510719140388, 1.186515949276290227, -70.54416184698391135 ) ) ;
#2817 = CARTESIAN_POINT ( 'NONE',  ( 60.72865454444709599, -45.52246636016900538, -47.10836437988919556 ) ) ;
#2818 = CARTESIAN_POINT ( 'NONE',  ( 82.57795157571968048, 13.96423584352574743, -47.00703096682629933 ) ) ;
#2819 = CARTESIAN_POINT ( 'NONE',  ( -0.007164427059776000244, -22.82436266295209748, -34.77269723891829756 ) ) ;
#2821 = CARTESIAN_POINT ( 'NONE',  ( 14.53139780415610005, 1.019008445896690151, -34.65800258959599489 ) ) ;
#2820 = CARTESIAN_POINT ( 'NONE',  ( 9.366881967297588929, -15.61636073738300112, -79.84717978380999170 ) ) ;
#2822 = EDGE_CURVE ( 'NONE', #14121, #19450, #21628, .T. ) ;
#2823 = LINE ( 'NONE', #42395, #32065 ) ;
#2824 = CARTESIAN_POINT ( 'NONE',  ( 20.99564842327679415, -21.94232784797836544, -41.79933425902736843 ) ) ;
#2825 = CARTESIAN_POINT ( 'NONE',  ( 10.72251060975740877, -19.77472240810697102, -41.24444634761481154 ) ) ;
#2826 = ORIENTED_EDGE ( 'NONE', *, *, #35749, .F. ) ;
#2827 = CARTESIAN_POINT ( 'NONE',  ( 16.13393739769620083, -15.61618894467929941, -22.14999999999999858 ) ) ;
#2828 = ADVANCED_FACE ( 'NONE', ( #9860 ), #10125, .T. ) ;
#2829 = ORIENTED_EDGE ( 'NONE', *, *, #51342, .T. ) ;
#2830 = ORIENTED_EDGE ( 'NONE', *, *, #29719, .F. ) ;
#2831 = CARTESIAN_POINT ( 'NONE',  ( 12.23389792222440065, -64.89608577200989714, -16.17187715587200003 ) ) ;
#2832 = FACE_OUTER_BOUND ( 'NONE', #24242, .T. ) ;
#2833 = DIRECTION ( 'NONE',  ( 0.000000000000000000, 0.000000000000000000, -1.000000000000000000 ) ) ;
#2834 = CARTESIAN_POINT ( 'NONE',  ( 10.60384355420380054, -64.91168656924629943, -47.04674094553849528 ) ) ;
#2835 = ORIENTED_EDGE ( 'NONE', *, *, #25274, .F. ) ;
#2836 = ORIENTED_EDGE ( 'NONE', *, *, #26536, .T. ) ;
#2837 = CARTESIAN_POINT ( 'NONE',  ( 53.42290160909190178, 20.83982452118389972, -54.29362578891399949 ) ) ;
#2838 = CARTESIAN_POINT ( 'NONE',  ( -14.86606260230379917, -15.61618894467933139, -15.65000000000000036 ) ) ;
#2839 = VECTOR ( 'NONE', #44271, 1000.000000000000114 ) ;
#2840 = LINE ( 'NONE', #35575, #50338 ) ;
#2841 = CARTESIAN_POINT ( 'NONE',  ( 62.16233645777079886, -0.1749398299712949800, -16.60655181478709963 ) ) ;
#2842 = CARTESIAN_POINT ( 'NONE',  ( 51.62358001281820208, -48.61618677531440369, -76.93789421597479361 ) ) ;
#2843 = CARTESIAN_POINT ( 'NONE',  ( 57.17297709606850020, -50.49682799391059973, -53.01978805370689685 ) ) ;
#2844 = EDGE_CURVE ( 'NONE', #29283, #50827, #32741, .T. ) ;
#2845 = ORIENTED_EDGE ( 'NONE', *, *, #17164, .T. ) ;
#2846 = CARTESIAN_POINT ( 'NONE',  ( 23.80355599767301555, -13.57222019766435039, -33.70949676018119590 ) ) ;
#2847 = CARTESIAN_POINT ( 'NONE',  ( -31.36606260230380272, -63.11618894467929408, 17.35000000000000142 ) ) ;
#2848 = ORIENTED_EDGE ( 'NONE', *, *, #1192, .F. ) ;
#2849 = CARTESIAN_POINT ( 'NONE',  ( 35.13393739769620083, -15.61618894467929941, 8.349999999999999645 ) ) ;
#2850 = CARTESIAN_POINT ( 'NONE',  ( 24.04493740689873960, -16.65173053041055695, -53.54933808698535103 ) ) ;
#2851 = EDGE_CURVE ( 'NONE', #46028, #38446, #39740, .T. ) ;
#2852 = CARTESIAN_POINT ( 'NONE',  ( 11.56509562211340025, -9.235559475632230786, -39.31469157680550097 ) ) ;
#2853 = CARTESIAN_POINT ( 'NONE',  ( 14.24102869631719948, -51.10273149057969988, -22.22788221432130129 ) ) ;
#2854 = LINE ( 'NONE', #35588, #3344 ) ;
#2855 = CARTESIAN_POINT ( 'NONE',  ( 56.82341722989219335, 13.94957864525430047, -16.89538187380119894 ) ) ;
#2856 = CARTESIAN_POINT ( 'NONE',  ( 10.72262850419906677, -11.45750429148510996, -77.66115289588985604 ) ) ;
#2857 = CARTESIAN_POINT ( 'NONE',  ( 71.13601697155240799, 1.385888765344509999, -70.30422512560809878 ) ) ;
#2858 = CARTESIAN_POINT ( 'NONE',  ( 9.135435583350210109, -14.74238603266360137, -39.88671798479069963 ) ) ;
#2859 = CARTESIAN_POINT ( 'NONE',  ( 22.90075166721855737, -15.61618922411645727, -44.45281379938008115 ) ) ;
#2860 = EDGE_LOOP ( 'NONE', ( #12695, #28886, #13030, #638 ) ) ;
#2861 = CARTESIAN_POINT ( 'NONE',  ( 47.02416321684500389, 22.58718688193119917, -75.82399966601029462 ) ) ;
#2862 = CARTESIAN_POINT ( 'NONE',  ( 64.86108678489040358, 1.186856010528209993, -60.73114026433219692 ) ) ;
#2863 = CARTESIAN_POINT ( 'NONE',  ( 20.11811289261132885, -8.703692175439130096, -51.17433320692831700 ) ) ;
#2864 = CARTESIAN_POINT ( 'NONE',  ( 68.13393739823651174, -1.166188944679350081, -49.64999999999999858 ) ) ;
#2865 = CARTESIAN_POINT ( 'NONE',  ( 71.33393739769670105, 0.9098571636355720083, -70.12325384926869276 ) ) ;
#2866 = DIRECTION ( 'NONE',  ( 2.754761277895425776E-28, -6.290312716002009228E-11, -1.000000000000000000 ) ) ;
#2867 = CARTESIAN_POINT ( 'NONE',  ( 82.48420028019749850, 13.86594486706619911, -46.54735908456930815 ) ) ;
#2868 = CONICAL_SURFACE ( 'NONE', #5419, 44.00000000000000000, 0.8066715494215099813 ) ;
#2869 = CARTESIAN_POINT ( 'NONE',  ( -18.34876765167589951, 3.165124538224290074, -50.94389406753779781 ) ) ;
#2870 = B_SPLINE_CURVE_WITH_KNOTS ( 'NONE', 3,
 ( #39553, #11003, #15187, #31148, #47173, #39295, #35618, #26699 ),
 .UNSPECIFIED., .F., .F.,
 ( 4, 2, 2, 4 ),
 ( 0.08070042245370699641, 0.09929974077558219314, 0.1184089355330240068, 0.1205773112035685712 ),
 .UNSPECIFIED. ) ;
#2872 = CARTESIAN_POINT ( 'NONE',  ( 18.20469613467166425, -23.32126666006107030, -58.20899800978780547 ) ) ;
#2871 = CARTESIAN_POINT ( 'NONE',  ( 53.31390735437268802, 19.22904354471013733, -77.17777228777733001 ) ) ;
#2873 = CARTESIAN_POINT ( 'NONE',  ( 20.73040871625291715, -9.100038570834694696, -71.20348830954932851 ) ) ;
#2874 = CARTESIAN_POINT ( 'NONE',  ( -28.69324816627959862, 4.182983592527669714, -54.99967661823389875 ) ) ;
#2875 = VERTEX_POINT ( 'NONE', #29751 ) ;
#2876 = CARTESIAN_POINT ( 'NONE',  ( 52.65621920618569618, -49.77598664841080733, -48.47378032971909789 ) ) ;
#2877 = ORIENTED_EDGE ( 'NONE', *, *, #19055, .T. ) ;
#2878 = LINE ( 'NONE', #45872, #1950 ) ;
#2879 = CARTESIAN_POINT ( 'NONE',  ( 9.543105373624433341, -13.84479165416296809, -41.53615350155577346 ) ) ;
#2880 = CARTESIAN_POINT ( 'NONE',  ( 13.77909129202510030, 19.73319454833459830, -21.81863451142220001 ) ) ;
#2881 = DIRECTION ( 'NONE',  ( 0.7071067811865473507, 0.7071067811865476838, 0.000000000000000000 ) ) ;
#2882 = CARTESIAN_POINT ( 'NONE',  ( 20.74023174533219915, -20.95703261207519930, -46.72628331570599869 ) ) ;
#2883 = CARTESIAN_POINT ( 'NONE',  ( 52.77947503461199830, 18.47416142194530053, -48.82716066735080318 ) ) ;
#2884 = CARTESIAN_POINT ( 'NONE',  ( 54.50030068701860131, -46.15578316411880166, -15.72721191834270194 ) ) ;
#2885 = DIRECTION ( 'NONE',  ( -1.000000000000000000, 0.000000000000000000, 0.000000000000000000 ) ) ;
#2886 = ADVANCED_FACE ( 'NONE', ( #41310 ), #21058, .F. ) ;
#2887 = ORIENTED_EDGE ( 'NONE', *, *, #50559, .F. ) ;
#2888 = AXIS2_PLACEMENT_3D ( 'NONE', #14526, #2468, #39416 ) ;
#2889 = CARTESIAN_POINT ( 'NONE',  ( 9.244676780691371221, -12.77985576054640049, -80.19166000563309638 ) ) ;
#2890 = ORIENTED_EDGE ( 'NONE', *, *, #5718, .T. ) ;
#2891 = EDGE_CURVE ( 'NONE', #27600, #14302, #17390, .T. ) ;
#2892 = CARTESIAN_POINT ( 'NONE',  ( 73.02919596257699197, 0.9065823421260970072, -69.11945805671248877 ) ) ;
#2893 = CARTESIAN_POINT ( 'NONE',  ( 13.00893739769619906, 34.28605925116850273, -47.75434321273180416 ) ) ;
#2894 = CARTESIAN_POINT ( 'NONE',  ( 72.93398937763220147, 1.264121749638659864, -62.30317625966389983 ) ) ;
#2895 = CARTESIAN_POINT ( 'NONE',  ( 54.13393739769620083, -15.61618894467929941, 1.600000000000000089 ) ) ;
#2896 = CARTESIAN_POINT ( 'NONE',  ( 52.82359347161857954, -49.70062430464942338, -48.95125679539614083 ) ) ;
#2897 = CARTESIAN_POINT ( 'NONE',  ( 9.366937397696199596, -15.61618894467949836, -28.45282021618999835 ) ) ;
#2898 = CARTESIAN_POINT ( 'NONE',  ( 50.51702630346309775, -53.30999449162459314, -54.91376886094779763 ) ) ;
#2899 = ORIENTED_EDGE ( 'NONE', *, *, #23030, .F. ) ;
#2900 = CARTESIAN_POINT ( 'NONE',  ( 64.91485532786460055, 1.370853092582090094, -70.32939881202800336 ) ) ;
#2901 = ORIENTED_EDGE ( 'NONE', *, *, #359, .F. ) ;
#2902 = CARTESIAN_POINT ( 'NONE',  ( 10.14269678154489895, -63.23625467025420477, -45.99342279163030156 ) ) ;
#2903 = DIRECTION ( 'NONE',  ( -1.000000000000000000, 0.000000000000000000, 0.000000000000000000 ) ) ;
#2904 = ORIENTED_EDGE ( 'NONE', *, *, #44817, .T. ) ;
#2905 = DIRECTION ( 'NONE',  ( 0.000000000000000000, -1.000000000000000000, 0.000000000000000000 ) ) ;
#2906 = CARTESIAN_POINT ( 'NONE',  ( 53.07595676737840762, 19.15211386111450054, -77.13124878406790685 ) ) ;
#2907 = ORIENTED_EDGE ( 'NONE', *, *, #3499, .T. ) ;
#2908 = CARTESIAN_POINT ( 'NONE',  ( 12.13162407143141941, -65.41884435351431648, -47.52833372959231895 ) ) ;
#2909 = CARTESIAN_POINT ( 'NONE',  ( 16.13393739769620083, -15.61618894467929941, -28.45282021618999835 ) ) ;
#2910 = CARTESIAN_POINT ( 'NONE',  ( 21.80550130585419311, -19.38323868333978695, -32.63959037186587864 ) ) ;
#2911 = CARTESIAN_POINT ( 'NONE',  ( 23.13393739769620083, -28.89524513604070322, -84.65000000000000568 ) ) ;
#2912 = ADVANCED_FACE ( 'NONE', ( #28371 ), #50372, .T. ) ;
#2913 = CARTESIAN_POINT ( 'NONE',  ( 19.30279291186920076, -23.22809243764550047, -60.16676433707729643 ) ) ;
#2914 = AXIS2_PLACEMENT_3D ( 'NONE', #17919, #50155, #13743 ) ;
#2915 = CARTESIAN_POINT ( 'NONE',  ( 61.75019796695539753, -46.11618894467930119, -46.37203261889099792 ) ) ;
#2916 = FACE_OUTER_BOUND ( 'NONE', #48205, .T. ) ;
#2917 = ORIENTED_EDGE ( 'NONE', *, *, #16683, .T. ) ;
#2918 = ORIENTED_EDGE ( 'NONE', *, *, #47019, .F. ) ;
#2919 = CARTESIAN_POINT ( 'NONE',  ( 74.17629866868290378, 1.883811055320649963, -65.34607522167520699 ) ) ;
#2920 = CARTESIAN_POINT ( 'NONE',  ( 20.88369410565369932, -9.876284326973658878, -53.95269993303519840 ) ) ;
#2921 = CARTESIAN_POINT ( 'NONE',  ( 9.015406492218581036, -14.49019859173800029, -32.14999999999999858 ) ) ;
#2922 = LINE ( 'NONE', #30420, #45089 ) ;
#2923 = VECTOR ( 'NONE', #49668, 1000.000000000000000 ) ;
#2924 = CARTESIAN_POINT ( 'NONE',  ( 0.1457839871805957643, 14.73018012514992137, -34.68167748489143776 ) ) ;
#2925 = CARTESIAN_POINT ( 'NONE',  ( 16.13393739769620083, -15.61618894467929941, -46.39999999999999858 ) ) ;
#2926 = CARTESIAN_POINT ( 'NONE',  ( 11.74706319441980007, 33.70588526301440169, -16.38446683800539816 ) ) ;
#2927 = CARTESIAN_POINT ( 'NONE',  ( 8.304045112041299248, -13.03248859362910039, -58.60912297524879477 ) ) ;
#2928 = CARTESIAN_POINT ( 'NONE',  ( 52.87639532687919797, -49.52782412333860407, -27.19604750702729845 ) ) ;
#2929 = CARTESIAN_POINT ( 'NONE',  ( 55.50491188657730390, -50.93693546367299518, -75.08273106147520082 ) ) ;
#2931 = DIRECTION ( 'NONE',  ( 0.000000000000000000, 0.000000000000000000, -1.000000000000000000 ) ) ;
#2930 = CARTESIAN_POINT ( 'NONE',  ( -5.479087955498720852, 16.54576887086220083, -6.304622368372980290 ) ) ;
#2932 = ADVANCED_BREP_SHAPE_REPRESENTATION ( '', ( #10006, #20940 ), #854 ) ;
#2933 = CARTESIAN_POINT ( 'NONE',  ( 47.51629483024640166, -54.56948809585979632, -54.66793506916069845 ) ) ;
#2934 = DIRECTION ( 'NONE',  ( 0.000000000000000000, 0.000000000000000000, -1.000000000000000000 ) ) ;
#2935 = EDGE_LOOP ( 'NONE', ( #27341, #12969, #36013, #4740 ) ) ;
#2936 = CARTESIAN_POINT ( 'NONE',  ( -9.549430425165668979, -43.62870283194010312, -5.615282516777119426 ) ) ;
#2937 = CARTESIAN_POINT ( 'NONE',  ( 47.68653297382180511, 23.26174403522189849, -54.85872168688340622 ) ) ;
#2938 = CARTESIAN_POINT ( 'NONE',  ( 16.23169237103991236, -7.684835125088456564, -65.29632762180530392 ) ) ;
#2939 = CARTESIAN_POINT ( 'NONE',  ( 63.54731047306190561, 1.396834109478120034, -62.44999999999999574 ) ) ;
#2940 = CARTESIAN_POINT ( 'NONE',  ( 13.44563218319239972, 19.36637353181840027, -21.34300943931999939 ) ) ;
#2941 = CARTESIAN_POINT ( 'NONE',  ( 61.36953742131760237, 14.18133800638229935, -47.42052028026720478 ) ) ;
#2942 = CARTESIAN_POINT ( 'NONE',  ( 11.47551314107550091, 33.73997922480180023, -16.61573023121770021 ) ) ;
#2943 = CARTESIAN_POINT ( 'NONE',  ( 52.14531965947149672, 18.65759927364149817, -76.93285152251199577 ) ) ;
#2944 = CARTESIAN_POINT ( 'NONE',  ( 53.13654529785400626, 18.26855529545099799, -48.84750850883899886 ) ) ;
#2945 = DIRECTION ( 'NONE',  ( -0.000000000000000000, 1.000000000000000000, 0.000000000000000000 ) ) ;
#2946 = LINE ( 'NONE', #19695, #33441 ) ;
#2947 = CARTESIAN_POINT ( 'NONE',  ( 52.81005473481379653, 18.43886536192449910, -28.08974515321689935 ) ) ;
#2948 = ADVANCED_FACE ( 'NONE', ( #16860 ), #32808, .F. ) ;
#2949 = CYLINDRICAL_SURFACE ( 'NONE', #22126, 6.766999999999998572 ) ;
#2950 = CARTESIAN_POINT ( 'NONE',  ( 68.13393739769618662, -15.41618894467939782, -65.65000000000000568 ) ) ;
#2951 = CARTESIAN_POINT ( 'NONE',  ( 52.67198247596510186, 18.54881933231609992, -48.75776900890529930 ) ) ;
#2952 = CARTESIAN_POINT ( 'NONE',  ( 37.13393739769620083, -15.61618894467929941, -12.65000000000000036 ) ) ;
#2953 = CARTESIAN_POINT ( 'NONE',  ( 71.27262092911099955, 0.8838110553206759423, -60.53635606803790381 ) ) ;
#2954 = CARTESIAN_POINT ( 'NONE',  ( 11.13393739769619906, 32.04700499139590164, -43.91469645497959817 ) ) ;
#2955 = CARTESIAN_POINT ( 'NONE',  ( -21.36606260230379917, 21.88381105532059934, 16.35000000000000142 ) ) ;
#2956 = CARTESIAN_POINT ( 'NONE',  ( 66.85053874715731581, -33.11604528757069943, -20.46403489035089862 ) ) ;
#2957 = CARTESIAN_POINT ( 'NONE',  ( 11.13393739769619906, 32.24968758154479787, -24.15000000000000213 ) ) ;
#2958 = EDGE_LOOP ( 'NONE', ( #3950, #45172, #15913, #20138 ) ) ;
#2959 = ORIENTED_EDGE ( 'NONE', *, *, #31324, .F. ) ;
#2960 = CARTESIAN_POINT ( 'NONE',  ( 42.62644315548489971, 11.62703185229469938, -3.197525305353829950 ) ) ;
#2961 = CARTESIAN_POINT ( 'NONE',  ( 50.03950439116019311, -1.319789489291227857, -15.98383729154298116 ) ) ;
#2962 = ORIENTED_EDGE ( 'NONE', *, *, #35366, .T. ) ;
#2963 = CARTESIAN_POINT ( 'NONE',  ( 11.89007180640820138, -65.09421494503590111, -45.69968209956180516 ) ) ;
#2964 = CARTESIAN_POINT ( 'NONE',  ( 57.65063410596479798, -45.12128949765089914, -25.41617693766169950 ) ) ;
#2965 = CARTESIAN_POINT ( 'NONE',  ( 13.58486031666897098, -23.12313378403861819, -78.11181520993953598 ) ) ;
#2966 = EDGE_CURVE ( 'NONE', #9803, #51621, #5334, .T. ) ;
#2967 = DIRECTION ( 'NONE',  ( 0.000000000000000000, 0.000000000000000000, -1.000000000000000000 ) ) ;
#2968 = ORIENTED_EDGE ( 'NONE', *, *, #2608, .F. ) ;
#2969 = CARTESIAN_POINT ( 'NONE',  ( 11.71770650845053829, 34.17304478383466204, -22.42848135754658045 ) ) ;
#2970 = CARTESIAN_POINT ( 'NONE',  ( 43.37366955983795691, 6.599305106106574392, -73.45127533249436169 ) ) ;
#2971 = CARTESIAN_POINT ( 'NONE',  ( 11.79202840372359873, 34.19503632603060339, -22.35240682345929741 ) ) ;
#2972 = ORIENTED_EDGE ( 'NONE', *, *, #46173, .T. ) ;
#2973 = EDGE_CURVE ( 'NONE', #50743, #27433, #16057, .T. ) ;
#2974 = FACE_OUTER_BOUND ( 'NONE', #13672, .T. ) ;
#2975 = CARTESIAN_POINT ( 'NONE',  ( 51.86285139979289482, 1.501691761424130522, -18.73280815860681159 ) ) ;
#2976 = CARTESIAN_POINT ( 'NONE',  ( 15.92174032690060059, 19.82163670650420073, -20.83925419535739820 ) ) ;
#2977 = EDGE_CURVE ( 'NONE', #6854, #15707, #8480, .T. ) ;
#2978 = CARTESIAN_POINT ( 'NONE',  ( 22.88218496723100159, -16.13676012226024170, -50.47731942806621674 ) ) ;
#2979 = CARTESIAN_POINT ( 'NONE',  ( 59.22431851757179544, -28.11149781888600074, -15.66519468461460107 ) ) ;
#2980 = DIRECTION ( 'NONE',  ( 0.000000000000000000, 0.000000000000000000, 1.000000000000000000 ) ) ;
#2981 = CARTESIAN_POINT ( 'NONE',  ( 47.24086420343820691, -54.75472043013769508, -74.36236381585459299 ) ) ;
#2982 = CARTESIAN_POINT ( 'NONE',  ( 45.33440053090729549, 12.30260350233129962, -5.407269074095729877 ) ) ;
#2983 = VECTOR ( 'NONE', #44297, 1000.000000000000114 ) ;
#2984 = VECTOR ( 'NONE', #43778, 1000.000000000000000 ) ;
#2985 = DIRECTION ( 'NONE',  ( -0.5110015285683598973, 0.4887508954475665024, -0.7071067811865485719 ) ) ;
#2986 = CARTESIAN_POINT ( 'NONE',  ( 65.24498301373863285, -31.35931339248442029, -16.97693345051512637 ) ) ;
#2987 = CARTESIAN_POINT ( 'NONE',  ( 10.09313298742930165, -21.22790907185699893, -36.26938441530820256 ) ) ;
#2988 = B_SPLINE_SURFACE_WITH_KNOTS ( 'NONE', 3, 3, ( 
 ( #49772, #24856, #24591, #13359, #44539, #36660, #5496, #17787, #29317, #17287, #45324, #8640, #44802, #1550, #12843, #8905 ),
 ( #21451, #40863, #49008, #763, #16759, #33247, #1036, #37451, #49264, #25632, #21701, #45579, #4968, #32713, #37709, #48739 ),
 ( #20935, #17030, #32981, #41636, #9428, #17538, #9674, #5744, #2324, #42945, #38758, #46886, #18049, #26409, #30084, #2853 ),
 ( #6263, #30858, #42688, #2589, #10713, #51059, #22739, #14891, #34799, #50544, #6784, #42429, #42164, #50804, #22223, #14636 ),
 ( #41903, #9928, #30345, #10973, #18817, #29821, #26940, #7042, #39015, #22994, #37971, #18564, #50025, #35052, #46109, #26154 ),
 ( #34269, #38230, #34015, #3110, #19078, #45839, #25890, #6003, #21962, #50292, #30606, #2071, #14118, #10195, #18298, #38488 ),
 ( #14380, #46624, #46368, #10456, #6519, #22481, #34540, #26668, #27957, #12002, #31370, #47142, #16175, #8066, #23762, #35322 ),
 ( #8317, #43961, #24012, #32133, #20101, #27193, #36090, #43206, #198, #43707, #51573, #15672, #24270, #31626, #47902, #51320 ),
 ( #15417, #48152, #11494, #3881, #28215, #40291, #12256, #47645, #44216, #40033, #4382, #4126, #3624, #20350, #36336, #15156 ),
 ( #19339, #47399, #7810, #31117, #19595, #39776, #31883, #35586, #27450, #11231, #7295, #23246, #39264, #3365, #43453, #11751 ) ),
 .UNSPECIFIED., .F., .F., .F.,
 ( 4, 1, 1, 1, 1, 1, 1, 4 ),
 ( 4, 2, 2, 2, 2, 2, 2, 4 ),
 ( -5.223814999999999915E-09, 0.1428571428571430157, 0.2857142857142860315, 0.4285714285714289917, 0.5714285714285709528, 0.7142857142857139685, 0.8571428571428569843, 1.000000005223810051 ),
 ( -5.223816000000000234E-09, 0.4421363464883489858, 0.9474350281893190173, 1.263246704252430019, 1.421152542283979914, 1.673801883134460100, 2.076007908835539872, 2.526493408654630013 ),
 .UNSPECIFIED. ) ;
#2989 = ORIENTED_EDGE ( 'NONE', *, *, #47820, .F. ) ;
#2990 = AXIS2_PLACEMENT_3D ( 'NONE', #15099, #4070, #141 ) ;
#2991 = DIRECTION ( 'NONE',  ( -0.2260571801428161165, 0.000000000000000000, 0.9741140340359943917 ) ) ;
#2992 = PRESENTATION_LAYER_ASSIGNMENT (  '', '', ( #4659 ) ) ;
#2993 = CARTESIAN_POINT ( 'NONE',  ( 0.1207629063369290018, -53.60130123069310315, -8.684987670772850166 ) ) ;
#2994 = CARTESIAN_POINT ( 'NONE',  ( 76.41176102376428503, -21.82315656738479959, -12.84719217718200035 ) ) ;
#2995 = CARTESIAN_POINT ( 'NONE',  ( 75.40794329062271117, 12.89811451530892938, -13.65441625236441325 ) ) ;
#2996 = CARTESIAN_POINT ( 'NONE',  ( 20.08285034307092687, -55.42068993749968797, -74.66535148654590159 ) ) ;
#2997 = LINE ( 'NONE', #18967, #459 ) ;
#2998 = CARTESIAN_POINT ( 'NONE',  ( 47.18324198357279897, 23.57489020266570279, -54.61058319554400242 ) ) ;
#2999 = CARTESIAN_POINT ( 'NONE',  ( 82.13853704237929776, -45.35390657427750227, -47.32252334011910477 ) ) ;
#3000 = CARTESIAN_POINT ( 'NONE',  ( 57.35806099734729457, -50.23336412204299961, -52.73965739960290477 ) ) ;
#3001 = CARTESIAN_POINT ( 'NONE',  ( 41.84726577509989909, 12.36321918212159865, -3.460729483473919732 ) ) ;
#3002 = CARTESIAN_POINT ( 'NONE',  ( 67.20199456633837087, -29.99687375860984062, -17.36203811242810957 ) ) ;
#3003 = CARTESIAN_POINT ( 'NONE',  ( -22.60072279458010058, -20.15755767129849829, -54.65015892017029842 ) ) ;
#3004 = DIRECTION ( 'NONE',  ( 0.000000000000000000, 0.000000000000000000, -1.000000000000000000 ) ) ;
#3005 = CARTESIAN_POINT ( 'NONE',  ( 67.04038824939742369, -50.70395984888145335, -73.25000000000218847 ) ) ;
#3006 = ADVANCED_FACE ( 'NONE', ( #24426 ), #9001, .T. ) ;
#3007 = CARTESIAN_POINT ( 'NONE',  ( 75.74828555535219721, -43.35025879547261951, -13.50093798269990053 ) ) ;
#3008 = CARTESIAN_POINT ( 'NONE',  ( 17.87926713331770046, -52.17875626651990473, -75.87012052777591009 ) ) ;
#3009 = CARTESIAN_POINT ( 'NONE',  ( 53.17864038894789758, -45.11618894467940066, -9.007559113946960849 ) ) ;
#3010 = CARTESIAN_POINT ( 'NONE',  ( 23.39063669964830083, -17.30349732769349913, -65.14006310354538698 ) ) ;
#3011 =( BOUNDED_CURVE ( )  B_SPLINE_CURVE ( 3, ( #22961, #38453, #19308, #2557 ),
 .UNSPECIFIED., .F., .T. ) 
 B_SPLINE_CURVE_WITH_KNOTS ( ( 4, 4 ),
 ( 5.063167621403719565, 6.283185307179586232 ),
 .UNSPECIFIED. ) 
 CURVE ( )  GEOMETRIC_REPRESENTATION_ITEM ( )  RATIONAL_B_SPLINE_CURVE ( ( 1.000000000000000000, 0.8797619680071214754, 0.8797619680071214754, 1.000000000000000000 ) ) 
 REPRESENTATION_ITEM ( '' )  );
#3012 = CARTESIAN_POINT ( 'NONE',  ( 63.62053861216700312, 1.408710407023049838, -62.16810826758219832 ) ) ;
#3013 = ORIENTED_EDGE ( 'NONE', *, *, #31196, .F. ) ;
#3014 = CARTESIAN_POINT ( 'NONE',  ( 2.774651518975000286, 25.39333629030980433, -11.69507786875200139 ) ) ;
#3015 = CARTESIAN_POINT ( 'NONE',  ( 69.73393739769620936, 10.88381105532070059, -61.94999999999999574 ) ) ;
#3016 = CARTESIAN_POINT ( 'NONE',  ( 73.03020225798630349, 1.267233196669030004, -68.81685389259939711 ) ) ;
#3017 = DIRECTION ( 'NONE',  ( 0.8660254037844387076, 0.4999999999999998890, 0.000000000000000000 ) ) ;
#3018 = AXIS2_PLACEMENT_3D ( 'NONE', #927, #12465, #4082 ) ;
#3019 = CARTESIAN_POINT ( 'NONE',  ( 16.13393739769620083, -45.61618894467940066, -35.14999999999999858 ) ) ;
#3020 = CARTESIAN_POINT ( 'NONE',  ( 45.08949527824870529, -45.82276084545720352, -8.804711001959010019 ) ) ;
#3021 = ORIENTED_EDGE ( 'NONE', *, *, #3116, .F. ) ;
#3022 = AXIS2_PLACEMENT_3D ( 'NONE', #41140, #50042, #10473 ) ;
#3023 = ORIENTED_EDGE ( 'NONE', *, *, #31311, .T. ) ;
#3024 = ORIENTED_EDGE ( 'NONE', *, *, #16197, .T. ) ;
#3025 = DIRECTION ( 'NONE',  ( 0.000000000000000000, 0.000000000000000000, 1.000000000000000000 ) ) ;
#3026 = CARTESIAN_POINT ( 'NONE',  ( 22.62424293246530382, -11.35212744648809924, -81.23899999999999011 ) ) ;
#3027 = CARTESIAN_POINT ( 'NONE',  ( 53.55386411653459788, -49.42051784504710099, -49.22808815827509932 ) ) ;
#3028 = LINE ( 'NONE', #46551, #19304 ) ;
#3029 = EDGE_LOOP ( 'NONE', ( #40475, #35569 ) ) ;
#3030 = CARTESIAN_POINT ( 'NONE',  ( 22.13393739769619728, -54.15188668067469990, -54.64999999999999858 ) ) ;
#3031 = VERTEX_POINT ( 'NONE', #17122 ) ;
#3032 = DIRECTION ( 'NONE',  ( -1.000000000000000000, 0.000000000000000000, 0.000000000000000000 ) ) ;
#3033 = ADVANCED_FACE ( 'NONE', ( #33075 ), #49103, .T. ) ;
#3034 = DIRECTION ( 'NONE',  ( 1.000000000000000000, 0.000000000000000000, 0.000000000000000000 ) ) ;
#3035 = VERTEX_POINT ( 'NONE', #29153 ) ;
#3036 = CARTESIAN_POINT ( 'NONE',  ( 9.781452946156626638, -20.36976900595904283, -50.30319433359476733 ) ) ;
#3037 = CARTESIAN_POINT ( 'NONE',  ( 52.14830239089789643, -51.14206852341889942, -76.06502807251010267 ) ) ;
#3038 = CARTESIAN_POINT ( 'NONE',  ( 60.69566241836140819, 14.32434429444830037, -47.28745234666029518 ) ) ;
#3039 = B_SPLINE_CURVE_WITH_KNOTS ( 'NONE', 3,
 ( #34854, #29875, #2646, #13919, #45895, #10249, #46422, #30401, #34328, #10510 ),
 .UNSPECIFIED., .F., .F.,
 ( 4, 2, 2, 2, 4 ),
 ( 0.000000000000000000, 0.08716332209593161129, 0.1743266441918632226, 0.2614899662877948616, 0.3486532883837264452 ),
 .UNSPECIFIED. ) ;
#3040 = CIRCLE ( 'NONE', #44899, 22.00000000000000000 ) ;
#3041 = DIRECTION ( 'NONE',  ( 0.000000000000000000, 0.000000000000000000, -1.000000000000000000 ) ) ;
#3042 = B_SPLINE_CURVE_WITH_KNOTS ( 'NONE', 3,
 ( #13509, #17175, #33906, #29464 ),
 .UNSPECIFIED., .F., .F.,
 ( 4, 4 ),
 ( 6.761997042909579925, 6.813952014709780514 ),
 .UNSPECIFIED. ) ;
#3043 = CARTESIAN_POINT ( 'NONE',  ( 42.11778985043759604, -43.34518763914169881, -3.278435071288769542 ) ) ;
#3044 = PLANE ( 'NONE',  #41262 ) ;
#3045 = CARTESIAN_POINT ( 'NONE',  ( -6.129785861383029832, 15.32157675170519973, -5.280748218974210317 ) ) ;
#3046 = CARTESIAN_POINT ( 'NONE',  ( 1.057008924473209932, -22.58759019641090049, -34.64999999999999858 ) ) ;
#3047 = CIRCLE ( 'NONE', #39905, 16.00000000000000000 ) ;
#3048 = FACE_OUTER_BOUND ( 'NONE', #4439, .T. ) ;
#3049 = DIRECTION ( 'NONE',  ( 0.000000000000000000, -1.000000000000000000, 0.000000000000000000 ) ) ;
#3050 = CARTESIAN_POINT ( 'NONE',  ( 12.31011725209880048, -8.763076682552949137, -50.62550482836309840 ) ) ;
#3051 = ORIENTED_EDGE ( 'NONE', *, *, #5133, .T. ) ;
#3052 = AXIS2_PLACEMENT_3D ( 'NONE', #26799, #47261, #6385 ) ;
#3053 = CARTESIAN_POINT ( 'NONE',  ( 61.29923170577789904, 16.44081181233369904, -45.87705507641510394 ) ) ;
#3054 = CARTESIAN_POINT ( 'NONE',  ( 57.43212237869229853, 18.98854805440929994, -52.72827966158989454 ) ) ;
#3055 = CARTESIAN_POINT ( 'NONE',  ( 71.66453485656519717, 1.138495779907619854, -70.44670231041529007 ) ) ;
#3056 = CARTESIAN_POINT ( 'NONE',  ( 44.80053834244425559, -40.01632457077029414, -62.78033700576844467 ) ) ;
#3057 = CARTESIAN_POINT ( 'NONE',  ( 15.94236692260559884, 19.75473188654670054, -20.14988694616360121 ) ) ;
#3058 = DIRECTION ( 'NONE',  ( 0.4646601886423053496, 0.000000000000000000, 0.8854890790353641128 ) ) ;
#3059 = CARTESIAN_POINT ( 'NONE',  ( 17.74966129736979781, -22.48146355349690140, -45.27360529711679504 ) ) ;
#3060 = CARTESIAN_POINT ( 'NONE',  ( 63.51397770047800861, 1.389468113695450091, -68.84985728199801258 ) ) ;
#3061 = CARTESIAN_POINT ( 'NONE',  ( 47.91340349060840254, -54.37608934015739948, -54.84711144667770810 ) ) ;
#3062 = CARTESIAN_POINT ( 'NONE',  ( 24.04493711684570201, -15.61369914127065428, -45.50757579690004206 ) ) ;
#3063 = AXIS2_PLACEMENT_3D ( 'NONE', #5647, #49672, #10086 ) ;
#3064 = ADVANCED_FACE ( 'NONE', ( #4800 ), #12937, .T. ) ;
#3065 = CARTESIAN_POINT ( 'NONE',  ( 56.41630124387919665, 19.34388386770270074, -52.96295731896090331 ) ) ;
#3066 = CARTESIAN_POINT ( 'NONE',  ( 20.11811137678875738, -22.52868662009152700, -37.84100380649100970 ) ) ;
#3067 = CARTESIAN_POINT ( 'NONE',  ( 47.75515754607199881, 23.22926032546549990, -54.87660553739110014 ) ) ;
#3068 = VERTEX_POINT ( 'NONE', #1389 ) ;
#3069 = ADVANCED_FACE ( 'NONE', ( #49358 ), #28630, .T. ) ;
#3070 = CARTESIAN_POINT ( 'NONE',  ( 17.86626912417429836, -8.779407102036641319, -74.42617192852868868 ) ) ;
#3071 = EDGE_CURVE ( 'NONE', #1664, #31547, #152, .T. ) ;
#3072 = VERTEX_POINT ( 'NONE', #32289 ) ;
#3073 = CARTESIAN_POINT ( 'NONE',  ( 71.37448966235888292, 1.264489825601020190, -70.50788383491540401 ) ) ;
#3074 = CARTESIAN_POINT ( 'NONE',  ( 13.00893739769619906, 34.28605925116850273, -47.75434321204170374 ) ) ;
#3075 = VECTOR ( 'NONE', #10209, 999.9999999999998863 ) ;
#3076 = CARTESIAN_POINT ( 'NONE',  ( 48.73678662100336823, -53.88539940205524914, -54.49010856789386281 ) ) ;
#3077 = CARTESIAN_POINT ( 'NONE',  ( 53.29384558423090112, 19.31433099946569953, -28.15000000000000213 ) ) ;
#3079 = CARTESIAN_POINT ( 'NONE',  ( 68.13393739769620083, 0.8838110553206759423, -65.65000000000000568 ) ) ;
#3078 = CARTESIAN_POINT ( 'NONE',  ( 40.85150231246245056, 8.399356969744889767, -81.87147178968719174 ) ) ;
#3081 = EDGE_CURVE ( 'NONE', #32578, #45801, #8506, .T. ) ;
#3080 = DIRECTION ( 'NONE',  ( -0.08481436951012806535, 0.9963967697281035374, 0.000000000000000000 ) ) ;
#3082 = CARTESIAN_POINT ( 'NONE',  ( 0.1457839871805957643, 14.73018012514992137, -34.68167748489143776 ) ) ;
#3083 = DIRECTION ( 'NONE',  ( 0.000000000000000000, -1.000000000000000000, 0.000000000000000000 ) ) ;
#3084 = ORIENTED_EDGE ( 'NONE', *, *, #11613, .T. ) ;
#3085 = CARTESIAN_POINT ( 'NONE',  ( 28.63393739769619728, -22.83306730954970121, -34.64999999999999858 ) ) ;
#3086 = ORIENTED_EDGE ( 'NONE', *, *, #7688, .F. ) ;
#3087 = ORIENTED_EDGE ( 'NONE', *, *, #20357, .F. ) ;
#3088 = DIRECTION ( 'NONE',  ( -0.04251717301921301151, 0.000000000000000000, 0.9990957361526743297 ) ) ;
#3089 = DIRECTION ( 'NONE',  ( 0.000000000000000000, 0.000000000000000000, 1.000000000000000000 ) ) ;
#3090 = DIRECTION ( 'NONE',  ( 0.000000000000000000, 0.000000000000000000, 1.000000000000000000 ) ) ;
#3091 = CARTESIAN_POINT ( 'NONE',  ( 11.15267625120379869, -65.14072497951910634, -47.20537807037530342 ) ) ;
#3092 = VECTOR ( 'NONE', #7022, 1000.000000000000000 ) ;
#3093 = EDGE_CURVE ( 'NONE', #20898, #15133, #12365, .T. ) ;
#3094 = ORIENTED_EDGE ( 'NONE', *, *, #49692, .F. ) ;
#3095 = ORIENTED_EDGE ( 'NONE', *, *, #32922, .F. ) ;
#3096 = CARTESIAN_POINT ( 'NONE',  ( 53.70964822437330355, 20.71768139653399743, -54.24308104583559498 ) ) ;
#3097 = VECTOR ( 'NONE', #18125, 1000.000000000000000 ) ;
#3098 = PLANE ( 'NONE',  #42125 ) ;
#3099 = FACE_OUTER_BOUND ( 'NONE', #13841, .T. ) ;
#3100 = CARTESIAN_POINT ( 'NONE',  ( 68.13393739769618662, -0.5161889446793590519, -65.65000000000000568 ) ) ;
#3101 = CARTESIAN_POINT ( 'NONE',  ( 64.80898460781330073, -0.3417096974386910624, -16.69305045354919770 ) ) ;
#3102 = ADVANCED_FACE ( 'NONE', ( #8736 ), #32539, .T. ) ;
#3103 = CARTESIAN_POINT ( 'NONE',  ( 51.64973235580259825, -49.25056687465429661, -76.82386385094510217 ) ) ;
#3104 = DIRECTION ( 'NONE',  ( 0.000000000000000000, 1.000000000000000000, 0.000000000000000000 ) ) ;
#3105 = VERTEX_POINT ( 'NONE', #867 ) ;
#3106 = CARTESIAN_POINT ( 'NONE',  ( 18.20470550922528119, -23.32126401386723202, -48.20899934070940418 ) ) ;
#3107 = CARTESIAN_POINT ( 'NONE',  ( 29.13393739769619728, -26.76363820448759867, -35.14999999999999858 ) ) ;
#3108 = CARTESIAN_POINT ( 'NONE',  ( 18.20468139625259596, -23.32127082703616949, -53.92433694102878405 ) ) ;
#3109 = CARTESIAN_POINT ( 'NONE',  ( 16.84904414660969962, -23.43126219636669916, -42.48344881935029349 ) ) ;
#3110 = CARTESIAN_POINT ( 'NONE',  ( 13.17520392672940055, -50.89446949932710851, -21.60492300268700205 ) ) ;
#3111 = CARTESIAN_POINT ( 'NONE',  ( 56.07939589478549891, 19.38381105532069881, -75.94606253248319661 ) ) ;
#3112 = FACE_OUTER_BOUND ( 'NONE', #29817, .T. ) ;
#3113 = CARTESIAN_POINT ( 'NONE',  ( 56.76189318125270233, 13.89673976699089941, -16.10745061695219960 ) ) ;
#3114 = CARTESIAN_POINT ( 'NONE',  ( 8.919738259460300966, 18.05571844226340161, -34.65024031912469837 ) ) ;
#3115 = CARTESIAN_POINT ( 'NONE',  ( 71.09849264842429761, 1.384887413063060180, -70.31636399389039127 ) ) ;
#3116 = EDGE_CURVE ( 'NONE', #11348, #17454, #51187, .T. ) ;
#3117 = CARTESIAN_POINT ( 'NONE',  ( 21.16241148139290118, -20.56159161423429893, -39.09452867415449617 ) ) ;
#3118 = DIRECTION ( 'NONE',  ( 0.000000000000000000, 0.000000000000000000, -1.000000000000000000 ) ) ;
#3119 = ORIENTED_EDGE ( 'NONE', *, *, #32389, .F. ) ;
#3120 = CARTESIAN_POINT ( 'NONE',  ( 14.33439054234879961, -51.26614876192449799, -74.93568190819630104 ) ) ;
#3121 = CARTESIAN_POINT ( 'NONE',  ( 64.89338513303370348, 1.264489825601020190, -60.79211616508469973 ) ) ;
#3122 = CARTESIAN_POINT ( 'NONE',  ( 23.62400244246320113, 17.52418497763099836, -35.12503119152809461 ) ) ;
#3123 = CARTESIAN_POINT ( 'NONE',  ( 17.71568183981793609, 20.46959823935371503, -75.56421430877649925 ) ) ;
#3124 = CARTESIAN_POINT ( 'NONE',  ( 8.830271178173081381, -49.11659379690700433, -34.68023162149790295 ) ) ;
#3125 = AXIS2_PLACEMENT_3D ( 'NONE', #49091, #44619, #21274 ) ;
#3126 = DIRECTION ( 'NONE',  ( -1.000000000000000000, -9.178581432917707304E-26, 1.529205156547310004E-10 ) ) ;
#3127 = CARTESIAN_POINT ( 'NONE',  ( 82.37381124112360453, 13.88258767056099963, -46.56085682599739783 ) ) ;
#3128 = CARTESIAN_POINT ( 'NONE',  ( 12.32273708341836915, -8.640312908610901843, -64.84861858487673203 ) ) ;
#3130 = CARTESIAN_POINT ( 'NONE',  ( 23.83903819154209458, -17.68686180718279743, -57.87566458210246623 ) ) ;
#3129 = CARTESIAN_POINT ( 'NONE',  ( 47.64143405046823432, 23.30250931194617436, -74.17387245449363320 ) ) ;
#3131 = CARTESIAN_POINT ( 'NONE',  ( 18.96081146330753597, -8.159879717317295444, -71.12286597728768811 ) ) ;
#3132 = B_SPLINE_CURVE_WITH_KNOTS ( 'NONE', 3,
 ( #37543, #7394, #3721, #3467, #14737, #51420, #47743, #35418, #51164, #15514, #23852, #50899, #23600, #34900, #14991, #15257, #31468, #47492 ),
 .UNSPECIFIED., .F., .F.,
 ( 4, 2, 2, 2, 2, 2, 2, 2, 4 ),
 ( 0.000000000000000000, 0.06249980403246548771, 0.1249996080649309754, 0.1874994120973964562, 0.2499992161298619509, 0.3124990201623274455, 0.3749988241947929124, 0.4374986282272584348, 0.4999984322597239017 ),
 .UNSPECIFIED. ) ;
#3133 = CARTESIAN_POINT ( 'NONE',  ( 68.13393739769620083, -15.61618894467929941, -65.65000000000000568 ) ) ;
#3134 = ORIENTED_EDGE ( 'NONE', *, *, #31521, .T. ) ;
#3135 = EDGE_CURVE ( 'NONE', #7519, #50005, #39973, .T. ) ;
#3136 = CARTESIAN_POINT ( 'NONE',  ( 52.93745306185230248, -49.61473117453819981, -48.89566031930959866 ) ) ;
#3137 = ORIENTED_EDGE ( 'NONE', *, *, #30281, .T. ) ;
#3138 = CARTESIAN_POINT ( 'NONE',  ( 46.99535652950729059, 8.020657431200683973, -55.88807232857796947 ) ) ;
#3139 = CARTESIAN_POINT ( 'NONE',  ( 9.367118387258660306, -15.61602127472129986, -41.45282021618999835 ) ) ;
#3140 = CARTESIAN_POINT ( 'NONE',  ( 14.05648281248510045, 19.92572429859249894, -22.83284005205619849 ) ) ;
#3141 = CARTESIAN_POINT ( 'NONE',  ( 51.99247890846820042, -49.49757107862999561, -77.11022715351130330 ) ) ;
#3142 = CARTESIAN_POINT ( 'NONE',  ( 14.55382961656019880, -22.48974829167110201, -57.02474435397660102 ) ) ;
#3144 = EDGE_CURVE ( 'NONE', #14662, #21348, #29924, .T. ) ;
#3143 = CARTESIAN_POINT ( 'NONE',  ( 53.15617284440619983, 18.31170051411429966, -49.11047172704059705 ) ) ;
#3145 = CARTESIAN_POINT ( 'NONE',  ( 54.56504510741340397, -45.97009618579260604, -15.64073160589219924 ) ) ;
#3146 = DIRECTION ( 'NONE',  ( 1.000000000000000000, 0.000000000000000000, 0.000000000000000000 ) ) ;
#3147 = ORIENTED_EDGE ( 'NONE', *, *, #22468, .F. ) ;
#3148 = CARTESIAN_POINT ( 'NONE',  ( 14.53095738391709979, -7.933948783221270951, -32.72202640798520434 ) ) ;
#3149 = EDGE_LOOP ( 'NONE', ( #47032, #20928, #29403, #20478, #18997, #6953, #32467, #41663 ) ) ;
#3150 = CARTESIAN_POINT ( 'NONE',  ( 53.59007319875249920, 18.17385789302069554, -49.22505640236219904 ) ) ;
#3151 = CARTESIAN_POINT ( 'NONE',  ( 11.74846882065989995, 34.09090366579489739, -47.38045816806030075 ) ) ;
#3152 = CARTESIAN_POINT ( 'NONE',  ( 73.01702207920239118, 1.186614556332920234, -62.31696408872340243 ) ) ;
#3153 = CARTESIAN_POINT ( 'NONE',  ( 49.98909701452470244, -52.82152540991150147, -53.22897615407840277 ) ) ;
#3154 = DIRECTION ( 'NONE',  ( 1.000000000000000000, 0.000000000000000000, 0.000000000000000000 ) ) ;
#3155 = CARTESIAN_POINT ( 'NONE',  ( 7.234750459571823278, -9.150551169462135093, -84.65000000000000568 ) ) ;
#3156 = CARTESIAN_POINT ( 'NONE',  ( 52.62939598134340002, -52.19035112265739684, -53.52988853690619919 ) ) ;
#3157 = EDGE_LOOP ( 'NONE', ( #8378, #16844, #1669, #13148, #19636, #26018 ) ) ;
#3158 = PLANE ( 'NONE',  #13451 ) ;
#3159 = CARTESIAN_POINT ( 'NONE',  ( 10.77213108896340010, -63.27130156652651038, -45.20475918482989641 ) ) ;
#3160 = CARTESIAN_POINT ( 'NONE',  ( 69.22748654599826068, 19.47158195952208004, -70.40645085170191919 ) ) ;
#3161 = ORIENTED_EDGE ( 'NONE', *, *, #11523, .F. ) ;
#3162 = CARTESIAN_POINT ( 'NONE',  ( 19.52320908822511569, -22.84352052172154401, -44.15244030110604712 ) ) ;
#3163 = DIRECTION ( 'NONE',  ( 1.000000000000000000, 0.000000000000000000, 0.000000000000000000 ) ) ;
#3164 = CARTESIAN_POINT ( 'NONE',  ( 53.36305338436599754, 19.31849222244400011, -76.89765214543919569 ) ) ;
#3165 = ORIENTED_EDGE ( 'NONE', *, *, #21582, .T. ) ;
#3166 = DIRECTION ( 'NONE',  ( 0.000000000000000000, 0.000000000000000000, 1.000000000000000000 ) ) ;
#3167 = CARTESIAN_POINT ( 'NONE',  ( 51.19516202202958510, 19.86383965925710626, -76.13919812682924260 ) ) ;
#3168 = CARTESIAN_POINT ( 'NONE',  ( 13.80921672251139931, -22.01564006803594964, -33.06388420368715941 ) ) ;
#3169 = VECTOR ( 'NONE', #37471, 1000.000000000000000 ) ;
#3170 = CARTESIAN_POINT ( 'NONE',  ( 32.63393739769630031, -15.61618894467929941, -6.649999999999999467 ) ) ;
#3171 = CARTESIAN_POINT ( 'NONE',  ( 9.618119672177739332, -20.66859821390469776, -58.58238571580489662 ) ) ;
#3172 = CARTESIAN_POINT ( 'NONE',  ( 24.04523214473702097, -15.61618869705131729, -47.50766735973101618 ) ) ;
#3173 = DIRECTION ( 'NONE',  ( -0.000000000000000000, -1.000000000000000000, -0.000000000000000000 ) ) ;
#3174 = AXIS2_PLACEMENT_3D ( 'NONE', #21807, #1647, #5591 ) ;
#3175 = VERTEX_POINT ( 'NONE', #37541 ) ;
#3176 = ORIENTED_EDGE ( 'NONE', *, *, #46926, .T. ) ;
#3177 = DIRECTION ( 'NONE',  ( 1.000000000000000000, 0.000000000000000000, 0.000000000000000000 ) ) ;
#3178 = CARTESIAN_POINT ( 'NONE',  ( 23.37302340462380457, -17.37753149780470352, -50.30862910410869659 ) ) ;
#3179 = EDGE_CURVE ( 'NONE', #3226, #41446, #4843, .T. ) ;
#3180 = CARTESIAN_POINT ( 'NONE',  ( 50.04794199436929603, 13.88381105532070059, -10.32001505388980078 ) ) ;
#3181 = DIRECTION ( 'NONE',  ( -0.05886216378138799110, 0.000000000000000000, -0.9982661196669817549 ) ) ;
#3182 = EDGE_CURVE ( 'NONE', #2875, #11745, #13280, .T. ) ;
#3183 = CARTESIAN_POINT ( 'NONE',  ( 56.61928439928508539, 14.09173447728649720, -31.98003398807230369 ) ) ;
#3184 = DIRECTION ( 'NONE',  ( 0.000000000000000000, 0.000000000000000000, -1.000000000000000000 ) ) ;
#3185 = EDGE_CURVE ( 'NONE', #30141, #12739, #17382, .T. ) ;
#3186 = FACE_OUTER_BOUND ( 'NONE', #42684, .T. ) ;
#3187 = CARTESIAN_POINT ( 'NONE',  ( 11.80495200725580140, 33.73638531772620297, -16.40176568414450031 ) ) ;
#3188 = CARTESIAN_POINT ( 'NONE',  ( 23.21148977389540136, -19.84596116917700215, -63.67913456332050259 ) ) ;
#3189 = CARTESIAN_POINT ( 'NONE',  ( 22.02707644877200011, -20.53240942572870154, -32.14999999999999858 ) ) ;
#3190 = CARTESIAN_POINT ( 'NONE',  ( 55.10512401493469525, -51.00770816830609533, -75.23756392707410612 ) ) ;
#3192 = CARTESIAN_POINT ( 'NONE',  ( 23.06214062797170072, -27.61618894467930119, -32.14999999999999858 ) ) ;
#3191 = CARTESIAN_POINT ( 'NONE',  ( -1.714040913996900173, 19.72568320566199773, -6.699893841482610135 ) ) ;
#3193 = CARTESIAN_POINT ( 'NONE',  ( 14.13393739769619906, -32.62399965035220362, -35.14999999999999858 ) ) ;
#3194 = DIRECTION ( 'NONE',  ( -1.000000000000000000, 0.000000000000000000, 0.000000000000000000 ) ) ;
#3195 = EDGE_LOOP ( 'NONE', ( #1272, #7409, #51083, #35729 ) ) ;
#3196 = CARTESIAN_POINT ( 'NONE',  ( -10.89209614968750017, -42.33678087173180415, -6.195842417017019876 ) ) ;
#3197 = CARTESIAN_POINT ( 'NONE',  ( 47.67808432772210381, 23.28069921495480088, -55.00342241055910364 ) ) ;
#3198 = AXIS2_PLACEMENT_3D ( 'NONE', #34860, #2381, #45902 ) ;
#3199 = DIRECTION ( 'NONE',  ( 0.000000000000000000, 0.000000000000000000, -1.000000000000000000 ) ) ;
#3200 = DIRECTION ( 'NONE',  ( 0.000000000000000000, 0.000000000000000000, -1.000000000000000000 ) ) ;
#3201 = CARTESIAN_POINT ( 'NONE',  ( 61.20223082393160041, 14.41488311889550111, -47.73662807001939967 ) ) ;
#3202 = CARTESIAN_POINT ( 'NONE',  ( 20.58572098376589921, -9.642218563498740735, -79.93650932190229241 ) ) ;
#3203 = CARTESIAN_POINT ( 'NONE',  ( 51.69077939775340269, 18.09910883672219839, -76.83272513777849611 ) ) ;
#3205 = EDGE_CURVE ( 'NONE', #32305, #6987, #34633, .T. ) ;
#3204 = CARTESIAN_POINT ( 'NONE',  ( 52.83011278983949666, 18.42835579809699809, -48.49876830664469907 ) ) ;
#3206 = DIRECTION ( 'NONE',  ( 0.000000000000000000, 1.000000000000000000, 0.000000000000000000 ) ) ;
#3207 = CARTESIAN_POINT ( 'NONE',  ( 53.36494266454960211, -49.38052133118390685, -48.76947209987829979 ) ) ;
#3208 = CARTESIAN_POINT ( 'NONE',  ( 52.77133031265780261, 18.46082998801760056, -28.15002739903220075 ) ) ;
#3209 = DIRECTION ( 'NONE',  ( 0.000000000000000000, 0.000000000000000000, -1.000000000000000000 ) ) ;
#3210 = CARTESIAN_POINT ( 'NONE',  ( 10.98008937475129976, -63.44096224164839981, -44.74889856825390666 ) ) ;
#3211 = CARTESIAN_POINT ( 'NONE',  ( 52.57435089425080577, 18.62009177781090230, -48.51307714252150305 ) ) ;
#3212 = CARTESIAN_POINT ( 'NONE',  ( 59.91580961932370286, -29.59054676811280160, -15.87157813189650213 ) ) ;
#3213 = CARTESIAN_POINT ( 'NONE',  ( 71.05099032166229733, 1.383136297697689976, -60.93121850368469694 ) ) ;
#3214 = CARTESIAN_POINT ( 'NONE',  ( 11.13393739769619906, 32.12568940449459376, -43.74939087321740061 ) ) ;
#3215 = CARTESIAN_POINT ( 'NONE',  ( 72.49387005411300322, 1.113948672550079788, -61.53426704495930011 ) ) ;
#3216 = CARTESIAN_POINT ( 'NONE',  ( 51.35985510312087143, -34.56615178299539082, -76.65611151696774073 ) ) ;
#3217 = CARTESIAN_POINT ( 'NONE',  ( 65.03603135424570780, -29.76883965895069650, -19.52361391316379979 ) ) ;
#3218 = ORIENTED_EDGE ( 'NONE', *, *, #42829, .T. ) ;
#3219 = EDGE_LOOP ( 'NONE', ( #48871, #17949, #41493, #25278 ) ) ;
#3220 = DIRECTION ( 'NONE',  ( 0.000000000000000000, 1.000000000000000000, 0.000000000000000000 ) ) ;
#3221 = CARTESIAN_POINT ( 'NONE',  ( 51.12546901458399162, 0.3428415324802153163, -17.03913216448443180 ) ) ;
#3222 = ORIENTED_EDGE ( 'NONE', *, *, #8942, .T. ) ;
#3223 = CARTESIAN_POINT ( 'NONE',  ( 57.55914395453869759, -45.13105435620409622, -25.54764931287219909 ) ) ;
#3224 = CARTESIAN_POINT ( 'NONE',  ( 14.84447007510781980, -23.42568434902701213, -78.05974216284950273 ) ) ;
#3225 = CARTESIAN_POINT ( 'NONE',  ( -0.007164427059776000244, -4.186223695871990280, -34.77269723891829756 ) ) ;
#3226 = VERTEX_POINT ( 'NONE', #38326 ) ;
#3227 = CARTESIAN_POINT ( 'NONE',  ( -11.80944000494479873, 2.826328597561450273, -45.03554556751399929 ) ) ;
#3228 = CARTESIAN_POINT ( 'NONE',  ( 43.41473102517175420, 6.605039987487077546, -73.24597267587351723 ) ) ;
#3229 = CARTESIAN_POINT ( 'NONE',  ( 11.37709144110930026, 32.70230954837069959, -24.34844091950509792 ) ) ;
#3230 = ORIENTED_EDGE ( 'NONE', *, *, #3666, .T. ) ;
#3231 = CARTESIAN_POINT ( 'NONE',  ( 23.19779881621899875, -19.86867582181319847, -31.96482487842879650 ) ) ;
#3232 = CARTESIAN_POINT ( 'NONE',  ( 51.21170306502393998, 0.4771360739093502001, -17.17315678632984799 ) ) ;
#3233 = CARTESIAN_POINT ( 'NONE',  ( 10.62399636376403222, 33.60002598301907994, -18.14935807941716561 ) ) ;
#3234 = CARTESIAN_POINT ( 'NONE',  ( 9.787098110040155063, -18.04122145005927536, -51.33655066882005968 ) ) ;
#3235 = CARTESIAN_POINT ( 'NONE',  ( 61.83357513733750466, -29.34433711196260219, -16.03557146812989842 ) ) ;
#3236 = B_SPLINE_CURVE_WITH_KNOTS ( 'NONE', 3,
 ( #15853, #24459, #36270, #4310, #44408, #21061, #12184, #47833, #36528, #4564, #31812, #634, #48864, #16620, #380, #32574, #24975, #130 ),
 .UNSPECIFIED., .F., .F.,
 ( 4, 2, 1, 1, 2, 2, 2, 1, 1, 2, 4 ),
 ( 0.5114743812812451162, 0.5267408068662060572, 0.5420072324511669981, 0.5725400836210982058, 0.6336057859609515175, 0.7557371906406565865, 0.7710036162256185266, 0.7862700418105804667, 0.8168028929804922456, 0.8778685953203280157, 1.000000000000000000 ),
 .UNSPECIFIED. ) ;
#3237 = CARTESIAN_POINT ( 'NONE',  ( 14.48179410283199431, 20.27135663923558084, -75.33783710295330138 ) ) ;
#3238 = CARTESIAN_POINT ( 'NONE',  ( 46.56684587109570117, -53.31662439353189598, -76.10144452841760199 ) ) ;
#3239 = CARTESIAN_POINT ( 'NONE',  ( 83.89200044194980421, 17.38381105532069881, -53.92796738110899923 ) ) ;
#3240 = CIRCLE ( 'NONE', #28344, 6.100000000000001421 ) ;
#3241 = CIRCLE ( 'NONE', #30110, 5.499999999999998224 ) ;
#3242 = EDGE_CURVE ( 'NONE', #16604, #49444, #38596, .T. ) ;
#3243 = CARTESIAN_POINT ( 'NONE',  ( 9.366602974803960535, -15.61605382581650048, -49.84717978381009118 ) ) ;
#3244 = ADVANCED_FACE ( 'NONE', ( #45675 ), #33706, .T. ) ;
#3245 = CARTESIAN_POINT ( 'NONE',  ( 83.96875769672529088, -44.33360226143160787, -47.04741150093960300 ) ) ;
#3246 = CARTESIAN_POINT ( 'NONE',  ( 38.67452568954060155, -36.11618894467930119, -81.65000000000000568 ) ) ;
#3247 = CARTESIAN_POINT ( 'NONE',  ( 11.52974377330020062, -22.18186745672379701, -32.20281262070909634 ) ) ;
#3248 = ORIENTED_EDGE ( 'NONE', *, *, #42965, .T. ) ;
#3249 = CARTESIAN_POINT ( 'NONE',  ( 52.95491184103799753, -49.55317193531470110, -27.75869128885100068 ) ) ;
#3250 = CARTESIAN_POINT ( 'NONE',  ( 7.377761082898449452, -59.78252037510630856, -11.86817158160470065 ) ) ;
#3251 = CARTESIAN_POINT ( 'NONE',  ( 75.83364580603620198, 0.5632187979614480255, -12.28588720292489889 ) ) ;
#3252 = CARTESIAN_POINT ( 'NONE',  ( 75.32649906090206571, 13.28935024932845543, -13.93656188709756272 ) ) ;
#3253 = CARTESIAN_POINT ( 'NONE',  ( 54.36675628530516491, -46.16659547561676646, 11.34999999999999964 ) ) ;
#3254 = FACE_OUTER_BOUND ( 'NONE', #19514, .T. ) ;
#3255 = CARTESIAN_POINT ( 'NONE',  ( 24.04493740109851529, -16.65173145406349775, -37.83400117407241936 ) ) ;
#3256 = CARTESIAN_POINT ( 'NONE',  ( 82.13853704237929776, -45.43815991012449729, -47.46441090728419709 ) ) ;
#3257 = CARTESIAN_POINT ( 'NONE',  ( 57.29916422955370336, -50.56256534964890648, -53.44854448085349929 ) ) ;
#3258 = CARTESIAN_POINT ( 'NONE',  ( 41.72814282206219616, 12.57486269224770048, -4.012820143008159590 ) ) ;
#3260 = EDGE_CURVE ( 'NONE', #50203, #24767, #5776, .T. ) ;
#3259 = CARTESIAN_POINT ( 'NONE',  ( 9.205734167420699166, -27.61618894467930119, -32.14999999999999858 ) ) ;
#3261 = DIRECTION ( 'NONE',  ( 0.000000000000000000, -1.000000000000000000, 0.000000000000000000 ) ) ;
#3262 = CARTESIAN_POINT ( 'NONE',  ( 53.48663704675579567, -49.34136594389470076, -49.00013169077909936 ) ) ;
#3263 = DIRECTION ( 'NONE',  ( -1.000000000000000000, 0.000000000000000000, 0.000000000000000000 ) ) ;
#3264 = CARTESIAN_POINT ( 'NONE',  ( 31.58225770014201572, -28.80002732852027947, -29.09832030244561807 ) ) ;
#3265 = CARTESIAN_POINT ( 'NONE',  ( 17.68198299984170063, -51.79680004542600358, -75.65449215554859563 ) ) ;
#3266 = EDGE_CURVE ( 'NONE', #17159, #22505, #30542, .T. ) ;
#3267 = CARTESIAN_POINT ( 'NONE',  ( 43.34846246081870191, -44.39964076787359915, -5.297725289369729751 ) ) ;
#3268 = CARTESIAN_POINT ( 'NONE',  ( 19.50497178776589990, -22.26019537749590071, -69.41788538098089134 ) ) ;
#3269 = CARTESIAN_POINT ( 'NONE',  ( 63.31978766800359892, 1.229084191802120030, -62.25930094257930136 ) ) ;
#3270 = ORIENTED_EDGE ( 'NONE', *, *, #33939, .T. ) ;
#3271 = DIRECTION ( 'NONE',  ( 0.7071067811865475727, -0.7071067811865475727, 0.000000000000000000 ) ) ;
#3272 = CYLINDRICAL_SURFACE ( 'NONE', #30970, 3.500000000000003109 ) ;
#3273 = CARTESIAN_POINT ( 'NONE',  ( 72.80768847295010460, 1.384447124000270035, -68.59133994763901399 ) ) ;
#3274 = VECTOR ( 'NONE', #25563, 1000.000000000000000 ) ;
#3275 = CARTESIAN_POINT ( 'NONE',  ( 9.543102826887107426, -13.84480091498138421, -73.53615355050735047 ) ) ;
#3276 = VECTOR ( 'NONE', #34005, 1000.000000000000000 ) ;
#3277 = CARTESIAN_POINT ( 'NONE',  ( 10.10545813131939852, -11.17681743330739863, -81.23899999999999011 ) ) ;
#3278 = CARTESIAN_POINT ( 'NONE',  ( 41.02380400077039724, -45.31415305091180556, -5.860748674566660377 ) ) ;
#3279 = ORIENTED_EDGE ( 'NONE', *, *, #2016, .T. ) ;
#3280 = CARTESIAN_POINT ( 'NONE',  ( 17.51665066424190087, 21.64019965034970028, -76.12465403027070465 ) ) ;
#3281 = VERTEX_POINT ( 'NONE', #26189 ) ;
#3282 = EDGE_LOOP ( 'NONE', ( #18547, #37830, #47118, #35387 ) ) ;
#3283 = CARTESIAN_POINT ( 'NONE',  ( 16.13393739769620083, -15.61618894467929941, -44.64999999999999858 ) ) ;
#3284 = CARTESIAN_POINT ( 'NONE',  ( 23.56919067231890352, -15.75467248557949773, -81.23899999999999011 ) ) ;
#3285 = DIRECTION ( 'NONE',  ( 0.000000000000000000, 0.000000000000000000, -1.000000000000000000 ) ) ;
#3286 = CYLINDRICAL_SURFACE ( 'NONE', #36887, 6.766999999999998572 ) ;
#3287 = VERTEX_POINT ( 'NONE', #45876 ) ;
#3288 = CARTESIAN_POINT ( 'NONE',  ( 17.16947923318423008, -7.705188139706350192, -53.04933681370027188 ) ) ;
#3289 = EDGE_LOOP ( 'NONE', ( #27738, #42439, #25974, #5934, #12896, #19451, #33209 ) ) ;
#3290 = LINE ( 'NONE', #6711, #35160 ) ;
#3291 = ORIENTED_EDGE ( 'NONE', *, *, #44590, .T. ) ;
#3292 = CARTESIAN_POINT ( 'NONE',  ( 44.13393739769620083, 1.883811055320659955, -54.27132075603810080 ) ) ;
#3293 = CARTESIAN_POINT ( 'NONE',  ( 51.19067522064119657, -50.75340530090790025, -76.16618595621679333 ) ) ;
#3294 = CARTESIAN_POINT ( 'NONE',  ( 61.13208011586430501, 14.28537189261369988, -47.54663226922669850 ) ) ;
#3295 = CARTESIAN_POINT ( 'NONE',  ( 22.85695788854713228, -14.82042754783183547, -40.41532941938547907 ) ) ;
#3296 = ADVANCED_FACE ( 'NONE', ( #41938 ), #6038, .T. ) ;
#3297 = FACE_OUTER_BOUND ( 'NONE', #27923, .T. ) ;
#3298 = CARTESIAN_POINT ( 'NONE',  ( -7.972635851128819340, 13.79869975764560053, -5.396154554284530391 ) ) ;
#3299 = AXIS2_PLACEMENT_3D ( 'NONE', #36928, #12572, #758 ) ;
#3300 = TOROIDAL_SURFACE ( 'NONE', #47640, 36.00000000000000000, 2.000000000000000000 ) ;
#3301 = CARTESIAN_POINT ( 'NONE',  ( 0.3209249304026170480, -15.61618894467929941, -35.14999999999999858 ) ) ;
#3302 = CARTESIAN_POINT ( 'NONE',  ( -31.36606260230380272, 21.88381105532059934, 16.35000000000000142 ) ) ;
#3303 = CIRCLE ( 'NONE', #12509, 9.768249999999998323 ) ;
#3304 = CIRCLE ( 'NONE', #16693, 39.39359268544610870 ) ;
#3305 = CARTESIAN_POINT ( 'NONE',  ( 21.03233565530110027, -9.484921319377349391, -53.00207276027180114 ) ) ;
#3306 = ORIENTED_EDGE ( 'NONE', *, *, #34954, .T. ) ;
#3307 = DIRECTION ( 'NONE',  ( -0.1961161351381836004, -1.134894647394604573E-15, -0.9805806756909204447 ) ) ;
#3309 = CONICAL_SURFACE ( 'NONE', #30936, 0.6299999999999942313, 0.7853981633974476129 ) ;
#3308 = FACE_OUTER_BOUND ( 'NONE', #3812, .T. ) ;
#3310 = UNCERTAINTY_MEASURE_WITH_UNIT (LENGTH_MEASURE( 1.000000000000000082E-05 ), #12066, 'distance_accuracy_value', 'NONE');
#3311 = CARTESIAN_POINT ( 'NONE',  ( 72.11129086675759936, 1.099201050715699957, -70.13622689935800736 ) ) ;
#3312 = CARTESIAN_POINT ( 'NONE',  ( 45.06945685171515947, -40.03533966481339945, -61.47576887606990681 ) ) ;
#3313 = DIRECTION ( 'NONE',  ( -1.000000000000000000, 0.000000000000000000, 0.000000000000000000 ) ) ;
#3314 =( BOUNDED_CURVE ( )  B_SPLINE_CURVE ( 2, ( #6934, #22889, #6156 ),
 .UNSPECIFIED., .F., .F. ) 
 B_SPLINE_CURVE_WITH_KNOTS ( ( 3, 3 ),
 ( 0.09013418064815610642, 2.097305204714880134 ),
 .UNSPECIFIED. ) 
 CURVE ( )  GEOMETRIC_REPRESENTATION_ITEM ( )  RATIONAL_B_SPLINE_CURVE ( ( 1.000760730674140175, 1.008874108732590091, 1.001093714201509943 ) ) 
 REPRESENTATION_ITEM ( '' )  );
#3315 = FACE_OUTER_BOUND ( 'NONE', #12503, .T. ) ;
#3316 = CARTESIAN_POINT ( 'NONE',  ( 22.89998289909242501, -16.39251803772393856, -44.88370135509944703 ) ) ;
#3317 = CARTESIAN_POINT ( 'NONE',  ( 16.13393739769620083, -15.61618894467929941, -19.83999999999999986 ) ) ;
#3318 = CARTESIAN_POINT ( 'NONE',  ( 48.49374681402279919, -54.15253515020039998, -55.04500232426880046 ) ) ;
#3319 = CARTESIAN_POINT ( 'NONE',  ( 63.28787718588009881, 0.9170817191178709527, -69.18823203240749820 ) ) ;
#3320 = CARTESIAN_POINT ( 'NONE',  ( 23.83903359263120336, -17.68688467594312996, -45.87568617554371286 ) ) ;
#3321 = ADVANCED_FACE ( 'NONE', ( #22256 ), #38263, .F. ) ;
#3322 = CARTESIAN_POINT ( 'NONE',  ( 47.64964229006460528, 23.29901286050539966, -55.13082436213569792 ) ) ;
#3323 = ORIENTED_EDGE ( 'NONE', *, *, #7860, .F. ) ;
#3324 = CARTESIAN_POINT ( 'NONE',  ( 21.42514567518789903, -10.37121405310790045, -32.81873922958869372 ) ) ;
#3325 = B_SPLINE_CURVE_WITH_KNOTS ( 'NONE', 3,
 ( #4241, #32248, #20463, #560, #16545, #5547, #36986, #49827, #9980, #13918, #21240, #29874, #41689, #41180, #41431, #17841 ),
 .UNSPECIFIED., .F., .F.,
 ( 4, 2, 2, 2, 2, 2, 2, 4 ),
 ( -8.881783999999999608E-16, 0.4504854996693090086, 0.8526915253703870601, 1.105340866220869911, 1.263246704252430019, 1.579058380315530030, 2.084357062016500173, 2.526493408504850269 ),
 .UNSPECIFIED. ) ;
#3326 = ORIENTED_EDGE ( 'NONE', *, *, #1568, .F. ) ;
#3327 = CARTESIAN_POINT ( 'NONE',  ( 71.31427394968270050, 1.395196698723390138, -70.24366017557039754 ) ) ;
#3328 = DIRECTION ( 'NONE',  ( 1.000000000000000000, 0.000000000000000000, 0.000000000000000000 ) ) ;
#3329 = CARTESIAN_POINT ( 'NONE',  ( 61.28610897262619517, 13.99802247707942549, -27.88820104294108049 ) ) ;
#3330 = CARTESIAN_POINT ( 'NONE',  ( 82.45630311851421368, 13.86034003618500066, -46.38988467804559690 ) ) ;
#3332 = CARTESIAN_POINT ( 'NONE',  ( 22.58711562570864118, -12.98538437038062021, -58.72346069000413848 ) ) ;
#3331 = CARTESIAN_POINT ( 'NONE',  ( 83.85375176557759858, 13.60279395407959946, -47.43402238021350570 ) ) ;
#3333 = DIRECTION ( 'NONE',  ( 0.000000000000000000, 8.281569874363147012E-12, -1.000000000000000000 ) ) ;
#3334 = CARTESIAN_POINT ( 'NONE',  ( 8.222955670729223954, -16.65187018699299060, -42.46600177219022498 ) ) ;
#3335 = CARTESIAN_POINT ( 'NONE',  ( 13.00893739761190027, 34.28605925116320208, -47.75434321210310173 ) ) ;
#3336 = ORIENTED_EDGE ( 'NONE', *, *, #76, .F. ) ;
#3337 = CARTESIAN_POINT ( 'NONE',  ( 84.44421879469800274, -43.32357668338529777, -47.46023938497990002 ) ) ;
#3338 = ORIENTED_EDGE ( 'NONE', *, *, #27033, .F. ) ;
#3339 = APPLICATION_CONTEXT ( 'automotive_design' ) ;
#3340 = ORIENTED_EDGE ( 'NONE', *, *, #31431, .T. ) ;
#3341 = DIRECTION ( 'NONE',  ( 0.000000000000000000, 0.000000000000000000, -1.000000000000000000 ) ) ;
#3342 = CIRCLE ( 'NONE', #24244, 17.09468304687050022 ) ;
#3343 = CARTESIAN_POINT ( 'NONE',  ( 9.221362871281039375, -11.63214536758718154, -38.95899421604067214 ) ) ;
#3344 = VECTOR ( 'NONE', #27194, 1000.000000000000000 ) ;
#3345 = CARTESIAN_POINT ( 'NONE',  ( 76.47407931131914438, -26.68129154492521593, -13.11572213019135269 ) ) ;
#3346 = CARTESIAN_POINT ( 'NONE',  ( 10.80326701815859991, -65.00358748232589789, -47.10395893127729749 ) ) ;
#3347 = AXIS2_PLACEMENT_3D ( 'NONE', #9560, #14261, #37581 ) ;
#3348 = EDGE_LOOP ( 'NONE', ( #26588, #12846, #38879, #28504, #5324, #24502, #22940, #36585, #42126 ) ) ;
#3349 = AXIS2_PLACEMENT_3D ( 'NONE', #48071, #12169, #32553 ) ;
#3350 = VERTEX_POINT ( 'NONE', #43927 ) ;
#3351 = CARTESIAN_POINT ( 'NONE',  ( 71.33393739769670105, 1.396834109478129804, -61.06337307536569625 ) ) ;
#3352 = CARTESIAN_POINT ( 'NONE',  ( 56.97449864924389829, -45.18768938411730574, -25.30071454757920435 ) ) ;
#3353 = CARTESIAN_POINT ( 'NONE',  ( 56.45679588454890308, -50.65543487096700659, -53.17273421675590583 ) ) ;
#3354 = VECTOR ( 'NONE', #19123, 1000.000000000000000 ) ;
#3355 = CARTESIAN_POINT ( 'NONE',  ( 21.47698520338149564, -11.41770701216577422, -46.24076139810592423 ) ) ;
#3356 = CARTESIAN_POINT ( 'NONE',  ( 61.22840165282480029, -0.4342326450878930544, -16.42153289494959978 ) ) ;
#3357 = CARTESIAN_POINT ( 'NONE',  ( 52.21414320235400197, -49.80349422312119856, -77.10081889737340077 ) ) ;
#3358 = CARTESIAN_POINT ( 'NONE',  ( 14.46582891625718048, -52.64324137128869552, -76.02665054608532103 ) ) ;
#3359 = VERTEX_POINT ( 'NONE', #23974 ) ;
#3360 = CARTESIAN_POINT ( 'NONE',  ( 64.93393739769609851, 11.38381105532070059, -61.94999999999999574 ) ) ;
#3361 = FACE_OUTER_BOUND ( 'NONE', #4018, .T. ) ;
#3362 = CARTESIAN_POINT ( 'NONE',  ( 12.72603898113892917, -9.703224850274590807, -51.78615268828129814 ) ) ;
#3363 = CARTESIAN_POINT ( 'NONE',  ( 53.59003930803689997, -49.40628012469949937, -49.22510501142529904 ) ) ;
#3364 = CARTESIAN_POINT ( 'NONE',  ( 17.29970893726160241, -23.37684125676760161, -52.46503413336629507 ) ) ;
#3365 = CARTESIAN_POINT ( 'NONE',  ( 13.50258242280349918, -50.13280576151589685, -20.96779971433539913 ) ) ;
#3366 = EDGE_CURVE ( 'NONE', #50035, #6096, #8024, .T. ) ;
#3367 = CARTESIAN_POINT ( 'NONE',  ( 9.366931599644679807, -15.61636246440640008, -63.84717978381009118 ) ) ;
#3368 = CARTESIAN_POINT ( 'NONE',  ( 56.63655303576899769, 13.89710862042509909, -15.89230735191339861 ) ) ;
#3370 = EDGE_CURVE ( 'NONE', #24679, #4176, #35816, .T. ) ;
#3369 = CARTESIAN_POINT ( 'NONE',  ( 61.06130050885990102, -45.43944728382009401, -47.36071542247660204 ) ) ;
#3371 = ADVANCED_FACE ( 'NONE', ( #23725 ), #26599, .T. ) ;
#3372 = DIRECTION ( 'NONE',  ( 0.000000000000000000, 0.000000000000000000, 1.000000000000000000 ) ) ;
#3373 = CARTESIAN_POINT ( 'NONE',  ( 22.00814659178010047, -11.71282814677829975, -50.66049260944289045 ) ) ;
#3374 = CARTESIAN_POINT ( 'NONE',  ( 16.13393739769620083, -15.61618894467929941, -34.64999999999999858 ) ) ;
#3375 = EDGE_CURVE ( 'NONE', #27673, #17098, #39949, .T. ) ;
#3376 = ORIENTED_EDGE ( 'NONE', *, *, #16874, .F. ) ;
#3377 = CARTESIAN_POINT ( 'NONE',  ( 14.28772440699220070, -51.14708712906860200, -74.55381114264599773 ) ) ;
#3378 = CARTESIAN_POINT ( 'NONE',  ( 64.89029781878299730, 1.096291039689149871, -60.65158056017160249 ) ) ;
#3379 = CIRCLE ( 'NONE', #36019, 1.000000000000000888 ) ;
#3380 = CARTESIAN_POINT ( 'NONE',  ( 41.58940156010519473, -45.68696317153209918, -6.490026235633630236 ) ) ;
#3381 = CARTESIAN_POINT ( 'NONE',  ( 34.63393739830264906, -15.61618894523020806, 9.349999999709213583 ) ) ;
#3382 = CIRCLE ( 'NONE', #21765, 3.000000000000001776 ) ;
#3383 = CARTESIAN_POINT ( 'NONE',  ( 10.30441904797920216, -10.14968042360930056, -54.74717805172168994 ) ) ;
#3384 = AXIS2_PLACEMENT_3D ( 'NONE', #29488, #44706, #25545 ) ;
#3385 = EDGE_CURVE ( 'NONE', #15485, #43570, #11557, .T. ) ;
#3386 = AXIS2_PLACEMENT_3D ( 'NONE', #38353, #49190, #18172 ) ;
#3388 = CONICAL_SURFACE ( 'NONE', #62, 1.079032500000002059, 0.7853981633974469467 ) ;
#3387 = CARTESIAN_POINT ( 'NONE',  ( 46.87137491217979601, -53.55967532393449915, -75.98463753095340678 ) ) ;
#3389 = CARTESIAN_POINT ( 'NONE',  ( 82.55523265057320259, 14.39697247100306043, -47.70981245347169875 ) ) ;
#3390 = CARTESIAN_POINT ( 'NONE',  ( 72.96483387528870423, 0.9208623934721549276, -69.20867653485849758 ) ) ;
#3392 = CARTESIAN_POINT ( 'NONE',  ( 44.37201056559310075, -37.88618800308559997, -68.45424654654109986 ) ) ;
#3391 = CARTESIAN_POINT ( 'NONE',  ( 51.67587649748560352, -48.61618894467930119, -77.01363636363639387 ) ) ;
#3393 = CARTESIAN_POINT ( 'NONE',  ( 18.95485614926927198, -23.03702254430130836, -32.17677060365137720 ) ) ;
#3394 = EDGE_CURVE ( 'NONE', #12214, #19324, #646, .T. ) ;
#3395 = CARTESIAN_POINT ( 'NONE',  ( 49.18437675156140187, 22.63228536849929995, -55.01176516154440321 ) ) ;
#3396 = ORIENTED_EDGE ( 'NONE', *, *, #43459, .T. ) ;
#3397 = CARTESIAN_POINT ( 'NONE',  ( 53.46717762220459491, -49.39950009416709520, -49.11454733997430111 ) ) ;
#3398 = ORIENTED_EDGE ( 'NONE', *, *, #47916, .F. ) ;
#3399 = CARTESIAN_POINT ( 'NONE',  ( 42.99808947197828957, 6.368226865670313153, -75.30230971069127577 ) ) ;
#3400 = DIRECTION ( 'NONE',  ( 0.000000000000000000, 0.000000000000000000, -1.000000000000000000 ) ) ;
#3401 = CARTESIAN_POINT ( 'NONE',  ( 13.90975851214690096, 19.95031597149180058, -22.51682738170260123 ) ) ;
#3402 = FACE_OUTER_BOUND ( 'NONE', #33535, .T. ) ;
#3403 = CARTESIAN_POINT ( 'NONE',  ( 10.50288950272969934, -11.36955989315870141, -57.65849580248539752 ) ) ;
#3404 = CARTESIAN_POINT ( 'NONE',  ( 52.97994248284770435, 18.38655893702810218, -49.03242408102300232 ) ) ;
#3405 = CARTESIAN_POINT ( 'NONE',  ( 55.89887109364280349, -45.90872632089149619, -17.63256066653320175 ) ) ;
#3406 = CARTESIAN_POINT ( 'NONE',  ( 83.89200044194980421, -50.48013859002959691, -53.20292136905285929 ) ) ;
#3407 = VERTEX_POINT ( 'NONE', #19559 ) ;
#3408 = CARTESIAN_POINT ( 'NONE',  ( 12.77237362966949874, -22.26499250170639854, -79.71634641925140841 ) ) ;
#3409 = ORIENTED_EDGE ( 'NONE', *, *, #14707, .T. ) ;
#3410 = CARTESIAN_POINT ( 'NONE',  ( 11.25424580253960016, -65.03526282482160070, -16.95782958517590089 ) ) ;
#3411 = CARTESIAN_POINT ( 'NONE',  ( 12.48759467934699963, 34.23991394352330531, -47.62022110721400026 ) ) ;
#3412 = CARTESIAN_POINT ( 'NONE',  ( 72.81333620972418430, 1.370853092582090094, -62.43091793016829882 ) ) ;
#3413 = CARTESIAN_POINT ( 'NONE',  ( 52.21171052997630113, -50.80767995673200232, -50.87743900096490535 ) ) ;
#3414 = CARTESIAN_POINT ( 'NONE',  ( 52.97667589433369528, -49.63212252085852327, -49.06651684377276723 ) ) ;
#3415 = CARTESIAN_POINT ( 'NONE',  ( 8.223031589278729570, -15.61632747405269939, -32.50766849176289952 ) ) ;
#3416 = EDGE_CURVE ( 'NONE', #9581, #17232, #26702, .T. ) ;
#3417 = ORIENTED_EDGE ( 'NONE', *, *, #29651, .T. ) ;
#3418 = CARTESIAN_POINT ( 'NONE',  ( -15.86606260230380094, -15.61618894467929941, -20.15000000000000213 ) ) ;
#3419 = CARTESIAN_POINT ( 'NONE',  ( 10.49497832658790131, -63.36864664907449196, -45.62743361653370044 ) ) ;
#3420 = LINE ( 'NONE', #35372, #25198 ) ;
#3421 = VERTEX_POINT ( 'NONE', #16138 ) ;
#3422 = CARTESIAN_POINT ( 'NONE',  ( 67.45368031047163981, -32.84183613245724587, -19.55784004926478303 ) ) ;
#3423 = CARTESIAN_POINT ( 'NONE',  ( 56.41694091142689871, 19.34565818385159730, -52.96189704198110348 ) ) ;
#3424 = CARTESIAN_POINT ( 'NONE',  ( 16.13393739769620083, -15.61618894467929941, -35.14999999999999858 ) ) ;
#3425 = VERTEX_POINT ( 'NONE', #35549 ) ;
#3426 = CARTESIAN_POINT ( 'NONE',  ( 44.94022070389027590, -33.11618894467929408, -54.43277924001892387 ) ) ;
#3427 = CARTESIAN_POINT ( 'NONE',  ( 51.42797782268906559, 19.97168430531649719, -76.10787250224279887 ) ) ;
#3428 = CARTESIAN_POINT ( 'NONE',  ( 82.45630311851421368, -45.09271792554360303, -46.38988467804559690 ) ) ;
#3429 = CARTESIAN_POINT ( 'NONE',  ( 8.223340741289188571, -15.61635616670070092, -42.79233150823699816 ) ) ;
#3430 = CIRCLE ( 'NONE', #17636, 3.500000000000003109 ) ;
#3431 = CARTESIAN_POINT ( 'NONE',  ( 24.36517369343270190, -16.09521827539409955, -63.81083516600379113 ) ) ;
#3432 = PLANE ( 'NONE',  #48129 ) ;
#3433 = CARTESIAN_POINT ( 'NONE',  ( 61.04001029137710077, -45.35933836075930259, -46.86320535112459851 ) ) ;
#3434 = DIRECTION ( 'NONE',  ( 1.000000000000000000, 0.000000000000000000, 0.000000000000000000 ) ) ;
#3435 = ORIENTED_EDGE ( 'NONE', *, *, #44316, .T. ) ;
#3436 = ORIENTED_EDGE ( 'NONE', *, *, #6939, .T. ) ;
#3437 = B_SPLINE_CURVE_WITH_KNOTS ( 'NONE', 3,
 ( #14956, #34603, #47459, #15222, #27003, #43011, #10519, #39325, #47205, #50606, #6850, #26735, #27513, #46432, #26477, #42494, #6583, #31175 ),
 .UNSPECIFIED., .F., .F.,
 ( 4, 2, 2, 2, 2, 2, 2, 2, 4 ),
 ( 0.4999984322597239017, 0.5624986282272584903, 0.6249988241947930234, 0.6874990201623275565, 0.7499992161298620896, 0.8124994120973966227, 0.8749996080649310448, 0.9374998040324655779, 1.000000000000000000 ),
 .UNSPECIFIED. ) ;
#3438 = DIRECTION ( 'NONE',  ( -0.4316160343590931259, -0.9020574254913764634, 0.000000000000000000 ) ) ;
#3439 = CARTESIAN_POINT ( 'NONE',  ( 23.53416472175010199, -16.47835444936559668, -54.26957565728959310 ) ) ;
#3440 = CARTESIAN_POINT ( 'NONE',  ( 53.41947877929930399, -49.46401953720199884, -49.21225703112880012 ) ) ;
#3441 = CARTESIAN_POINT ( 'NONE',  ( 50.39461351434339775, -50.13496434787850120, -76.14999999999999147 ) ) ;
#3442 = CARTESIAN_POINT ( 'NONE',  ( 9.718336914000449411, -19.70433485797880380, -32.14999999999999858 ) ) ;
#3443 = ADVANCED_FACE ( 'NONE', ( #51539 ), #25754, .T. ) ;
#3444 = CARTESIAN_POINT ( 'NONE',  ( 47.20691373745980002, 23.45218668536150020, -74.72489560329549363 ) ) ;
#3445 = DIRECTION ( 'NONE',  ( -0.5779418439120764805, 0.8120748150972384449, -0.08073239585380144467 ) ) ;
#3446 = DIRECTION ( 'NONE',  ( -0.5110015285683607855, -0.4887508954475661693, -0.7071067811865481278 ) ) ;
#3447 = CARTESIAN_POINT ( 'NONE',  ( 12.21465728044820054, 33.46871344512319979, -15.93455456221940025 ) ) ;
#3448 = CARTESIAN_POINT ( 'NONE',  ( 12.64353542633499927, -8.146261583098500125, -72.86853056670030071 ) ) ;
#3449 = CARTESIAN_POINT ( 'NONE',  ( 21.21709022629629970, -21.48422859372540117, -32.14999999999999858 ) ) ;
#3450 = CARTESIAN_POINT ( 'NONE',  ( 55.74676111446309790, -50.61618894632059806, -76.24128155003170093 ) ) ;
#3452 = CARTESIAN_POINT ( 'NONE',  ( 30.78462454764483169, -35.68771960809947785, -84.61927628510844102 ) ) ;
#3451 = CARTESIAN_POINT ( 'NONE',  ( -9.494487167629941382, 12.56563882403370158, -6.502785074734050319 ) ) ;
#3453 = CARTESIAN_POINT ( 'NONE',  ( 63.02699984107479025, 0.9952464559119579279, -68.78371246661670568 ) ) ;
#3454 = ADVANCED_FACE ( 'NONE', ( #35495, #20003 ), #19761, .T. ) ;
#3455 = LINE ( 'NONE', #35677, #7197 ) ;
#3456 = ORIENTED_EDGE ( 'NONE', *, *, #50652, .F. ) ;
#3457 = CIRCLE ( 'NONE', #9331, 1.999999999999996669 ) ;
#3458 = CARTESIAN_POINT ( 'NONE',  ( -9.120882960642459736, -44.01580188134359872, -5.427931969706110138 ) ) ;
#3459 = TOROIDAL_SURFACE ( 'NONE', #13496, 2.999999897106000013, 1.999999999830609942 ) ;
#3460 = CARTESIAN_POINT ( 'NONE',  ( 47.74455983969129846, 23.22759274665880014, -54.83598561554559581 ) ) ;
#3461 = LINE ( 'NONE', #23594, #41261 ) ;
#3462 = CARTESIAN_POINT ( 'NONE',  ( 8.317988017466229067, -17.01659171872782750, -66.73595314439963033 ) ) ;
#3463 = CARTESIAN_POINT ( 'NONE',  ( 61.31447405025300412, 14.34038816827110097, -47.65179949294859796 ) ) ;
#3464 = CARTESIAN_POINT ( 'NONE',  ( 23.06708755827619939, -12.88889676084650127, -70.11336187001349174 ) ) ;
#3465 = CARTESIAN_POINT ( 'NONE',  ( 52.21413925781470056, 18.57111292375499900, -77.10081778803849772 ) ) ;
#3466 = CARTESIAN_POINT ( 'NONE',  ( 53.18571383884999904, 18.24204644525839925, -48.81732522206360159 ) ) ;
#3467 = CARTESIAN_POINT ( 'NONE',  ( 9.221449781846978055, -19.60038109878267321, -70.62566536415043572 ) ) ;
#3468 = CARTESIAN_POINT ( 'NONE',  ( -0.3684971866671489238, -45.31814476460159824, -35.08739145837887463 ) ) ;
#3469 = CARTESIAN_POINT ( 'NONE',  ( 51.00410689780089513, 21.58760788935499875, -53.76372497442359588 ) ) ;
#3470 = CARTESIAN_POINT ( 'NONE',  ( 16.29993763818361430, -23.52570124991906653, -62.00099320790554458 ) ) ;
#3471 = CARTESIAN_POINT ( 'NONE',  ( 22.46009718676461375, -10.75450352810032051, -37.58400065247785449 ) ) ;
#3472 = DIRECTION ( 'NONE',  ( 0.000000000000000000, 0.000000000000000000, 1.000000000000000000 ) ) ;
#3473 = CARTESIAN_POINT ( 'NONE',  ( 59.04235398677249691, -28.10938722064719641, -15.65226459872759790 ) ) ;
#3474 = CARTESIAN_POINT ( 'NONE',  ( 71.35858828687760536, 1.188042061556800144, -60.70318061837799917 ) ) ;
#3475 = FACE_OUTER_BOUND ( 'NONE', #27619, .T. ) ;
#3476 = CARTESIAN_POINT ( 'NONE',  ( 72.49279582477680606, 1.028300555801489935, -61.52602141601349928 ) ) ;
#3477 = EDGE_CURVE ( 'NONE', #13741, #41355, #8180, .T. ) ;
#3478 = CARTESIAN_POINT ( 'NONE',  ( 16.89732681591289776, -22.62759363779219868, -41.31265874393579907 ) ) ;
#3479 = DIRECTION ( 'NONE',  ( 0.000000000000000000, 0.000000000000000000, 1.000000000000000000 ) ) ;
#3480 = ORIENTED_EDGE ( 'NONE', *, *, #42206, .F. ) ;
#3481 = ADVANCED_FACE ( 'NONE', ( #51485 ), #16102, .T. ) ;
#3482 = VERTEX_POINT ( 'NONE', #4041 ) ;
#3483 = DIRECTION ( 'NONE',  ( 0.000000000000000000, 1.000000000000000000, 0.000000000000000000 ) ) ;
#3484 = CARTESIAN_POINT ( 'NONE',  ( 1.864336597259699468, -25.98366078385575761, 14.62639320225000006 ) ) ;
#3485 = ORIENTED_EDGE ( 'NONE', *, *, #25888, .T. ) ;
#3486 = CARTESIAN_POINT ( 'NONE',  ( 57.38200685792909894, -45.11824297016489993, -25.39251393572369864 ) ) ;
#3487 = CARTESIAN_POINT ( 'NONE',  ( 14.08272732913061809, -23.27416204732341853, -78.09098556571072436 ) ) ;
#3488 = ADVANCED_FACE ( 'NONE', ( #35997 ), #48321, .F. ) ;
#3489 = DIRECTION ( 'NONE',  ( 0.000000000000000000, 0.000000000000000000, 1.000000000000000000 ) ) ;
#3490 = ORIENTED_EDGE ( 'NONE', *, *, #21143, .T. ) ;
#3491 = CARTESIAN_POINT ( 'NONE',  ( 10.64863409883700029, 32.21085600226960111, -23.66469670114080159 ) ) ;
#3492 = CARTESIAN_POINT ( 'NONE',  ( 43.38751250541962889, 6.601242059090285608, -73.38206190525755801 ) ) ;
#3493 = CARTESIAN_POINT ( 'NONE',  ( 12.34051464139020027, 34.21035364286279901, -23.27951631307980307 ) ) ;
#3494 = VERTEX_POINT ( 'NONE', #44129 ) ;
#3495 = CARTESIAN_POINT ( 'NONE',  ( 12.19021776734980023, -8.375346760609819086, -35.13358212097350020 ) ) ;
#3496 = CARTESIAN_POINT ( 'NONE',  ( 0.3209249304026170480, -26.47788675693900018, -34.64999999999999858 ) ) ;
#3497 = CARTESIAN_POINT ( 'NONE',  ( 65.46029542295769943, -1.463538230407920082, -16.55376543218019947 ) ) ;
#3498 = CARTESIAN_POINT ( 'NONE',  ( 59.44268701500750041, -28.43641637611329998, -15.69409845278869930 ) ) ;
#3499 = EDGE_CURVE ( 'NONE', #33091, #3494, #5082, .T. ) ;
#3500 = AXIS2_PLACEMENT_3D ( 'NONE', #30825, #46853, #10941 ) ;
#3501 = DIRECTION ( 'NONE',  ( 0.000000000000000000, 1.000000000000000000, 0.000000000000000000 ) ) ;
#3502 = CARTESIAN_POINT ( 'NONE',  ( 46.35275103504449845, -52.90993241930539881, -76.14999999999999147 ) ) ;
#3503 = CARTESIAN_POINT ( 'NONE',  ( 9.898752574389790837, -20.38160789906219961, -74.80477269330690149 ) ) ;
#3504 = CIRCLE ( 'NONE', #36960, 13.00000000000000178 ) ;
#3505 = AXIS2_PLACEMENT_3D ( 'NONE', #31358, #7032, #10962 ) ;
#3506 = CARTESIAN_POINT ( 'NONE',  ( 40.78718667651179430, 13.97481543807150040, -5.637855851295809906 ) ) ;
#3507 = EDGE_CURVE ( 'NONE', #35613, #9275, #29894, .T. ) ;
#3508 = CARTESIAN_POINT ( 'NONE',  ( 10.25785795057082872, 23.94995057986916365, -45.86872051532979100 ) ) ;
#3509 = CARTESIAN_POINT ( 'NONE',  ( 84.38271246941039294, -43.47090129257950508, -47.29654027836490116 ) ) ;
#3510 = CARTESIAN_POINT ( 'NONE',  ( 27.13393739769620083, 7.383811055320659733, -72.14999999999999147 ) ) ;
#3511 = CARTESIAN_POINT ( 'NONE',  ( 18.53886225874440186, -23.50282682920819965, -39.91345524423469726 ) ) ;
#3512 = ORIENTED_EDGE ( 'NONE', *, *, #17381, .F. ) ;
#3513 = CARTESIAN_POINT ( 'NONE',  ( 53.31766142530319996, -49.23794969896809448, -27.39069684441169983 ) ) ;
#3514 = CARTESIAN_POINT ( 'NONE',  ( 14.22165922049939901, -50.54429837671820280, -21.01402899346189912 ) ) ;
#3515 = CARTESIAN_POINT ( 'NONE',  ( 75.31916300594728853, -5.906200963950169580, -11.62634963242759945 ) ) ;
#3516 = CARTESIAN_POINT ( 'NONE',  ( 75.41772322313477162, 12.83423812364906169, -13.62006770663721689 ) ) ;
#3517 = CYLINDRICAL_SURFACE ( 'NONE', #18958, 2.999999999999999112 ) ;
#3518 = DIRECTION ( 'NONE',  ( 0.000000000000000000, 0.000000000000000000, -1.000000000000000000 ) ) ;
#3519 = CARTESIAN_POINT ( 'NONE',  ( -0.03447620312153085176, -4.141051901845263394, -34.79644660940673617 ) ) ;
#3520 = CARTESIAN_POINT ( 'NONE',  ( 14.36278677302630591, -22.20708724394357958, -49.03615438224388612 ) ) ;
#3521 = CARTESIAN_POINT ( 'NONE',  ( 82.13853704237929776, -45.17484520962380401, -46.86219204859769860 ) ) ;
#3522 = CARTESIAN_POINT ( 'NONE',  ( 57.34721623897170417, -50.32126388940520201, -52.87018747239729777 ) ) ;
#3523 = CARTESIAN_POINT ( 'NONE',  ( 42.16203278445299674, 12.96059013387869818, -4.955231385700390234 ) ) ;
#3524 = CARTESIAN_POINT ( 'NONE',  ( 22.90093741918837722, -16.50198006501137016, -64.49448900876036816 ) ) ;
#3525 = CYLINDRICAL_SURFACE ( 'NONE', #20727, 14.50000000000000178 ) ;
#3526 = CARTESIAN_POINT ( 'NONE',  ( 53.82714908703680123, -49.13835843630199918, -48.71552173647079798 ) ) ;
#3527 = DIRECTION ( 'NONE',  ( -0.9304380493636941196, -0.3664492274467011090, 0.000000000000000000 ) ) ;
#3528 = CARTESIAN_POINT ( 'NONE',  ( 105.5832649133809156, -15.41618894467909051, -28.20067248431509199 ) ) ;
#3529 = CARTESIAN_POINT ( 'NONE',  ( 17.82691427187729971, -51.53888401296669741, -75.38689171750549178 ) ) ;
#3530 = CARTESIAN_POINT ( 'NONE',  ( 43.19159875137410154, -44.97844352163669868, -6.001981098335629206 ) ) ;
#3531 = VECTOR ( 'NONE', #19258, 1000.000000000000000 ) ;
#3532 = CARTESIAN_POINT ( 'NONE',  ( 23.50430387603210036, -14.52789104733479952, -61.02067868823719721 ) ) ;
#3533 = DIRECTION ( 'NONE',  ( 0.000000000000000000, 0.000000000000000000, -1.000000000000000000 ) ) ;
#3534 = CARTESIAN_POINT ( 'NONE',  ( 53.63393739769619373, -62.11618894467930119, 11.84999999999999964 ) ) ;
#3535 = ORIENTED_EDGE ( 'NONE', *, *, #13510, .T. ) ;
#3536 = DIRECTION ( 'NONE',  ( 0.000000000000000000, 1.205285871143275290E-11, 1.000000000000000000 ) ) ;
#3537 = CIRCLE ( 'NONE', #31112, 9.703299832284479010 ) ;
#3538 = SPHERICAL_SURFACE ( 'NONE', #19274, 2.000000000000000000 ) ;
#3539 = CARTESIAN_POINT ( 'NONE',  ( 72.92255733887110125, 1.374300485541529948, -68.58542282960749503 ) ) ;
#3540 = CARTESIAN_POINT ( 'NONE',  ( 73.24087495431770378, 0.9952464559119579279, -62.51628753338329858 ) ) ;
#3541 = CARTESIAN_POINT ( 'NONE',  ( 9.072718278985821172, -13.88952453628539985, -81.23899999999999011 ) ) ;
#3542 = EDGE_LOOP ( 'NONE', ( #2317, #36067, #29860, #17462, #34941, #27374 ) ) ;
#3543 = FACE_OUTER_BOUND ( 'NONE', #47129, .T. ) ;
#3544 = EDGE_CURVE ( 'NONE', #13029, #17698, #39292, .T. ) ;
#3545 = ORIENTED_EDGE ( 'NONE', *, *, #42948, .T. ) ;
#3546 = VERTEX_POINT ( 'NONE', #17130 ) ;
#3547 = PLANE ( 'NONE',  #36927 ) ;
#3548 = CARTESIAN_POINT ( 'NONE',  ( 23.33198322512879841, -13.07647044784360091, -81.23899999999999011 ) ) ;
#3549 = ADVANCED_FACE ( 'NONE', ( #13211 ), #33351, .T. ) ;
#3550 = CARTESIAN_POINT ( 'NONE',  ( 61.53725015800320364, 14.07761012407289947, -47.23307395042449741 ) ) ;
#3551 = ORIENTED_EDGE ( 'NONE', *, *, #2309, .F. ) ;
#3552 = CARTESIAN_POINT ( 'NONE',  ( 24.04493738849360795, -14.58064088933272373, -53.46600475365202954 ) ) ;
#3553 = ORIENTED_EDGE ( 'NONE', *, *, #50879, .T. ) ;
#3554 = CARTESIAN_POINT ( 'NONE',  ( 82.55417034916375485, 14.39382471871442881, -47.70637854188409221 ) ) ;
#3555 = CYLINDRICAL_SURFACE ( 'NONE', #36846, 1.000000000000000888 ) ;
#3556 = ORIENTED_EDGE ( 'NONE', *, *, #15841, .F. ) ;
#3557 = CARTESIAN_POINT ( 'NONE',  ( 44.68310481377952215, 1.934496889718864132, -44.40181776504896760 ) ) ;
#3558 = CARTESIAN_POINT ( 'NONE',  ( 51.18087450742270050, -50.74724387720399932, -76.16568686308029612 ) ) ;
#3559 = CARTESIAN_POINT ( 'NONE',  ( 60.28868092514770893, 14.57684442129959912, -47.55394404419389787 ) ) ;
#3560 = ADVANCED_FACE ( 'NONE', ( #4542, #36508 ), #48584, .T. ) ;
#3561 = CARTESIAN_POINT ( 'NONE',  ( 22.90093739503438641, -15.61216303397516647, -40.45263532482819357 ) ) ;
#3562 = EDGE_CURVE ( 'NONE', #43383, #48498, #39432, .T. ) ;
#3563 = FACE_OUTER_BOUND ( 'NONE', #32081, .T. ) ;
#3564 = CARTESIAN_POINT ( 'NONE',  ( -2.836119465579209908, 17.80585329168859943, -5.545754995944120580 ) ) ;
#3565 = AXIS2_PLACEMENT_3D ( 'NONE', #21246, #37255, #33309 ) ;
#3566 = B_SPLINE_CURVE_WITH_KNOTS ( 'NONE', 3,
 ( #9262, #17882, #29149, #45415, #28889, #5329, #49867, #17633, #44892, #25210 ),
 .UNSPECIFIED., .F., .F.,
 ( 4, 2, 2, 2, 4 ),
 ( 0.000000000000000000, 0.03537882351746304832, 0.3488581273460797383, 0.9706547651737063021, 1.000000000000000000 ),
 .UNSPECIFIED. ) ;
#3567 = VECTOR ( 'NONE', #12251, 1000.000000000000000 ) ;
#3568 = CIRCLE ( 'NONE', #27789, 2.000000000000060396 ) ;
#3569 = DIRECTION ( 'NONE',  ( 0.000000000000000000, -1.000000000000000000, 0.000000000000000000 ) ) ;
#3570 = CARTESIAN_POINT ( 'NONE',  ( -33.86606260230380627, -15.61618894467930474, -74.14999999999999147 ) ) ;
#3571 = CARTESIAN_POINT ( 'NONE',  ( 23.80689242842739972, -13.96921921831510005, -55.22020283005320351 ) ) ;
#3572 = ORIENTED_EDGE ( 'NONE', *, *, #2480, .F. ) ;
#3573 = DIRECTION ( 'NONE',  ( 0.8732394366197182567, 0.4872913772396111343, 1.665334536937735304E-16 ) ) ;
#3574 = CARTESIAN_POINT ( 'NONE',  ( 57.46463958512929793, 19.38381105532060289, -53.92796738110899923 ) ) ;
#3575 = CARTESIAN_POINT ( 'NONE',  ( 71.67217357260551580, 0.9170823515327879427, -70.49605724842400889 ) ) ;
#3576 = CARTESIAN_POINT ( 'NONE',  ( 43.43392086188707424, -39.90592420333850043, -69.40102220065354288 ) ) ;
#3577 = CARTESIAN_POINT ( 'NONE',  ( 14.89545651469759946, 19.58260512638929640, -21.03875510983240105 ) ) ;
#3578 = SURFACE_STYLE_USAGE ( .BOTH. , #47350 ) ;
#3579 = CYLINDRICAL_SURFACE ( 'NONE', #18691, 7.910999999999997812 ) ;
#3580 = CARTESIAN_POINT ( 'NONE',  ( 63.54731047306190561, 1.396834109478120034, -68.84999999999999432 ) ) ;
#3581 = CARTESIAN_POINT ( 'NONE',  ( 48.44792705533350130, -54.06183843665910160, -54.63497078953220409 ) ) ;
#3582 = CYLINDRICAL_SURFACE ( 'NONE', #37346, 1.999999999999995559 ) ;
#3583 = CARTESIAN_POINT ( 'NONE',  ( 23.83903782902317303, -17.68686365390393078, -37.59100454951404657 ) ) ;
#3584 = CARTESIAN_POINT ( 'NONE',  ( 47.82967227365460161, 23.17104661939929855, -54.77576043164239650 ) ) ;
#3585 = ORIENTED_EDGE ( 'NONE', *, *, #18831, .F. ) ;
#3586 = CARTESIAN_POINT ( 'NONE',  ( 23.55010335841370051, -14.90402549293309953, -35.03686929936998951 ) ) ;
#3587 = DIRECTION ( 'NONE',  ( -0.7782863420137342558, 0.3536342755907660451, 0.5188575613424891708 ) ) ;
#3588 = EDGE_LOOP ( 'NONE', ( #49351, #47072, #10285, #4049 ) ) ;
#3589 = CARTESIAN_POINT ( 'NONE',  ( 71.54590618381259048, 1.188860127980290171, -70.48451794758248923 ) ) ;
#3590 = CARTESIAN_POINT ( 'NONE',  ( 60.94474915215729993, -45.41359427234949919, -47.07753893340869666 ) ) ;
#3591 = CARTESIAN_POINT ( 'NONE',  ( 0.2007819157888829364, -20.71710295694509441, -34.66110989977897106 ) ) ;
#3592 = DIRECTION ( 'NONE',  ( 0.000000000000000000, 0.000000000000000000, -1.000000000000000000 ) ) ;
#3594 = CARTESIAN_POINT ( 'NONE',  ( 72.33393739769618946, 10.88381105532070059, -62.44999999999999574 ) ) ;
#3593 = CARTESIAN_POINT ( 'NONE',  ( 84.32823919854369876, 12.72937383798579880, -47.43652016892809797 ) ) ;
#3595 = DIRECTION ( 'NONE',  ( 0.000000000000000000, -8.635067969306036542E-13, -1.000000000000000000 ) ) ;
#3596 = CARTESIAN_POINT ( 'NONE',  ( 56.72051766553079943, 19.45439143119499903, -53.84018978621899976 ) ) ;
#3597 = ORIENTED_EDGE ( 'NONE', *, *, #6221, .F. ) ;
#3598 = DIRECTION ( 'NONE',  ( 0.000000000000000000, 0.000000000000000000, 1.000000000000000000 ) ) ;
#3599 = ORIENTED_EDGE ( 'NONE', *, *, #45140, .F. ) ;
#3600 = EDGE_CURVE ( 'NONE', #5111, #28199, #28726, .T. ) ;
#3601 = ORIENTED_EDGE ( 'NONE', *, *, #16653, .F. ) ;
#3602 = CARTESIAN_POINT ( 'NONE',  ( 61.13393739769620083, -33.11618894467940066, -84.38499399519520239 ) ) ;
#3603 = CARTESIAN_POINT ( 'NONE',  ( 11.27219059296783854, -9.290075776696600229, -39.08399250801967639 ) ) ;
#3604 = CIRCLE ( 'NONE', #29537, 18.50000000000000000 ) ;
#3605 = CARTESIAN_POINT ( 'NONE',  ( 76.42354666252261097, -22.55147712810201810, -12.89797355987789018 ) ) ;
#3606 = CARTESIAN_POINT ( 'NONE',  ( 9.496404720408110123, -64.31007826197829047, -46.84592557732370466 ) ) ;
#3607 = VECTOR ( 'NONE', #5631, 1000.000000000000114 ) ;
#3608 = EDGE_LOOP ( 'NONE', ( #47559, #47230, #1424, #49345 ) ) ;
#3609 = ORIENTED_EDGE ( 'NONE', *, *, #50771, .F. ) ;
#3610 = DIRECTION ( 'NONE',  ( 1.000000000000000000, 0.000000000000000000, 0.000000000000000000 ) ) ;
#3611 = CARTESIAN_POINT ( 'NONE',  ( -20.20258579638655050, -1.450742213106093859, -52.59143307560878355 ) ) ;
#3612 = DIRECTION ( 'NONE',  ( 0.000000000000000000, 0.000000000000000000, 1.000000000000000000 ) ) ;
#3613 = CARTESIAN_POINT ( 'NONE',  ( 16.65209534521472889, -8.850437320969684052, -45.97722336490771511 ) ) ;
#3614 = CARTESIAN_POINT ( 'NONE',  ( 59.15655000470670188, -2.504444135221610246, -15.68085838234140006 ) ) ;
#3615 = CARTESIAN_POINT ( 'NONE',  ( 51.73306673000479350, -49.00921834144799760, -77.03096706476540589 ) ) ;
#3616 = CARTESIAN_POINT ( 'NONE',  ( 15.05440318628160057, -53.11618894467930119, -76.14999999999999147 ) ) ;
#3617 = ORIENTED_EDGE ( 'NONE', *, *, #17482, .T. ) ;
#3618 = CARTESIAN_POINT ( 'NONE',  ( 63.22343968446809725, 0.9036513197889539661, -69.09785636402048681 ) ) ;
#3619 = CARTESIAN_POINT ( 'NONE',  ( 47.18324198357289845, -54.80726809202429450, -74.14999999999999147 ) ) ;
#3620 = DIRECTION ( 'NONE',  ( 0.000000000000000000, -1.000000000000000000, 0.000000000000000000 ) ) ;
#3621 = DIRECTION ( 'NONE',  ( 0.000000000000000000, 0.000000000000000000, -1.000000000000000000 ) ) ;
#3622 = CARTESIAN_POINT ( 'NONE',  ( 18.72609985679629929, -23.02344493979749629, -50.40534192571220018 ) ) ;
#3623 = EDGE_CURVE ( 'NONE', #42328, #18363, #40012, .T. ) ;
#3624 = CARTESIAN_POINT ( 'NONE',  ( 13.32596385126870153, -50.17279131214790056, -21.04426679283869817 ) ) ;
#3625 = EDGE_CURVE ( 'NONE', #12367, #46682, #11287, .T. ) ;
#3626 = CARTESIAN_POINT ( 'NONE',  ( 46.85765394103209758, -52.69486303297070151, -55.14905519569939685 ) ) ;
#3627 = CARTESIAN_POINT ( 'NONE',  ( 60.98011298575943329, -45.39072023738052764, -46.91885902351079807 ) ) ;
#3628 = CARTESIAN_POINT ( 'NONE',  ( 60.86406070507459987, -45.56987455658860142, -47.52785903502709886 ) ) ;
#3629 =( BOUNDED_CURVE ( )  B_SPLINE_CURVE ( 3, ( #15946, #27727, #51844, #31131 ),
 .UNSPECIFIED., .F., .T. ) 
 B_SPLINE_CURVE_WITH_KNOTS ( ( 4, 4 ),
 ( 4.675428907228452502, 4.913492185948230784 ),
 .UNSPECIFIED. ) 
 CURVE ( )  GEOMETRIC_REPRESENTATION_ITEM ( )  RATIONAL_B_SPLINE_CURVE ( ( 1.000000000000000000, 0.9952827299573674402, 0.9952827299573674402, 1.000000000000000000 ) ) 
 REPRESENTATION_ITEM ( '' )  );
#3630 = CARTESIAN_POINT ( 'NONE',  ( 15.24819415861908212, -22.38319558909093487, -38.99448831724205888 ) ) ;
#3631 = CARTESIAN_POINT ( 'NONE',  ( 9.141711747553159739, -14.69350826755799844, -55.88894205964179207 ) ) ;
#3632 = CARTESIAN_POINT ( 'NONE',  ( 10.22096416429083554, -12.20830314663815663, -43.61946976819260868 ) ) ;
#3633 = EDGE_LOOP ( 'NONE', ( #9251, #51181, #8497, #30528 ) ) ;
#3634 = CARTESIAN_POINT ( 'NONE',  ( 14.27557881312050014, -51.11618622139269519, -74.14993436883828792 ) ) ;
#3635 = CARTESIAN_POINT ( 'NONE',  ( 65.00323391584400667, 1.328073773609210084, -60.83220757462540007 ) ) ;
#3636 = CARTESIAN_POINT ( 'NONE',  ( 8.428878250350352985, -13.54536072994490326, -50.59100158115866464 ) ) ;
#3637 = AXIS2_PLACEMENT_3D ( 'NONE', #50198, #34179, #33670 ) ;
#3638 = CARTESIAN_POINT ( 'NONE',  ( 14.35459849512296238, -51.14555453227163184, -74.54430098194714560 ) ) ;
#3639 = CIRCLE ( 'NONE', #10337, 2.000000000000000000 ) ;
#3640 = CARTESIAN_POINT ( 'NONE',  ( 8.784728771152170879, -54.93525725209899235, -46.67204636145419983 ) ) ;
#3641 = CARTESIAN_POINT ( 'NONE',  ( 10.62399383826485710, -64.83240141107415866, -18.14936727198398358 ) ) ;
#3642 = CARTESIAN_POINT ( 'NONE',  ( 11.45636326042960107, 34.13238412238349895, -18.01147071074940342 ) ) ;
#3643 = CARTESIAN_POINT ( 'NONE',  ( 71.71886329086420631, 0.9254890127224479901, -70.46161719983020078 ) ) ;
#3645 = CARTESIAN_POINT ( 'NONE',  ( 45.28676693330019987, -37.97973142300439520, -63.87794661417289888 ) ) ;
#3644 = FACE_OUTER_BOUND ( 'NONE', #17708, .T. ) ;
#3646 = FACE_OUTER_BOUND ( 'NONE', #21924, .T. ) ;
#3647 = DIRECTION ( 'NONE',  ( 0.7071067811865475727, 0.000000000000000000, 0.7071067811865475727 ) ) ;
#3648 = PRODUCT_RELATED_PRODUCT_CATEGORY ( 'part', '', ( #46688 ) ) ;
#3649 = CARTESIAN_POINT ( 'NONE',  ( 49.71697407881379860, 22.41840834450090014, -55.07777775019549438 ) ) ;
#3650 = ORIENTED_EDGE ( 'NONE', *, *, #17260, .T. ) ;
#3651 = CARTESIAN_POINT ( 'NONE',  ( 53.50261634512969522, -49.38508019297159990, -49.11501020125410122 ) ) ;
#3652 = ORIENTED_EDGE ( 'NONE', *, *, #49696, .T. ) ;
#3653 = CARTESIAN_POINT ( 'NONE',  ( 46.06859774010791853, 7.964158654876348109, -60.46635192367470069 ) ) ;
#3654 = CARTESIAN_POINT ( 'NONE',  ( 53.63393739769619373, 30.88381105532059934, 11.84999999999999964 ) ) ;
#3655 = CARTESIAN_POINT ( 'NONE',  ( 16.13393739769620083, -15.61618894467929941, -19.08999999999999986 ) ) ;
#3656 = CARTESIAN_POINT ( 'NONE',  ( 16.13393739769599833, 14.38381105532070059, -62.64999999999999858 ) ) ;
#3657 = CARTESIAN_POINT ( 'NONE',  ( 20.38450248183900015, -21.24426633950000110, -52.74692207654109666 ) ) ;
#3658 = CARTESIAN_POINT ( 'NONE',  ( 53.51287195967390176, 18.19965013284789990, -49.22146522496750265 ) ) ;
#3659 = CARTESIAN_POINT ( 'NONE',  ( 55.59742021819219815, -45.60898701366559749, -16.21687166337950003 ) ) ;
#3660 = LINE ( 'NONE', #27995, #39032 ) ;
#3661 = AXIS2_PLACEMENT_3D ( 'NONE', #22445, #3533, #38452 ) ;
#3662 = ORIENTED_EDGE ( 'NONE', *, *, #28140, .F. ) ;
#3663 = EDGE_CURVE ( 'NONE', #5274, #7868, #44156, .T. ) ;
#3664 = CARTESIAN_POINT ( 'NONE',  ( 21.36084080367719906, -21.46992527011509821, -45.55549324029160374 ) ) ;
#3665 = ORIENTED_EDGE ( 'NONE', *, *, #28898, .T. ) ;
#3666 = EDGE_CURVE ( 'NONE', #45770, #10362, #18922, .T. ) ;
#3667 = CARTESIAN_POINT ( 'NONE',  ( 11.88973812647869899, -65.43508066229159681, -17.85918014674359711 ) ) ;
#3668 = CARTESIAN_POINT ( 'NONE',  ( 10.81618306470670099, 33.23750078974720168, -46.19159279582959954 ) ) ;
#3669 = CARTESIAN_POINT ( 'NONE',  ( 73.11834175676820280, 0.9272522097098119254, -62.30994913869029972 ) ) ;
#3670 = PLANE ( 'NONE',  #39408 ) ;
#3672 = EDGE_CURVE ( 'NONE', #33168, #36842, #26002, .T. ) ;
#3671 = CARTESIAN_POINT ( 'NONE',  ( 8.812209671510000675, 32.03058768159100111, -46.67110737466700243 ) ) ;
#3673 = DIRECTION ( 'NONE',  ( 0.6676418852213039656, 0.2329255526947077437, 0.7071067811865533459 ) ) ;
#3674 = EDGE_LOOP ( 'NONE', ( #48511, #3456, #31767, #43641, #39332, #12826 ) ) ;
#3675 = CARTESIAN_POINT ( 'NONE',  ( 64.70533732122689230, 1.100585178971990041, -70.52983742103261022 ) ) ;
#3676 = CARTESIAN_POINT ( 'NONE',  ( 11.13393739769619906, -63.41372582578870265, -43.92068416175130352 ) ) ;
#3677 = CARTESIAN_POINT ( 'NONE',  ( 13.39998208309999939, 20.55440457967890211, -74.14999999999999147 ) ) ;
#3678 = VERTEX_POINT ( 'NONE', #14482 ) ;
#3679 = CARTESIAN_POINT ( 'NONE',  ( 24.04145801234410129, -15.86957246127301424, -43.80251945200132724 ) ) ;
#3680 = CARTESIAN_POINT ( 'NONE',  ( 56.46340970881719556, 19.25363520061540257, -52.83593731267799143 ) ) ;
#3681 = FACE_OUTER_BOUND ( 'NONE', #18794, .T. ) ;
#3682 = ORIENTED_EDGE ( 'NONE', *, *, #13821, .T. ) ;
#3683 = AXIS2_PLACEMENT_3D ( 'NONE', #2595, #14641, #18569 ) ;
#3684 = CARTESIAN_POINT ( 'NONE',  ( 14.06320179395276071, -23.32127433849228382, -62.37566354910524069 ) ) ;
#3685 = CARTESIAN_POINT ( 'NONE',  ( 16.13393739769620083, -15.61618894467929941, -81.65000000000000568 ) ) ;
#3686 = CARTESIAN_POINT ( 'NONE',  ( 16.03039053705856887, -22.42402112133541792, -32.95781074573184100 ) ) ;
#3687 = CARTESIAN_POINT ( 'NONE',  ( 49.42285922342860260, 22.23360713278520251, -54.10983389954889589 ) ) ;
#3688 = CARTESIAN_POINT ( 'NONE',  ( 12.76833210023839982, -23.14316848747460043, -74.42617192852888763 ) ) ;
#3689 = CARTESIAN_POINT ( 'NONE',  ( 67.48834183618497207, -5.818188944679350882, -65.18094736867061556 ) ) ;
#3690 = PLANE ( 'NONE',  #47627 ) ;
#3691 = SHAPE_DEFINITION_REPRESENTATION ( #26116, #4683 ) ;
#3692 = ORIENTED_EDGE ( 'NONE', *, *, #45795, .T. ) ;
#3693 = ADVANCED_FACE ( 'NONE', ( #50131 ), #33866, .T. ) ;
#3694 = EDGE_LOOP ( 'NONE', ( #903, #5641, #2989, #46289 ) ) ;
#3695 = CARTESIAN_POINT ( 'NONE',  ( 22.16647721471450083, -11.24410052365730017, -62.03303090152439125 ) ) ;
#3696 = DIRECTION ( 'NONE',  ( 0.000000000000000000, 0.000000000000000000, 1.000000000000000000 ) ) ;
#3697 = CARTESIAN_POINT ( 'NONE',  ( 10.37974942112630039, -20.72019953162940098, -32.14999999999999858 ) ) ;
#3698 = VECTOR ( 'NONE', #48354, 1000.000000000000114 ) ;
#3699 = CARTESIAN_POINT ( 'NONE',  ( 46.35275103504439898, 21.67755452994670406, -76.14999999999999147 ) ) ;
#3700 = DIRECTION ( 'NONE',  ( 1.000000000000000000, 0.000000000000000000, 5.637851296924970156E-15 ) ) ;
#3701 = DIRECTION ( 'NONE',  ( -0.6911981449639432729, 0.7226652920947591596, 0.000000000000000000 ) ) ;
#3702 = ADVANCED_FACE ( 'NONE', ( #18154, #6367 ), #13720, .T. ) ;
#3703 = CARTESIAN_POINT ( 'NONE',  ( 19.38037798442189796, -23.19532769692779794, -75.87884994711779996 ) ) ;
#3704 = CARTESIAN_POINT ( 'NONE',  ( 52.58045726207989645, -49.84558690476340104, -28.06891840855830011 ) ) ;
#3705 = CARTESIAN_POINT ( 'NONE',  ( 56.13041345539360094, -50.64099428910919443, -75.55393924165630892 ) ) ;
#3707 = CARTESIAN_POINT ( 'NONE',  ( 10.57536502229777220, -55.22799900453085797, -45.48887427433546549 ) ) ;
#3706 = CARTESIAN_POINT ( 'NONE',  ( -11.32741173536820156, 10.64927170302630088, -6.269854646706059853 ) ) ;
#3708 = CIRCLE ( 'NONE', #18768, 0.9999999999568496278 ) ;
#3709 = CARTESIAN_POINT ( 'NONE',  ( 63.17514626975080461, 1.276058558775509999, -68.69062364193268877 ) ) ;
#3710 = CARTESIAN_POINT ( 'NONE',  ( 61.14456834629570636, 14.07465811252290067, -46.86919079265500443 ) ) ;
#3711 = DIRECTION ( 'NONE',  ( 0.5877852522924696954, 0.8090169943749498938, 0.000000000000000000 ) ) ;
#3712 = VERTEX_POINT ( 'NONE', #34120 ) ;
#3713 = CARTESIAN_POINT ( 'NONE',  ( 52.80356385740750369, -49.67514632639190353, -48.56463695142829806 ) ) ;
#3714 = CARTESIAN_POINT ( 'NONE',  ( 47.66693464750959919, 23.24250025773469730, -54.67859957007570415 ) ) ;
#3715 = CARTESIAN_POINT ( 'NONE',  ( 8.222787824498201559, -15.61638397318239946, -64.79233150823698395 ) ) ;
#3716 = DIRECTION ( 'NONE',  ( 0.000000000000000000, 0.000000000000000000, 1.000000000000000000 ) ) ;
#3717 = FACE_OUTER_BOUND ( 'NONE', #29745, .T. ) ;
#3718 = CARTESIAN_POINT ( 'NONE',  ( 18.08382399952279940, -22.80678252554330143, -72.64836766404950197 ) ) ;
#3719 = CARTESIAN_POINT ( 'NONE',  ( 51.78789577860580806, 18.59342600884450292, -76.67262230958300506 ) ) ;
#3720 = CARTESIAN_POINT ( 'NONE',  ( 53.00021627873709917, 18.34579924662379824, -48.89297487182130197 ) ) ;
#3721 = CARTESIAN_POINT ( 'NONE',  ( 8.428860607946825567, -17.68695301239758777, -70.70899843619372405 ) ) ;
#3722 = CARTESIAN_POINT ( 'NONE',  ( 53.39109823518269593, -49.36681769490010652, -48.76214596301609561 ) ) ;
#3723 = EDGE_LOOP ( 'NONE', ( #51692, #50268, #43375, #15101 ) ) ;
#3724 = EDGE_CURVE ( 'NONE', #51441, #12739, #28238, .T. ) ;
#3725 = CARTESIAN_POINT ( 'NONE',  ( 22.90078883224852291, -15.66462347074845596, -40.45510235809472732 ) ) ;
#3726 = EDGE_CURVE ( 'NONE', #50083, #10111, #5850, .T. ) ;
#3727 = CARTESIAN_POINT ( 'NONE',  ( 47.72346410858899901, -54.45426597620080145, -54.74160369805280624 ) ) ;
#3728 = DIRECTION ( 'NONE',  ( 0.2260571801428161165, -1.387778780781444597E-17, -0.9741140340359943917 ) ) ;
#3729 = DIRECTION ( 'NONE',  ( 0.000000000000000000, 0.7071067811865463515, -0.7071067811865487940 ) ) ;
#3730 = CARTESIAN_POINT ( 'NONE',  ( 59.81249386774219801, -29.83678189827580240, -15.94359662707469916 ) ) ;
#3732 = EDGE_CURVE ( 'NONE', #27321, #49113, #20650, .T. ) ;
#3731 = CARTESIAN_POINT ( 'NONE',  ( 71.19525238180870019, 1.198183261254780030, -60.61312937625270081 ) ) ;
#3733 = DIRECTION ( 'NONE',  ( 0.000000000000000000, 0.000000000000000000, -1.000000000000000000 ) ) ;
#3734 = CARTESIAN_POINT ( 'NONE',  ( 72.79984470539690733, 0.9644290104361010751, -61.87674839326469822 ) ) ;
#3735 = DIRECTION ( 'NONE',  ( 1.495533000000000082E-10, 6.370073999999999783E-11, -1.000000000000000000 ) ) ;
#3736 = EDGE_CURVE ( 'NONE', #40665, #23799, #1930, .T. ) ;
#3737 = DIRECTION ( 'NONE',  ( 0.000000000000000000, 0.000000000000000000, -1.000000000000000000 ) ) ;
#3738 = ORIENTED_EDGE ( 'NONE', *, *, #25277, .F. ) ;
#3739 = ORIENTED_EDGE ( 'NONE', *, *, #47152, .F. ) ;
#3740 = AXIS2_PLACEMENT_3D ( 'NONE', #18177, #33376, #21062 ) ;
#3741 = CARTESIAN_POINT ( 'NONE',  ( 24.04466642925503095, -15.61618863334376250, -55.79233649161735542 ) ) ;
#3742 = CARTESIAN_POINT ( 'NONE',  ( 50.82041483519691383, -31.10319463887767455, -16.62067175138126274 ) ) ;
#3743 = ORIENTED_EDGE ( 'NONE', *, *, #42316, .F. ) ;
#3744 = DIRECTION ( 'NONE',  ( 0.000000000000000000, 0.000000000000000000, -1.000000000000000000 ) ) ;
#3745 = CARTESIAN_POINT ( 'NONE',  ( 1.057008924472659928, -8.644787692947790703, -34.64999999999999858 ) ) ;
#3746 = B_SPLINE_CURVE_WITH_KNOTS ( 'NONE', 3,
 ( #44103, #28353, #16841, #43849, #16569, #27847, #7945, #44614, #36478, #4015, #12141, #13629, #31765, #20234, #16061, #11893, #36222, #39920, #47784, #8720 ),
 .UNSPECIFIED., .F., .F.,
 ( 4, 2, 2, 2, 2, 2, 2, 2, 2, 4 ),
 ( 0.000000000000000000, 0.08842031323028211320, 0.2261927319929608049, 0.3750000000000007216, 0.4999999999999988898, 0.5624999999999988898, 0.6624999999999994227, 0.7986771749361281092, 0.9352917551345886205, 1.000000000000000000 ),
 .UNSPECIFIED. ) ;
#3747 = ORIENTED_EDGE ( 'NONE', *, *, #35785, .F. ) ;
#3748 = LINE ( 'NONE', #19960, #24289 ) ;
#3749 = CARTESIAN_POINT ( 'NONE',  ( 43.72566957196067250, 6.648299627497703312, -71.69133740782910991 ) ) ;
#3750 = CARTESIAN_POINT ( 'NONE',  ( 8.222496981792570381, -15.61604333543320067, -34.50766849176299900 ) ) ;
#3751 = AXIS2_PLACEMENT_3D ( 'NONE', #46899, #19353, #35601 ) ;
#3752 = CARTESIAN_POINT ( 'NONE',  ( 11.33371065636610098, -8.912418118662481348, -39.09452867415449617 ) ) ;
#3753 = PLANE ( 'NONE',  #44725 ) ;
#3754 = VECTOR ( 'NONE', #30945, 1000.000000000000000 ) ;
#3755 = CARTESIAN_POINT ( 'NONE',  ( 20.57778927394911861, -22.22610635818881875, -50.10404926845265550 ) ) ;
#3756 = EDGE_CURVE ( 'NONE', #21139, #28005, #11909, .T. ) ;
#3757 = CARTESIAN_POINT ( 'NONE',  ( 65.32733128089900276, -30.99350611824779733, -16.78960899708049936 ) ) ;
#3758 = CARTESIAN_POINT ( 'NONE',  ( 14.52013050453804688, 20.37931109195778845, -75.46937998419714688 ) ) ;
#3759 = CARTESIAN_POINT ( 'NONE',  ( 15.27045073980099943, -23.41626191762090059, -76.54758917670669405 ) ) ;
#3760 = CARTESIAN_POINT ( 'NONE',  ( 55.54883708180769730, 14.75989776373999973, -16.75766202486890322 ) ) ;
#3761 = CARTESIAN_POINT ( 'NONE',  ( 40.85469175895860161, 14.12133229819039926, -5.792857911654750502 ) ) ;
#3762 = DIRECTION ( 'NONE',  ( 0.000000000000000000, 0.000000000000000000, 1.000000000000000000 ) ) ;
#3763 = CARTESIAN_POINT ( 'NONE',  ( 84.37646258656080533, -43.45890480302480796, -47.26568110888489826 ) ) ;
#3764 = DIRECTION ( 'NONE',  ( -0.7071067811865475727, 0.000000000000000000, 0.7071067811865475727 ) ) ;
#3765 = ADVANCED_FACE ( 'NONE', ( #19237 ), #11391, .F. ) ;
#3766 = B_SPLINE_CURVE_WITH_KNOTS ( 'NONE', 3,
 ( #47660, #3897, #35854, #7310, #3383, #35335, #11767, #25064, #36886, #36355, #28753, #987, #29017, #32934, #44495, #40559, #16194, #4140, #41080, #464, #5193, #24027, #211, #1249, #21146, #16985, #28231, #32404, #48960 ),
 .UNSPECIFIED., .F., .F.,
 ( 4, 2, 2, 2, 2, 2, 2, 2, 2, 2, 1, 1, 1, 1, 1, 2, 4 ),
 ( 0.000000000000000000, 0.06250045598305266348, 0.1250009119661053270, 0.1875013679491579766, 0.2500018239322106539, 0.3125022799152633035, 0.3750027358983159531, 0.4375031918813686582, 0.4687534198728949830, 0.4843785338686582564, 0.4921910908665399487, 0.4960973693654808225, 0.4980505086149513150, 0.4990270782396864502, 0.4995153630520540733, 0.4997595054582379404, 0.5000036478644217519 ),
 .UNSPECIFIED. ) ;
#3767 = CARTESIAN_POINT ( 'NONE',  ( 17.05134355889540032, -7.422222466570630672, -47.04315903996049286 ) ) ;
#3768 = ORIENTED_EDGE ( 'NONE', *, *, #20321, .F. ) ;
#3770 = EDGE_CURVE ( 'NONE', #17150, #38311, #35485, .T. ) ;
#3769 = LINE ( 'NONE', #23387, #35574 ) ;
#3771 = CIRCLE ( 'NONE', #38902, 2.000000000000002220 ) ;
#3772 = FACE_OUTER_BOUND ( 'NONE', #6181, .T. ) ;
#3773 = CARTESIAN_POINT ( 'NONE',  ( 50.48003419941433378, -36.11835380732057388, -76.20110286221279239 ) ) ;
#3774 = CARTESIAN_POINT ( 'NONE',  ( 61.65798985235609564, -45.21281149609252736, -46.99565652671198990 ) ) ;
#3775 = CARTESIAN_POINT ( 'NONE',  ( 13.50258242564699884, -50.13280577118869985, -20.96779971931389852 ) ) ;
#3776 = ORIENTED_EDGE ( 'NONE', *, *, #40349, .T. ) ;
#3777 = CARTESIAN_POINT ( 'NONE',  ( -5.178173089599670043, -47.26880399451710701, -5.229689596307480315 ) ) ;
#3778 = CARTESIAN_POINT ( 'NONE',  ( 47.18324198357279897, 23.57489020266570279, -54.61058319554400242 ) ) ;
#3779 = CARTESIAN_POINT ( 'NONE',  ( 63.24512423172760833, 1.266538207494809942, -62.46861950876320435 ) ) ;
#3780 = CARTESIAN_POINT ( 'NONE',  ( 57.55751162058999881, -50.37847131510899601, -52.97747665993289701 ) ) ;
#3781 = CARTESIAN_POINT ( 'NONE',  ( 43.17397272685330023, 12.05888459682840086, -4.721727401627280329 ) ) ;
#3782 = CARTESIAN_POINT ( 'NONE',  ( -18.32056709076247714, -20.94004174811257357, -50.69739520735551253 ) ) ;
#3783 = CARTESIAN_POINT ( 'NONE',  ( 64.36428085589631110, -45.11618894467940066, -12.32250341870529908 ) ) ;
#3784 = CARTESIAN_POINT ( 'NONE',  ( 58.28839273895309248, -46.80098789154040162, -47.64211241846629719 ) ) ;
#3785 = CARTESIAN_POINT ( 'NONE',  ( 20.11801398371856919, -8.703633029438034185, -75.45904336070280749 ) ) ;
#3786 = CARTESIAN_POINT ( 'NONE',  ( 11.97525993411146139, -21.02750440564567924, -63.16115020960447168 ) ) ;
#3787 = CARTESIAN_POINT ( 'NONE',  ( 17.27947697856539833, -52.93030938277399855, -76.14999999999999147 ) ) ;
#3788 = B_SPLINE_CURVE_WITH_KNOTS ( 'NONE', 3,
 ( #4598, #40767, #13008, #28963, #21097, #9335, #44962, #9064, #1455, #37100 ),
 .UNSPECIFIED., .F., .F.,
 ( 4, 2, 2, 2, 4 ),
 ( 0.000000000000000000, 0.1750000000135994438, 0.3750000000291418001, 0.5000000000388558075, 0.5540946774305016698 ),
 .UNSPECIFIED. ) ;
#3789 = EDGE_CURVE ( 'NONE', #23989, #16929, #20000, .T. ) ;
#3790 = CARTESIAN_POINT ( 'NONE',  ( 23.54258513496609950, -16.40272123479050137, -69.10100965672640427 ) ) ;
#3791 = CARTESIAN_POINT ( 'NONE',  ( 47.12245394960989842, 8.044248941898629823, -35.02700949942429531 ) ) ;
#3792 = CARTESIAN_POINT ( 'NONE',  ( 63.33916480286269746, 1.229734285826310058, -62.22610693502240053 ) ) ;
#3793 = ORIENTED_EDGE ( 'NONE', *, *, #10880, .T. ) ;
#3794 = CARTESIAN_POINT ( 'NONE',  ( -18.35638189584738456, -50.98649365362386021, 16.21999999999999886 ) ) ;
#3795 = CARTESIAN_POINT ( 'NONE',  ( 22.89700924243567570, -15.86553210016712256, -34.46454548921436611 ) ) ;
#3796 = CARTESIAN_POINT ( 'NONE',  ( 72.89060928222170332, 1.370937308141410238, -68.67294022748990301 ) ) ;
#3797 = DIRECTION ( 'NONE',  ( 0.000000000000000000, 0.000000000000000000, -1.000000000000000000 ) ) ;
#3798 = CARTESIAN_POINT ( 'NONE',  ( 10.07131628902749831, -11.23148262131390140, -81.23899999999999011 ) ) ;
#3799 = EDGE_CURVE ( 'NONE', #22659, #47961, #48145, .T. ) ;
#3800 = ORIENTED_EDGE ( 'NONE', *, *, #6521, .F. ) ;
#3801 = CARTESIAN_POINT ( 'NONE',  ( 17.37246673088850102, 21.53776777092619810, -76.12726769927830617 ) ) ;
#3802 = ORIENTED_EDGE ( 'NONE', *, *, #51070, .T. ) ;
#3803 = EDGE_LOOP ( 'NONE', ( #43124, #165, #44393, #40521 ) ) ;
#3804 = CARTESIAN_POINT ( 'NONE',  ( 57.11002074634209436, -45.86944388580869969, -26.25113386676060045 ) ) ;
#3805 = CARTESIAN_POINT ( 'NONE',  ( 23.51291121479609814, -16.19875826520710049, -81.23899999999999011 ) ) ;
#3806 = CARTESIAN_POINT ( 'NONE',  ( 61.66564617331420095, 13.97241000098359898, -46.96226704611760283 ) ) ;
#3807 = EDGE_LOOP ( 'NONE', ( #37932, #37044 ) ) ;
#3808 = CARTESIAN_POINT ( 'NONE',  ( 18.14187589073995710, -9.105712570752443114, -80.04820986649650649 ) ) ;
#3809 = EDGE_LOOP ( 'NONE', ( #48930, #11439, #41179, #33989 ) ) ;
#3810 = DIRECTION ( 'NONE',  ( 1.000000000000000000, 0.000000000000000000, 0.000000000000000000 ) ) ;
#3811 = CARTESIAN_POINT ( 'NONE',  ( 45.27455033981039634, -33.67802718498660397, -34.68571053370059332 ) ) ;
#3812 = EDGE_LOOP ( 'NONE', ( #44592, #44226, #6302, #17764 ) ) ;
#3813 = AXIS2_PLACEMENT_3D ( 'NONE', #15544, #31243, #23631 ) ;
#3814 = ORIENTED_EDGE ( 'NONE', *, *, #36862, .T. ) ;
#3815 = CARTESIAN_POINT ( 'NONE',  ( 44.30108064003440660, 1.883811055320657291, -51.43657703546407589 ) ) ;
#3816 = CARTESIAN_POINT ( 'NONE',  ( 10.85466640530910176, -64.96697012893029921, -17.55961383758990024 ) ) ;
#3817 = CARTESIAN_POINT ( 'NONE',  ( 60.44876012278479749, 14.56718382513089871, -47.68802017693349882 ) ) ;
#3818 = CARTESIAN_POINT ( 'NONE',  ( 9.366488261363459245, -15.61629045172390029, -39.45282021618999835 ) ) ;
#3819 = CARTESIAN_POINT ( 'NONE',  ( 40.40277276999439948, -44.85701247348080045, -4.354462746277440566 ) ) ;
#3820 = CARTESIAN_POINT ( 'NONE',  ( -6.168089167389290139, 15.43748276452459933, -5.539338566224690119 ) ) ;
#3821 = CARTESIAN_POINT ( 'NONE',  ( 47.17214967034067286, 23.54985037105774026, -74.50417146786301714 ) ) ;
#3822 = CARTESIAN_POINT ( 'NONE',  ( 15.57679709041789984, -22.64698931536659998, -43.37235095159000053 ) ) ;
#3823 = ADVANCED_FACE ( 'NONE', ( #4034 ), #19994, .T. ) ;
#3824 = CARTESIAN_POINT ( 'NONE',  ( 8.307315901316570717, -15.04108535784360079, -66.31085317895978903 ) ) ;
#3825 = ORIENTED_EDGE ( 'NONE', *, *, #39065, .T. ) ;
#3826 = ADVANCED_FACE ( 'NONE', ( #43103 ), #3525, .F. ) ;
#3827 = CARTESIAN_POINT ( 'NONE',  ( 41.08565836803850146, 14.27946363452990042, -6.051015727772759867 ) ) ;
#3828 = CARTESIAN_POINT ( 'NONE',  ( 72.31796842074359688, 1.033013263524880099, -69.95125361163759692 ) ) ;
#3829 = EDGE_CURVE ( 'NONE', #5028, #39996, #43349, .T. ) ;
#3830 = CARTESIAN_POINT ( 'NONE',  ( 42.26101777068934950, -39.79243905365653688, -75.07061934747760290 ) ) ;
#3831 = CARTESIAN_POINT ( 'NONE',  ( 14.14835400967140089, 19.11410306511140078, -20.86158003109679981 ) ) ;
#3832 = DIRECTION ( 'NONE',  ( 0.000000000000000000, -1.000000000000000000, 0.000000000000000000 ) ) ;
#3833 = AXIS2_PLACEMENT_3D ( 'NONE', #46056, #25837, #5191 ) ;
#3834 = CARTESIAN_POINT ( 'NONE',  ( 63.45453858566830974, 1.370853092582090094, -68.86908206983169123 ) ) ;
#3835 = CARTESIAN_POINT ( 'NONE',  ( 48.31420000707529994, -54.21845507221640048, -54.97975724495599792 ) ) ;
#3836 = AXIS2_PLACEMENT_3D ( 'NONE', #18832, #50819, #14910 ) ;
#3837 = CARTESIAN_POINT ( 'NONE',  ( 51.99322000344975692, -32.94168956680540106, -19.32981501234134569 ) ) ;
#3838 = DIRECTION ( 'NONE',  ( 0.000000000000000000, 0.000000000000000000, -1.000000000000000000 ) ) ;
#3839 = CARTESIAN_POINT ( 'NONE',  ( 11.27234542262131889, -21.94241925001478322, -38.21600269195644017 ) ) ;
#3840 = CARTESIAN_POINT ( 'NONE',  ( 23.04645466576749513, -11.63204637672123276, -71.62566002335191229 ) ) ;
#3841 = VERTEX_POINT ( 'NONE', #3003 ) ;
#3842 = CARTESIAN_POINT ( 'NONE',  ( 21.37438191210599925, -20.33663280004660123, -81.08056213787280342 ) ) ;
#3843 = CARTESIAN_POINT ( 'NONE',  ( 17.01970131259685459, -22.38319384293092895, -76.91116700029822084 ) ) ;
#3844 = ORIENTED_EDGE ( 'NONE', *, *, #28430, .F. ) ;
#3845 = FACE_OUTER_BOUND ( 'NONE', #4508, .T. ) ;
#3846 = CARTESIAN_POINT ( 'NONE',  ( 61.00611420029130727, -45.43078731296289874, -47.28201515225099882 ) ) ;
#3847 = LINE ( 'NONE', #31852, #11193 ) ;
#3848 = DIRECTION ( 'NONE',  ( 1.000000000000000000, 0.000000000000000000, 0.000000000000000000 ) ) ;
#3850 = CARTESIAN_POINT ( 'NONE',  ( 22.90077909847273219, -15.61618896438501203, -58.84717277627543552 ) ) ;
#3849 = CARTESIAN_POINT ( 'NONE',  ( 41.61087022781433831, 8.489620259922302736, -78.20791600774551000 ) ) ;
#3851 = CARTESIAN_POINT ( 'NONE',  ( 72.83393739769620367, 1.883811055320669947, -62.44999999999999574 ) ) ;
#3852 = DIRECTION ( 'NONE',  ( 0.000000000000000000, 1.000000000000000000, 0.000000000000000000 ) ) ;
#3853 = EDGE_CURVE ( 'NONE', #33352, #667, #18974, .T. ) ;
#3854 = ORIENTED_EDGE ( 'NONE', *, *, #28869, .F. ) ;
#3855 = CARTESIAN_POINT ( 'NONE',  ( 51.67587649748560352, 17.38381105532069881, -77.01363636363639387 ) ) ;
#3856 = EDGE_LOOP ( 'NONE', ( #24963, #23173, #26739, #46276 ) ) ;
#3857 = ORIENTED_EDGE ( 'NONE', *, *, #38749, .T. ) ;
#3858 = DIRECTION ( 'NONE',  ( 0.000000000000000000, 0.000000000000000000, -1.000000000000000000 ) ) ;
#3859 = CARTESIAN_POINT ( 'NONE',  ( 29.13393739769619728, -26.76363820448759867, -35.14999999999999858 ) ) ;
#3860 = CARTESIAN_POINT ( 'NONE',  ( 13.52272076457530048, -9.064539772954379515, -62.22645654473139842 ) ) ;
#3861 = CIRCLE ( 'NONE', #23906, 1.000000000000000888 ) ;
#3862 = ORIENTED_EDGE ( 'NONE', *, *, #14967, .T. ) ;
#3863 = ORIENTED_EDGE ( 'NONE', *, *, #2197, .T. ) ;
#3864 = CARTESIAN_POINT ( 'NONE',  ( 48.54525988008339255, 22.76209179570290075, -54.56845936111729856 ) ) ;
#3865 = VECTOR ( 'NONE', #26245, 1000.000000000000000 ) ;
#3866 = CARTESIAN_POINT ( 'NONE',  ( -22.10874326092599418, -7.786548904876307908, -54.22730359629444052 ) ) ;
#3867 = CARTESIAN_POINT ( 'NONE',  ( 56.48240963976540030, -50.76892851967889442, -53.80988698027800154 ) ) ;
#3868 = CARTESIAN_POINT ( 'NONE',  ( 13.73527022026340028, -50.20735447812900532, -20.93080062776369843 ) ) ;
#3869 = CARTESIAN_POINT ( 'NONE',  ( 59.99603231228150690, -1.358522701324750059, -15.95392620586269850 ) ) ;
#3870 = CARTESIAN_POINT ( 'NONE',  ( 51.97624292331419582, -50.01153706258679676, -76.70088690366090134 ) ) ;
#3871 = B_SPLINE_SURFACE_WITH_KNOTS ( 'NONE', 3, 3, ( 
 ( #42721, #47430, #51606, #31655, #15700, #23790, #2623, #6816, #4670, #4156, #28511, #40834, #48182, #4933, #16727, #20905 ),
 ( #40063, #36902, #1002, #48709, #48975, #12813, #28247, #13081, #20643, #20130, #44508, #17002, #12286, #32949, #32682, #29034 ),
 ( #36122, #45030, #9130, #28767, #39806, #44769, #44245, #8873, #8351, #3914, #24826, #19877, #35868, #51860, #8611, #24303 ),
 ( #226, #40319, #4415, #15961, #20381, #36629, #8099, #31914, #24042, #47936, #16209, #24560, #12037, #27990, #43993, #36370 ),
 ( #32167, #478, #16465, #32420, #731, #48443, #12544, #40573, #33728, #42132, #29544, #41867, #45547, #17757, #5971, #9642 ),
 ( #41097, #2293, #22187, #38197, #37674, #25083, #37940, #26121, #33474, #21418, #34234, #46336, #13328, #41605, #1520, #6231 ),
 ( #49492, #25852, #25598, #21928, #5710, #21667, #5464, #5208, #1776, #14344, #30047, #17505, #21161, #49233, #29288, #49741 ),
 ( #2034, #45809, #18014, #13831, #37419, #50257, #18266, #30314, #37167, #45289, #33980, #1264, #29788, #49995, #17252, #33216 ),
 ( #9398, #25347, #41347, #9896, #13579, #14086, #46073, #10160, #3331, #14861, #22708, #14603, #15386, #31339, #42392, #46593 ),
 ( #6752, #51025, #23472, #3593, #7524, #26907, #39495, #39233, #19566, #51288, #50772, #43170, #47365, #43424, #11463, #19046 ) ),
 .UNSPECIFIED., .F., .F., .F.,
 ( 4, 1, 1, 1, 1, 1, 1, 4 ),
 ( 4, 2, 2, 2, 2, 2, 2, 4 ),
 ( -1.469098915510469939E-05, 0.1428571428571430157, 0.2857142857142860315, 0.4285714285714289917, 0.5714285714285709528, 0.7142857142857139685, 0.8571428571428569843, 1.000011663802299999 ),
 ( -1.570796326794899889, -1.322743703599180032, -1.039254991375500037, -0.8620745462357000122, -0.7734843236657999999, -0.6317399675539610016, -0.4049489977750169722, -0.1533416749778110100 ),
 .UNSPECIFIED. ) ;
#3872 = CARTESIAN_POINT ( 'NONE',  ( 68.13393739769620083, -43.11618894467930119, -65.65000000000000568 ) ) ;
#3873 = ORIENTED_EDGE ( 'NONE', *, *, #43714, .F. ) ;
#3874 = CARTESIAN_POINT ( 'NONE',  ( 16.13393739769620083, -15.61618894467929941, -11.65000000000000036 ) ) ;
#3875 = CARTESIAN_POINT ( 'NONE',  ( 62.63393739769619373, -53.11618894467930119, 11.84999999999999964 ) ) ;
#3876 = CARTESIAN_POINT ( 'NONE',  ( 20.64167000759333348, -10.49200264909508995, -34.18273036881165439 ) ) ;
#3877 = DIRECTION ( 'NONE',  ( 1.000000000000000000, 0.000000000000000000, 0.000000000000000000 ) ) ;
#3878 = VECTOR ( 'NONE', #44820, 1000.000000000000000 ) ;
#3879 = CARTESIAN_POINT ( 'NONE',  ( 20.44785949262530167, -22.17186005833840312, -58.32723503207409976 ) ) ;
#3880 = AXIS2_PLACEMENT_3D ( 'NONE', #37818, #1911, #20771 ) ;
#3881 = CARTESIAN_POINT ( 'NONE',  ( 12.52592233819879830, -50.09802290064689601, -21.14436588474130119 ) ) ;
#3882 = CARTESIAN_POINT ( 'NONE',  ( 56.00869119085820103, 19.38893017032829746, -75.85262141779099920 ) ) ;
#3884 = B_SPLINE_CURVE_WITH_KNOTS ( 'NONE', 3,
 ( #23548, #48196, #3671, #15713, #15974, #51619, #27757, #32180, #35880, #240, #39820, #44260, #31669, #4169, #12301, #28260 ),
 .UNSPECIFIED., .F., .F.,
 ( 4, 2, 2, 2, 2, 2, 2, 4 ),
 ( 0.000000000000000000, 0.1775000000000006573, 0.3375000000000000222, 0.4374999999999991118, 0.4999999999999999445, 0.6249999999999994449, 0.8249999999999999556, 1.000000000000000000 ),
 .UNSPECIFIED. ) ;
#3883 = CARTESIAN_POINT ( 'NONE',  ( 42.76911844754650360, -36.11618894467930119, -61.17703620997009750 ) ) ;
#3885 = CARTESIAN_POINT ( 'NONE',  ( 68.13393739769649926, -48.11618894467630270, -70.54999999999999716 ) ) ;
#3886 = CARTESIAN_POINT ( 'NONE',  ( 60.89660960531970346, -45.43840501675690291, -47.10135066908280521 ) ) ;
#3887 = CARTESIAN_POINT ( 'NONE',  ( 22.90093739769620029, -15.61618894467913243, -28.45282021618999835 ) ) ;
#3888 = CARTESIAN_POINT ( 'NONE',  ( 21.43993832425640278, -20.26257607252319914, -49.07611398817049775 ) ) ;
#3889 = CARTESIAN_POINT ( 'NONE',  ( -0.02503409344753749696, -22.81475709047199985, -34.78823607925542660 ) ) ;
#3890 = ORIENTED_EDGE ( 'NONE', *, *, #14378, .F. ) ;
#3892 = EDGE_CURVE ( 'NONE', #18872, #38732, #21031, .T. ) ;
#3891 = DIRECTION ( 'NONE',  ( 0.000000000000000000, 0.000000000000000000, -1.000000000000000000 ) ) ;
#3893 = CARTESIAN_POINT ( 'NONE',  ( 47.24561095051279835, -54.75899299496529693, -54.64386179031699697 ) ) ;
#3894 = SURFACE_SIDE_STYLE ('',( #36351 ) ) ;
#3895 = CARTESIAN_POINT ( 'NONE',  ( 10.42914237396198196, 33.65646982228821571, -47.08729022406233611 ) ) ;
#3896 = CARTESIAN_POINT ( 'NONE',  ( 56.06467566929225654, -46.69807061730856645, -26.34903397246540635 ) ) ;
#3897 = CARTESIAN_POINT ( 'NONE',  ( 8.222915678894278102, -14.38730632297055045, -54.55712915330399682 ) ) ;
#3898 = CIRCLE ( 'NONE', #42436, 0.4999999999999962252 ) ;
#3899 = CARTESIAN_POINT ( 'NONE',  ( 10.61752692138360032, -64.82564047392860118, -18.17418372802830007 ) ) ;
#3900 = AXIS2_PLACEMENT_3D ( 'NONE', #12611, #29097, #28574 ) ;
#3901 = CARTESIAN_POINT ( 'NONE',  ( 9.410656861959711961, -11.36542763060938555, -64.68701949937872087 ) ) ;
#3902 = CARTESIAN_POINT ( 'NONE',  ( 43.46118252345650035, -37.78219224926380093, -73.01045585346660971 ) ) ;
#3903 = CARTESIAN_POINT ( 'NONE',  ( 16.13393739769620083, -15.61618894467929941, -69.65000000000000568 ) ) ;
#3904 = DIRECTION ( 'NONE',  ( 1.000000000000000000, 0.000000000000000000, 0.000000000000000000 ) ) ;
#3905 = CARTESIAN_POINT ( 'NONE',  ( 49.03027862569489770, 22.68258847135309964, -54.93684304997719892 ) ) ;
#3906 = EDGE_CURVE ( 'NONE', #50052, #1350, #37032, .T. ) ;
#3907 = EDGE_LOOP ( 'NONE', ( #21243, #50346, #15812, #6714, #11117 ) ) ;
#3908 = CARTESIAN_POINT ( 'NONE',  ( 52.85422459453599231, -49.67664456668449446, -48.94261454323000748 ) ) ;
#3909 = ORIENTED_EDGE ( 'NONE', *, *, #15800, .T. ) ;
#3910 = CARTESIAN_POINT ( 'NONE',  ( 43.53205667065411433, 7.709292839630085048, -73.05708749340493569 ) ) ;
#3911 = AXIS2_PLACEMENT_3D ( 'NONE', #4798, #13457, #29151 ) ;
#3912 = CARTESIAN_POINT ( 'NONE',  ( 68.13393739769620083, 17.38381105532069881, -83.65000000000000568 ) ) ;
#3913 = CARTESIAN_POINT ( 'NONE',  ( -18.86606260230390220, 19.38381105532060289, 14.21249999999999858 ) ) ;
#3914 = CARTESIAN_POINT ( 'NONE',  ( 83.54531734280119792, 13.40902645347810029, -46.66630366969080512 ) ) ;
#3915 = CARTESIAN_POINT ( 'NONE',  ( 22.98684880019740362, -17.28357132616680047, -50.52879200675969429 ) ) ;
#3916 = CARTESIAN_POINT ( 'NONE',  ( 52.60294686985729840, 18.59530815018699812, -48.60888033553569443 ) ) ;
#3917 = CARTESIAN_POINT ( 'NONE',  ( 56.20733314801729819, -45.19218008104289908, -15.77257108625240001 ) ) ;
#3918 = EDGE_CURVE ( 'NONE', #4949, #28243, #8141, .T. ) ;
#3919 = CARTESIAN_POINT ( 'NONE',  ( 52.82512926767439865, 18.35096675686769885, -27.26906326477459785 ) ) ;
#3920 = CIRCLE ( 'NONE', #10617, 33.00000000000000000 ) ;
#3921 = EDGE_LOOP ( 'NONE', ( #23053, #38154, #15338, #36303 ) ) ;
#3922 = CARTESIAN_POINT ( 'NONE',  ( 16.49996568077149917, -7.777007132833650083, -40.80235737647439720 ) ) ;
#3923 = EDGE_CURVE ( 'NONE', #41326, #5472, #17124, .T. ) ;
#3924 = VERTEX_POINT ( 'NONE', #36499 ) ;
#3925 = CARTESIAN_POINT ( 'NONE',  ( 11.81751875573920074, -65.31523040516019307, -17.14434872735650117 ) ) ;
#3926 = CARTESIAN_POINT ( 'NONE',  ( 12.12676297962169869, 34.11083646916790002, -47.13081205359050330 ) ) ;
#3927 = CARTESIAN_POINT ( 'NONE',  ( 73.11516444234040080, 0.9966178393190270324, -62.31828917185450223 ) ) ;
#3928 = DIRECTION ( 'NONE',  ( 0.000000000000000000, 0.000000000000000000, 1.000000000000000000 ) ) ;
#3929 = CARTESIAN_POINT ( 'NONE',  ( 11.38213983923405337, -65.24847911815764689, -22.77752646547867954 ) ) ;
#3930 = DIRECTION ( 'NONE',  ( 0.000000000000000000, 0.000000000000000000, 1.000000000000000000 ) ) ;
#3931 = ORIENTED_EDGE ( 'NONE', *, *, #43527, .T. ) ;
#3932 = CARTESIAN_POINT ( 'NONE',  ( 64.68494473060250982, 1.102139304147779830, -70.51608385812039614 ) ) ;
#3933 = CARTESIAN_POINT ( 'NONE',  ( 10.97882772194960133, -63.26469174528480721, -44.74230523385489988 ) ) ;
#3934 = CARTESIAN_POINT ( 'NONE',  ( 68.13393739769630031, 16.88381105532149817, -68.79999999999999716 ) ) ;
#3935 = ORIENTED_EDGE ( 'NONE', *, *, #17729, .F. ) ;
#3936 = CARTESIAN_POINT ( 'NONE',  ( 23.61468320491630024, -48.77463972988229557, -35.01184033120630090 ) ) ;
#3937 = CARTESIAN_POINT ( 'NONE',  ( 8.277338810346954290, -14.47788413087303638, -76.55341515652921203 ) ) ;
#3938 = CARTESIAN_POINT ( 'NONE',  ( 63.54731047306190561, 1.396834109478129804, -68.84999999999999432 ) ) ;
#3939 = CARTESIAN_POINT ( 'NONE',  ( 14.96646045001671865, -7.755344280765369191, -48.96083666094899201 ) ) ;
#3940 =( BOUNDED_CURVE ( )  B_SPLINE_CURVE ( 3, ( #17954, #7204, #40202, #47313 ),
 .UNSPECIFIED., .F., .T. ) 
 B_SPLINE_CURVE_WITH_KNOTS ( ( 4, 4 ),
 ( 1.485879941667409998, 1.496022784645234083 ),
 .UNSPECIFIED. ) 
 CURVE ( )  GEOMETRIC_REPRESENTATION_ITEM ( )  RATIONAL_B_SPLINE_CURVE ( ( 1.000000000000000000, 0.9999914269130683042, 0.9999914269130683042, 1.000000000000000000 ) ) 
 REPRESENTATION_ITEM ( '' )  );
#3941 = EDGE_LOOP ( 'NONE', ( #31296, #22311, #33123, #14822, #9849, #24848 ) ) ;
#3942 = DIRECTION ( 'NONE',  ( 1.000000000000000000, 0.000000000000000000, 0.000000000000000000 ) ) ;
#3943 = DIRECTION ( 'NONE',  ( 1.241897755690669394E-30, -1.000000000000000000, -8.684364315601310195E-16 ) ) ;
#3945 = DIRECTION ( 'NONE',  ( 1.000000000000000000, 0.000000000000000000, 0.000000000000000000 ) ) ;
#3944 = CIRCLE ( 'NONE', #5632, 1.999999999999998668 ) ;
#3946 = CARTESIAN_POINT ( 'NONE',  ( 2.452285341914063110, -25.68011462166456127, -34.81767276520687915 ) ) ;
#3947 = CARTESIAN_POINT ( 'NONE',  ( 16.77504506022210151, -7.395988155100910788, -73.31710689363809763 ) ) ;
#3948 = DIRECTION ( 'NONE',  ( 0.3918900565005459247, -0.9200120562340468044, 0.000000000000000000 ) ) ;
#3949 = CARTESIAN_POINT ( 'NONE',  ( 24.04493739769619864, -15.61618894467929941, -32.14999999999999858 ) ) ;
#3950 = ORIENTED_EDGE ( 'NONE', *, *, #13564, .F. ) ;
#3951 = CARTESIAN_POINT ( 'NONE',  ( 16.27864033302759950, -23.06506502538119818, -64.72647455768748159 ) ) ;
#3952 = CARTESIAN_POINT ( 'NONE',  ( 53.51347036073359931, -49.43255037905120730, -49.22285071034340120 ) ) ;
#3953 = VECTOR ( 'NONE', #2046, 1000.000000000000000 ) ;
#3954 = CARTESIAN_POINT ( 'NONE',  ( 11.87719327230648680, 10.74943050428830560, -34.64999999999999858 ) ) ;
#3955 = CARTESIAN_POINT ( 'NONE',  ( 10.35872898856410096, -20.69271781505580066, -32.14999999999999858 ) ) ;
#3957 = EDGE_CURVE ( 'NONE', #336, #32835, #38063, .T. ) ;
#3956 = CARTESIAN_POINT ( 'NONE',  ( 46.69150152944290255, 22.32070490622299985, -76.02679354016848379 ) ) ;
#3958 = CARTESIAN_POINT ( 'NONE',  ( 71.20900144662560649, 1.388715606738720076, -61.01996879627380110 ) ) ;
#3959 = DIRECTION ( 'NONE',  ( 0.000000000000000000, 0.000000000000000000, -1.000000000000000000 ) ) ;
#3960 = CARTESIAN_POINT ( 'NONE',  ( 11.73339007446990045, 33.77567933031070169, -16.50122832063929934 ) ) ;
#3961 = CARTESIAN_POINT ( 'NONE',  ( 24.02699963285100182, -17.99994423013719924, -71.60102766968249455 ) ) ;
#3962 = CARTESIAN_POINT ( 'NONE',  ( 55.71241392848639862, -50.61618636397409432, -76.18756357822059044 ) ) ;
#3963 = CARTESIAN_POINT ( 'NONE',  ( 21.54526424423086439, -11.45752564796633699, -60.24446586214138932 ) ) ;
#3964 = CARTESIAN_POINT ( 'NONE',  ( 63.46018632244250313, 1.384447124000270035, -68.59133994763901399 ) ) ;
#3965 = CARTESIAN_POINT ( 'NONE',  ( 61.43594907124419535, 13.96124516595140008, -46.78941255914340047 ) ) ;
#3966 = DIRECTION ( 'NONE',  ( 0.000000000000000000, -0.7071067811865582309, 0.7071067811865366926 ) ) ;
#3967 = ORIENTED_EDGE ( 'NONE', *, *, #18742, .F. ) ;
#3968 = CARTESIAN_POINT ( 'NONE',  ( 53.02240710655750178, -49.55998530720779627, -48.78672999826219581 ) ) ;
#3969 = FACE_OUTER_BOUND ( 'NONE', #16953, .T. ) ;
#3970 = DIRECTION ( 'NONE',  ( 1.000000000000000000, 0.000000000000000000, 0.000000000000000000 ) ) ;
#3971 = CARTESIAN_POINT ( 'NONE',  ( 61.44924444735519842, 14.16613670727899965, -47.39916440910469930 ) ) ;
#3972 = CARTESIAN_POINT ( 'NONE',  ( 8.687503549248530632, -15.85559810456780028, -71.22242690490419648 ) ) ;
#3973 = CARTESIAN_POINT ( 'NONE',  ( 51.64973234263280233, 18.01818895620939998, -76.82386384811070457 ) ) ;
#3974 = CARTESIAN_POINT ( 'NONE',  ( 53.42701933212400434, 18.14767980575969730, -49.00234330185679710 ) ) ;
#3975 = CARTESIAN_POINT ( 'NONE',  ( 14.13393739769630031, 1.391621760993509982, -35.14999999999999858 ) ) ;
#3976 = CARTESIAN_POINT ( 'NONE',  ( 75.13393739769618662, 1.883811055320649963, -84.38499399519520239 ) ) ;
#3977 = B_SPLINE_CURVE_WITH_KNOTS ( 'NONE', 3,
 ( #25139, #5255, #21209, #41925 ),
 .UNSPECIFIED., .F., .F.,
 ( 4, 4 ),
 ( 0.000000000000000000, 1.000000000000000000 ),
 .UNSPECIFIED. ) ;
#3978 = VERTEX_POINT ( 'NONE', #869 ) ;
#3979 = CARTESIAN_POINT ( 'NONE',  ( 53.35699421374690132, 18.69401400300939642, -74.14999999999999147 ) ) ;
#3980 = ADVANCED_FACE ( 'NONE', ( #13462 ), #45021, .T. ) ;
#3981 = CARTESIAN_POINT ( 'NONE',  ( 47.67996957097940225, -54.51610847055570019, -55.06157314954699444 ) ) ;
#3982 = CARTESIAN_POINT ( 'NONE',  ( -10.89822638428740120, 11.09799366572489987, -6.199143116732470205 ) ) ;
#3983 = DIRECTION ( 'NONE',  ( 0.000000000000000000, 0.000000000000000000, 1.000000000000000000 ) ) ;
#3984 = CARTESIAN_POINT ( 'NONE',  ( 62.76787785535929487, -30.70400768739660080, -16.43756860717520141 ) ) ;
#3985 = CARTESIAN_POINT ( 'NONE',  ( 71.52074786344320501, 0.8966068345641440285, -60.69721413447479819 ) ) ;
#3986 = DIRECTION ( 'NONE',  ( 0.000000000000000000, 1.000000000000000000, 0.000000000000000000 ) ) ;
#3987 = CARTESIAN_POINT ( 'NONE',  ( 72.15626456945139466, 1.443019669817199979, -61.49113342732780296 ) ) ;
#3988 = AXIS2_PLACEMENT_3D ( 'NONE', #24676, #44110, #12396 ) ;
#3989 = CARTESIAN_POINT ( 'NONE',  ( 10.13393739769589885, 22.91950879131600161, -54.64999999999999858 ) ) ;
#3990 = DIRECTION ( 'NONE',  ( 1.000000000000000000, 0.000000000000000000, 0.000000000000000000 ) ) ;
#3991 = ORIENTED_EDGE ( 'NONE', *, *, #50405, .T. ) ;
#3992 = ORIENTED_EDGE ( 'NONE', *, *, #14794, .F. ) ;
#3993 = CARTESIAN_POINT ( 'NONE',  ( 57.36123081079020380, 18.90300135422739913, -52.61896059691729732 ) ) ;
#3994 = FACE_OUTER_BOUND ( 'NONE', #38869, .T. ) ;
#3995 = EDGE_LOOP ( 'NONE', ( #51630, #38929, #49640, #34889, #16898, #16657 ) ) ;
#3996 = CARTESIAN_POINT ( 'NONE',  ( 68.13393739769620083, 1.383811055320669947, -65.65000000000000568 ) ) ;
#3997 = CARTESIAN_POINT ( 'NONE',  ( 55.41808927438875543, 19.74831332310506227, -75.07139216123769643 ) ) ;
#3998 = ORIENTED_EDGE ( 'NONE', *, *, #51342, .F. ) ;
#3999 = CARTESIAN_POINT ( 'NONE',  ( 11.44965733209057390, 34.05957685831252491, -22.70627853750865199 ) ) ;
#4000 = CARTESIAN_POINT ( 'NONE',  ( 17.63393739769629676, 0.9255523191756780399, -34.64999999999999858 ) ) ;
#4001 = CARTESIAN_POINT ( 'NONE',  ( 61.22588934636690539, 14.38309530880740006, -47.69104795661070284 ) ) ;
#4002 = CARTESIAN_POINT ( 'NONE',  ( 8.715470921945700056, -12.01770659734159885, -38.93609081202730238 ) ) ;
#4003 = CARTESIAN_POINT ( 'NONE',  ( 8.222941217535151281, -16.65176438257585900, -68.46600170818715014 ) ) ;
#4004 = FACE_OUTER_BOUND ( 'NONE', #32311, .T. ) ;
#4005 = DIRECTION ( 'NONE',  ( 0.000000000000000000, 0.000000000000000000, 1.000000000000000000 ) ) ;
#4006 = CARTESIAN_POINT ( 'NONE',  ( 59.22256780989010139, -28.32779697543540109, -15.66491663685500058 ) ) ;
#4007 = CARTESIAN_POINT ( 'NONE',  ( 14.06334520972920288, -23.32131147013534189, -42.37566460173350436 ) ) ;
#4008 = CARTESIAN_POINT ( 'NONE',  ( 8.705489043054660314, -15.04623381650379876, -35.25703220202099430 ) ) ;
#4009 = CARTESIAN_POINT ( 'NONE',  ( 41.33277327098829801, 14.31091597718369890, -6.226138135101860094 ) ) ;
#4010 = EDGE_CURVE ( 'NONE', #19315, #47534, #12437, .T. ) ;
#4011 = CARTESIAN_POINT ( 'NONE',  ( -11.07640030671909948, 8.018182000708311108, -19.14999999999999858 ) ) ;
#4012 = EDGE_CURVE ( 'NONE', #33090, #11777, #1589, .T. ) ;
#4013 = CARTESIAN_POINT ( 'NONE',  ( 83.71674455129429759, -44.49277106579119589, -46.72760658838089398 ) ) ;
#4014 = AXIS2_PLACEMENT_3D ( 'NONE', #1830, #41658, #33529 ) ;
#4015 = CARTESIAN_POINT ( 'NONE',  ( 64.09336526242300636, 1.458407755040209919, -69.75916877191829713 ) ) ;
#4016 = ADVANCED_FACE ( 'NONE', ( #17378 ), #603, .T. ) ;
#4017 = CARTESIAN_POINT ( 'NONE',  ( 17.02638215719250070, -23.81291164709050179, -41.97314745188879215 ) ) ;
#4018 = EDGE_LOOP ( 'NONE', ( #1208, #17337, #50078, #12723 ) ) ;
#4019 = CARTESIAN_POINT ( 'NONE',  ( 54.55982533688380443, -47.81947338028329852, -26.42778140218189975 ) ) ;
#4020 = CARTESIAN_POINT ( 'NONE',  ( 10.88038546904039983, -65.03853012327121519, -17.65323373620159941 ) ) ;
#4021 = CARTESIAN_POINT ( 'NONE',  ( 24.01727330109450165, -16.33183074238797872, -39.53649162746054913 ) ) ;
#4022 = AXIS2_PLACEMENT_3D ( 'NONE', #32356, #10745, #39489 ) ;
#4023 = CARTESIAN_POINT ( 'NONE',  ( 22.90070561427262064, -15.61618657793558818, -56.45282510079097449 ) ) ;
#4024 = APPLICATION_CONTEXT ( 'automotive_design' ) ;
#4025 = CARTESIAN_POINT ( 'NONE',  ( 61.75019796695539753, -46.11618894467930119, -37.26101630944549470 ) ) ;
#4026 = ORIENTED_EDGE ( 'NONE', *, *, #28835, .F. ) ;
#4027 = CARTESIAN_POINT ( 'NONE',  ( -6.917791992670210277, -46.04619488212870237, -5.579573692652759931 ) ) ;
#4028 = CARTESIAN_POINT ( 'NONE',  ( -0.02503409344748377258, -4.155984009993316519, -34.78823607925539108 ) ) ;
#4029 = DIRECTION ( 'NONE',  ( 1.000000000000000000, 0.000000000000000000, 0.000000000000000000 ) ) ;
#4030 = CARTESIAN_POINT ( 'NONE',  ( 63.05799534064709633, 1.101170701158060039, -62.53612607382319766 ) ) ;
#4031 = CARTESIAN_POINT ( 'NONE',  ( 57.55751162057470083, -50.45075475114750674, -53.12582022100689727 ) ) ;
#4032 = CARTESIAN_POINT ( 'NONE',  ( 41.87064654090709581, 13.25620980835100049, -5.149960901716640116 ) ) ;
#4033 = DIRECTION ( 'NONE',  ( -1.000000000000000000, -1.040834085586084257E-16, 0.000000000000000000 ) ) ;
#4034 = FACE_OUTER_BOUND ( 'NONE', #42148, .T. ) ;
#4035 = LINE ( 'NONE', #11646, #36771 ) ;
#4036 = CARTESIAN_POINT ( 'NONE',  ( 68.13393739769847457, -50.70395984888145335, -72.15645085170113759 ) ) ;
#4037 = CARTESIAN_POINT ( 'NONE',  ( 9.367501421782780113, -15.61622054991689978, -37.45282021618999835 ) ) ;
#4038 = CARTESIAN_POINT ( 'NONE',  ( 17.21347160910390173, -53.11618894467930119, -76.14999999999999147 ) ) ;
#4039 = ADVANCED_FACE ( 'NONE', ( #16588 ), #5746, .T. ) ;
#4040 = CARTESIAN_POINT ( 'NONE',  ( -6.866062602303790285, -15.61618894467929941, -84.65000000000000568 ) ) ;
#4041 = CARTESIAN_POINT ( 'NONE',  ( 24.04523903120960782, -15.61618918343368101, -41.50766953063602926 ) ) ;
#4042 = EDGE_LOOP ( 'NONE', ( #42727, #4940, #2959, #32771 ) ) ;
#4043 = CARTESIAN_POINT ( 'NONE',  ( 8.812209671510000675, 32.03058768159100111, -46.67110737466700243 ) ) ;
#4044 = CARTESIAN_POINT ( 'NONE',  ( 61.31807987947320271, 14.40950277385760003, -47.72348187476750070 ) ) ;
#4045 = CARTESIAN_POINT ( 'NONE',  ( 10.05451364342030018, -11.25897035538629964, -81.23899999999999011 ) ) ;
#4046 = EDGE_LOOP ( 'NONE', ( #26630, #19959, #21704 ) ) ;
#4047 = CARTESIAN_POINT ( 'NONE',  ( 17.29296856898550061, 21.71079195693500097, -76.14999999999999147 ) ) ;
#4048 = ORIENTED_EDGE ( 'NONE', *, *, #4107, .F. ) ;
#4049 = ORIENTED_EDGE ( 'NONE', *, *, #799, .F. ) ;
#4050 = CARTESIAN_POINT ( 'NONE',  ( 68.13393739769618662, -15.41618894467939782, -65.65000000000000568 ) ) ;
#4051 = CARTESIAN_POINT ( 'NONE',  ( 22.65381097660240428, -11.40563906863610022, -81.23899999999999011 ) ) ;
#4052 = CARTESIAN_POINT ( 'NONE',  ( -22.39277411605872459, 14.52970908907091996, 10.84999999999999964 ) ) ;
#4053 = AXIS2_PLACEMENT_3D ( 'NONE', #21380, #5423, #32911 ) ;
#4054 = ADVANCED_FACE ( 'NONE', ( #32541 ), #24167, .F. ) ;
#4055 = EDGE_LOOP ( 'NONE', ( #48221, #8044, #14685, #18845 ) ) ;
#4056 = EDGE_LOOP ( 'NONE', ( #43631, #23206, #8346, #7539 ) ) ;
#4057 = FACE_OUTER_BOUND ( 'NONE', #46291, .T. ) ;
#4058 = DIRECTION ( 'NONE',  ( 0.000000000000000000, 0.000000000000000000, -1.000000000000000000 ) ) ;
#4059 = VERTEX_POINT ( 'NONE', #40442 ) ;
#4060 = EDGE_LOOP ( 'NONE', ( #950, #1933, #44000, #39317 ) ) ;
#4061 = CARTESIAN_POINT ( 'NONE',  ( 44.66749666976073740, 1.931639890059055675, -44.69767322463768267 ) ) ;
#4062 = CARTESIAN_POINT ( 'NONE',  ( 11.35626934712506220, -65.29495918738072646, -17.73521848461691874 ) ) ;
#4063 = CARTESIAN_POINT ( 'NONE',  ( 60.36512744982970702, 14.56893724137899859, -47.62198983653560447 ) ) ;
#4064 = CARTESIAN_POINT ( 'NONE',  ( 9.581787940992585462, -13.67368164010640186, -39.54428995716352802 ) ) ;
#4065 = CARTESIAN_POINT ( 'NONE',  ( 40.68015302493939345, -44.62521549934429999, -4.085853159663479950 ) ) ;
#4066 = B_SPLINE_CURVE_WITH_KNOTS ( 'NONE', 3,
 ( #13968, #7906, #3468, #51421, #27041, #14992, #48, #11331, #16025, #23094, #47493, #11853, #38857, #12100 ),
 .UNSPECIFIED., .F., .F.,
 ( 4, 2, 2, 2, 2, 2, 4 ),
 ( 0.000000000000000000, 0.2500000000000620615, 0.3750000000001004197, 0.4375000000001131872, 0.4687500000001195155, 0.5000000000001258993, 1.000000000000000000 ),
 .UNSPECIFIED. ) ;
#4067 = CARTESIAN_POINT ( 'NONE',  ( -6.423975383169469922, 14.97160766071710114, -4.833031552625280725 ) ) ;
#4068 = B_SPLINE_CURVE_WITH_KNOTS ( 'NONE', 3,
 ( #7040, #35319, #6261, #14377, #39012, #30082, #30343, #34795, #26665, #50542, #10971, #14889, #38228, #2586, #46366, #42686 ),
 .UNSPECIFIED., .F., .F.,
 ( 4, 2, 2, 2, 2, 2, 2, 4 ),
 ( 0.000000000000000000, 2.041349754395100025, 4.374320902275219858, 5.832427869700300249, 6.561481353412840001, 7.727966927352889925, 9.594343845656990055, 11.66485573940060050 ),
 .UNSPECIFIED. ) ;
#4069 = CARTESIAN_POINT ( 'NONE',  ( 46.46257399784555986, 21.93137732320808553, -76.13734531346138112 ) ) ;
#4070 = DIRECTION ( 'NONE',  ( 0.000000000000000000, 0.000000000000000000, -1.000000000000000000 ) ) ;
#4071 = EDGE_CURVE ( 'NONE', #18887, #27054, #50936, .T. ) ;
#4072 = CARTESIAN_POINT ( 'NONE',  ( 20.92727658674290225, -21.82993560848299808, -67.57835607597769467 ) ) ;
#4073 = VERTEX_POINT ( 'NONE', #29921 ) ;
#4074 = CARTESIAN_POINT ( 'NONE',  ( 22.80253552484781210, -13.86357800176847199, -76.76474318907416716 ) ) ;
#4075 = CARTESIAN_POINT ( 'NONE',  ( 11.92002530253619952, 33.88340405295690516, -45.75731838001080121 ) ) ;
#4076 = CARTESIAN_POINT ( 'NONE',  ( 72.50011317461130034, 1.195685806282509978, -69.72628720609149866 ) ) ;
#4077 = CARTESIAN_POINT ( 'NONE',  ( 42.94455545980090250, -39.86079545475082142, -71.76762032940678182 ) ) ;
#4078 = FACE_OUTER_BOUND ( 'NONE', #44012, .T. ) ;
#4079 = AXIS2_PLACEMENT_3D ( 'NONE', #16959, #8831, #28469 ) ;
#4080 = CARTESIAN_POINT ( 'NONE',  ( 47.02944413358449793, 23.17759013347800234, -75.36156511192869800 ) ) ;
#4081 = CARTESIAN_POINT ( 'NONE',  ( 48.70705169239410282, -54.01489688557619218, -54.80929227398259940 ) ) ;
#4082 = DIRECTION ( 'NONE',  ( 1.000000000000000000, 0.000000000000000000, 0.000000000000000000 ) ) ;
#4083 = CARTESIAN_POINT ( 'NONE',  ( 16.13393739769620083, -15.61618894467929941, -48.64999999999999858 ) ) ;
#4084 = CARTESIAN_POINT ( 'NONE',  ( 14.06330850377756292, -23.32130196735118588, -54.37566615248211122 ) ) ;
#4085 = ORIENTED_EDGE ( 'NONE', *, *, #36354, .T. ) ;
#4086 = CARTESIAN_POINT ( 'NONE',  ( 18.76418403170740135, -22.58673428566360286, -33.45249067809769628 ) ) ;
#4087 = CARTESIAN_POINT ( 'NONE',  ( 10.22099316920907697, -19.02412432503898287, -77.28616187159222761 ) ) ;
#4088 = EDGE_LOOP ( 'NONE', ( #3909, #18481, #33156, #2442 ) ) ;
#4089 = CARTESIAN_POINT ( 'NONE',  ( 71.44880243016270072, 1.326666718054990035, -70.38086014838010840 ) ) ;
#4090 = CARTESIAN_POINT ( 'NONE',  ( 60.33724287810149889, -45.72939421683570060, -47.29483955813599749 ) ) ;
#4091 = CARTESIAN_POINT ( 'NONE',  ( 55.04426526048000312, -48.50067717176560222, -48.28429872967510050 ) ) ;
#4092 = CYLINDRICAL_SURFACE ( 'NONE', #31109, 0.5000000000000014433 ) ;
#4093 = CARTESIAN_POINT ( 'NONE',  ( 41.55703060469905097, 8.483152042567137840, -78.46913939333057897 ) ) ;
#4094 = DIRECTION ( 'NONE',  ( 0.000000000000000000, 1.000000000000000000, 0.000000000000000000 ) ) ;
#4095 = CARTESIAN_POINT ( 'NONE',  ( 9.807855859684124766, -10.75440353299834584, -66.71600124055041192 ) ) ;
#4096 = ORIENTED_EDGE ( 'NONE', *, *, #22619, .T. ) ;
#4097 = CYLINDRICAL_SURFACE ( 'NONE', #8912, 1.000000000000000888 ) ;
#4098 = EDGE_LOOP ( 'NONE', ( #30063, #38795, #31362, #19912, #6388, #948, #13536 ) ) ;
#4099 = ORIENTED_EDGE ( 'NONE', *, *, #44191, .T. ) ;
#4100 = DIRECTION ( 'NONE',  ( 0.000000000000000000, 0.000000000000000000, -1.000000000000000000 ) ) ;
#4101 = CARTESIAN_POINT ( 'NONE',  ( 53.27448929283489321, -49.51683810077160075, -49.18721518522060165 ) ) ;
#4102 = CARTESIAN_POINT ( 'NONE',  ( 23.83903634813313843, -13.54550697675067283, -79.70900030893358235 ) ) ;
#4103 = CARTESIAN_POINT ( 'NONE',  ( 76.39889423561334070, -19.26091417457611854, -12.79178202693621813 ) ) ;
#4104 = CARTESIAN_POINT ( 'NONE',  ( 49.85166797725670307, -53.37057052038269944, -54.14856546049170305 ) ) ;
#4105 = AXIS2_PLACEMENT_3D ( 'NONE', #36156, #49009, #24337 ) ;
#4106 = ORIENTED_EDGE ( 'NONE', *, *, #268, .F. ) ;
#4107 = EDGE_CURVE ( 'NONE', #46028, #38136, #30447, .T. ) ;
#4108 = ORIENTED_EDGE ( 'NONE', *, *, #47218, .F. ) ;
#4109 = CARTESIAN_POINT ( 'NONE',  ( 47.94837612362730539, 23.09355010960259946, -54.72220175608870107 ) ) ;
#4110 = DIRECTION ( 'NONE',  ( 1.000000000000000000, 0.000000000000000000, 0.000000000000000000 ) ) ;
#4111 = ADVANCED_FACE ( 'NONE', ( #50124 ), #49621, .T. ) ;
#4112 = CARTESIAN_POINT ( 'NONE',  ( 56.41630124387939560, -50.57626175706130311, -52.96295731896090331 ) ) ;
#4113 = CARTESIAN_POINT ( 'NONE',  ( 21.54530141090581452, -11.45757666743581638, -36.24448471271439587 ) ) ;
#4114 = CARTESIAN_POINT ( 'NONE',  ( 64.53955642881849997, 0.8952382593903849273, -17.65707518710819812 ) ) ;
#4115 = CARTESIAN_POINT ( 'NONE',  ( 52.08784388273989663, -49.61362219112419325, -77.13961893560180272 ) ) ;
#4116 = EDGE_CURVE ( 'NONE', #48985, #14240, #25473, .T. ) ;
#4117 = TOROIDAL_SURFACE ( 'NONE', #22626, 7.050000000000200551, 2.999999999999960032 ) ;
#4118 = ORIENTED_EDGE ( 'NONE', *, *, #33456, .F. ) ;
#4119 = FACE_OUTER_BOUND ( 'NONE', #30254, .T. ) ;
#4120 = CARTESIAN_POINT ( 'NONE',  ( 53.36305439838449871, -50.55087041970300277, -76.89765195167041156 ) ) ;
#4121 = CARTESIAN_POINT ( 'NONE',  ( 60.28868092514782973, 14.57684442129954761, -47.55394404419391918 ) ) ;
#4122 = CIRCLE ( 'NONE', #745, 1.999999999999998224 ) ;
#4123 = CARTESIAN_POINT ( 'NONE',  ( 2.277530937145189949, -15.61618894467929941, -24.14999999999999858 ) ) ;
#4124 = CIRCLE ( 'NONE', #9960, 0.5000000000000004441 ) ;
#4125 = CARTESIAN_POINT ( 'NONE',  ( 23.83408638490000087, -14.10144369664360120, -55.95066710016559597 ) ) ;
#4126 = CARTESIAN_POINT ( 'NONE',  ( 13.23341202568920139, -50.15389934968320063, -21.05834214923379832 ) ) ;
#4127 = CARTESIAN_POINT ( 'NONE',  ( 16.13393739769620083, -15.61618894467929941, -5.690000000000000391 ) ) ;
#4128 = CARTESIAN_POINT ( 'NONE',  ( 66.23540447448814916, -49.95860450174190248, -75.14853292321149070 ) ) ;
#4129 = CARTESIAN_POINT ( 'NONE',  ( 60.80455843160299878, -45.48718825086960038, -47.16343365292970446 ) ) ;
#4130 = DIRECTION ( 'NONE',  ( -0.6377178376947741922, -0.7702700562049011879, 0.000000000000000000 ) ) ;
#4131 = CARTESIAN_POINT ( 'NONE',  ( 11.55539561595339926, -20.98084311128560131, -55.57206633538729790 ) ) ;
#4132 = CARTESIAN_POINT ( 'NONE',  ( 97.41201884798559263, -30.66618894467940137, -65.65000000000000568 ) ) ;
#4133 = EDGE_CURVE ( 'NONE', #27748, #44502, #4915, .T. ) ;
#4134 = ORIENTED_EDGE ( 'NONE', *, *, #38233, .F. ) ;
#4135 = CARTESIAN_POINT ( 'NONE',  ( 11.27206271272561011, -65.28199317941199809, -18.17421237899035447 ) ) ;
#4136 = CARTESIAN_POINT ( 'NONE',  ( 47.32580105348969823, -54.70279562150209784, -54.71536561081010319 ) ) ;
#4137 = CYLINDRICAL_SURFACE ( 'NONE', #14898, 20.00000000000000000 ) ;
#4138 = CARTESIAN_POINT ( 'NONE',  ( 0.1754120801744591396, 19.58041923384463345, -34.67138862792307918 ) ) ;
#4139 = DIRECTION ( 'NONE',  ( 0.000000000000000000, 0.000000000000000000, 1.000000000000000000 ) ) ;
#4140 = CARTESIAN_POINT ( 'NONE',  ( 23.97633652620590183, -14.55430446190974969, -55.46484585604141415 ) ) ;
#4141 = CARTESIAN_POINT ( 'NONE',  ( 22.04683749721616692, -12.20817609659607328, -76.28613765794165147 ) ) ;
#4142 = CARTESIAN_POINT ( 'NONE',  ( 10.64977475916229999, 33.62388472332079914, -18.05902683574160150 ) ) ;
#4144 = CARTESIAN_POINT ( 'NONE',  ( 13.32898877073008848, -51.15116428088592926, -21.92090656186747211 ) ) ;
#4143 = CARTESIAN_POINT ( 'NONE',  ( 18.71043739769620018, -15.61618894467929941, -40.14999999999999858 ) ) ;
#4145 = CARTESIAN_POINT ( 'NONE',  ( 16.13393739769620083, -15.61618894467929941, -35.14999999999999858 ) ) ;
#4146 = CARTESIAN_POINT ( 'NONE',  ( 48.42521416700790127, 25.14253336855949783, -60.76348542011150045 ) ) ;
#4147 = CARTESIAN_POINT ( 'NONE',  ( 49.32485110899289538, 22.33724018645339982, -54.24613943530840032 ) ) ;
#4148 = VERTEX_POINT ( 'NONE', #21809 ) ;
#4149 = CIRCLE ( 'NONE', #41787, 2.999999999999999112 ) ;
#4150 = CARTESIAN_POINT ( 'NONE',  ( 52.95534740401019747, -49.62986309362070614, -49.01774101255579552 ) ) ;
#4151 = EDGE_LOOP ( 'NONE', ( #44976, #16825, #37376, #26694 ) ) ;
#4152 = AXIS2_PLACEMENT_3D ( 'NONE', #36944, #32724, #49020 ) ;
#4153 = CARTESIAN_POINT ( 'NONE',  ( 42.15399884802307895, 7.540547227200079305, -79.88060530502062306 ) ) ;
#4154 = DIRECTION ( 'NONE',  ( 0.000000000000000000, -1.000000000000000000, 0.000000000000000000 ) ) ;
#4155 = DIRECTION ( 'NONE',  ( 1.060511545910580040E-15, 5.351958659602149705E-17, -1.000000000000000000 ) ) ;
#4157 = CARTESIAN_POINT ( 'NONE',  ( 53.54812521361419897, 17.65605455213760067, -26.94805828179969964 ) ) ;
#4156 = CARTESIAN_POINT ( 'NONE',  ( 83.53665286397169609, 13.38078810466280011, -46.51476939800780741 ) ) ;
#4158 = CARTESIAN_POINT ( 'NONE',  ( 12.80387281675960054, -9.399016871829989128, -51.79629490377769940 ) ) ;
#4159 = CARTESIAN_POINT ( 'NONE',  ( 52.69474333003019950, 18.53535902989789719, -48.79529474154600166 ) ) ;
#4160 = CARTESIAN_POINT ( 'NONE',  ( 56.32660178866539979, -45.39391173880739672, -16.96744964118260057 ) ) ;
#4161 = DIRECTION ( 'NONE',  ( 0.000000000000000000, -1.000000000000000000, 0.000000000000000000 ) ) ;
#4162 = VERTEX_POINT ( 'NONE', #14220 ) ;
#4163 = CARTESIAN_POINT ( 'NONE',  ( 16.98336371009930090, -23.41780564399109821, -41.75298454923780156 ) ) ;
#4164 = EDGE_LOOP ( 'NONE', ( #18936, #34770 ) ) ;
#4165 = CARTESIAN_POINT ( 'NONE',  ( 11.36506045489740124, -65.29567750107250390, -17.70888282129770275 ) ) ;
#4166 = CARTESIAN_POINT ( 'NONE',  ( 12.83617943148310125, 34.27320782901589524, -47.68841635077260577 ) ) ;
#4167 = DIRECTION ( 'NONE',  ( 0.000000000000000000, 1.000000000000000000, 0.000000000000000000 ) ) ;
#4168 = CARTESIAN_POINT ( 'NONE',  ( 47.41031548299500287, -54.68188730245149998, -54.95579447497389936 ) ) ;
#4169 = CARTESIAN_POINT ( 'NONE',  ( 8.788582027835408539, 31.90262041517649649, -46.67125809046000029 ) ) ;
#4170 = DIRECTION ( 'NONE',  ( 1.000000000000000000, 0.000000000000000000, 0.000000000000000000 ) ) ;
#4171 = ORIENTED_EDGE ( 'NONE', *, *, #45777, .F. ) ;
#4172 = CARTESIAN_POINT ( 'NONE',  ( 10.83485818036387371, 24.03123212219991345, -45.05995267079551780 ) ) ;
#4173 = CARTESIAN_POINT ( 'NONE',  ( 11.13393739769619906, -63.22724917335859374, -43.91336038921839702 ) ) ;
#4174 = EDGE_CURVE ( 'NONE', #11477, #17310, #6617, .T. ) ;
#4175 = CARTESIAN_POINT ( 'NONE',  ( 13.39998208309985550, 20.55440457967879553, -74.33587756533620450 ) ) ;
#4176 = VERTEX_POINT ( 'NONE', #33607 ) ;
#4177 = CARTESIAN_POINT ( 'NONE',  ( 24.04471994510320343, -15.67954950804986680, -43.79487400242773276 ) ) ;
#4178 = CARTESIAN_POINT ( 'NONE',  ( 56.77163878576220668, 19.44106416691489869, -53.71547587232010557 ) ) ;
#4179 = LINE ( 'NONE', #34921, #51035 ) ;
#4180 = ADVANCED_FACE ( 'NONE', ( #18148, #38328 ), #38598, .T. ) ;
#4181 = FACE_OUTER_BOUND ( 'NONE', #18744, .T. ) ;
#4182 = ORIENTED_EDGE ( 'NONE', *, *, #38309, .T. ) ;
#4183 = CARTESIAN_POINT ( 'NONE',  ( 22.46009133970864369, -20.47788239125953424, -62.00066238588659218 ) ) ;
#4184 = CARTESIAN_POINT ( 'NONE',  ( 18.02855964079323670, -32.51455091268738329, -34.84133294386911217 ) ) ;
#4185 = CARTESIAN_POINT ( 'NONE',  ( 24.04477596867337041, -15.61618922203197357, -43.50766101656756746 ) ) ;
#4186 = CARTESIAN_POINT ( 'NONE',  ( 59.27104365041189027, 16.03377513504399943, -49.27951717864250725 ) ) ;
#4187 = CARTESIAN_POINT ( 'NONE',  ( 9.019481128741650977, -19.78359005965110029, -70.62366323747509966 ) ) ;
#4188 = DIRECTION ( 'NONE',  ( -1.000000000000000000, 0.000000000000000000, 0.000000000000000000 ) ) ;
#4189 = CARTESIAN_POINT ( 'NONE',  ( 54.37485829101720469, 19.90489201363050142, -75.46191895107959624 ) ) ;
#4190 = APPLICATION_PROTOCOL_DEFINITION ( 'draft international standard', 'automotive_design', 1998, #34465 ) ;
#4191 = VERTEX_POINT ( 'NONE', #26258 ) ;
#4192 = VECTOR ( 'NONE', #49646, 1000.000000000000000 ) ;
#4193 = CARTESIAN_POINT ( 'NONE',  ( 9.274006477917760449, -12.70963745175619941, -65.36022600619639888 ) ) ;
#4194 = DIRECTION ( 'NONE',  ( 0.000000000000000000, 0.000000000000000000, 1.000000000000000000 ) ) ;
#4195 = AXIS2_PLACEMENT_3D ( 'NONE', #17134, #1139, #33617 ) ;
#4196 = CARTESIAN_POINT ( 'NONE',  ( 12.55905327122290061, -22.66178945083330021, -32.14999999999999858 ) ) ;
#4197 = VECTOR ( 'NONE', #1154, 1000.000000000000000 ) ;
#4198 = ADVANCED_FACE ( 'NONE', ( #2689 ), #18661, .T. ) ;
#4199 = CARTESIAN_POINT ( 'NONE',  ( 47.11820049732209981, 23.26876160514180114, -75.17431011251740358 ) ) ;
#4200 = EDGE_CURVE ( 'NONE', #8473, #5858, #45646, .T. ) ;
#4201 = DIRECTION ( 'NONE',  ( -1.000000000000000000, 0.000000000000000000, 0.000000000000000000 ) ) ;
#4202 = CARTESIAN_POINT ( 'NONE',  ( 61.72540784289278548, -31.18892121339349899, -16.65167593768012821 ) ) ;
#4203 = B_SPLINE_CURVE_WITH_KNOTS ( 'NONE', 3,
 ( #8870, #9127, #41344, #20639, #1261, #17249, #28508, #48440, #32946, #16724 ),
 .UNSPECIFIED., .F., .F.,
 ( 4, 2, 2, 2, 4 ),
 ( -0.0004281134588448370026, 0.000000000000000000, 0.02012916873217849775, 0.03942875605114479903, 0.05028014561732389170 ),
 .UNSPECIFIED. ) ;
#4204 = DIRECTION ( 'NONE',  ( 0.000000000000000000, 0.7071067811865492381, -0.7071067811865457964 ) ) ;
#4205 = CARTESIAN_POINT ( 'NONE',  ( 9.670066446664469240, -20.73488927165520224, -74.29447132584539304 ) ) ;
#4206 = CARTESIAN_POINT ( 'NONE',  ( 53.99435962611450179, -50.67304520127230205, -76.55038729938830500 ) ) ;
#4208 = DIRECTION ( 'NONE',  ( 1.000000000000000000, 0.000000000000000000, 0.000000000000000000 ) ) ;
#4207 = CARTESIAN_POINT ( 'NONE',  ( 68.13393739769618662, -30.31618894467939995, -81.65000000000000568 ) ) ;
#4209 = CARTESIAN_POINT ( 'NONE',  ( 63.31614497232158811, 1.328073773609220076, -68.78070348185231353 ) ) ;
#4210 = CARTESIAN_POINT ( 'NONE',  ( 61.39588077177570824, 13.94803686931489928, -46.41028556702730157 ) ) ;
#4211 = DIRECTION ( 'NONE',  ( -0.5877852522924744694, -0.8090169943749464521, 0.000000000000000000 ) ) ;
#4212 = ORIENTED_EDGE ( 'NONE', *, *, #33100, .F. ) ;
#4213 = CARTESIAN_POINT ( 'NONE',  ( 53.30277398520830445, -49.41309324413840187, -48.78464791978749560 ) ) ;
#4214 = CARTESIAN_POINT ( 'NONE',  ( 61.35843256309839688, -45.19499326282659979, -28.04812333717190143 ) ) ;
#4215 = CARTESIAN_POINT ( 'NONE',  ( 23.24841639254534087, -19.17784153847612316, -65.93991975907368897 ) ) ;
#4216 = CARTESIAN_POINT ( 'NONE',  ( 56.51875352494170102, 14.92161442796829895, -26.24278457129210196 ) ) ;
#4217 = CARTESIAN_POINT ( 'NONE',  ( 11.16173748537739918, -21.16451498386290098, -72.96524338830400325 ) ) ;
#4218 = CARTESIAN_POINT ( 'NONE',  ( 50.90450009015570032, 18.64662547016060046, -76.22583872417631312 ) ) ;
#4219 = CARTESIAN_POINT ( 'NONE',  ( 52.85417440126129662, 18.42047290032009954, -48.78849739474269853 ) ) ;
#4220 = CARTESIAN_POINT ( 'NONE',  ( 71.28940315555229290, 0.9947083095259759977, -70.74365995857920097 ) ) ;
#4221 = CARTESIAN_POINT ( 'NONE',  ( 64.93393739769619799, 1.383811055320669947, -69.84999999999999432 ) ) ;
#4222 = ORIENTED_EDGE ( 'NONE', *, *, #34472, .T. ) ;
#4223 = CARTESIAN_POINT ( 'NONE',  ( 9.894687805641289913, 22.37488585622680048, -34.64999999999999858 ) ) ;
#4224 = CIRCLE ( 'NONE', #29322, 29.70020322226740106 ) ;
#4225 = CARTESIAN_POINT ( 'NONE',  ( 47.76095205451260739, -54.43479718813880197, -54.75002775354360551 ) ) ;
#4226 = CARTESIAN_POINT ( 'NONE',  ( -6.923399356020619066, 14.58998760014879892, -4.778090148566289663 ) ) ;
#4227 = CIRCLE ( 'NONE', #41860, 1.000000000000000888 ) ;
#4228 =( BOUNDED_CURVE ( )  B_SPLINE_CURVE ( 3, ( #16661, #44965, #9068, #25016 ),
 .UNSPECIFIED., .F., .T. ) 
 B_SPLINE_CURVE_WITH_KNOTS ( ( 4, 4 ),
 ( 0.000000000000000000, 0.3709736340029385904 ),
 .UNSPECIFIED. ) 
 CURVE ( )  GEOMETRIC_REPRESENTATION_ITEM ( )  RATIONAL_B_SPLINE_CURVE ( ( 1.000000000000000000, 0.9885643905736447579, 0.9885643905736447579, 1.000000000000000000 ) ) 
 REPRESENTATION_ITEM ( '' )  );
#4229 = DIRECTION ( 'NONE',  ( 0.1414213562373085320, 0.000000000000000000, 0.9899494936611666907 ) ) ;
#4230 = CARTESIAN_POINT ( 'NONE',  ( 61.61848170108899581, -30.28435294235449859, -16.19051669735609877 ) ) ;
#4231 = CARTESIAN_POINT ( 'NONE',  ( 71.44595490529870574, 0.9958340104639651358, -60.65579263520140074 ) ) ;
#4232 = CARTESIAN_POINT ( 'NONE',  ( 46.63604585716099393, 7.879209231990749629, -34.65000333419789769 ) ) ;
#4233 = CARTESIAN_POINT ( 'NONE',  ( 72.29430833700220660, 1.199410787637519960, -61.36310690539009727 ) ) ;
#4234 = VECTOR ( 'NONE', #48785, 1000.000000000000000 ) ;
#4235 = AXIS2_PLACEMENT_3D ( 'NONE', #15787, #23363, #12123 ) ;
#4236 = CIRCLE ( 'NONE', #11813, 5.499999999999998224 ) ;
#4237 = CARTESIAN_POINT ( 'NONE',  ( 51.23435946743376945, -34.79825311741358007, -76.55133624385516100 ) ) ;
#4238 = CARTESIAN_POINT ( 'NONE',  ( 65.05533261316259086, 1.330484379554840002, -70.49093568668439502 ) ) ;
#4239 = ORIENTED_EDGE ( 'NONE', *, *, #13488, .F. ) ;
#4240 = ORIENTED_EDGE ( 'NONE', *, *, #42017, .F. ) ;
#4241 = CARTESIAN_POINT ( 'NONE',  ( 14.34417029198879945, -51.11618894467930119, -22.49240188329099865 ) ) ;
#4242 = ADVANCED_FACE ( 'NONE', ( #50390 ), #49873, .T. ) ;
#4243 = CARTESIAN_POINT ( 'NONE',  ( 0.03729862092327890233, -45.78233701092020169, -34.73403371893299862 ) ) ;
#4244 = ORIENTED_EDGE ( 'NONE', *, *, #12983, .T. ) ;
#4245 = CARTESIAN_POINT ( 'NONE',  ( 56.76523583744410217, -45.25640930880150137, -25.29480072339120156 ) ) ;
#4246 = CARTESIAN_POINT ( 'NONE',  ( 53.76111468063071896, 20.07186374916310712, -75.55241714225449812 ) ) ;
#4247 = ORIENTED_EDGE ( 'NONE', *, *, #8942, .F. ) ;
#4248 = CARTESIAN_POINT ( 'NONE',  ( 10.84316497021790227, 33.36836038292673123, -23.37164403024571513 ) ) ;
#4249 = CARTESIAN_POINT ( 'NONE',  ( 42.30695455116141801, 6.440213284654995540, -78.78491382788429576 ) ) ;
#4250 = CARTESIAN_POINT ( 'NONE',  ( 21.60595093793588006, -21.40777320653291937, -65.76646804696460435 ) ) ;
#4251 = CARTESIAN_POINT ( 'NONE',  ( 11.51910120158669848, -22.44890487167439730, -44.48141598648059158 ) ) ;
#4252 = FACE_OUTER_BOUND ( 'NONE', #47687, .T. ) ;
#4253 = CARTESIAN_POINT ( 'NONE',  ( 41.95606716547078463, -37.61662454033810121, -80.53928227081438251 ) ) ;
#4254 = SHAPE_REPRESENTATION_RELATIONSHIP ( 'NONE' , 'NONE' ,  #49550, #12204 ) ;
#4255 = VERTEX_POINT ( 'NONE', #22581 ) ;
#4256 = DIRECTION ( 'NONE',  ( 0.000000000000000000, 0.000000000000000000, -1.000000000000000000 ) ) ;
#4257 = CARTESIAN_POINT ( 'NONE',  ( 23.54000810228229668, -16.42662742094869799, -38.26735158243859303 ) ) ;
#4258 = CARTESIAN_POINT ( 'NONE',  ( 45.38213474528080127, 14.14634435393059952, -8.365266594206339335 ) ) ;
#4259 = EDGE_CURVE ( 'NONE', #4597, #47505, #32483, .T. ) ;
#4260 = CARTESIAN_POINT ( 'NONE',  ( 14.46981516282570013, 20.61263520652270032, -75.69337827730609547 ) ) ;
#4261 = LINE ( 'NONE', #26718, #4910 ) ;
#4262 = CARTESIAN_POINT ( 'NONE',  ( 24.03244302888166217, -16.09623076095370209, -59.81164409149027250 ) ) ;
#4263 = CARTESIAN_POINT ( 'NONE',  ( 82.81544245083729550, -45.32786319503500039, -47.32222464724249988 ) ) ;
#4264 = CYLINDRICAL_SURFACE ( 'NONE', #16195, 7.910999999999997812 ) ;
#4265 = CARTESIAN_POINT ( 'NONE',  ( 14.97627619889470019, -7.452700642625790017, -38.96282807147130001 ) ) ;
#4266 = ORIENTED_EDGE ( 'NONE', *, *, #15303, .F. ) ;
#4267 = CARTESIAN_POINT ( 'NONE',  ( 52.86928981489899826, -49.61879012794779698, -27.87016756703999931 ) ) ;
#4268 = CARTESIAN_POINT ( 'NONE',  ( 15.72192118513690140, -50.88627069933389890, -20.20712476364090193 ) ) ;
#4269 = CARTESIAN_POINT ( 'NONE',  ( 50.83473830212534494, -35.51255236623077138, -76.31871491474301195 ) ) ;
#4270 = DIRECTION ( 'NONE',  ( -1.000000000000000000, 0.000000000000000000, 0.000000000000000000 ) ) ;
#4271 = CARTESIAN_POINT ( 'NONE',  ( 6.133937397696199945, -15.61618894467930119, -2.149999999999999911 ) ) ;
#4272 = CARTESIAN_POINT ( 'NONE',  ( 13.19554430456510019, -50.05398003317129962, -21.01912116927340435 ) ) ;
#4273 = ORIENTED_EDGE ( 'NONE', *, *, #28109, .T. ) ;
#4274 = CARTESIAN_POINT ( 'NONE',  ( -9.067911617064609686, -44.12703459110060322, -5.856042089190190758 ) ) ;
#4275 = CARTESIAN_POINT ( 'NONE',  ( 47.44010287600260511, 23.38619148779610057, -54.64745420776859675 ) ) ;
#4276 = CARTESIAN_POINT ( 'NONE',  ( 17.59555472085904171, 18.38379266497329212, -83.19301782015158153 ) ) ;
#4277 = CARTESIAN_POINT ( 'NONE',  ( 63.14473109323350286, 1.096110717717199812, -62.39142878032480155 ) ) ;
#4278 = CARTESIAN_POINT ( 'NONE',  ( 18.13393739769620083, -41.61618894467930119, -35.14999999999999858 ) ) ;
#4279 = CARTESIAN_POINT ( 'NONE',  ( 43.67695093021549724, 12.07467661710849960, -4.963296560282329573 ) ) ;
#4280 = CARTESIAN_POINT ( 'NONE',  ( 33.13393739769620083, 7.383811055320659733, -59.64999999999999147 ) ) ;
#4281 = CARTESIAN_POINT ( 'NONE',  ( 16.13393739769620083, -15.61618894467929941, -49.12910085600329779 ) ) ;
#4282 = DIRECTION ( 'NONE',  ( 0.000000000000000000, 0.000000000000000000, 1.000000000000000000 ) ) ;
#4283 = CARTESIAN_POINT ( 'NONE',  ( 68.13393739769840352, -50.61618894467879670, -73.25000000000220268 ) ) ;
#4284 = CARTESIAN_POINT ( 'NONE',  ( 68.13393739769658453, -28.80002732851820468, -102.2016796975550079 ) ) ;
#4285 = DIRECTION ( 'NONE',  ( 0.000000000000000000, -1.000000000000000000, 0.000000000000000000 ) ) ;
#4286 = CARTESIAN_POINT ( 'NONE',  ( 18.20470492032551846, -7.911113710251287401, -73.09100141137088258 ) ) ;
#4287 = CARTESIAN_POINT ( 'NONE',  ( 63.25226693078700180, 1.024253516290730026, -62.17688587085479668 ) ) ;
#4288 = VERTEX_POINT ( 'NONE', #34635 ) ;
#4289 = CARTESIAN_POINT ( 'NONE',  ( 68.13393739769630031, 16.88381105531836823, -74.20000000000023022 ) ) ;
#4290 = CYLINDRICAL_SURFACE ( 'NONE', #12513, 10.00000000000000355 ) ;
#4291 = CARTESIAN_POINT ( 'NONE',  ( 22.90065656494205726, -15.61616387038935017, -34.45281736178981902 ) ) ;
#4292 = CARTESIAN_POINT ( 'NONE',  ( 10.32524240406999994, -10.84237056084089978, -81.23899999999999011 ) ) ;
#4293 = ORIENTED_EDGE ( 'NONE', *, *, #30139, .F. ) ;
#4294 = CARTESIAN_POINT ( 'NONE',  ( 18.56913828510419862, 20.72643819036759893, -75.26885115310530239 ) ) ;
#4295 = ORIENTED_EDGE ( 'NONE', *, *, #330, .F. ) ;
#4296 = EDGE_CURVE ( 'NONE', #47510, #44411, #34113, .T. ) ;
#4297 = VERTEX_POINT ( 'NONE', #29417 ) ;
#4298 = CARTESIAN_POINT ( 'NONE',  ( 56.70262180045499889, -46.08091195091049741, -26.25054577630639940 ) ) ;
#4299 = CARTESIAN_POINT ( 'NONE',  ( 18.77361538871150159, -21.88214511621840330, -81.23899999999999011 ) ) ;
#4300 = EDGE_CURVE ( 'NONE', #40766, #40450, #5593, .T. ) ;
#4301 = AXIS2_PLACEMENT_3D ( 'NONE', #5206, #17250, #44767 ) ;
#4302 = CARTESIAN_POINT ( 'NONE',  ( 24.04493739743120173, -14.58064912574057992, -73.75066485288634510 ) ) ;
#4303 = EDGE_CURVE ( 'NONE', #20658, #37252, #3132, .T. ) ;
#4304 = CIRCLE ( 'NONE', #41149, 0.5000000000000004441 ) ;
#4305 = CARTESIAN_POINT ( 'NONE',  ( 10.11051084926620014, -19.28509774568809831, -69.67303606471168109 ) ) ;
#4306 = VECTOR ( 'NONE', #24386, 1000.000000000000000 ) ;
#4307 = ADVANCED_FACE ( 'NONE', ( #31212 ), #26772, .T. ) ;
#4308 = CARTESIAN_POINT ( 'NONE',  ( 11.96242356392005846, 34.20360893564268423, -17.67418118889332490 ) ) ;
#4309 = VERTEX_POINT ( 'NONE', #3975 ) ;
#4310 = CARTESIAN_POINT ( 'NONE',  ( 11.63254243215296135, -64.84373839395865957, -23.90641762642841783 ) ) ;
#4311 = DIRECTION ( 'NONE',  ( 0.000000000000000000, 0.000000000000000000, -1.000000000000000000 ) ) ;
#4312 = ORIENTED_EDGE ( 'NONE', *, *, #51576, .T. ) ;
#4313 = EDGE_LOOP ( 'NONE', ( #41035, #49809, #2848, #24121 ) ) ;
#4314 = DIRECTION ( 'NONE',  ( 0.000000000000000000, 1.000000000000000000, 0.000000000000000000 ) ) ;
#4315 = CARTESIAN_POINT ( 'NONE',  ( 10.96947365136730923, -65.06555258025436217, -17.60046481881581215 ) ) ;
#4316 = CARTESIAN_POINT ( 'NONE',  ( 60.96233653960639742, 14.34520385656299979, -47.58503771552609862 ) ) ;
#4317 = EDGE_CURVE ( 'NONE', #5478, #3425, #19940, .T. ) ;
#4318 = B_SPLINE_CURVE_WITH_KNOTS ( 'NONE', 3,
 ( #32621, #17706, #49180, #37363, #48650, #675, #45753, #1203, #45493, #1722, #24763, #13271, #36838, #9591, #41292, #13014, #37617, #49434 ),
 .UNSPECIFIED., .F., .F.,
 ( 4, 2, 2, 2, 2, 2, 2, 2, 4 ),
 ( 0.000000000000000000, 0.2367773115722650590, 0.3750000000000009437, 0.5000000000000017764, 0.5625000000000022204, 0.6625000000000008660, 0.8225000000000022293, 0.9835464721590492232, 1.000000000000000000 ),
 .UNSPECIFIED. ) ;
#4319 = CARTESIAN_POINT ( 'NONE',  ( 48.01232633225529867, 14.92653732367729980, -11.04036235616349870 ) ) ;
#4320 = EDGE_CURVE ( 'NONE', #28785, #3175, #34218, .T. ) ;
#4321 = LINE ( 'NONE', #1432, #39291 ) ;
#4322 = CARTESIAN_POINT ( 'NONE',  ( -7.646760217796759740, 14.02655874010070036, -5.000276550805019760 ) ) ;
#4323 = DIRECTION ( 'NONE',  ( 1.000000000000000000, 0.000000000000000000, 0.000000000000000000 ) ) ;
#4324 = CARTESIAN_POINT ( 'NONE',  ( 54.67238578969960372, 14.97123595123641415, -15.88465852508373999 ) ) ;
#4325 = CARTESIAN_POINT ( 'NONE',  ( 22.00167714248629736, -20.82736716755679751, -65.51866386832359979 ) ) ;
#4326 = VERTEX_POINT ( 'NONE', #35686 ) ;
#4327 = B_SPLINE_CURVE_WITH_KNOTS ( 'NONE', 3,
 ( #30081, #17283, #49003, #41376, #42160, #38227 ),
 .UNSPECIFIED., .F., .F.,
 ( 4, 2, 4 ),
 ( 0.000000000000000000, 0.4925159341063432006, 0.9850318682126864012 ),
 .UNSPECIFIED. ) ;
#4328 = CARTESIAN_POINT ( 'NONE',  ( 57.31674080195730170, 16.10205221464649838, -48.00267488721029707 ) ) ;
#4329 = LINE ( 'NONE', #8787, #43662 ) ;
#4330 = CARTESIAN_POINT ( 'NONE',  ( 11.23465093859169883, 32.93573061327259666, -44.29738226443560478 ) ) ;
#4331 = B_SPLINE_CURVE_WITH_KNOTS ( 'NONE', 3,
 ( #36813, #44167, #8007, #23962, #8262, #40239, #12455, #28425, #40490, #4583 ),
 .UNSPECIFIED., .F., .F.,
 ( 4, 1, 1, 1, 1, 1, 1, 4 ),
 ( 0.000000000000000000, 0.1428489515031106383, 0.2857044903109892675, 0.4285600291188678690, 0.5714155679267454158, 0.7142711067346241283, 0.8571266455425027297, 1.000000000000000000 ),
 .UNSPECIFIED. ) ;
#4332 = CARTESIAN_POINT ( 'NONE',  ( 72.51126090687719739, 1.112168069084249922, -69.74683124610460538 ) ) ;
#4333 = CARTESIAN_POINT ( 'NONE',  ( 44.00040578421071302, -39.95470630028139425, -66.65770786811647497 ) ) ;
#4334 = AXIS2_PLACEMENT_3D ( 'NONE', #15389, #47116, #11205 ) ;
#4336 = EDGE_CURVE ( 'NONE', #43415, #18539, #8273, .T. ) ;
#4335 = CARTESIAN_POINT ( 'NONE',  ( 8.223596773276058869, -15.61622589296290009, -36.79233150823699816 ) ) ;
#4337 = CARTESIAN_POINT ( 'NONE',  ( 46.52573464699440109, 22.06354468997819751, -76.11300885443861830 ) ) ;
#4338 = CARTESIAN_POINT ( 'NONE',  ( 48.65218399916620484, -54.01178499192519666, -54.72548888424969959 ) ) ;
#4339 = CARTESIAN_POINT ( 'NONE',  ( 51.45119095509264184, -32.08428337519749363, -17.60359467805431777 ) ) ;
#4340 = CARTESIAN_POINT ( 'NONE',  ( 64.64302830678670375, 0.9098571636355720083, -70.52991329011129551 ) ) ;
#4341 = CARTESIAN_POINT ( 'NONE',  ( 14.63183004844949942, -32.15985502643049898, -34.65000333055159842 ) ) ;
#4342 = LINE ( 'NONE', #43924, #15577 ) ;
#4343 = ORIENTED_EDGE ( 'NONE', *, *, #8321, .F. ) ;
#4344 = CARTESIAN_POINT ( 'NONE',  ( 18.30559885472430182, -8.906037589390139786, -80.44681068936390034 ) ) ;
#4345 = DIRECTION ( 'NONE',  ( 1.000000000000000000, 0.000000000000000000, 0.000000000000000000 ) ) ;
#4346 = ORIENTED_EDGE ( 'NONE', *, *, #24452, .F. ) ;
#4347 = CARTESIAN_POINT ( 'NONE',  ( 71.62484648860569791, 0.9098571636355680115, -70.52991329011140920 ) ) ;
#4348 = CARTESIAN_POINT ( 'NONE',  ( 60.28868092514740340, -45.80922231065850525, -47.55394404419410392 ) ) ;
#4349 = CARTESIAN_POINT ( 'NONE',  ( 23.48034592329180015, 17.80194031521820008, -34.71551406240349280 ) ) ;
#4350 = CARTESIAN_POINT ( 'NONE',  ( 82.13853704237929776, 13.88381105532070059, -46.37203261889099792 ) ) ;
#4352 = CARTESIAN_POINT ( 'NONE',  ( 14.13393739769619906, -41.61618894467930119, -54.64999999999999858 ) ) ;
#4351 = CARTESIAN_POINT ( 'NONE',  ( 42.26549200200313550, 8.560451897770759544, -75.04938479633833026 ) ) ;
#4353 = LINE ( 'NONE', #420, #12540 ) ;
#4354 = CARTESIAN_POINT ( 'NONE',  ( 8.428842546461108753, -17.68688734103686500, -52.42433491449200034 ) ) ;
#4355 = ORIENTED_EDGE ( 'NONE', *, *, #17566, .F. ) ;
#4356 = CARTESIAN_POINT ( 'NONE',  ( 84.41203222934960593, -43.51893176132989538, -47.41895602134449916 ) ) ;
#4357 = VERTEX_POINT ( 'NONE', #18916 ) ;
#4358 = ORIENTED_EDGE ( 'NONE', *, *, #8638, .F. ) ;
#4359 = CARTESIAN_POINT ( 'NONE',  ( 61.31728467875730360, -45.31601413538380285, -47.18620263350000243 ) ) ;
#4360 = CARTESIAN_POINT ( 'NONE',  ( 11.87263544330925846, -55.38869636903399396, -22.13631662224942787 ) ) ;
#4361 = CARTESIAN_POINT ( 'NONE',  ( 76.39892101097316868, -19.26612468183901328, -12.79189735567145902 ) ) ;
#4362 = CARTESIAN_POINT ( 'NONE',  ( 51.12088197827599600, -52.83173572655250183, -53.84322824623650661 ) ) ;
#4363 = ADVANCED_FACE ( 'NONE', ( #46989 ), #11666, .T. ) ;
#4364 = ORIENTED_EDGE ( 'NONE', *, *, #6824, .F. ) ;
#4365 = EDGE_LOOP ( 'NONE', ( #44840, #47760, #127, #9465, #41618, #39040, #11895 ) ) ;
#4366 = ADVANCED_FACE ( 'NONE', ( #30957 ), #11852, .T. ) ;
#4367 = CARTESIAN_POINT ( 'NONE',  ( 16.13393739769620083, -15.61618894467929941, -15.65000000000000036 ) ) ;
#4368 = CARTESIAN_POINT ( 'NONE',  ( 56.70649773145339623, -45.28348190995249922, -25.29428280798650164 ) ) ;
#4369 = CARTESIAN_POINT ( 'NONE',  ( 56.48532837834070364, -50.76773061328089653, -53.84782101877240024 ) ) ;
#4370 = LINE ( 'NONE', #961, #51202 ) ;
#4371 = DIRECTION ( 'NONE',  ( 0.000000000000000000, 0.000000000000000000, -1.000000000000000000 ) ) ;
#4372 = DIRECTION ( 'NONE',  ( 0.6933752452815366007, -0.7071067811865471286, -0.1386750490563077864 ) ) ;
#4373 = AXIS2_PLACEMENT_3D ( 'NONE', #35818, #23480, #28194 ) ;
#4374 = SHAPE_REPRESENTATION ( 'Top Mounting Plate', ( #20940 ), #40219 ) ;
#4375 = VERTEX_POINT ( 'NONE', #19177 ) ;
#4376 = CARTESIAN_POINT ( 'NONE',  ( 0.4723711254741681520, 21.40360305360503901, -7.245998062423555375 ) ) ;
#4378 = CARTESIAN_POINT ( 'NONE',  ( 53.31396980585229528, -50.46140905625839679, -77.17790061419020731 ) ) ;
#4377 = AXIS2_PLACEMENT_3D ( 'NONE', #9647, #26640, #18271 ) ;
#4379 = CARTESIAN_POINT ( 'NONE',  ( 19.55461702279360026, -22.74941205225439944, -32.14999999999999858 ) ) ;
#4380 = LINE ( 'NONE', #36088, #4452 ) ;
#4381 = CARTESIAN_POINT ( 'NONE',  ( 19.61313273130900114, -22.65052952657820029, -54.36628847889309668 ) ) ;
#4382 = CARTESIAN_POINT ( 'NONE',  ( 13.08906387764550061, -50.12942787500359998, -21.07936304675460093 ) ) ;
#4383 = EDGE_CURVE ( 'NONE', #22924, #40090, #30698, .T. ) ;
#4384 = CARTESIAN_POINT ( 'NONE',  ( 29.13393739769619728, 4.555383930574470774, -84.65000000000000568 ) ) ;
#4385 = CARTESIAN_POINT ( 'NONE',  ( 16.13393739769620083, -15.61618894467929941, -28.45282021618999835 ) ) ;
#4386 = CARTESIAN_POINT ( 'NONE',  ( -0.01592648613901120544, -27.06133052499065172, -34.78031642072627250 ) ) ;
#4387 = CARTESIAN_POINT ( 'NONE',  ( 53.59007319875249920, 18.17385789302069554, -49.22505640236219904 ) ) ;
#4388 = CARTESIAN_POINT ( 'NONE',  ( 61.28085239525059791, 14.36939662108470017, -47.67834120296360112 ) ) ;
#4389 = CARTESIAN_POINT ( 'NONE',  ( 9.096621006920289076, -15.14849546539219993, -49.86830329880680068 ) ) ;
#4390 = CARTESIAN_POINT ( 'NONE',  ( 40.36721523010790236, 13.65407319109839790, -4.296538310233780855 ) ) ;
#4391 = ORIENTED_EDGE ( 'NONE', *, *, #13433, .F. ) ;
#4392 = CARTESIAN_POINT ( 'NONE',  ( 14.63260219478210011, -51.92834279550939414, -75.76244777734170555 ) ) ;
#4393 = CARTESIAN_POINT ( 'NONE',  ( 47.23726808012239786, -54.76554284521510141, -54.66460646074769869 ) ) ;
#4394 = UNCERTAINTY_MEASURE_WITH_UNIT (LENGTH_MEASURE( 1.000000000000000082E-05 ), #23715, 'distance_accuracy_value', 'NONE');
#4395 = CARTESIAN_POINT ( 'NONE',  ( 19.89586642153968299, -12.88298752151932014, -9.721247897589949005 ) ) ;
#4396 = CARTESIAN_POINT ( 'NONE',  ( 12.24650116548775003, 34.20510744208135634, -47.55800081747561592 ) ) ;
#4397 = CARTESIAN_POINT ( 'NONE',  ( 9.367432603602109609, -15.61609789975089946, -77.84717978380999170 ) ) ;
#4398 = CARTESIAN_POINT ( 'NONE',  ( 60.92372936349968171, -45.44413726905956707, -47.20208884485387557 ) ) ;
#4399 = EDGE_CURVE ( 'NONE', #34917, #38938, #45135, .T. ) ;
#4400 = CARTESIAN_POINT ( 'NONE',  ( 55.82671577406989627, -45.92588907196979875, -17.31876445303114309 ) ) ;
#4402 = EDGE_CURVE ( 'NONE', #31635, #37056, #28349, .T. ) ;
#4401 = CARTESIAN_POINT ( 'NONE',  ( 11.42280562906969976, 34.12559483387010317, -18.14299411086210156 ) ) ;
#4404 = CARTESIAN_POINT ( 'NONE',  ( 20.99565372478078729, -21.94232361745867621, -73.79933465604877085 ) ) ;
#4403 = CARTESIAN_POINT ( 'NONE',  ( 53.63393739769619373, 30.88381105532059934, 16.35000000000000142 ) ) ;
#4405 = LINE ( 'NONE', #36362, #6671 ) ;
#4406 = CARTESIAN_POINT ( 'NONE',  ( 43.75992006955644342, 12.39321587538100822, -5.076600544086916855 ) ) ;
#4407 = CARTESIAN_POINT ( 'NONE',  ( 48.55446773597019927, 22.85509828786500108, -54.84877711739730444 ) ) ;
#4408 = EDGE_LOOP ( 'NONE', ( #44563, #7907, #15080, #17680 ) ) ;
#4409 = CARTESIAN_POINT ( 'NONE',  ( 52.72600133020739577, -49.74232360282439913, -48.79686034740650058 ) ) ;
#4410 = CONICAL_SURFACE ( 'NONE', #21127, 14.87302494707580180, 1.249045772398249987 ) ;
#4411 = EDGE_LOOP ( 'NONE', ( #10415, #31036, #10999, #24776 ) ) ;
#4412 = DIRECTION ( 'NONE',  ( 0.000000000000000000, 0.000000000000000000, 1.000000000000000000 ) ) ;
#4413 = CARTESIAN_POINT ( 'NONE',  ( 48.42521416700790127, -56.37491125791819968, -64.38029159777090626 ) ) ;
#4414 = CARTESIAN_POINT ( 'NONE',  ( 56.93701003829870189, -50.64063337602150483, -53.86363391158519676 ) ) ;
#4416 = CARTESIAN_POINT ( 'NONE',  ( 53.98867551104529383, 17.11644939637280061, -26.51198043128849946 ) ) ;
#4415 = CARTESIAN_POINT ( 'NONE',  ( 84.38271246941039294, 12.23852340322079968, -47.29654027836490116 ) ) ;
#4417 = CARTESIAN_POINT ( 'NONE',  ( 19.17564323794969994, -9.252967725988789027, -62.09475594204819515 ) ) ;
#4418 = CARTESIAN_POINT ( 'NONE',  ( 52.75108811105570084, 18.50140338450120225, -48.86094477483089804 ) ) ;
#4419 = CARTESIAN_POINT ( 'NONE',  ( 56.51485985564450232, -45.12984804823710050, -15.71382745701569839 ) ) ;
#4420 = CARTESIAN_POINT ( 'NONE',  ( 18.20469955901954862, -23.32126569534955962, -80.20899953292267526 ) ) ;
#4421 = VERTEX_POINT ( 'NONE', #23093 ) ;
#4422 = ORIENTED_EDGE ( 'NONE', *, *, #41330, .T. ) ;
#4423 = CARTESIAN_POINT ( 'NONE',  ( 11.37461208536520019, -65.06764363074510982, -16.88571178953269936 ) ) ;
#4424 = CARTESIAN_POINT ( 'NONE',  ( 11.63281624934139913, 33.81340851509290246, -46.46564656908429924 ) ) ;
#4425 = CARTESIAN_POINT ( 'NONE',  ( 18.83587408709283650, 20.46262858050933886, -15.79022535844386965 ) ) ;
#4426 = ADVANCED_FACE ( 'NONE', ( #7141 ), #7473, .F. ) ;
#4427 = CARTESIAN_POINT ( 'NONE',  ( 44.34239523011500239, -43.97607093873300244, -3.187564294433600232 ) ) ;
#4428 = CARTESIAN_POINT ( 'NONE',  ( 10.89822354151269934, -64.67713789139354219, -23.30988825783105511 ) ) ;
#4429 = FACE_OUTER_BOUND ( 'NONE', #6380, .T. ) ;
#4430 = ORIENTED_EDGE ( 'NONE', *, *, #17903, .F. ) ;
#4431 = ADVANCED_FACE ( 'NONE', ( #27040 ), #49339, .F. ) ;
#4432 = CARTESIAN_POINT ( 'NONE',  ( 17.16941045954151690, -7.705178316448852094, -75.04930124495368204 ) ) ;
#4433 = CARTESIAN_POINT ( 'NONE',  ( 10.97839846337910075, -63.20796340677059533, -44.74189274530859706 ) ) ;
#4434 = CIRCLE ( 'NONE', #5309, 0.5000000000000000000 ) ;
#4435 = CARTESIAN_POINT ( 'NONE',  ( 59.49262858449159808, -48.61618894467930119, -53.92796738110899923 ) ) ;
#4436 = CARTESIAN_POINT ( 'NONE',  ( 72.35673087767170841, 1.454949836291170140, -69.56035747320190410 ) ) ;
#4437 = CARTESIAN_POINT ( 'NONE',  ( 63.50390619396998915, 1.388715606738730068, -62.57493595107060713 ) ) ;
#4438 = CARTESIAN_POINT ( 'NONE',  ( 52.38386464390320185, 18.65344693462920134, -77.22931088682960876 ) ) ;
#4439 = EDGE_LOOP ( 'NONE', ( #45347, #26205, #5406, #13616 ) ) ;
#4440 = CARTESIAN_POINT ( 'NONE',  ( 15.09838727772565647, -23.52718862466428718, -36.04933377307653330 ) ) ;
#4441 = DIRECTION ( 'NONE',  ( 0.000000000000000000, 0.000000000000000000, 1.000000000000000000 ) ) ;
#4442 = DIRECTION ( 'NONE',  ( -1.000000000000000000, 0.000000000000000000, 0.000000000000000000 ) ) ;
#4443 = CARTESIAN_POINT ( 'NONE',  ( 55.50962190611750202, 15.95222788008109838, -46.54932604926320039 ) ) ;
#4444 = CARTESIAN_POINT ( 'NONE',  ( 24.31683970193839883, -16.62753949476709892, -69.83147392683889620 ) ) ;
#4445 = CARTESIAN_POINT ( 'NONE',  ( 11.12422127314902731, -55.30202234704525921, -21.40295201840961070 ) ) ;
#4446 = LINE ( 'NONE', #40864, #45982 ) ;
#4447 = ITEM_DEFINED_TRANSFORMATION ( 'NONE', 'NONE', #5109,  #20940 ) ;
#4448 = CARTESIAN_POINT ( 'NONE',  ( 46.79542243668350210, -53.50887967020530311, -76.01632185952030341 ) ) ;
#4449 = ORIENTED_EDGE ( 'NONE', *, *, #48595, .T. ) ;
#4450 = AXIS2_PLACEMENT_3D ( 'NONE', #24682, #861, #33071 ) ;
#4451 = CARTESIAN_POINT ( 'NONE',  ( 17.14173437892020146, -8.234384351642349387, -63.77584738492399197 ) ) ;
#4452 = VECTOR ( 'NONE', #48150, 1000.000000000000000 ) ;
#4453 = CARTESIAN_POINT ( 'NONE',  ( 68.13393739769618662, -1.666188944679350081, -65.65000000000000568 ) ) ;
#4454 = CARTESIAN_POINT ( 'NONE',  ( 18.71043739769620018, -15.61618894467929941, -22.64999999999999858 ) ) ;
#4455 = CARTESIAN_POINT ( 'NONE',  ( 46.48058913279649573, 21.92052743937680148, -76.13714234130850400 ) ) ;
#4456 = CARTESIAN_POINT ( 'NONE',  ( 16.13393739769620083, -15.61618894467929941, 6.349999999999999645 ) ) ;
#4457 = FACE_OUTER_BOUND ( 'NONE', #46813, .T. ) ;
#4458 = CARTESIAN_POINT ( 'NONE',  ( 33.53393739769619231, -15.61618894467929763, -10.44999999999999929 ) ) ;
#4459 = CARTESIAN_POINT ( 'NONE',  ( 23.31098559560239991, -11.55753154673280036, -73.34384415308208816 ) ) ;
#4460 = ADVANCED_FACE ( 'NONE', ( #24627 ), #4828, .T. ) ;
#4461 = AXIS2_PLACEMENT_3D ( 'NONE', #3913, #8610, #27741 ) ;
#4462 = CARTESIAN_POINT ( 'NONE',  ( 56.39839003427439934, -50.66188084753460430, -75.14917411940758996 ) ) ;
#4464 = DIRECTION ( 'NONE',  ( 1.000000000000000000, 2.460964292799963328E-14, 0.000000000000000000 ) ) ;
#4463 = CYLINDRICAL_SURFACE ( 'NONE', #8996, 6.766999999999998572 ) ;
#4465 = CARTESIAN_POINT ( 'NONE',  ( 63.21844385136499511, 1.269319268680890067, -68.77895457036579785 ) ) ;
#4466 = CARTESIAN_POINT ( 'NONE',  ( 61.26594051415460029, 14.01037552971329880, -46.68275217642920438 ) ) ;
#4467 = CARTESIAN_POINT ( 'NONE',  ( -28.48658230523989943, -35.31887766905860104, -54.95457219459440523 ) ) ;
#4468 = EDGE_CURVE ( 'NONE', #42029, #6481, #14979, .T. ) ;
#4469 = EDGE_LOOP ( 'NONE', ( #21660, #15593, #7563, #28992 ) ) ;
#4470 = CARTESIAN_POINT ( 'NONE',  ( 52.87578377016760101, -49.63680538124820885, -48.67531175415550138 ) ) ;
#4471 = CARTESIAN_POINT ( 'NONE',  ( 61.10919664416649510, -45.15820646057929366, -27.23097577694250049 ) ) ;
#4472 = CARTESIAN_POINT ( 'NONE',  ( 23.04644707764643741, -19.60034574208615510, -71.95901429853738307 ) ) ;
#4473 = CARTESIAN_POINT ( 'NONE',  ( 56.72744220692439399, 14.83176467157860046, -26.24945950869589950 ) ) ;
#4474 = CARTESIAN_POINT ( 'NONE',  ( 9.101765327396449834, -15.07663851068110006, -35.47719510467199910 ) ) ;
#4475 = CARTESIAN_POINT ( 'NONE',  ( 51.13982992927869731, 19.47025619440540112, -76.16554326337229952 ) ) ;
#4476 = CARTESIAN_POINT ( 'NONE',  ( 53.00693766222299530, 18.33849153667809873, -48.85763909861859844 ) ) ;
#4477 = CARTESIAN_POINT ( 'NONE',  ( 71.15378634064809660, 1.278021359705829862, -70.61864533961639268 ) ) ;
#4478 = CARTESIAN_POINT ( 'NONE',  ( 43.42022383785410256, -43.54919953056790405, -4.975730455609930658 ) ) ;
#4479 = ORIENTED_EDGE ( 'NONE', *, *, #36354, .F. ) ;
#4480 = DIRECTION ( 'NONE',  ( -1.000000000000000000, 0.000000000000000000, 0.000000000000000000 ) ) ;
#4481 = CIRCLE ( 'NONE', #297, 19.30901699437490038 ) ;
#4482 = CARTESIAN_POINT ( 'NONE',  ( 47.66583891269780082, -54.50953961429650008, -54.89454647195640291 ) ) ;
#4483 = FACE_OUTER_BOUND ( 'NONE', #38412, .T. ) ;
#4484 = DIRECTION ( 'NONE',  ( 0.000000000000000000, -1.000000000000000000, 0.000000000000000000 ) ) ;
#4485 = CARTESIAN_POINT ( 'NONE',  ( 59.34568438161719683, 16.86995364085609950, -50.40761009331129827 ) ) ;
#4486 = CARTESIAN_POINT ( 'NONE',  ( 71.31509885739851029, 1.369976237678180109, -60.95504431261769440 ) ) ;
#4487 = CARTESIAN_POINT ( 'NONE',  ( 14.63393739769620083, -23.61618894467940066, -35.14999999999999858 ) ) ;
#4488 = CIRCLE ( 'NONE', #35431, 4.065501003882420861 ) ;
#4489 = CARTESIAN_POINT ( 'NONE',  ( 71.39063606569699516, 1.391735898526160087, -61.04516847149080405 ) ) ;
#4490 = LINE ( 'NONE', #9215, #44415 ) ;
#4491 = ADVANCED_FACE ( 'NONE', ( #3845 ), #8026, .F. ) ;
#4492 = CARTESIAN_POINT ( 'NONE',  ( 65.16938214696820353, 1.384887413063050188, -70.31636399389039127 ) ) ;
#4493 = VERTEX_POINT ( 'NONE', #19818 ) ;
#4494 = ORIENTED_EDGE ( 'NONE', *, *, #17547, .T. ) ;
#4495 = CARTESIAN_POINT ( 'NONE',  ( 57.35856957515439092, 18.90358493360990266, -52.61941485521469986 ) ) ;
#4496 = ORIENTED_EDGE ( 'NONE', *, *, #12191, .T. ) ;
#4497 = CYLINDRICAL_SURFACE ( 'NONE', #50152, 6.766999999999998572 ) ;
#4498 = CARTESIAN_POINT ( 'NONE',  ( 56.92979928365449638, -45.19979990857069652, -25.29906707419310052 ) ) ;
#4499 = CARTESIAN_POINT ( 'NONE',  ( 18.66275191049972193, -9.321185306396447601, -50.07447558512664187 ) ) ;
#4500 = VERTEX_POINT ( 'NONE', #11972 ) ;
#4501 = DIRECTION ( 'NONE',  ( 0.000000000000000000, 1.000000000000000000, 0.000000000000000000 ) ) ;
#4502 = CARTESIAN_POINT ( 'NONE',  ( 41.96574616844770844, 6.385856618463681578, -80.49088675293293704 ) ) ;
#4503 = CARTESIAN_POINT ( 'NONE',  ( 24.04493739922218509, -15.61697502474068244, -65.50769812753713950 ) ) ;
#4504 = CARTESIAN_POINT ( 'NONE',  ( 16.88526009776989767, -23.82704969470360012, -42.26328591669929580 ) ) ;
#4505 = CARTESIAN_POINT ( 'NONE',  ( 45.32664390791340026, 2.629232284582370127, -34.65030768300919561 ) ) ;
#4506 = CARTESIAN_POINT ( 'NONE',  ( 42.40338535657301833, -37.68800879611313093, -78.30275109164772118 ) ) ;
#4507 =( NAMED_UNIT ( * ) PLANE_ANGLE_UNIT ( ) SI_UNIT ( $, .RADIAN. ) );
#4508 = EDGE_LOOP ( 'NONE', ( #28300, #30974, #7549, #21789, #13623 ) ) ;
#4509 = CARTESIAN_POINT ( 'NONE',  ( 11.89321894728460016, -65.43602743322060178, -22.25048311349110008 ) ) ;
#4510 = CARTESIAN_POINT ( 'NONE',  ( 23.02829992630010025, -12.79228046009130004, -38.10891372031129976 ) ) ;
#4511 = CARTESIAN_POINT ( 'NONE',  ( 11.72631995337559907, -10.41982837502230019, -32.14999999999999858 ) ) ;
#4512 = CARTESIAN_POINT ( 'NONE',  ( 14.49461893737620066, 21.34486587698399873, -76.03043890231919022 ) ) ;
#4513 = CARTESIAN_POINT ( 'NONE',  ( 51.78349585950329725, 17.91029630874730216, -77.04629326439351189 ) ) ;
#4514 = CARTESIAN_POINT ( 'NONE',  ( 84.37071767335301331, -43.44691413872259744, -47.23470317516529349 ) ) ;
#4515 = CARTESIAN_POINT ( 'NONE',  ( 18.11900864776900022, 1.362847559348050019, -35.02873218748179340 ) ) ;
#4516 = CARTESIAN_POINT ( 'NONE',  ( 8.654671703226251012, -12.14584236537350037, -38.64595234721679162 ) ) ;
#4517 = ORIENTED_EDGE ( 'NONE', *, *, #25718, .T. ) ;
#4518 = CARTESIAN_POINT ( 'NONE',  ( 54.67056220863920402, -47.85029607447599886, -26.56517469137810039 ) ) ;
#4519 = EDGE_CURVE ( 'NONE', #38150, #34997, #2485, .T. ) ;
#4520 = CARTESIAN_POINT ( 'NONE',  ( 10.69486856911679773, -64.90650667235888704, -18.00056245200230265 ) ) ;
#4521 = CARTESIAN_POINT ( 'NONE',  ( 50.92222208382837323, -35.35889331638581012, -76.36000770886168709 ) ) ;
#4522 = CARTESIAN_POINT ( 'NONE',  ( 57.35094531453410127, 19.00534567308480050, -52.73804475687700233 ) ) ;
#4523 = CARTESIAN_POINT ( 'NONE',  ( 22.90093474723966338, -15.62310588710952430, -56.45315049504032601 ) ) ;
#4524 = DIRECTION ( 'NONE',  ( 0.000000000000000000, 1.000000000000000000, 0.000000000000000000 ) ) ;
#4525 = ORIENTED_EDGE ( 'NONE', *, *, #44169, .T. ) ;
#4526 = CARTESIAN_POINT ( 'NONE',  ( -11.32734370190460105, -41.88171845330919751, -6.430192534648670133 ) ) ;
#4527 = CARTESIAN_POINT ( 'NONE',  ( 47.36546503952629905, 23.43920771176249929, -54.65494689270030193 ) ) ;
#4528 = CARTESIAN_POINT ( 'NONE',  ( 22.90114886013774864, -15.61618877916400017, -48.45281860778688809 ) ) ;
#4529 = CARTESIAN_POINT ( 'NONE',  ( 63.35267264707980672, 1.373356196620449943, -62.69406858229250901 ) ) ;
#4530 = CARTESIAN_POINT ( 'NONE',  ( 56.24183557072737472, 15.29150438182242944, -26.31651977536066767 ) ) ;
#4531 = CARTESIAN_POINT ( 'NONE',  ( 41.32046355873320209, 13.29656256355710120, -4.975096813130970297 ) ) ;
#4532 = CARTESIAN_POINT ( 'NONE',  ( 51.13393739769620083, 19.38381105532069881, 10.84999999999999964 ) ) ;
#4533 = CARTESIAN_POINT ( 'NONE',  ( -13.73674066540309902, -30.55263188852779876, -46.71145918530379504 ) ) ;
#4534 = CARTESIAN_POINT ( 'NONE',  ( 53.97862732855089263, -49.20418162442920362, -49.10777757132959920 ) ) ;
#4535 = CARTESIAN_POINT ( 'NONE',  ( 24.03381927417788688, -15.16328978430293617, -75.77410088211345851 ) ) ;
#4536 = CIRCLE ( 'NONE', #25476, 9.500000000000000000 ) ;
#4537 = CARTESIAN_POINT ( 'NONE',  ( 64.99178804968060774, 1.386446979194299933, -61.00873193152619933 ) ) ;
#4538 = CARTESIAN_POINT ( 'NONE',  ( 17.35260714571270313, -52.98224883304730071, -76.14999999999999147 ) ) ;
#4539 = ADVANCED_FACE ( 'NONE', ( #48119 ), #16401, .T. ) ;
#4540 = CARTESIAN_POINT ( 'NONE',  ( 8.428888066787989075, -13.54532504059405262, -72.59100176599271492 ) ) ;
#4541 = CARTESIAN_POINT ( 'NONE',  ( 19.57810744170729933, -21.77087888895180257, -80.79042367306239214 ) ) ;
#4542 = FACE_BOUND ( 'NONE', #42157, .T. ) ;
#4543 = ORIENTED_EDGE ( 'NONE', *, *, #19788, .T. ) ;
#4544 = CARTESIAN_POINT ( 'NONE',  ( 16.13393739769620083, -15.61618894467929941, -22.14999999999999858 ) ) ;
#4545 = CARTESIAN_POINT ( 'NONE',  ( 10.14752524939349954, 32.07972278140049838, -45.99340881354279986 ) ) ;
#4546 = CARTESIAN_POINT ( 'NONE',  ( 28.28038400710291356, -22.62894316431776431, -34.79644660940672907 ) ) ;
#4547 = CARTESIAN_POINT ( 'NONE',  ( 68.11938491324369238, -30.76296629286689921, -18.02961409148510086 ) ) ;
#4548 = ORIENTED_EDGE ( 'NONE', *, *, #51697, .T. ) ;
#4549 = EDGE_CURVE ( 'NONE', #4830, #40276, #37563, .T. ) ;
#4550 = CARTESIAN_POINT ( 'NONE',  ( 18.67864726532610220, 20.47004600267149854, -74.90176971618339508 ) ) ;
#4551 = ORIENTED_EDGE ( 'NONE', *, *, #20681, .F. ) ;
#4552 = EDGE_LOOP ( 'NONE', ( #47795, #4567, #42876, #32069 ) ) ;
#4553 = VECTOR ( 'NONE', #12928, 1000.000000000000000 ) ;
#4554 = EDGE_CURVE ( 'NONE', #17966, #12701, #23468, .T. ) ;
#4555 = ORIENTED_EDGE ( 'NONE', *, *, #12898, .F. ) ;
#4556 = CARTESIAN_POINT ( 'NONE',  ( 10.69868903310229946, -63.71459361368848562, -45.45668842281379796 ) ) ;
#4557 = DIRECTION ( 'NONE',  ( 0.000000000000000000, 0.000000000000000000, 1.000000000000000000 ) ) ;
#4558 = CARTESIAN_POINT ( 'NONE',  ( 22.59237592338839917, -18.78433718290749965, -81.23899999999999011 ) ) ;
#4559 = CARTESIAN_POINT ( 'NONE',  ( 0.4371248283888460318, -8.845792823550640449, -35.02873218748179340 ) ) ;
#4560 = ORIENTED_EDGE ( 'NONE', *, *, #15196, .T. ) ;
#4561 = CARTESIAN_POINT ( 'NONE',  ( 75.25805505272104767, 3.492023333372584304, -12.32941048424839714 ) ) ;
#4562 = FACE_OUTER_BOUND ( 'NONE', #8022, .T. ) ;
#4563 = ORIENTED_EDGE ( 'NONE', *, *, #42965, .F. ) ;
#4564 = CARTESIAN_POINT ( 'NONE',  ( 11.27243636593874321, -64.25380594475855389, -24.07146289791958083 ) ) ;
#4565 = CARTESIAN_POINT ( 'NONE',  ( 51.67587649748470113, 2.735120682347050192, -77.01363636363508647 ) ) ;
#4566 = ORIENTED_EDGE ( 'NONE', *, *, #27452, .F. ) ;
#4567 = ORIENTED_EDGE ( 'NONE', *, *, #29640, .F. ) ;
#4568 = DIRECTION ( 'NONE',  ( 0.000000000000000000, 1.000000000000000000, 0.000000000000000000 ) ) ;
#4569 = DIRECTION ( 'NONE',  ( 0.000000000000000000, 0.000000000000000000, 1.000000000000000000 ) ) ;
#4570 = CARTESIAN_POINT ( 'NONE',  ( 72.83796717360608852, 13.88381330399790059, -14.37527876787380166 ) ) ;
#4571 = CARTESIAN_POINT ( 'NONE',  ( 46.77197036051299506, 13.96716929081839886, -8.919993557679239515 ) ) ;
#4572 = AXIS2_PLACEMENT_3D ( 'NONE', #20874, #40799, #13047 ) ;
#4573 = CARTESIAN_POINT ( 'NONE',  ( 11.27229808032523728, -21.94238343154312076, -68.50066414062398223 ) ) ;
#4574 = CARTESIAN_POINT ( 'NONE',  ( -7.653322383143519758, 14.02129102275489991, -4.959142628649059859 ) ) ;
#4575 = CARTESIAN_POINT ( 'NONE',  ( 9.849809295681199117, -62.03066548993875529, -13.59693312241669538 ) ) ;
#4576 = CARTESIAN_POINT ( 'NONE',  ( 61.29464672451849339, 13.96904609170759848, -27.75181424375799821 ) ) ;
#4577 = CARTESIAN_POINT ( 'NONE',  ( 8.411629955056419305, -17.01358507482030191, -58.23052221047058907 ) ) ;
#4578 = ORIENTED_EDGE ( 'NONE', *, *, #29513, .T. ) ;
#4579 = CARTESIAN_POINT ( 'NONE',  ( 60.34379256561150129, 14.63564648314799932, -47.72732608210890248 ) ) ;
#4580 = EDGE_CURVE ( 'NONE', #30985, #23531, #19208, .T. ) ;
#4581 = VECTOR ( 'NONE', #6997, 1000.000000000000000 ) ;
#4582 = CARTESIAN_POINT ( 'NONE',  ( 19.11048863820259669, -9.222230711542339421, -76.48586413618289725 ) ) ;
#4583 = CARTESIAN_POINT ( 'NONE',  ( 54.17308945005400034, -50.61618894467930119, -77.01198594373980200 ) ) ;
#4584 = CARTESIAN_POINT ( 'NONE',  ( 72.32470129585499308, 1.409272994606969975, -69.70523042975179351 ) ) ;
#4585 = CARTESIAN_POINT ( 'NONE',  ( 43.69898371111283097, -39.92948724415479234, -68.11687742724626560 ) ) ;
#4586 = DIRECTION ( 'NONE',  ( -0.6209860917175333839, 0.7838215829468996310, 0.000000000000000000 ) ) ;
#4587 = CARTESIAN_POINT ( 'NONE',  ( 47.13701186032770352, 23.47047141344530274, -74.81156593794960941 ) ) ;
#4588 = CARTESIAN_POINT ( 'NONE',  ( 49.54719217692459665, -53.70731863405879380, -54.90723160129140012 ) ) ;
#4589 = DIRECTION ( 'NONE',  ( 0.000000000000000000, 0.000000000000000000, 1.000000000000000000 ) ) ;
#4590 = CARTESIAN_POINT ( 'NONE',  ( 13.03988958525129505, -22.92537339708916022, -34.13518226141717804 ) ) ;
#4591 = LINE ( 'NONE', #48369, #38012 ) ;
#4592 = CARTESIAN_POINT ( 'NONE',  ( 21.09281434348020667, -20.63137574190061230, -71.09897682385668816 ) ) ;
#4593 = ORIENTED_EDGE ( 'NONE', *, *, #26317, .T. ) ;
#4594 = EDGE_CURVE ( 'NONE', #21370, #1802, #16307, .T. ) ;
#4595 = CARTESIAN_POINT ( 'NONE',  ( 10.99422185684939812, -10.22267260582209936, -42.32501095722309259 ) ) ;
#4596 = CARTESIAN_POINT ( 'NONE',  ( 64.91115770917910766, 1.389801772588449946, -61.03316673290180461 ) ) ;
#4597 = VERTEX_POINT ( 'NONE', #32615 ) ;
#4598 = CARTESIAN_POINT ( 'NONE',  ( 84.44784216359251161, -43.11618894467930119, -47.47585302082339354 ) ) ;
#4599 = CARTESIAN_POINT ( 'NONE',  ( 60.68483835214470190, -45.58309487373249880, -47.38195381330299938 ) ) ;
#4600 = CARTESIAN_POINT ( 'NONE',  ( 56.91872540560049742, 19.41123227373109827, -53.86107397111689465 ) ) ;
#4601 = CARTESIAN_POINT ( 'NONE',  ( 53.58978845500833188, -43.47732832942402581, -7.400799757652920974 ) ) ;
#4602 = ADVANCED_FACE ( 'NONE', ( #5659 ), #41286, .T. ) ;
#4604 = CARTESIAN_POINT ( 'NONE',  ( 20.99560079206503360, -21.94236587381720938, -78.08399595254924463 ) ) ;
#4603 = CARTESIAN_POINT ( 'NONE',  ( 42.87835492171312524, 8.621997877449000924, -72.08792712645744416 ) ) ;
#4605 = CARTESIAN_POINT ( 'NONE',  ( 57.34776335324270491, 14.57942837581910034, -26.27178905609630277 ) ) ;
#4606 = DIRECTION ( 'NONE',  ( 6.073366656256538404E-31, 1.365304166073849981E-11, -1.000000000000000000 ) ) ;
#4607 = ORIENTED_EDGE ( 'NONE', *, *, #42486, .T. ) ;
#4608 = CARTESIAN_POINT ( 'NONE',  ( 84.40405423732200063, -43.50691743144619750, -47.38850513265820297 ) ) ;
#4609 = AXIS2_PLACEMENT_3D ( 'NONE', #34730, #30537, #37644 ) ;
#4610 = ORIENTED_EDGE ( 'NONE', *, *, #24701, .T. ) ;
#4611 = ORIENTED_EDGE ( 'NONE', *, *, #18736, .F. ) ;
#4612 = ADVANCED_FACE ( 'NONE', ( #12743 ), #17699, .F. ) ;
#4613 = ORIENTED_EDGE ( 'NONE', *, *, #36546, .T. ) ;
#4614 = CYLINDRICAL_SURFACE ( 'NONE', #30289, 6.766999999999998572 ) ;
#4615 = CARTESIAN_POINT ( 'NONE',  ( 53.42052211308229914, -49.46494215952650109, -49.21491387939300211 ) ) ;
#4616 = LINE ( 'NONE', #20587, #47502 ) ;
#4617 = AXIS2_PLACEMENT_3D ( 'NONE', #27838, #18951, #35190 ) ;
#4618 = CARTESIAN_POINT ( 'NONE',  ( 76.44636317954351057, -6.604856247326271301, -12.99628919329122567 ) ) ;
#4619 = B_SPLINE_CURVE_WITH_KNOTS ( 'NONE', 3,
 ( #46484, #30977, #50656, #34915, #14492, #27311, #39381, #43317, #14752, #7410, #19191 ),
 .UNSPECIFIED., .F., .F.,
 ( 4, 1, 1, 1, 1, 1, 1, 1, 4 ),
 ( 0.4999961688222710476, 0.5146094102817740934, 0.5938283413453584458, 0.6730472724089429093, 0.7522662034725273728, 0.8314851345361116142, 0.9107040655996961886, 0.9899229966632812072, 1.000000000000000000 ),
 .UNSPECIFIED. ) ;
#4620 = CARTESIAN_POINT ( 'NONE',  ( 49.93407130271199890, -53.44037199461649834, -54.35262932774689659 ) ) ;
#4621 = ORIENTED_EDGE ( 'NONE', *, *, #27776, .T. ) ;
#4622 = EDGE_LOOP ( 'NONE', ( #484, #25916 ) ) ;
#4623 = CARTESIAN_POINT ( 'NONE',  ( 16.13393739769620083, -15.61618894467929941, -15.65000000000000036 ) ) ;
#4624 = CARTESIAN_POINT ( 'NONE',  ( 56.39270785951039500, 19.29512406318060158, -52.86271188469099513 ) ) ;
#4625 = DIRECTION ( 'NONE',  ( 0.000000000000000000, 0.000000000000000000, 1.000000000000000000 ) ) ;
#4626 = CARTESIAN_POINT ( 'NONE',  ( 17.00689302767908728, -14.98194955443502252, -14.88746750000000141 ) ) ;
#4627 = CARTESIAN_POINT ( 'NONE',  ( 61.88703750214839516, -0.1196547126231959912, -16.64423871873319882 ) ) ;
#4628 = ORIENTED_EDGE ( 'NONE', *, *, #882, .F. ) ;
#4629 = FACE_OUTER_BOUND ( 'NONE', #21935, .T. ) ;
#4630 = CARTESIAN_POINT ( 'NONE',  ( 52.62506682249000534, -50.12296729442330445, -77.17021719677750013 ) ) ;
#4631 = CARTESIAN_POINT ( 'NONE',  ( 10.33236275321031883, -12.06453136622874744, -33.62757847280354895 ) ) ;
#4632 = CARTESIAN_POINT ( 'NONE',  ( 83.07525789764410717, -45.50438969202907913, -47.60488146813197829 ) ) ;
#4633 = CARTESIAN_POINT ( 'NONE',  ( 10.18757820060029928, -10.49490396035219852, -63.23880875801859958 ) ) ;
#4634 = CARTESIAN_POINT ( 'NONE',  ( -0.1437508118502176246, -3.968240916618980041, -34.89146800830123851 ) ) ;
#4635 = DIRECTION ( 'NONE',  ( 1.000000000000000000, 0.000000000000000000, 0.000000000000000000 ) ) ;
#4636 = CARTESIAN_POINT ( 'NONE',  ( 43.46307289448600386, -43.09202836464690023, -4.765184494693460060 ) ) ;
#4637 = CARTESIAN_POINT ( 'NONE',  ( 18.46789571041282230, -51.27714561189082332, -15.70464893408844276 ) ) ;
#4638 = CARTESIAN_POINT ( 'NONE',  ( 56.07568387335299320, 13.88381105532070059, -14.74720100809580003 ) ) ;
#4639 = DIRECTION ( 'NONE',  ( 0.000000000000000000, 0.000000000000000000, -1.000000000000000000 ) ) ;
#4640 = CARTESIAN_POINT ( 'NONE',  ( 63.91099139885979241, 1.441354206319580111, -69.60041390115910076 ) ) ;
#4641 = VECTOR ( 'NONE', #24025, 1000.000000000000000 ) ;
#4642 = CARTESIAN_POINT ( 'NONE',  ( 24.04526736911255469, -15.61618908158827068, -41.79233198438217300 ) ) ;
#4643 = VERTEX_POINT ( 'NONE', #28698 ) ;
#4644 = AXIS2_PLACEMENT_3D ( 'NONE', #28363, #48053, #8214 ) ;
#4645 = CARTESIAN_POINT ( 'NONE',  ( 14.15218391821419885, -52.24722748763079494, -75.79330468503940210 ) ) ;
#4646 = EDGE_CURVE ( 'NONE', #48924, #17157, #40980, .T. ) ;
#4647 = CARTESIAN_POINT ( 'NONE',  ( 47.28316422028650123, -54.73279202814679678, -54.73281782041389931 ) ) ;
#4648 = CARTESIAN_POINT ( 'NONE',  ( 10.22101148145273264, -12.20822225728566757, -37.61948740445134831 ) ) ;
#4649 = EDGE_CURVE ( 'NONE', #17198, #22850, #10005, .T. ) ;
#4650 = FACE_OUTER_BOUND ( 'NONE', #24412, .T. ) ;
#4651 = EDGE_CURVE ( 'NONE', #367, #12539, #11308, .T. ) ;
#4652 = CARTESIAN_POINT ( 'NONE',  ( 61.01465046515617274, -45.45355287326128746, -47.35110780635755390 ) ) ;
#4653 = CARTESIAN_POINT ( 'NONE',  ( 22.89031856386410269, -13.37760718783400193, -32.14999999999999858 ) ) ;
#4654 = CARTESIAN_POINT ( 'NONE',  ( 16.98877563629383403, -17.26294695554419434, -34.79644660940672907 ) ) ;
#4655 = EDGE_CURVE ( 'NONE', #14522, #39228, #39303, .T. ) ;
#4656 = DIRECTION ( 'NONE',  ( 0.000000000000000000, -1.000000000000000000, 0.000000000000000000 ) ) ;
#4658 = CARTESIAN_POINT ( 'NONE',  ( 17.16950934076716351, -23.52718544910446496, -52.25066344205447422 ) ) ;
#4657 = DIRECTION ( 'NONE',  ( 8.462868000000000073E-18, -1.066343000000000058E-17, 1.000000000000000000 ) ) ;
#4659 = STYLED_ITEM ( 'NONE', ( #16128 ), #10006 ) ;
#4660 = CARTESIAN_POINT ( 'NONE',  ( 51.13393739769659874, -56.11618894467899565, 14.21249999999999858 ) ) ;
#4661 = CARTESIAN_POINT ( 'NONE',  ( 43.60412366721264732, 12.47234831454305848, -5.064848483119741118 ) ) ;
#4662 = CARTESIAN_POINT ( 'NONE',  ( 48.40438293219020238, 22.95961779500990119, -55.05471046037709471 ) ) ;
#4663 = ORIENTED_EDGE ( 'NONE', *, *, #43243, .F. ) ;
#4664 = CARTESIAN_POINT ( 'NONE',  ( 22.58529838043510196, -18.46618905781010156, -66.97959240854848417 ) ) ;
#4665 = ORIENTED_EDGE ( 'NONE', *, *, #41164, .T. ) ;
#4666 = CARTESIAN_POINT ( 'NONE',  ( 82.81464131963001307, 11.88381105532070059, -49.28546657628889704 ) ) ;
#4667 = CARTESIAN_POINT ( 'NONE',  ( 64.95360084570980064, 1.395196698723390138, -61.05633982442969909 ) ) ;
#4669 = EDGE_CURVE ( 'NONE', #17870, #23355, #3788, .T. ) ;
#4668 = CARTESIAN_POINT ( 'NONE',  ( 14.16379049631229847, 19.89932139981819859, -22.70798728939849909 ) ) ;
#4671 = CARTESIAN_POINT ( 'NONE',  ( 55.57695098842009429, 15.27039860521809977, -25.90100721923549898 ) ) ;
#4670 = CARTESIAN_POINT ( 'NONE',  ( 83.66217889154638954, 13.27350842653780028, -46.56966809452239886 ) ) ;
#4672 = CARTESIAN_POINT ( 'NONE',  ( 9.352034712855139986, -13.68012214057080023, -69.54133546202830019 ) ) ;
#4673 = LINE ( 'NONE', #25856, #43488 ) ;
#4674 = CARTESIAN_POINT ( 'NONE',  ( 54.68760425043940643, -45.72106579749050326, -15.47702710567550000 ) ) ;
#4675 = CARTESIAN_POINT ( 'NONE',  ( 16.13393739769620083, -15.61618894467929941, -28.45282021618999835 ) ) ;
#4676 = CIRCLE ( 'NONE', #8049, 1.000000000000000888 ) ;
#4677 = VERTEX_POINT ( 'NONE', #1197 ) ;
#4678 = EDGE_CURVE ( 'NONE', #46513, #35078, #33136, .T. ) ;
#4679 = ORIENTED_EDGE ( 'NONE', *, *, #9772, .F. ) ;
#4680 = CARTESIAN_POINT ( 'NONE',  ( 12.17742765526699955, -65.07456428805339499, -16.46016921340210004 ) ) ;
#4681 = CARTESIAN_POINT ( 'NONE',  ( 9.991756373883710296, 32.50750339410230083, -46.24817865174940579 ) ) ;
#4682 = CARTESIAN_POINT ( 'NONE',  ( 61.48314149772338766, -45.36441574363837503, -47.33726207365202043 ) ) ;
#4683 = SHAPE_REPRESENTATION ( 'Swivel Caster Main Housing', ( #20940 ), #5952 ) ;
#4684 = CARTESIAN_POINT ( 'NONE',  ( 52.44527164998969937, -50.16109774121770215, -49.63631393125859859 ) ) ;
#4685 = CARTESIAN_POINT ( 'NONE',  ( 38.13393739769620083, -15.61618894467929941, -11.65000000000000036 ) ) ;
#4686 = AXIS2_PLACEMENT_3D ( 'NONE', #42969, #7065, #31135 ) ;
#4687 = EDGE_LOOP ( 'NONE', ( #16161, #11162, #14067, #13168, #7804, #45026, #23795, #41306, #40315, #4026, #17541, #8817, #48344 ) ) ;
#4688 = CARTESIAN_POINT ( 'NONE',  ( 0.7917425790954289999, -51.06248658143009322, -34.07803169642789953 ) ) ;
#4689 = AXIS2_PLACEMENT_3D ( 'NONE', #50977, #18740, #18486 ) ;
#4690 = CARTESIAN_POINT ( 'NONE',  ( 11.10555363379370064, -63.31361069873520364, -44.25268286828919884 ) ) ;
#4691 = DIRECTION ( 'NONE',  ( 1.000000000000000000, 0.000000000000000000, 0.000000000000000000 ) ) ;
#4692 = CARTESIAN_POINT ( 'NONE',  ( 14.28038400710302724, 1.354373803797940035, -34.79644660940672907 ) ) ;
#4693 = CARTESIAN_POINT ( 'NONE',  ( 50.32395457461500143, -49.73758701539929916, -76.14999999999999147 ) ) ;
#4694 = CARTESIAN_POINT ( 'NONE',  ( 72.83393739769620367, 0.8838110553206759423, -68.50657137141709541 ) ) ;
#4695 = ORIENTED_EDGE ( 'NONE', *, *, #47943, .T. ) ;
#4696 = FACE_OUTER_BOUND ( 'NONE', #37476, .T. ) ;
#4697 = FACE_OUTER_BOUND ( 'NONE', #33299, .T. ) ;
#4698 = ORIENTED_EDGE ( 'NONE', *, *, #4678, .F. ) ;
#4699 = DIRECTION ( 'NONE',  ( 0.6339889056055382222, 0.000000000000000000, -0.7733421413379021336 ) ) ;
#4700 = CARTESIAN_POINT ( 'NONE',  ( 29.11900864776890074, -26.73446727828369873, -35.02873218748179340 ) ) ;
#4701 = EDGE_CURVE ( 'NONE', #15133, #12469, #22280, .T. ) ;
#4702 = CARTESIAN_POINT ( 'NONE',  ( 24.23411650087799885, -17.15561044391580126, -75.85211268767397996 ) ) ;
#4703 = CARTESIAN_POINT ( 'NONE',  ( 52.84698449767209638, -49.68627056466029757, -48.96050383872009348 ) ) ;
#4704 = CARTESIAN_POINT ( 'NONE',  ( 22.90065884458136480, -15.61618680935524317, -64.84717769963093303 ) ) ;
#4705 = CARTESIAN_POINT ( 'NONE',  ( 54.83350709104630027, 19.86271698526680041, -75.27563804332019970 ) ) ;
#4706 = CARTESIAN_POINT ( 'NONE',  ( 46.74688800147040268, -53.53748093643939399, -76.01521976086429788 ) ) ;
#4707 = VERTEX_POINT ( 'NONE', #29220 ) ;
#4708 = CARTESIAN_POINT ( 'NONE',  ( 17.01975004494453714, -22.38318688418750213, -36.91115206468915488 ) ) ;
#4709 = CARTESIAN_POINT ( 'NONE',  ( 18.99729670757870181, -22.49426042349189814, -60.60709014237919234 ) ) ;
#4710 = CARTESIAN_POINT ( 'NONE',  ( 53.55249253148920019, -49.41945639387319744, -49.22526694372639611 ) ) ;
#4711 = DIRECTION ( 'NONE',  ( 0.000000000000000000, 0.000000000000000000, -1.000000000000000000 ) ) ;
#4712 = CARTESIAN_POINT ( 'NONE',  ( 54.63655381128389621, -48.05296878824569973, -26.73577887340519865 ) ) ;
#4713 = AXIS2_PLACEMENT_3D ( 'NONE', #7079, #23029, #3146 ) ;
#4714 = CARTESIAN_POINT ( 'NONE',  ( 46.39783855510299304, 21.74930147051340157, -76.14870548336060097 ) ) ;
#4715 = CARTESIAN_POINT ( 'NONE',  ( 19.75782039012221603, -54.33761034372771093, -17.50926154277789948 ) ) ;
#4716 = CARTESIAN_POINT ( 'NONE',  ( 63.02122824129657630, -31.65172625870799195, -17.11446970408973201 ) ) ;
#4717 = EDGE_CURVE ( 'NONE', #39634, #49564, #51006, .T. ) ;
#4718 = CARTESIAN_POINT ( 'NONE',  ( 12.26572565712310059, 33.38422248552610228, -15.83807272485699968 ) ) ;
#4719 = VECTOR ( 'NONE', #36360, 1000.000000000000000 ) ;
#4720 = CARTESIAN_POINT ( 'NONE',  ( 53.63393739769619373, -63.11618894467929408, 11.84999999999999964 ) ) ;
#4721 = ADVANCED_FACE ( 'NONE', ( #10885 ), #3309, .F. ) ;
#4722 = CIRCLE ( 'NONE', #30557, 2.000000000000001776 ) ;
#4723 = DIRECTION ( 'NONE',  ( 1.000000000000000000, 0.000000000000000000, 0.000000000000000000 ) ) ;
#4724 = CARTESIAN_POINT ( 'NONE',  ( 38.67452568954060155, 6.328436186825679322, -81.65000000000000568 ) ) ;
#4725 = CARTESIAN_POINT ( 'NONE',  ( 63.27605356278090198, 1.264489825601020190, -68.89055226466270199 ) ) ;
#4726 = CARTESIAN_POINT ( 'NONE',  ( 61.45294235306059960, 13.92837752391369932, -46.41419044209769851 ) ) ;
#4727 = CARTESIAN_POINT ( 'NONE',  ( 23.04646983122121284, -11.63207477299024717, -79.34100340100883386 ) ) ;
#4728 = CARTESIAN_POINT ( 'NONE',  ( -18.46512919571979694, -52.41504996104650616, -54.23003070569399853 ) ) ;
#4729 = ORIENTED_EDGE ( 'NONE', *, *, #45631, .T. ) ;
#4730 = CARTESIAN_POINT ( 'NONE',  ( 52.82298710676560205, -49.66654477726660843, -48.69818472591780534 ) ) ;
#4731 = DIRECTION ( 'NONE',  ( -0.3294064756440890918, 0.9441882088883233326, 0.000000000000000000 ) ) ;
#4732 = CARTESIAN_POINT ( 'NONE',  ( 48.31044912363459787, -54.24991223489359982, -55.31379430672990338 ) ) ;
#4733 = CARTESIAN_POINT ( 'NONE',  ( 56.41325250503939515, 14.84688818548599976, -26.18647423063130120 ) ) ;
#4734 = CARTESIAN_POINT ( 'NONE',  ( 10.21265337833550113, -11.78461560499999905, -35.63563296679929948 ) ) ;
#4735 = CARTESIAN_POINT ( 'NONE',  ( 51.01140993929779910, 18.25269707675350261, -76.32135044011170066 ) ) ;
#4736 = CARTESIAN_POINT ( 'NONE',  ( 53.19189966491499888, 18.24357405876429894, -48.89717422996369578 ) ) ;
#4737 = CARTESIAN_POINT ( 'NONE',  ( 71.40893329644839582, 0.8879664753683469414, -70.67740027405400838 ) ) ;
#4738 = CYLINDRICAL_SURFACE ( 'NONE', #15871, 1.999999999999999112 ) ;
#4739 = DIRECTION ( 'NONE',  ( 0.000000000000000000, -1.000000000000000000, 0.000000000000000000 ) ) ;
#4740 = ORIENTED_EDGE ( 'NONE', *, *, #43940, .T. ) ;
#4741 = CARTESIAN_POINT ( 'NONE',  ( 62.63393739769619373, -63.11618894467939356, 11.84999999999999964 ) ) ;
#4742 = CARTESIAN_POINT ( 'NONE',  ( 8.683925679600550396, -15.55278753634380173, -60.07005151547389943 ) ) ;
#4743 = CARTESIAN_POINT ( 'NONE',  ( 73.10713808934470137, 0.9971903505820729485, -68.99379187066199393 ) ) ;
#4744 = CARTESIAN_POINT ( 'NONE',  ( 47.56760501474590086, -54.55410667736709485, -54.80386054826420406 ) ) ;
#4745 = CARTESIAN_POINT ( 'NONE',  ( 13.95270971513190084, -8.909117678376349048, -68.24709530556648929 ) ) ;
#4746 = CARTESIAN_POINT ( 'NONE',  ( 72.85271889401160195, 1.383136297697689976, -62.73294707603399445 ) ) ;
#4747 = CARTESIAN_POINT ( 'NONE',  ( 42.29536634374500181, 11.94537196368429832, -3.241362035758810212 ) ) ;
#4748 = CARTESIAN_POINT ( 'NONE',  ( 57.15466225109279463, 18.99064698095470405, -52.70648794892409938 ) ) ;
#4749 = CARTESIAN_POINT ( 'NONE',  ( 71.42252419164299226, 1.263738073398980033, -60.81786852648419028 ) ) ;
#4750 = FACE_OUTER_BOUND ( 'NONE', #30338, .T. ) ;
#4751 = CARTESIAN_POINT ( 'NONE',  ( 71.96129531186480222, 1.170697810385400217, -61.07138367721960037 ) ) ;
#4752 = AXIS2_PLACEMENT_3D ( 'NONE', #37533, #25205, #40949 ) ;
#4753 = DIRECTION ( 'NONE',  ( -1.000000000000000000, 0.000000000000000000, 0.000000000000000000 ) ) ;
#4754 = CARTESIAN_POINT ( 'NONE',  ( 65.11408845474450402, 1.278021359705819870, -70.61864533961639268 ) ) ;
#4755 = ORIENTED_EDGE ( 'NONE', *, *, #16219, .T. ) ;
#4756 = VERTEX_POINT ( 'NONE', #30515 ) ;
#4757 = CARTESIAN_POINT ( 'NONE',  ( 17.16943767478000638, -7.705182206336107953, -55.33398825597025450 ) ) ;
#4758 = CARTESIAN_POINT ( 'NONE',  ( 68.13393739769627189, -15.41618894467850254, -103.0993275156849194 ) ) ;
#4759 = ORIENTED_EDGE ( 'NONE', *, *, #8913, .F. ) ;
#4760 = CARTESIAN_POINT ( 'NONE',  ( 12.10067367342139910, -65.23675915737399578, -45.96376737918109967 ) ) ;
#4761 = CARTESIAN_POINT ( 'NONE',  ( 16.13393739769620083, -15.61618894467929941, -22.14999999999999858 ) ) ;
#4762 = CARTESIAN_POINT ( 'NONE',  ( 9.366859039486531202, -15.61635947376150035, -49.45282021618999835 ) ) ;
#4763 = CARTESIAN_POINT ( 'NONE',  ( 52.64727086977080006, 19.37578117508699904, -76.52291747780199671 ) ) ;
#4764 = VERTEX_POINT ( 'NONE', #18985 ) ;
#4765 = DIRECTION ( 'NONE',  ( 1.000000000000000000, 0.000000000000000000, 0.000000000000000000 ) ) ;
#4766 = CARTESIAN_POINT ( 'NONE',  ( 42.31162289222356776, 6.440951911319115375, -78.76157231913752810 ) ) ;
#4767 = VECTOR ( 'NONE', #13403, 1000.000000000000000 ) ;
#4768 = CARTESIAN_POINT ( 'NONE',  ( 37.63393739769591662, -15.61618894467939711, -10.44999999999999929 ) ) ;
#4769 = EDGE_CURVE ( 'NONE', #31549, #43692, #43204, .T. ) ;
#4770 = CARTESIAN_POINT ( 'NONE',  ( 10.32617582395110034, -21.46876321233829898, -46.54110819413470068 ) ) ;
#4771 = EDGE_CURVE ( 'NONE', #45496, #21348, #31301, .T. ) ;
#4772 = CARTESIAN_POINT ( 'NONE',  ( 16.13393739769620083, -15.61618894467929941, 8.349999999999999645 ) ) ;
#4773 = CARTESIAN_POINT ( 'NONE',  ( 43.25224801953689990, -37.81438149150337580, -74.05839184249462903 ) ) ;
#4774 = EDGE_CURVE ( 'NONE', #31931, #24462, #23372, .T. ) ;
#4775 = VERTEX_POINT ( 'NONE', #42069 ) ;
#4776 = CARTESIAN_POINT ( 'NONE',  ( 12.55603873008839955, -65.48958817767790208, -23.08740377524289755 ) ) ;
#4777 = CARTESIAN_POINT ( 'NONE',  ( 9.603064799516298322, -19.96764128708570141, -80.82541145414208472 ) ) ;
#4778 = CARTESIAN_POINT ( 'NONE',  ( 40.72222893655849418, 14.05123486567899960, -5.660115700743969747 ) ) ;
#4779 = CARTESIAN_POINT ( 'NONE',  ( 14.80888071766799996, 21.59920855125570327, -76.12873484255680978 ) ) ;
#4780 = CARTESIAN_POINT ( 'NONE',  ( 64.93393739769619799, 1.883811055320669947, -69.84999999999999432 ) ) ;
#4781 = CARTESIAN_POINT ( 'NONE',  ( 83.71081252132769634, -44.47204336813729952, -46.63777445865510174 ) ) ;
#4782 = CARTESIAN_POINT ( 'NONE',  ( 10.96947365134820629, 33.83317469089056573, -17.60046481885576952 ) ) ;
#4783 = CARTESIAN_POINT ( 'NONE',  ( 18.99083791357429973, -23.35058227262370067, -49.89504055825069884 ) ) ;
#4784 = EDGE_CURVE ( 'NONE', #21587, #12629, #43494, .T. ) ;
#4785 = EDGE_LOOP ( 'NONE', ( #7919, #39560 ) ) ;
#4786 = CARTESIAN_POINT ( 'NONE',  ( 52.93377756553670110, -49.56154788943119627, -27.74629457784710240 ) ) ;
#4787 = CARTESIAN_POINT ( 'NONE',  ( 14.30960224998150032, -51.11619537004450109, -22.40439468542479773 ) ) ;
#4788 = CARTESIAN_POINT ( 'NONE',  ( 76.10260541693969571, 10.92673604474729920, -13.51091013548749942 ) ) ;
#4789 = CARTESIAN_POINT ( 'NONE',  ( 11.13393739769619906, 24.07008072128950005, -24.15000000000000213 ) ) ;
#4790 = LINE ( 'NONE', #44620, #29645 ) ;
#4791 = DIRECTION ( 'NONE',  ( -1.000000000000000000, 0.000000000000000000, 0.000000000000000000 ) ) ;
#4792 = ORIENTED_EDGE ( 'NONE', *, *, #47727, .T. ) ;
#4793 = CARTESIAN_POINT ( 'NONE',  ( -3.467811284925150339, -48.61559609778869628, -5.474417138839919872 ) ) ;
#4794 = CARTESIAN_POINT ( 'NONE',  ( 47.37190771255519905, 23.43321186050379978, -54.63786165043430287 ) ) ;
#4795 = CIRCLE ( 'NONE', #22365, 0.9999999999999964473 ) ;
#4796 = CARTESIAN_POINT ( 'NONE',  ( 13.13393739769600010, 18.38381105532060289, -83.01107220193038927 ) ) ;
#4797 = CARTESIAN_POINT ( 'NONE',  ( 63.28287142701680068, 1.331842543267529821, -62.59469824041600816 ) ) ;
#4798 = CARTESIAN_POINT ( 'NONE',  ( 71.83393739769618946, 10.88381105532070059, -62.44999999999999574 ) ) ;
#4799 = CARTESIAN_POINT ( 'NONE',  ( 11.08386349027339968, 33.85827347894340278, -17.36951630520609768 ) ) ;
#4800 = FACE_OUTER_BOUND ( 'NONE', #5727, .T. ) ;
#4801 = CARTESIAN_POINT ( 'NONE',  ( 18.20465301297571159, -7.911099042431281703, -61.37566303211916363 ) ) ;
#4802 = DIRECTION ( 'NONE',  ( 0.000000000000000000, -1.000000000000000000, 0.000000000000000000 ) ) ;
#4803 = CARTESIAN_POINT ( 'NONE',  ( 59.53476406250169362, -46.29126728519970158, -47.84522406268589378 ) ) ;
#4804 = CARTESIAN_POINT ( 'NONE',  ( 68.13393739769841773, -50.61618894467878960, -73.25000000000220268 ) ) ;
#4805 = CARTESIAN_POINT ( 'NONE',  ( 64.75883903758510485, 0.9989215084294049696, -60.69776330465320058 ) ) ;
#4806 = CARTESIAN_POINT ( 'NONE',  ( 17.48526846705000182, -52.41676442117930179, -76.03098605356829864 ) ) ;
#4807 = CARTESIAN_POINT ( 'NONE',  ( 0.8878875035446542885, -15.61618894467929763, -7.101316701949489385 ) ) ;
#4808 = CARTESIAN_POINT ( 'NONE',  ( 11.93488811383480019, -65.43955691952199061, -17.90291648171000105 ) ) ;
#4809 = CARTESIAN_POINT ( 'NONE',  ( 48.37121793203289855, 13.88381105532070059, -9.155085387781159767 ) ) ;
#4810 = ORIENTED_EDGE ( 'NONE', *, *, #31046, .T. ) ;
#4811 = CARTESIAN_POINT ( 'NONE',  ( 68.13393739769620083, 16.88381105532069881, -67.99999999999998579 ) ) ;
#4812 = CARTESIAN_POINT ( 'NONE',  ( 9.737940527390820833, 31.99035019930730073, -46.29782643814709786 ) ) ;
#4813 = CARTESIAN_POINT ( 'NONE',  ( 11.13393739769619906, -63.11543068638779630, -43.74348518090240390 ) ) ;
#4814 = CARTESIAN_POINT ( 'NONE',  ( 67.77843577628229355, -31.93894155608530028, -18.45138847496160039 ) ) ;
#4815 = ORIENTED_EDGE ( 'NONE', *, *, #49750, .T. ) ;
#4816 = CARTESIAN_POINT ( 'NONE',  ( 18.41048271170079786, 20.19843276291189937, -74.93307507168100301 ) ) ;
#4817 = ORIENTED_EDGE ( 'NONE', *, *, #22288, .T. ) ;
#4818 = ORIENTED_EDGE ( 'NONE', *, *, #3789, .T. ) ;
#4819 = ORIENTED_EDGE ( 'NONE', *, *, #513, .T. ) ;
#4820 = CARTESIAN_POINT ( 'NONE',  ( 11.03295843064409887, -64.45566759814450108, -45.85509474990620049 ) ) ;
#4821 = DIRECTION ( 'NONE',  ( 0.3294064756441309472, 0.9441882088883087887, 3.053113317719179500E-16 ) ) ;
#4822 = CARTESIAN_POINT ( 'NONE',  ( 20.78638485713110029, -20.82189247438619972, -81.23899999999999011 ) ) ;
#4823 = DIRECTION ( 'NONE',  ( -0.6522074047277892639, -0.2731766849828938248, 0.7071067811865464625 ) ) ;
#4824 = CARTESIAN_POINT ( 'NONE',  ( 61.65692969715129834, 13.95730600902359875, -46.91096927817520168 ) ) ;
#4825 = B_SPLINE_CURVE_WITH_KNOTS ( 'NONE', 3,
 ( #12810, #20902, #49489, #24557, #24300, #29030, #48973, #40316 ),
 .UNSPECIFIED., .F., .F.,
 ( 4, 2, 2, 4 ),
 ( 0.000000000000000000, 0.1882768039131864080, 0.3749999999922790650, 0.5000003605016758446 ),
 .UNSPECIFIED. ) ;
#4826 = ORIENTED_EDGE ( 'NONE', *, *, #40807, .T. ) ;
#4827 = DIRECTION ( 'NONE',  ( 0.000000000000000000, 0.000000000000000000, -1.000000000000000000 ) ) ;
#4828 = B_SPLINE_SURFACE_WITH_KNOTS ( 'NONE', 3, 3, ( 
 ( #44571, #20194, #8163, #45093, #4477, #9200, #16276, #40639, #5007, #31980 ),
 ( #25152, #1065, #36434, #28572, #17061, #8420, #48252, #41157, #21221, #40127 ),
 ( #28312, #12099, #33014, #16797, #20704, #36695, #5270, #4220, #8672, #44837 ),
 ( #795, #28832, #20447, #13145, #292, #47999, #24368, #47, #16024, #29095 ),
 ( #28055, #44311, #40381, #44057, #24106, #36184, #32229, #32745, #49037, #48772 ),
 ( #12876, #12346, #542, #8943, #16528, #32478, #48508, #24885, #40897, #4737 ),
 ( #12609, #20967, #36968, #42127, #50510, #18262, #9461, #1330, #26117, #33282 ),
 ( #37233, #50253, #49299, #17318, #13395, #19041, #18530, #38721, #15121, #14341 ),
 ( #38449, #22957, #46589, #30310, #46331, #26633, #2288, #46850, #29353, #14600 ),
 ( #10418, #45359, #11197, #6227, #26371, #22183, #7008, #31080, #42387, #6484 ),
 ( #38193, #22442, #27158, #2552, #3073, #10937, #34503, #30568, #26903, #10678 ),
 ( #42650, #6748, #22705, #43166, #51021, #2816, #34761, #50766, #38979, #30822 ),
 ( #42910, #35017, #47108, #7260, #15893, #47361, #8282, #20315, #24230, #31590 ),
 ( #166, #51541, #51790, #28180, #27927, #36056, #43929, #15638, #44182, #23976 ),
 ( #3327, #47869, #19562, #43420, #35286, #47611, #7520, #20063, #35551, #40255 ),
 ( #23727, #32358, #39743, #4089, #11712, #3589, #39229, #51284, #35806, #4347 ) ),
 .UNSPECIFIED., .F., .F., .F.,
 ( 4, 2, 2, 2, 2, 2, 2, 4 ),
 ( 4, 1, 1, 1, 1, 1, 1, 4 ),
 ( -1.891009999999999936E-14, 0.07216186899279498912, 0.1546325764131530056, 0.2061767685508769932, 0.2319488646197390147, 0.2731842183299179605, 0.3391607842662049954, 0.4123535371017729712 ),
 ( 0.000000000000000000, 0.1428571428571430157, 0.2857142857142860315, 0.4285714285714289917, 0.5714285714285709528, 0.7142857142857139685, 0.8571428571428569843, 1.000000000000000000 ),
 .UNSPECIFIED. ) ;
#4829 = CARTESIAN_POINT ( 'NONE',  ( 22.90012820302155205, -16.52286888951047317, -34.88983980414008812 ) ) ;
#4830 = VERTEX_POINT ( 'NONE', #46538 ) ;
#4831 = CARTESIAN_POINT ( 'NONE',  ( 47.78347364068760328, -46.15536227680040327, -10.88058668116050143 ) ) ;
#4832 = EDGE_CURVE ( 'NONE', #21944, #39379, #8754, .T. ) ;
#4833 = CARTESIAN_POINT ( 'NONE',  ( 61.51122975691189509, -45.14516155341349446, -46.37203261889099792 ) ) ;
#4834 = CARTESIAN_POINT ( 'NONE',  ( 22.90093739769620029, -15.61618894467913243, -28.45282021618999835 ) ) ;
#4835 = EDGE_CURVE ( 'NONE', #6855, #8577, #15062, .T. ) ;
#4836 = ORIENTED_EDGE ( 'NONE', *, *, #3385, .T. ) ;
#4837 = VERTEX_POINT ( 'NONE', #6954 ) ;
#4838 = DIRECTION ( 'NONE',  ( 0.000000000000000000, 0.000000000000000000, 1.000000000000000000 ) ) ;
#4839 = CARTESIAN_POINT ( 'NONE',  ( 62.88393739769619373, 11.88381105532070059, -84.94863984844531046 ) ) ;
#4840 = LINE ( 'NONE', #25254, #34555 ) ;
#4841 = AXIS2_PLACEMENT_3D ( 'NONE', #7105, #43008, #22283 ) ;
#4842 = CARTESIAN_POINT ( 'NONE',  ( 45.14275768348990425, 14.67924369193939960, -8.929573269535710622 ) ) ;
#4843 = CIRCLE ( 'NONE', #36619, 2.999999999999994227 ) ;
#4844 = CARTESIAN_POINT ( 'NONE',  ( 46.98749078828947034, 4.883811055320659733, -34.79644660940672907 ) ) ;
#4845 = CARTESIAN_POINT ( 'NONE',  ( 11.53606103740170674, 24.11867657901759188, -21.73577486392030167 ) ) ;
#4846 = CARTESIAN_POINT ( 'NONE',  ( 55.57909954016480469, 14.75263197375267765, -16.80477431159009782 ) ) ;
#4847 = CARTESIAN_POINT ( 'NONE',  ( 22.32699604808950156, -20.43622761008139932, -59.49802510748859419 ) ) ;
#4848 = EDGE_CURVE ( 'NONE', #51191, #12580, #3940, .T. ) ;
#4849 = ORIENTED_EDGE ( 'NONE', *, *, #13792, .F. ) ;
#4850 = CARTESIAN_POINT ( 'NONE',  ( 58.92301001618189815, 15.23611622987800018, -47.52857555498080444 ) ) ;
#4851 = CARTESIAN_POINT ( 'NONE',  ( 11.36895924000850044, 33.23916916644579800, -44.41074867359769485 ) ) ;
#4852 = ADVANCED_FACE ( 'NONE', ( #45747 ), #51487, .T. ) ;
#4853 = CARTESIAN_POINT ( 'NONE',  ( 72.20074884524329661, 1.275252243133929930, -69.97672534177469572 ) ) ;
#4854 = CARTESIAN_POINT ( 'NONE',  ( 41.52003636951408794, -39.71129688314757544, -78.64757901482110469 ) ) ;
#4855 = CARTESIAN_POINT ( 'NONE',  ( 48.42521416700790127, -56.37491125791819968, -74.14999999999999147 ) ) ;
#4856 = CARTESIAN_POINT ( 'NONE',  ( 72.31796842074339793, 1.033013263524880099, -69.95125361163771061 ) ) ;
#4857 = B_SPLINE_CURVE_WITH_KNOTS ( 'NONE', 3,
 ( #45852, #26163, #46118, #9937, #13622, #10464, #30092, #42697, #33518, #25898, #14387 ),
 .UNSPECIFIED., .F., .F.,
 ( 4, 1, 1, 1, 1, 1, 1, 1, 4 ),
 ( 0.000000000000000000, 0.0002423770808862299518, 0.07946130814449685331, 0.1586802392081063384, 0.2378991702717181134, 0.3171181013353275846, 0.3963370323989381938, 0.4755559634625476928, 0.5000037312039752324 ),
 .UNSPECIFIED. ) ;
#4858 = CARTESIAN_POINT ( 'NONE',  ( 47.07822479275279903, 23.33748360234629970, -75.12259518105788914 ) ) ;
#4859 = CARTESIAN_POINT ( 'NONE',  ( 48.84430051460839906, -53.91533838276139790, -54.66094892452610310 ) ) ;
#4860 = CARTESIAN_POINT ( 'NONE',  ( -2.927827710953269769, 17.96742650791509988, -5.740515240579870060 ) ) ;
#4861 = CARTESIAN_POINT ( 'NONE',  ( 23.80906457898844053, -17.59608236765743428, -33.58805050710569873 ) ) ;
#4862 = CARTESIAN_POINT ( 'NONE',  ( 68.77953295920740118, -25.01418894467940035, -65.18094736867061556 ) ) ;
#4863 = CARTESIAN_POINT ( 'NONE',  ( 23.62413055734869971, -48.75525398023999912, -35.14999999999999858 ) ) ;
#4864 = ORIENTED_EDGE ( 'NONE', *, *, #8510, .F. ) ;
#4865 = CARTESIAN_POINT ( 'NONE',  ( 10.35842378612870007, -20.32258213489830112, -41.84969737084129093 ) ) ;
#4866 = CARTESIAN_POINT ( 'NONE',  ( 64.12726891144080810, 1.458412159422780130, -61.50690654180700534 ) ) ;
#4867 = VERTEX_POINT ( 'NONE', #11401 ) ;
#4868 = DIRECTION ( 'NONE',  ( 0.000000000000000000, -1.000000000000000000, 0.000000000000000000 ) ) ;
#4869 = CARTESIAN_POINT ( 'NONE',  ( 61.23319982858109967, -45.48283502369449849, -47.51874276278909548 ) ) ;
#4870 = CARTESIAN_POINT ( 'NONE',  ( 8.222919723998259656, -14.85903073721773993, -80.82280372480568076 ) ) ;
#4871 = CARTESIAN_POINT ( 'NONE',  ( 12.22498197106229867, 18.79317372273670017, -21.14999999999999858 ) ) ;
#4872 = CARTESIAN_POINT ( 'NONE',  ( 41.42126661153417189, 8.467416272844669578, -79.12460387921866811 ) ) ;
#4873 = CARTESIAN_POINT ( 'NONE',  ( 28.63393739769619728, -8.399310579809030841, -34.64999999999999858 ) ) ;
#4874 = FACE_OUTER_BOUND ( 'NONE', #39965, .T. ) ;
#4875 = EDGE_LOOP ( 'NONE', ( #25712, #23871, #69, #2308 ) ) ;
#4876 = CARTESIAN_POINT ( 'NONE',  ( 83.36355911687300591, -45.34682523223490591, -47.55049236202179230 ) ) ;
#4877 = B_SPLINE_CURVE_WITH_KNOTS ( 'NONE', 3,
 ( #26076, #50208, #10639, #2507, #14820, #18488, #6187, #46288, #30527, #42870, #6705, #22662 ),
 .UNSPECIFIED., .F., .F.,
 ( 4, 1, 1, 1, 1, 1, 1, 1, 1, 4 ),
 ( 0.000000000000000000, 0.1111152296621469165, 0.2222304593242938331, 0.3333456889864405137, 0.4444609186485874441, 0.5555761483107353182, 0.6666913779728821376, 0.7778066076350290681, 0.8889218372971758875, 1.000000000000000000 ),
 .UNSPECIFIED. ) ;
#4878 = ORIENTED_EDGE ( 'NONE', *, *, #11252, .T. ) ;
#4879 = ORIENTED_EDGE ( 'NONE', *, *, #19390, .F. ) ;
#4880 = ORIENTED_EDGE ( 'NONE', *, *, #1937, .T. ) ;
#4881 = DIRECTION ( 'NONE',  ( 0.000000000000000000, -1.000000000000000000, 0.000000000000000000 ) ) ;
#4882 = CARTESIAN_POINT ( 'NONE',  ( 52.90396775623960224, -49.66420589288500054, -49.02012042725169749 ) ) ;
#4883 = CARTESIAN_POINT ( 'NONE',  ( 60.84441632817985379, 14.22943762888878005, -47.04815909370046256 ) ) ;
#4884 = CARTESIAN_POINT ( 'NONE',  ( 76.40750186186460269, -10.73206780545592487, -12.82882999751005393 ) ) ;
#4885 = CARTESIAN_POINT ( 'NONE',  ( 55.75774054045910333, -51.07765005165450134, -53.93517881746969778 ) ) ;
#4886 = VERTEX_POINT ( 'NONE', #39437 ) ;
#4887 = EDGE_LOOP ( 'NONE', ( #26863, #36509, #18735, #27371 ) ) ;
#4888 = CARTESIAN_POINT ( 'NONE',  ( 49.00556831830410687, 22.49847617784580223, -54.36652964084350259 ) ) ;
#4889 = CARTESIAN_POINT ( 'NONE',  ( -7.203365501241526303, 15.66981567447505519, -41.43129459776488233 ) ) ;
#4890 = CARTESIAN_POINT ( 'NONE',  ( 14.62183896472512323, 18.38379308823580516, -83.18933379704752440 ) ) ;
#4891 = EDGE_CURVE ( 'NONE', #18307, #16420, #47055, .T. ) ;
#4892 = CARTESIAN_POINT ( 'NONE',  ( 8.792282373222519709, -63.15413706425750462, -46.67070408018280148 ) ) ;
#4893 = CARTESIAN_POINT ( 'NONE',  ( 62.74890333807501008, 0.2393393690175290023, -16.93594147870210165 ) ) ;
#4894 = B_SPLINE_CURVE_WITH_KNOTS ( 'NONE', 3,
 ( #21443, #8897, #8633, #1542, #48467, #4958, #33238, #16489, #49255, #12569, #24583, #29056, #37441, #36392, #37189, #28531, #45312, #44532 ),
 .UNSPECIFIED., .F., .F.,
 ( 4, 2, 2, 2, 2, 2, 2, 2, 4 ),
 ( 0.4999961881505365913, 0.5624966646317195451, 0.6249971411129024990, 0.6874976175940853418, 0.7499980940752682956, 0.8124985705564512495, 0.8749990470376340923, 0.9374995235188170462, 1.000000000000000000 ),
 .UNSPECIFIED. ) ;
#4895 = CARTESIAN_POINT ( 'NONE',  ( 71.62484648860579739, 0.9098571636355720083, -60.77008670988870165 ) ) ;
#4896 = ORIENTED_EDGE ( 'NONE', *, *, #13025, .T. ) ;
#4897 = CARTESIAN_POINT ( 'NONE',  ( -2.235188499061480538, 18.67038793989973655, -5.998756751858821623 ) ) ;
#4898 = CARTESIAN_POINT ( 'NONE',  ( -5.833909485681573415, -15.61618894467930119, 5.729250452415290518 ) ) ;
#4899 = CARTESIAN_POINT ( 'NONE',  ( 22.85640968062299194, -16.50885056875128498, -46.49478737242424131 ) ) ;
#4900 = CARTESIAN_POINT ( 'NONE',  ( 60.42907245139279837, 14.44704792307930141, -47.19657908371780053 ) ) ;
#4901 = CARTESIAN_POINT ( 'NONE',  ( 23.23545949276009992, -12.27625907641840008, -63.87256020652749555 ) ) ;
#4902 = CARTESIAN_POINT ( 'NONE',  ( 24.04493739769619864, -15.61618894467929941, -32.14999999999999858 ) ) ;
#4903 = CARTESIAN_POINT ( 'NONE',  ( 41.18706455731800276, -44.61555498641789796, -5.042666981957509620 ) ) ;
#4904 = CARTESIAN_POINT ( 'NONE',  ( 17.92370450347650035, -51.11618894467930119, -15.67980085856620143 ) ) ;
#4905 = CARTESIAN_POINT ( 'NONE',  ( 68.13393739769840352, -50.61618894467879670, -73.25000000000220268 ) ) ;
#4906 = CARTESIAN_POINT ( 'NONE',  ( 68.13393739769618662, 0.9838110553206419473, -65.65000000000000568 ) ) ;
#4907 = CIRCLE ( 'NONE', #17481, 5.251829701412240148 ) ;
#4908 = CARTESIAN_POINT ( 'NONE',  ( 64.09336526242300636, 1.458407755040209919, -69.75916877191829713 ) ) ;
#4909 = DIRECTION ( 'NONE',  ( 0.000000000000000000, 0.000000000000000000, -1.000000000000000000 ) ) ;
#4910 = VECTOR ( 'NONE', #31415, 1000.000000000000114 ) ;
#4911 = CARTESIAN_POINT ( 'NONE',  ( 66.02286391504910057, 1.436401451597350221, -18.53624686056960158 ) ) ;
#4912 = ORIENTED_EDGE ( 'NONE', *, *, #21269, .T. ) ;
#4913 = CARTESIAN_POINT ( 'NONE',  ( 14.54748625655889960, -51.81226317974009987, -75.66803551354809088 ) ) ;
#4915 = CIRCLE ( 'NONE', #16622, 2.000000000000000888 ) ;
#4914 = CARTESIAN_POINT ( 'NONE',  ( 47.34550006616409945, -54.68667022654160803, -54.66557013501159901 ) ) ;
#4916 = EDGE_CURVE ( 'NONE', #44194, #35613, #4980, .T. ) ;
#4917 = CARTESIAN_POINT ( 'NONE',  ( 0.2749857802900130266, 19.51618704702660168, -34.65028054350399600 ) ) ;
#4918 = CARTESIAN_POINT ( 'NONE',  ( 84.44784216359251161, 11.88381105532070059, -47.47585302082339354 ) ) ;
#4919 = CARTESIAN_POINT ( 'NONE',  ( 61.03029461452958770, -45.45771770995002470, -47.37445190977187082 ) ) ;
#4920 = CARTESIAN_POINT ( 'NONE',  ( 22.43194022673959864, -19.90881204782320069, -32.14999999999999858 ) ) ;
#4921 = CARTESIAN_POINT ( 'NONE',  ( 57.34776335324270491, 14.57942837581910034, -26.27178905609630277 ) ) ;
#4922 = CARTESIAN_POINT ( 'NONE',  ( 11.90332973438740005, 34.20450943514180153, -18.04110290859920340 ) ) ;
#4924 = CARTESIAN_POINT ( 'NONE',  ( -5.256770087461370089, -47.44903047538170426, -5.577592548843699483 ) ) ;
#4923 = CARTESIAN_POINT ( 'NONE',  ( 0.4644698840366610071, -8.836735345369399752, -34.95504743437659556 ) ) ;
#4925 = PLANE ( 'NONE',  #2470 ) ;
#4926 = CARTESIAN_POINT ( 'NONE',  ( 48.47801679748619819, 22.94615690571940192, -55.28610629251650010 ) ) ;
#4927 = ORIENTED_EDGE ( 'NONE', *, *, #35785, .T. ) ;
#4928 = CARTESIAN_POINT ( 'NONE',  ( 16.39219225208960040, -22.66429958545629830, -63.33552157962199658 ) ) ;
#4929 = ORIENTED_EDGE ( 'NONE', *, *, #2191, .F. ) ;
#4930 = CYLINDRICAL_SURFACE ( 'NONE', #32849, 1.999999999999997113 ) ;
#4931 = CARTESIAN_POINT ( 'NONE',  ( 65.19259745005730622, 1.384447124000270035, -60.97624892474630087 ) ) ;
#4932 = DIRECTION ( 'NONE',  ( -1.000000000000000000, 0.000000000000000000, 0.000000000000000000 ) ) ;
#4934 = CARTESIAN_POINT ( 'NONE',  ( 55.99380635880790180, 14.75626973559459998, -25.81789497692459889 ) ) ;
#4933 = CARTESIAN_POINT ( 'NONE',  ( 82.78852321480360388, 13.78813943271330089, -46.36931865296670452 ) ) ;
#4935 = CARTESIAN_POINT ( 'NONE',  ( 14.95389657571809927, -22.56960985492850114, -67.00632966799250312 ) ) ;
#4936 = DIRECTION ( 'NONE',  ( 4.006994122734829692E-31, -1.000000000000000000, -3.740764114965449782E-16 ) ) ;
#4937 = CARTESIAN_POINT ( 'NONE',  ( 3.755977383759285360, -24.60930330475428462, -6.649999999999999467 ) ) ;
#4938 = CYLINDRICAL_SURFACE ( 'NONE', #8869, 6.766999999999998572 ) ;
#4939 = ORIENTED_EDGE ( 'NONE', *, *, #6666, .T. ) ;
#4940 = ORIENTED_EDGE ( 'NONE', *, *, #28237, .F. ) ;
#4941 = CARTESIAN_POINT ( 'NONE',  ( 11.47551314106880049, -64.97235711416220738, -16.61573023122599935 ) ) ;
#4942 = CARTESIAN_POINT ( 'NONE',  ( 10.93332210773090019, 32.19736207414519669, -44.88523382134809481 ) ) ;
#4943 = DIRECTION ( 'NONE',  ( 0.5720614028176835841, -0.4156269377774527984, -0.7071067811865484609 ) ) ;
#4944 = CARTESIAN_POINT ( 'NONE',  ( 49.68126013218329717, -52.84574376966489950, -52.91783866924430413 ) ) ;
#4945 = DIRECTION ( 'NONE',  ( 0.000000000000000000, 1.000000000000000000, 0.000000000000000000 ) ) ;
#4946 = TOROIDAL_SURFACE ( 'NONE', #7465, 6.949999999999999289, 2.999999999999960032 ) ;
#4947 = AXIS2_PLACEMENT_3D ( 'NONE', #37990, #32999, #37215 ) ;
#4948 = VECTOR ( 'NONE', #49581, 1000.000000000000000 ) ;
#4949 = VERTEX_POINT ( 'NONE', #31796 ) ;
#4950 = CARTESIAN_POINT ( 'NONE',  ( 8.133937397696209715, 28.10308010054979988, -21.14999999999999858 ) ) ;
#4951 = CARTESIAN_POINT ( 'NONE',  ( 54.50979703755457706, 16.93725552086487340, -26.78135896009203520 ) ) ;
#4952 = FACE_OUTER_BOUND ( 'NONE', #12439, .T. ) ;
#4953 = EDGE_CURVE ( 'NONE', #51520, #51462, #15055, .T. ) ;
#4954 = CARTESIAN_POINT ( 'NONE',  ( 49.26469448778690463, 22.42219932542450067, -54.34642017524310376 ) ) ;
#4955 = CARTESIAN_POINT ( 'NONE',  ( 3.987490788289483667, -22.62894316431776787, -34.79644660940672907 ) ) ;
#4956 = CARTESIAN_POINT ( 'NONE',  ( 50.30621308613430642, -48.61618509234789798, -76.16272939236809236 ) ) ;
#4957 = EDGE_CURVE ( 'NONE', #36007, #36393, #12168, .T. ) ;
#4958 = CARTESIAN_POINT ( 'NONE',  ( 20.99561544827837167, -21.94235417058543547, -43.79935663472948448 ) ) ;
#4959 = ORIENTED_EDGE ( 'NONE', *, *, #40157, .F. ) ;
#4960 = EDGE_CURVE ( 'NONE', #15778, #32833, #13382, .T. ) ;
#4961 =( NAMED_UNIT ( * ) PLANE_ANGLE_UNIT ( ) SI_UNIT ( $, .RADIAN. ) );
#4962 = DIRECTION ( 'NONE',  ( 0.000000000000000000, 0.000000000000000000, -1.000000000000000000 ) ) ;
#4963 = VERTEX_POINT ( 'NONE', #7728 ) ;
#4964 = FACE_OUTER_BOUND ( 'NONE', #1226, .T. ) ;
#4965 = PLANE ( 'NONE',  #27012 ) ;
#4966 = ADVANCED_FACE ( 'NONE', ( #48070 ), #4290, .T. ) ;
#4967 = CARTESIAN_POINT ( 'NONE',  ( 21.06068861467879927, -9.004846484592640365, -79.49618351660039650 ) ) ;
#4968 = CARTESIAN_POINT ( 'NONE',  ( 14.12377191986709946, -51.13901785078579820, -22.60596972032639940 ) ) ;
#4969 = CARTESIAN_POINT ( 'NONE',  ( 56.57215025654439700, 19.50075534991569981, -74.14931637192330527 ) ) ;
#4970 = CARTESIAN_POINT ( 'NONE',  ( 46.79040325823919488, -53.60681267845629350, -75.98188598372340152 ) ) ;
#4971 = ORIENTED_EDGE ( 'NONE', *, *, #3081, .F. ) ;
#4972 = CARTESIAN_POINT ( 'NONE',  ( 55.38284522413690070, 14.79968809196030044, -16.52949576727229797 ) ) ;
#4973 = CARTESIAN_POINT ( 'NONE',  ( 57.25859902730019968, -50.61616371649569857, -53.75766468090039751 ) ) ;
#4974 = EDGE_CURVE ( 'NONE', #34590, #34588, #34256, .T. ) ;
#4975 = CARTESIAN_POINT ( 'NONE',  ( 9.557361903038261275, -13.06853739366259859, -31.96482487842879650 ) ) ;
#4976 = CYLINDRICAL_SURFACE ( 'NONE', #11963, 2.999999999999999112 ) ;
#4977 = CARTESIAN_POINT ( 'NONE',  ( 47.18938042008029754, 23.12896336020899923, -75.29141078596350667 ) ) ;
#4978 = CARTESIAN_POINT ( 'NONE',  ( 47.13393649688870113, -39.28050833195659663, -53.76790015415899404 ) ) ;
#4979 = EDGE_CURVE ( 'NONE', #38690, #45896, #10062, .T. ) ;
#4980 = B_SPLINE_CURVE_WITH_KNOTS ( 'NONE', 3,
 ( #16089, #39689, #7462, #23416, #19763, #27363 ),
 .UNSPECIFIED., .F., .F.,
 ( 4, 1, 1, 4 ),
 ( 0.000000000000000000, 0.3333333332445601038, 0.6666666664890206206, 1.000000000000000000 ),
 .UNSPECIFIED. ) ;
#4981 = VECTOR ( 'NONE', #38444, 1000.000000000000000 ) ;
#4982 = CARTESIAN_POINT ( 'NONE',  ( 58.92073396209919878, -28.11618894467929763, -15.65000000000000036 ) ) ;
#4983 = VECTOR ( 'NONE', #45903, 1000.000000000000000 ) ;
#4984 = FACE_OUTER_BOUND ( 'NONE', #24961, .T. ) ;
#4985 = VECTOR ( 'NONE', #43340, 1000.000000000000000 ) ;
#4986 = VECTOR ( 'NONE', #39113, 1000.000000000000000 ) ;
#4988 = AXIS2_PLACEMENT_3D ( 'NONE', #39937, #36243, #4033 ) ;
#4987 = CARTESIAN_POINT ( 'NONE',  ( 13.13486993893959998, -7.935803858833188507, -78.88916932753539868 ) ) ;
#4989 = CARTESIAN_POINT ( 'NONE',  ( 8.222732946675209931, -15.61637358666110131, -80.79233150823698395 ) ) ;
#4991 = FACE_OUTER_BOUND ( 'NONE', #43607, .T. ) ;
#4990 = LINE ( 'NONE', #8146, #29886 ) ;
#4992 = AXIS2_PLACEMENT_3D ( 'NONE', #28126, #32048, #3536 ) ;
#4993 = CARTESIAN_POINT ( 'NONE',  ( 63.16328864814500577, 1.096044978595170027, -68.93830798183888930 ) ) ;
#4994 = FACE_OUTER_BOUND ( 'NONE', #19302, .T. ) ;
#4995 = CARTESIAN_POINT ( 'NONE',  ( 8.222933577955913620, -14.58066943308473995, -68.54933528812181009 ) ) ;
#4996 = CARTESIAN_POINT ( 'NONE',  ( -12.67430703014960081, -56.52710054866469847, -51.91878751810809689 ) ) ;
#4997 = EDGE_LOOP ( 'NONE', ( #29743, #2502 ) ) ;
#4998 =( BOUNDED_CURVE ( )  B_SPLINE_CURVE ( 2, ( #19943, #39881, #8166 ),
 .UNSPECIFIED., .F., .T. ) 
 B_SPLINE_CURVE_WITH_KNOTS ( ( 3, 3 ),
 ( 2.168627590050199672, 3.232274745523169734 ),
 .UNSPECIFIED. ) 
 CURVE ( )  GEOMETRIC_REPRESENTATION_ITEM ( )  RATIONAL_B_SPLINE_CURVE ( ( 1.425426480542939967, 1.425426480542939967, 1.323085463760209857 ) ) 
 REPRESENTATION_ITEM ( '' )  );
#4999 = CARTESIAN_POINT ( 'NONE',  ( 53.32368397926410353, -49.40866304911550344, -48.89504827794529973 ) ) ;
#5000 = ADVANCED_FACE ( 'NONE', ( #20005 ), #40812, .T. ) ;
#5001 = CARTESIAN_POINT ( 'NONE',  ( 8.222524523195870572, -15.61634168869099959, -38.50766849176289952 ) ) ;
#5002 = DIRECTION ( 'NONE',  ( -1.000000000000000000, 0.000000000000000000, 0.000000000000000000 ) ) ;
#5003 = CARTESIAN_POINT ( 'NONE',  ( 56.72799476710019917, 14.59936194371569940, -26.16780803237229946 ) ) ;
#5004 = CARTESIAN_POINT ( 'NONE',  ( 12.02786555360810006, -9.881842189571759860, -39.75501738210749636 ) ) ;
#5005 = CARTESIAN_POINT ( 'NONE',  ( 51.38507389488840005, 19.29610779897900130, -76.23533787841168419 ) ) ;
#5006 = CARTESIAN_POINT ( 'NONE',  ( 52.98874186162730382, 18.36389844763469625, -48.96317217183759851 ) ) ;
#5007 = CARTESIAN_POINT ( 'NONE',  ( 71.25019707560579718, 0.9212109678634080590, -70.77727272727280194 ) ) ;
#5008 = CARTESIAN_POINT ( 'NONE',  ( 42.11778985043759604, -43.34518763914159933, -3.278435071288769542 ) ) ;
#5009 = CARTESIAN_POINT ( 'NONE',  ( 72.23296425804250021, -44.31211235131849691, -12.76840841843079843 ) ) ;
#5010 = ORIENTED_EDGE ( 'NONE', *, *, #14896, .F. ) ;
#5011 = CARTESIAN_POINT ( 'NONE',  ( 23.57566764420120009, -15.97304352090550239, -79.08259497074239164 ) ) ;
#5012 = ORIENTED_EDGE ( 'NONE', *, *, #50529, .T. ) ;
#5013 = CARTESIAN_POINT ( 'NONE',  ( 72.77520546617009245, 1.386446979194289941, -68.79214934801569825 ) ) ;
#5014 = CARTESIAN_POINT ( 'NONE',  ( 47.45216272503800070, -54.62528982994189874, -54.83349227997879893 ) ) ;
#5015 = CARTESIAN_POINT ( 'NONE',  ( -11.32734372065470119, 10.64934054434680100, -6.430561461456250072 ) ) ;
#5016 = CARTESIAN_POINT ( 'NONE',  ( 73.19748134167231512, 1.099973129953850215, -62.51484271732719833 ) ) ;
#5017 = FACE_OUTER_BOUND ( 'NONE', #23671, .T. ) ;
#5018 = CARTESIAN_POINT ( 'NONE',  ( 71.41482173131041122, 1.096036836948800053, -60.67470092284240479 ) ) ;
#5019 = LINE ( 'NONE', #13157, #32475 ) ;
#5020 = CARTESIAN_POINT ( 'NONE',  ( 72.07540109225739400, 1.000506532484820132, -61.12530190143370135 ) ) ;
#5021 = CARTESIAN_POINT ( 'NONE',  ( 66.72561048531049721, -33.11618894467940066, -20.65000000000000213 ) ) ;
#5022 = CARTESIAN_POINT ( 'NONE',  ( 64.85894149894409111, 0.8879664753683379486, -70.67740027405400838 ) ) ;
#5023 = ORIENTED_EDGE ( 'NONE', *, *, #45322, .T. ) ;
#5024 = ORIENTED_EDGE ( 'NONE', *, *, #8621, .F. ) ;
#5025 = CARTESIAN_POINT ( 'NONE',  ( 8.797781558458089179, -63.18317285479920997, -46.67022811708060459 ) ) ;
#5026 = CIRCLE ( 'NONE', #34281, 10.00000000000000711 ) ;
#5027 = LINE ( 'NONE', #20464, #33589 ) ;
#5028 = VERTEX_POINT ( 'NONE', #39120 ) ;
#5029 = CARTESIAN_POINT ( 'NONE',  ( 16.56130706594500168, -8.576308665788749508, -72.36647972087459380 ) ) ;
#5030 = CARTESIAN_POINT ( 'NONE',  ( 24.04493741779556260, -14.58064063100057339, -59.46598965420297844 ) ) ;
#5031 = CARTESIAN_POINT ( 'NONE',  ( 56.46551622901163370, 19.54378670599449919, -74.28390251812621159 ) ) ;
#5032 = AXIS2_PLACEMENT_3D ( 'NONE', #32126, #40537, #44208 ) ;
#5033 = CARTESIAN_POINT ( 'NONE',  ( 51.81517742707350749, 18.95102032179380203, -76.50774528508080152 ) ) ;
#5034 = AXIS2_PLACEMENT_3D ( 'NONE', #39017, #15420, #8068 ) ;
#5035 = ORIENTED_EDGE ( 'NONE', *, *, #9537, .F. ) ;
#5036 = CARTESIAN_POINT ( 'NONE',  ( 61.20224358684065180, 14.04196190244037368, -46.71246603851685109 ) ) ;
#5037 = CARTESIAN_POINT ( 'NONE',  ( 42.03721945691450657, 6.397288423599181151, -80.13352371291058773 ) ) ;
#5038 = CARTESIAN_POINT ( 'NONE',  ( 60.34379259250669492, 14.63564649040839960, -47.72732609510669732 ) ) ;
#5039 = CIRCLE ( 'NONE', #3349, 16.00000000000000000 ) ;
#5040 = ADVANCED_FACE ( 'NONE', ( #11339 ), #23102, .T. ) ;
#5041 = B_SPLINE_SURFACE_WITH_KNOTS ( 'NONE', 3, 3, ( 
 ( #43057, #17079, #45110, #49054, #8692, #4754, #32244, #20209, #5286, #16542 ),
 ( #28325, #813, #33029, #44074, #17336, #13163, #36197, #29111, #9216, #25170 ),
 ( #8437, #21238, #33301, #307, #28586, #40396, #24119, #41177, #28849, #32761 ),
 ( #37247, #16288, #20722, #1345, #12112, #28068, #1080, #32496, #8176, #12362 ),
 ( #48521, #48266, #24643, #44853, #40139, #36710, #4238, #44325, #24381, #4492 ),
 ( #5022, #12628, #8957, #48786, #20459, #36449, #12894, #556, #44586, #24900 ),
 ( #16814, #40655, #40913, #20987, #36983, #50074, #46419, #25685, #6314, #22271 ),
 ( #21756, #17839, #30136, #30397, #25426, #33811, #10246, #45373, #26204, #41428 ),
 ( #49824, #37501, #13661, #46159, #42215, #13916, #38544, #45892, #1601, #18098 ),
 ( #38282, #29624, #29372, #50341, #2371, #37766, #6054, #41958, #42478, #18348 ),
 ( #14427, #49315, #34325, #1860, #14169, #22012, #33560, #29872, #49577, #9978 ),
 ( #18611, #41687, #10506, #25940, #38023, #6570, #2117, #26464, #5795, #45625 ),
 ( #34064, #22532, #2643, #13410, #9479, #5545, #21500, #17588, #9725, #11799 ),
 ( #23045, #15467, #39568, #15716, #19644, #31164, #27239, #2900, #42740, #27762 ),
 ( #43757, #50850, #23293, #3675, #14684, #39824, #35637, #6838, #51622, #31674 ),
 ( #42997, #30906, #7858, #3932, #22787, #51106, #11022, #46678, #47697, #51367 ) ),
 .UNSPECIFIED., .F., .F., .F.,
 ( 4, 2, 2, 2, 2, 2, 2, 4 ),
 ( 4, 1, 1, 1, 1, 1, 1, 4 ),
 ( 0.000000000000000000, 0.07216186899278899392, 0.1546325764131200042, 0.2061767685508260062, 0.2319488646196800063, 0.2731842183298449633, 0.3391607842661090166, 0.4123535371016520124 ),
 ( 0.000000000000000000, 0.1428571428571430157, 0.2857142857142860315, 0.4285714285714289917, 0.5714285714285709528, 0.7142857142857139685, 0.8571428571428569843, 1.000000000000000000 ),
 .UNSPECIFIED. ) ;
#5042 = CARTESIAN_POINT ( 'NONE',  ( 16.18347776944520078, -7.371174341447729539, -51.29424405795199249 ) ) ;
#5043 = DIRECTION ( 'NONE',  ( 0.7800418122827239564, 0.000000000000000000, -0.6257273935913973961 ) ) ;
#5044 = CIRCLE ( 'NONE', #36812, 2.999999999999960920 ) ;
#5045 = CARTESIAN_POINT ( 'NONE',  ( 42.27252180811520788, -37.66705137823122129, -78.95707406319118604 ) ) ;
#5046 = ORIENTED_EDGE ( 'NONE', *, *, #7221, .F. ) ;
#5047 = CARTESIAN_POINT ( 'NONE',  ( 12.17383947079069983, -65.46069624394010589, -22.71972408461549975 ) ) ;
#5048 = CARTESIAN_POINT ( 'NONE',  ( 16.23152780737629897, -23.46331552995090064, -80.50853572988748397 ) ) ;
#5049 = CARTESIAN_POINT ( 'NONE',  ( 10.85080901074660176, -11.16945680538309915, -32.14999999999999858 ) ) ;
#5050 = CARTESIAN_POINT ( 'NONE',  ( 14.56816760167549951, 21.04130707244170040, -75.96082109999758814 ) ) ;
#5051 = EDGE_CURVE ( 'NONE', #15767, #18307, #15877, .T. ) ;
#5052 = CARTESIAN_POINT ( 'NONE',  ( 9.658618216099990050, -20.27044307813694601, -60.59413031184570997 ) ) ;
#5053 = CARTESIAN_POINT ( 'NONE',  ( 83.45793240077840380, -44.68224995836130375, -46.53859470524309216 ) ) ;
#5054 = CARTESIAN_POINT ( 'NONE',  ( 22.33694808633480022, -21.04807435451730058, -49.73660269612349794 ) ) ;
#5055 = ORIENTED_EDGE ( 'NONE', *, *, #42227, .T. ) ;
#5056 = CARTESIAN_POINT ( 'NONE',  ( 53.38096221179280576, -49.16063623257220172, -27.30168355108260059 ) ) ;
#5057 = CARTESIAN_POINT ( 'NONE',  ( 16.19818216287970003, -51.11138666575850209, -21.03492549854079741 ) ) ;
#5058 = CARTESIAN_POINT ( 'NONE',  ( 18.20470375856487166, -23.32126450859495748, -64.20899946892900800 ) ) ;
#5059 = CARTESIAN_POINT ( 'NONE',  ( 15.24805240113982663, -22.38317849424599970, -56.99443076857846791 ) ) ;
#5060 = DIRECTION ( 'NONE',  ( 0.000000000000000000, 0.000000000000000000, -1.000000000000000000 ) ) ;
#5061 = AXIS2_PLACEMENT_3D ( 'NONE', #46242, #45189, #42298 ) ;
#5062 = VERTEX_POINT ( 'NONE', #11861 ) ;
#5063 = AXIS2_PLACEMENT_3D ( 'NONE', #28786, #12304, #47952 ) ;
#5064 = CARTESIAN_POINT ( 'NONE',  ( -7.435201089644969841, -45.47238293868839776, -5.298195296883859484 ) ) ;
#5065 = AXIS2_PLACEMENT_3D ( 'NONE', #38936, #15342, #43128 ) ;
#5066 = CARTESIAN_POINT ( 'NONE',  ( 47.28790744643029598, 23.49698345083890061, -54.73855453374710578 ) ) ;
#5067 = EDGE_CURVE ( 'NONE', #23939, #2764, #251, .T. ) ;
#5069 = VECTOR ( 'NONE', #48799, 1000.000000000000114 ) ;
#5068 = CARTESIAN_POINT ( 'NONE',  ( 22.19151943370611946, 22.78899166960877309, -34.82441657595546758 ) ) ;
#5070 = CARTESIAN_POINT ( 'NONE',  ( 63.19277908840750513, 0.9325382164350239922, -62.24624853760359855 ) ) ;
#5071 = VECTOR ( 'NONE', #25438, 1000.000000000000000 ) ;
#5072 = CARTESIAN_POINT ( 'NONE',  ( 42.35079399890570784, 13.08996448889170061, -5.113119482875689847 ) ) ;
#5073 = CARTESIAN_POINT ( 'NONE',  ( 9.367491665984019278, -15.61623476897930018, -53.45282021618999124 ) ) ;
#5074 = FACE_OUTER_BOUND ( 'NONE', #22721, .T. ) ;
#5075 = CARTESIAN_POINT ( 'NONE',  ( -1.453061824024428850, -23.46064660281889047, -43.67210485538161890 ) ) ;
#5076 = CARTESIAN_POINT ( 'NONE',  ( 60.34434042017240074, -45.86867586488080661, -47.72879939364779744 ) ) ;
#5077 = FACE_OUTER_BOUND ( 'NONE', #29029, .T. ) ;
#5078 = ADVANCED_FACE ( 'NONE', ( #3475 ), #23609, .T. ) ;
#5079 = CARTESIAN_POINT ( 'NONE',  ( 52.99344130519229878, 21.02275823560599832, -54.37359777462930310 ) ) ;
#5080 = EDGE_CURVE ( 'NONE', #25882, #7747, #49095, .T. ) ;
#5081 = CARTESIAN_POINT ( 'NONE',  ( 11.97526571559677677, -21.02750872198566157, -61.16116878873128115 ) ) ;
#5082 = LINE ( 'NONE', #21294, #34116 ) ;
#5083 = EDGE_LOOP ( 'NONE', ( #10646, #26586, #21157, #15720 ) ) ;
#5084 = DIRECTION ( 'NONE',  ( 0.000000000000000000, 0.7071067811865475727, 0.7071067811865475727 ) ) ;
#5085 = CARTESIAN_POINT ( 'NONE',  ( 10.13537795804320041, 31.89605224914739878, -45.99742856566899718 ) ) ;
#5086 = CARTESIAN_POINT ( 'NONE',  ( 26.63393739769619728, -15.61618894467929941, -18.58999999999999986 ) ) ;
#5087 = FACE_OUTER_BOUND ( 'NONE', #38255, .T. ) ;
#5088 = ORIENTED_EDGE ( 'NONE', *, *, #24618, .F. ) ;
#5089 = CARTESIAN_POINT ( 'NONE',  ( 17.80738288411419745, 20.21128881784739661, -75.25165125838280744 ) ) ;
#5090 = VERTEX_POINT ( 'NONE', #59 ) ;
#5091 = EDGE_LOOP ( 'NONE', ( #31573, #33406, #26990, #15134, #49184, #11411, #36586 ) ) ;
#5092 = CARTESIAN_POINT ( 'NONE',  ( 49.08512682873279687, 22.68755118111490177, -55.26163594736860318 ) ) ;
#5093 = ORIENTED_EDGE ( 'NONE', *, *, #38340, .F. ) ;
#5094 = CARTESIAN_POINT ( 'NONE',  ( 10.51395742882619899, -64.02946666124979913, -45.97815992060260726 ) ) ;
#5095 = CARTESIAN_POINT ( 'NONE',  ( 57.15508372626799627, -45.65320873106580279, -26.17772718789539965 ) ) ;
#5096 = CARTESIAN_POINT ( 'NONE',  ( 22.12745480022610067, -19.48200407513829902, -81.23899999999999011 ) ) ;
#5097 = EDGE_CURVE ( 'NONE', #44163, #47510, #44344, .T. ) ;
#5098 = B_SPLINE_CURVE_WITH_KNOTS ( 'NONE', 3,
 ( #49582, #6060, #33817, #36718, #45379, #5294, #25177, #49321 ),
 .UNSPECIFIED., .F., .F.,
 ( 4, 2, 2, 4 ),
 ( 0.000000000000000000, 0.1749999999962247588, 0.3749999999919103599, 0.4999997377388590292 ),
 .UNSPECIFIED. ) ;
#5099 = CARTESIAN_POINT ( 'NONE',  ( 61.61622621241649966, 13.95300478508159969, -46.89001122893169793 ) ) ;
#5100 = CARTESIAN_POINT ( 'NONE',  ( 63.76999183493178691, 1.442158793902849956, -61.94395472936509606 ) ) ;
#5101 = EDGE_LOOP ( 'NONE', ( #37784, #33545, #50537, #27702 ) ) ;
#5102 = CARTESIAN_POINT ( 'NONE',  ( 85.26960572018148810, -50.03040250705240055, -53.60827425107920874 ) ) ;
#5103 = EDGE_CURVE ( 'NONE', #45283, #49938, #42559, .T. ) ;
#5104 = CARTESIAN_POINT ( 'NONE',  ( 12.33251668000310808, 33.41328466589543922, -15.86092358591091589 ) ) ;
#5105 = ORIENTED_EDGE ( 'NONE', *, *, #50128, .T. ) ;
#5106 = CARTESIAN_POINT ( 'NONE',  ( 16.13393739769620083, -15.61618894467929941, -5.690000000000000391 ) ) ;
#5107 = CARTESIAN_POINT ( 'NONE',  ( 24.04460909154476056, -15.61619055174803172, -33.79232989763376338 ) ) ;
#5108 = CARTESIAN_POINT ( 'NONE',  ( 58.54079899187081537, -45.63568207302990487, -26.46003400569485464 ) ) ;
#5110 = ORIENTED_EDGE ( 'NONE', *, *, #23506, .F. ) ;
#5109 = AXIS2_PLACEMENT_3D ( 'NONE', #51385, #51130, #15226 ) ;
#5111 = VERTEX_POINT ( 'NONE', #8954 ) ;
#5112 = DIRECTION ( 'NONE',  ( 0.000000000000000000, 1.000000000000000000, 0.000000000000000000 ) ) ;
#5113 = CARTESIAN_POINT ( 'NONE',  ( 46.68381635779479666, -53.67199518238830080, -75.98463753095340678 ) ) ;
#5114 = VECTOR ( 'NONE', #35544, 1000.000000000000000 ) ;
#5115 = CARTESIAN_POINT ( 'NONE',  ( 60.59736966202989805, 14.55571675506389973, -47.75487759591599968 ) ) ;
#5116 = CIRCLE ( 'NONE', #20984, 1.500000000000001332 ) ;
#5117 = CARTESIAN_POINT ( 'NONE',  ( 50.27314737944030298, 14.74472902852030032, -12.51578207897900086 ) ) ;
#5118 = CARTESIAN_POINT ( 'NONE',  ( 29.13393739769619728, 4.883811055320659733, -81.65000000000000568 ) ) ;
#5119 = CARTESIAN_POINT ( 'NONE',  ( -4.842671363392640593, 16.07518510873240203, -4.485484122326420575 ) ) ;
#5120 = CARTESIAN_POINT ( 'NONE',  ( 11.55539561595326425, -20.98084311128575763, -55.57206633538740448 ) ) ;
#5121 = CARTESIAN_POINT ( 'NONE',  ( 59.45158862381180143, 14.23092646871359968, -26.67082509506299814 ) ) ;
#5122 = CARTESIAN_POINT ( 'NONE',  ( 10.31024158113670097, -20.87654209055929755, -68.05366966235949633 ) ) ;
#5123 = ORIENTED_EDGE ( 'NONE', *, *, #9783, .T. ) ;
#5124 = CARTESIAN_POINT ( 'NONE',  ( 59.74618096160109815, 14.90151641663299920, -47.73567920125140063 ) ) ;
#5125 = CARTESIAN_POINT ( 'NONE',  ( -10.65957727951819933, -41.24256659105780187, -4.264195539817489333 ) ) ;
#5126 = CARTESIAN_POINT ( 'NONE',  ( 72.83393739769620367, 1.883811055320669947, -62.44999999999999574 ) ) ;
#5127 = CARTESIAN_POINT ( 'NONE',  ( 73.01560786460549934, 1.024253516290730026, -69.12311412914529285 ) ) ;
#5128 = CARTESIAN_POINT ( 'NONE',  ( 14.37540540599747452, -41.85765695298066902, -34.70142521051218409 ) ) ;
#5129 = CARTESIAN_POINT ( 'NONE',  ( 11.49562787870944014, 34.14054113714986016, -18.17421237829643843 ) ) ;
#5130 = CARTESIAN_POINT ( 'NONE',  ( 47.16778299211050296, 23.48143463812749943, -74.72646181054710723 ) ) ;
#5131 = CARTESIAN_POINT ( 'NONE',  ( 48.81910031065179822, -53.88745037611909794, -54.56221240745009737 ) ) ;
#5132 = CARTESIAN_POINT ( 'NONE',  ( 18.20454803119799791, -23.32130851867060173, -56.20901675537331954 ) ) ;
#5133 = EDGE_CURVE ( 'NONE', #26643, #35688, #49380, .T. ) ;
#5134 = CARTESIAN_POINT ( 'NONE',  ( 76.73547614042425380, -43.17979320943853594, -14.45192718277627009 ) ) ;
#5135 = CARTESIAN_POINT ( 'NONE',  ( 65.70572778047942109, -32.85841247341685545, -18.95019540820560877 ) ) ;
#5136 = CARTESIAN_POINT ( 'NONE',  ( 23.83903696605923273, -17.68686790340041526, -53.87566772557626393 ) ) ;
#5137 = ADVANCED_FACE ( 'NONE', ( #45106 ), #303, .T. ) ;
#5138 = ORIENTED_EDGE ( 'NONE', *, *, #13611, .T. ) ;
#5139 = VECTOR ( 'NONE', #50255, 1000.000000000000000 ) ;
#5140 = CARTESIAN_POINT ( 'NONE',  ( 13.30627730215510063, -22.50901367206249759, -41.69125950871409003 ) ) ;
#5141 = CARTESIAN_POINT ( 'NONE',  ( 64.43841554592269460, 1.426105412861020216, -61.24861962585290343 ) ) ;
#5142 = ORIENTED_EDGE ( 'NONE', *, *, #2657, .F. ) ;
#5143 = CARTESIAN_POINT ( 'NONE',  ( 51.13393739769620083, 19.38381105532069881, 14.21249999999999858 ) ) ;
#5144 = CARTESIAN_POINT ( 'NONE',  ( 60.55906510858309844, -45.72613536122689482, -47.62951512971719836 ) ) ;
#5145 = DIRECTION ( 'NONE',  ( 0.000000000000000000, -1.000000000000000000, 0.000000000000000000 ) ) ;
#5146 = DIRECTION ( 'NONE',  ( 0.000000000000000000, 1.000000000000000000, 0.000000000000000000 ) ) ;
#5148 = CARTESIAN_POINT ( 'NONE',  ( 44.66618967801522899, -33.16378185082322005, -44.72241104285924251 ) ) ;
#5147 = CARTESIAN_POINT ( 'NONE',  ( 43.22233765097706737, 8.654584815917743867, -70.42371853659152237 ) ) ;
#5149 = AXIS2_PLACEMENT_3D ( 'NONE', #40918, #25429, #1349 ) ;
#5150 = CARTESIAN_POINT ( 'NONE',  ( 11.96660005458890019, -42.11618894467939356, -34.64999999999999858 ) ) ;
#5151 = DIRECTION ( 'NONE',  ( 1.000000000000000000, 0.000000000000000000, 0.000000000000000000 ) ) ;
#5152 = ORIENTED_EDGE ( 'NONE', *, *, #43152, .F. ) ;
#5153 = CARTESIAN_POINT ( 'NONE',  ( 83.82044569750020457, -44.78926617021760848, -47.35730118573349756 ) ) ;
#5154 = ORIENTED_EDGE ( 'NONE', *, *, #51140, .F. ) ;
#5155 = ORIENTED_EDGE ( 'NONE', *, *, #14417, .T. ) ;
#5156 = EDGE_LOOP ( 'NONE', ( #30866, #5782, #7269, #12914 ) ) ;
#5157 = CARTESIAN_POINT ( 'NONE',  ( 61.75020731935619267, -45.11618170104340209, -46.51046377108719554 ) ) ;
#5158 = CARTESIAN_POINT ( 'NONE',  ( 76.43577037016747511, -7.494458964928895739, -12.95064323996461653 ) ) ;
#5159 = LINE ( 'NONE', #21115, #49443 ) ;
#5160 = ORIENTED_EDGE ( 'NONE', *, *, #15390, .F. ) ;
#5161 = EDGE_LOOP ( 'NONE', ( #18099, #21194, #41304 ) ) ;
#5162 = EDGE_CURVE ( 'NONE', #32442, #28421, #40136, .T. ) ;
#5163 = CARTESIAN_POINT ( 'NONE',  ( 11.63514989718968273, 34.14682459674944681, -22.51338914225708621 ) ) ;
#5164 = VERTEX_POINT ( 'NONE', #24639 ) ;
#5165 = CARTESIAN_POINT ( 'NONE',  ( 56.58636862632249631, 19.37200252008349821, -53.13121941621520250 ) ) ;
#5166 = CARTESIAN_POINT ( 'NONE',  ( 10.64863409883700029, 32.21085600226960111, -23.66469670114080159 ) ) ;
#5167 = CARTESIAN_POINT ( 'NONE',  ( 8.223585368203801593, -15.61624251583899969, -52.79233150823699816 ) ) ;
#5168 = CARTESIAN_POINT ( 'NONE',  ( 7.820074255002061214, -21.65656408986289350, -5.690000000000000391 ) ) ;
#5169 = EDGE_CURVE ( 'NONE', #40090, #611, #16285, .T. ) ;
#5170 = FACE_OUTER_BOUND ( 'NONE', #18389, .T. ) ;
#5171 = ORIENTED_EDGE ( 'NONE', *, *, #30069, .F. ) ;
#5172 = CARTESIAN_POINT ( 'NONE',  ( -0.1957178007246416773, 20.73075855749606689, -6.909876211445776129 ) ) ;
#5173 = CARTESIAN_POINT ( 'NONE',  ( 52.28361278957570590, -49.79955569159500328, -77.20042821566700297 ) ) ;
#5174 = CARTESIAN_POINT ( 'NONE',  ( 20.48510588023628287, -20.83495730151230418, -46.73167619432699382 ) ) ;
#5175 = CARTESIAN_POINT ( 'NONE',  ( 60.75684423228010189, 14.27531910353349964, -47.09517711229599968 ) ) ;
#5176 = CARTESIAN_POINT ( 'NONE',  ( 22.77332867066339972, -11.43226362077250080, -67.83350675970849863 ) ) ;
#5177 = CARTESIAN_POINT ( 'NONE',  ( 65.13393739769620083, 1.383811055320669947, -65.65000000000000568 ) ) ;
#5178 = CARTESIAN_POINT ( 'NONE',  ( 42.70540900715619870, 13.77437978117109907, -6.147237832590779938 ) ) ;
#5179 = CARTESIAN_POINT ( 'NONE',  ( 42.63373764987009906, -44.09845193377589823, -5.023048285612619956 ) ) ;
#5180 = CARTESIAN_POINT ( 'NONE',  ( 68.13393739769841773, -50.61618894467878960, -73.25000000000220268 ) ) ;
#5181 = DIRECTION ( 'NONE',  ( 0.000000000000000000, -1.000000000000000000, 0.000000000000000000 ) ) ;
#5182 = AXIS2_PLACEMENT_3D ( 'NONE', #9588, #32618, #29223 ) ;
#5183 = AXIS2_PLACEMENT_3D ( 'NONE', #46554, #10643, #3032 ) ;
#5184 = CARTESIAN_POINT ( 'NONE',  ( 64.08753032830780683, 1.107039789628780024, -70.07374305313838647 ) ) ;
#5185 = CARTESIAN_POINT ( 'NONE',  ( 11.27237010540747875, -9.289939966437113839, -41.08399800701788962 ) ) ;
#5186 = AXIS2_PLACEMENT_3D ( 'NONE', #4280, #48311, #40440 ) ;
#5187 = CARTESIAN_POINT ( 'NONE',  ( 67.77237649856910195, 1.249209544680260242, -19.08110282771260202 ) ) ;
#5188 = ORIENTED_EDGE ( 'NONE', *, *, #7898, .T. ) ;
#5189 = CARTESIAN_POINT ( 'NONE',  ( 14.00496991351040066, -51.89834789502650381, -75.53980707817230211 ) ) ;
#5190 = CARTESIAN_POINT ( 'NONE',  ( 57.34209066734109683, 19.16565926987989599, -53.00664426348080127 ) ) ;
#5191 = DIRECTION ( 'NONE',  ( 0.7071067811865472397, -0.7071067811865479058, 0.000000000000000000 ) ) ;
#5192 = CARTESIAN_POINT ( 'NONE',  ( 83.67474298203126182, 13.26187872094980946, -46.57587824071405436 ) ) ;
#5193 = CARTESIAN_POINT ( 'NONE',  ( 24.03754256302241998, -15.24659606640338083, -55.49280163511743780 ) ) ;
#5194 = CARTESIAN_POINT ( 'NONE',  ( 22.65097095636950186, -12.86430221781309946, -32.14999999999999858 ) ) ;
#5195 = CARTESIAN_POINT ( 'NONE',  ( 55.89888397486434002, -45.90870921158190043, -17.63255904996966095 ) ) ;
#5196 = DIRECTION ( 'NONE',  ( 0.000000000000000000, -1.000000000000000000, 0.000000000000000000 ) ) ;
#5198 = CARTESIAN_POINT ( 'NONE',  ( 28.13393739769619728, -22.54439217495490055, -47.64999999999999858 ) ) ;
#5197 = DIRECTION ( 'NONE',  ( 0.000000000000000000, 0.000000000000000000, -1.000000000000000000 ) ) ;
#5199 = EDGE_CURVE ( 'NONE', #42670, #47254, #25165, .T. ) ;
#5200 = CARTESIAN_POINT ( 'NONE',  ( 56.33973134792619675, 19.37458302847869973, -52.96823346731370208 ) ) ;
#5201 = CARTESIAN_POINT ( 'NONE',  ( 48.72449300217610357, 22.67606569047629961, -54.53033886993310375 ) ) ;
#5202 = ORIENTED_EDGE ( 'NONE', *, *, #42442, .T. ) ;
#5203 = CARTESIAN_POINT ( 'NONE',  ( 9.278031783360169982, -17.27121685434340037, -67.77178171918468763 ) ) ;
#5204 = ORIENTED_EDGE ( 'NONE', *, *, #5633, .F. ) ;
#5205 = FACE_OUTER_BOUND ( 'NONE', #21731, .T. ) ;
#5206 = CARTESIAN_POINT ( 'NONE',  ( 53.29384558423090112, 19.31433099946569953, -48.47378032971769812 ) ) ;
#5207 = DIRECTION ( 'NONE',  ( -0.8732394366197182567, 0.4872913772396111343, -1.665334536937735304E-16 ) ) ;
#5209 = CARTESIAN_POINT ( 'NONE',  ( 53.76692370360909479, 17.31591783857309963, -26.47372352232380166 ) ) ;
#5208 = CARTESIAN_POINT ( 'NONE',  ( 83.82017571155999747, 13.44570198998940036, -47.23783155238629661 ) ) ;
#5210 = CARTESIAN_POINT ( 'NONE',  ( 21.62437782416010279, -20.04310916307899859, -60.66881518290298914 ) ) ;
#5211 = DIRECTION ( 'NONE',  ( 1.000000000000000000, 2.460964292799963328E-14, 0.000000000000000000 ) ) ;
#5212 = CARTESIAN_POINT ( 'NONE',  ( 57.05054250623780376, -45.11618894467940066, -16.05309365090189999 ) ) ;
#5213 = CARTESIAN_POINT ( 'NONE',  ( 52.56521993351449851, 18.62941884369810097, -28.15000000000000213 ) ) ;
#5214 = ORIENTED_EDGE ( 'NONE', *, *, #16566, .T. ) ;
#5215 = VERTEX_POINT ( 'NONE', #20456 ) ;
#5216 = CARTESIAN_POINT ( 'NONE',  ( 12.06856799516239853, -65.14762389849769875, -16.61922514011519780 ) ) ;
#5217 = CARTESIAN_POINT ( 'NONE',  ( 11.35079409783939930, 33.43282641247379416, -45.67788118199990066 ) ) ;
#5218 = CARTESIAN_POINT ( 'NONE',  ( 63.43393739769620510, 1.383811055320669947, -68.50657137141709541 ) ) ;
#5219 = CIRCLE ( 'NONE', #47894, 1.000000000000003109 ) ;
#5220 = CARTESIAN_POINT ( 'NONE',  ( 49.31205535909459314, -53.03485293375030096, -52.41062034357430122 ) ) ;
#5221 = CARTESIAN_POINT ( 'NONE',  ( 22.46012706948180337, -20.47783335039490993, -63.71600312820974210 ) ) ;
#5222 = VECTOR ( 'NONE', #34185, 1000.000000000000000 ) ;
#5223 = ORIENTED_EDGE ( 'NONE', *, *, #23856, .T. ) ;
#5224 = EDGE_CURVE ( 'NONE', #40777, #11419, #40652, .T. ) ;
#5225 = CARTESIAN_POINT ( 'NONE',  ( -22.69159524740030065, -13.72712742066280001, -54.49830448709099784 ) ) ;
#5226 = CARTESIAN_POINT ( 'NONE',  ( 54.27274129413513748, 17.15418818842660542, -26.87180614142805624 ) ) ;
#5227 = CARTESIAN_POINT ( 'NONE',  ( 8.222268241235530795, -15.61616536502389962, -60.50766849176299900 ) ) ;
#5228 = ADVANCED_FACE ( 'NONE', ( #49051, #1342 ), #17075, .T. ) ;
#5229 = CARTESIAN_POINT ( 'NONE',  ( 72.14060588395169304, 1.458412159422780130, -69.79309345819311261 ) ) ;
#5230 = CARTESIAN_POINT ( 'NONE',  ( 63.44018392888030178, 1.383811055320669947, -62.77287342953649585 ) ) ;
#5231 = CARTESIAN_POINT ( 'NONE',  ( 22.29130106582169901, -53.79438198982389707, -34.67842804303180060 ) ) ;
#5232 = ORIENTED_EDGE ( 'NONE', *, *, #16379, .T. ) ;
#5233 = CARTESIAN_POINT ( 'NONE',  ( 17.01981006685115716, -8.849199573316891332, -67.99448558109631335 ) ) ;
#5234 = FACE_OUTER_BOUND ( 'NONE', #13150, .T. ) ;
#5235 = EDGE_LOOP ( 'NONE', ( #3490, #5546, #8752, #48826 ) ) ;
#5236 = CARTESIAN_POINT ( 'NONE',  ( 12.14977632440493416, -8.703682543532863747, -53.12566589029975717 ) ) ;
#5237 = DIRECTION ( 'NONE',  ( 0.000000000000000000, 0.000000000000000000, -1.000000000000000000 ) ) ;
#5238 = CARTESIAN_POINT ( 'NONE',  ( 23.30211932285680021, -18.81054576247569798, -36.14593433426069424 ) ) ;
#5239 = CARTESIAN_POINT ( 'NONE',  ( -21.36606260230379917, -63.11618894467929408, 11.84999999999999964 ) ) ;
#5240 = CARTESIAN_POINT ( 'NONE',  ( 56.16528524747329953, 19.58792304710189924, -74.72304216316619829 ) ) ;
#5241 = CARTESIAN_POINT ( 'NONE',  ( 47.28500118035560007, -54.39529810738689974, -75.17099345517469544 ) ) ;
#5242 = ORIENTED_EDGE ( 'NONE', *, *, #21442, .F. ) ;
#5243 = CARTESIAN_POINT ( 'NONE',  ( 55.51083792958409902, 14.38702645469839858, -16.12015598830499741 ) ) ;
#5244 = CARTESIAN_POINT ( 'NONE',  ( 57.18740755751830562, -50.43062217190990282, -53.01833411754459746 ) ) ;
#5245 = CARTESIAN_POINT ( 'NONE',  ( 10.96668629868520028, -20.41640511211859987, -35.60889570735529475 ) ) ;
#5246 = CARTESIAN_POINT ( 'NONE',  ( 72.83393739769620367, 1.883811055320669947, -68.84999999999999432 ) ) ;
#5247 = ORIENTED_EDGE ( 'NONE', *, *, #8981, .F. ) ;
#5248 = CARTESIAN_POINT ( 'NONE',  ( 47.37718579482119452, 23.30994691619889991, -74.80618026387681141 ) ) ;
#5249 = CARTESIAN_POINT ( 'NONE',  ( 19.95138792988717569, -54.89243911056428260, -18.38918865259743285 ) ) ;
#5250 = CARTESIAN_POINT ( 'NONE',  ( 40.93885366971109363, -45.45026610025310276, -5.915603290955130156 ) ) ;
#5251 = VECTOR ( 'NONE', #12315, 1000.000000000000000 ) ;
#5252 = CARTESIAN_POINT ( 'NONE',  ( 12.33251669429169972, 33.41328467211270237, -15.86092359079939840 ) ) ;
#5253 = CARTESIAN_POINT ( 'NONE',  ( 10.93345605571719936, -9.217934799021591630, -80.79042367306230688 ) ) ;
#5254 = CARTESIAN_POINT ( 'NONE',  ( 60.34379258661509482, -45.86802437805019395, -47.72732609191810127 ) ) ;
#5256 = CARTESIAN_POINT ( 'NONE',  ( 44.04591232117690680, -40.05666563364601984, -66.03710115006609271 ) ) ;
#5255 = CARTESIAN_POINT ( 'NONE',  ( 14.13393739769630031, 1.380694156556678820, -35.10658870009210375 ) ) ;
#5257 = EDGE_CURVE ( 'NONE', #10013, #30043, #34998, .T. ) ;
#5258 = CARTESIAN_POINT ( 'NONE',  ( 52.56522529778620623, -49.86179102641759897, -48.47379134784809906 ) ) ;
#5259 = CARTESIAN_POINT ( 'NONE',  ( 17.16953355736119136, -7.705195898817367883, -79.04933618277276253 ) ) ;
#5260 = CARTESIAN_POINT ( 'NONE',  ( -26.85818705357539926, -41.76596063699349770, -55.57881993978430302 ) ) ;
#5261 = ADVANCED_FACE ( 'NONE', ( #12357 ), #28321, .T. ) ;
#5262 = ORIENTED_EDGE ( 'NONE', *, *, #12390, .F. ) ;
#5263 = CARTESIAN_POINT ( 'NONE',  ( 53.28342433172029757, -49.42919346652210066, -48.89794257291740109 ) ) ;
#5264 = CARTESIAN_POINT ( 'NONE',  ( 61.57714813399910270, -45.11618897791640137, -27.37584119844559893 ) ) ;
#5265 = DIRECTION ( 'NONE',  ( 0.000000000000000000, 0.000000000000000000, -1.000000000000000000 ) ) ;
#5266 = CARTESIAN_POINT ( 'NONE',  ( 56.63434221316140338, 14.45566336728010093, -26.04414657594499971 ) ) ;
#5267 = CARTESIAN_POINT ( 'NONE',  ( 22.99833165505350152, -17.23564876112759947, -34.52656793190860185 ) ) ;
#5268 = CARTESIAN_POINT ( 'NONE',  ( 51.06184042306900039, 18.36344697847389895, -76.32371533076559444 ) ) ;
#5269 = CARTESIAN_POINT ( 'NONE',  ( 52.87494882852160316, 18.41383132391699817, -48.84793717290940407 ) ) ;
#5270 = CARTESIAN_POINT ( 'NONE',  ( 71.26909468036909345, 1.099973129953850215, -70.71354394397609155 ) ) ;
#5271 = DIRECTION ( 'NONE',  ( 0.000000000000000000, 0.000000000000000000, -1.000000000000000000 ) ) ;
#5272 = CARTESIAN_POINT ( 'NONE',  ( 63.61124308565409535, -44.96453999798260526, -11.13477462305379895 ) ) ;
#5273 = AXIS2_PLACEMENT_3D ( 'NONE', #39370, #3728, #7662 ) ;
#5274 = VERTEX_POINT ( 'NONE', #36446 ) ;
#5275 = CARTESIAN_POINT ( 'NONE',  ( 20.29274154463319846, -21.79769704592460045, -73.37883193416179495 ) ) ;
#5276 = VERTEX_POINT ( 'NONE', #16538 ) ;
#5277 = CARTESIAN_POINT ( 'NONE',  ( 73.09245838956729813, 1.096153228089730147, -68.95757157983499042 ) ) ;
#5278 = CARTESIAN_POINT ( 'NONE',  ( 47.38360762733800158, -54.66752147347639834, -54.85966442921209563 ) ) ;
#5279 = CARTESIAN_POINT ( 'NONE',  ( 20.48567924760130055, -8.989398011352820461, -49.47734670041616312 ) ) ;
#5280 = DIRECTION ( 'NONE',  ( 0.000000000000000000, 0.000000000000000000, -1.000000000000000000 ) ) ;
#5281 = CARTESIAN_POINT ( 'NONE',  ( 57.51923301339540728, 18.59880830977609989, -52.27870191450410431 ) ) ;
#5282 = CARTESIAN_POINT ( 'NONE',  ( 71.33379467969419352, 1.389468113695450091, -61.03004030278179926 ) ) ;
#5283 = DIRECTION ( 'NONE',  ( -0.4640893551880601597, -0.8857883891771953788, 0.000000000000000000 ) ) ;
#5284 = CARTESIAN_POINT ( 'NONE',  ( 71.85037942476280648, 1.056975075119080065, -60.94761944900709949 ) ) ;
#5285 = CARTESIAN_POINT ( 'NONE',  ( -27.51648586239810257, -147.0143260265109859, -50.16206650068949813 ) ) ;
#5286 = CARTESIAN_POINT ( 'NONE',  ( 65.25794138637670017, 1.383811055320669947, -70.38195992526379996 ) ) ;
#5287 = ORIENTED_EDGE ( 'NONE', *, *, #49903, .F. ) ;
#5288 = VERTEX_POINT ( 'NONE', #809 ) ;
#5289 = CARTESIAN_POINT ( 'NONE',  ( 9.746758075853771075, -63.31345910889199757, -46.29788637164419640 ) ) ;
#5290 = DIRECTION ( 'NONE',  ( 0.000000000000000000, 1.000000000000000000, 0.000000000000000000 ) ) ;
#5291 = ORIENTED_EDGE ( 'NONE', *, *, #40410, .T. ) ;
#5292 = ADVANCED_FACE ( 'NONE', ( #4750 ), #20717, .T. ) ;
#5293 = CARTESIAN_POINT ( 'NONE',  ( 16.13393739769620083, -15.61618894467929941, -32.14999999999999858 ) ) ;
#5294 = CARTESIAN_POINT ( 'NONE',  ( 84.09627343997037485, 13.28281128162446123, -47.44643142069161712 ) ) ;
#5295 = CARTESIAN_POINT ( 'NONE',  ( 76.30797822825405774, -44.53040250705239345, -14.99128760117881676 ) ) ;
#5296 = CARTESIAN_POINT ( 'NONE',  ( 52.66575367246569783, 19.57588115571789800, -76.31205015641521072 ) ) ;
#5297 = EDGE_LOOP ( 'NONE', ( #15399, #9848 ) ) ;
#5298 = AXIS2_PLACEMENT_3D ( 'NONE', #3239, #48744, #39402 ) ;
#5299 = CARTESIAN_POINT ( 'NONE',  ( 17.92370450339619836, 20.88381105532299742, -76.14999999999999147 ) ) ;
#5300 = CARTESIAN_POINT ( 'NONE',  ( 22.68113533337184151, -13.84826337360422421, -72.36886283329307901 ) ) ;
#5301 = CARTESIAN_POINT ( 'NONE',  ( 24.01953185394659940, -14.96960027129633097, -43.76628852390030744 ) ) ;
#5302 = CARTESIAN_POINT ( 'NONE',  ( 24.35800691670550222, -15.02678195249309923, -51.76955764433359519 ) ) ;
#5303 = DIRECTION ( 'NONE',  ( 0.000000000000000000, 1.000000000000000000, 0.000000000000000000 ) ) ;
#5304 = CARTESIAN_POINT ( 'NONE',  ( 42.63564515191668391, -37.72326100604439603, -77.14139479405923794 ) ) ;
#5305 = ORIENTED_EDGE ( 'NONE', *, *, #38281, .F. ) ;
#5306 = LINE ( 'NONE', #38045, #43451 ) ;
#5307 = CARTESIAN_POINT ( 'NONE',  ( 23.47193497312810351, -16.90478717069920123, -44.28799034327369100 ) ) ;
#5308 = CARTESIAN_POINT ( 'NONE',  ( 24.04500464303940888, -15.61618902416171295, -53.50766607493442706 ) ) ;
#5309 = AXIS2_PLACEMENT_3D ( 'NONE', #5246, #12853, #14995 ) ;
#5310 = CARTESIAN_POINT ( 'NONE',  ( 14.86656154879790037, 21.55824172761710145, -76.12873484255680978 ) ) ;
#5311 = CARTESIAN_POINT ( 'NONE',  ( 51.70989020191399277, 17.69254107218870331, -77.02393701207040522 ) ) ;
#5312 =( BOUNDED_CURVE ( )  B_SPLINE_CURVE ( 3, ( #23473, #35022, #39748, #39496 ),
 .UNSPECIFIED., .F., .F. ) 
 B_SPLINE_CURVE_WITH_KNOTS ( ( 4, 4 ),
 ( 1.696124157962962009, 1.772154247585227438 ),
 .UNSPECIFIED. ) 
 CURVE ( )  GEOMETRIC_REPRESENTATION_ITEM ( )  RATIONAL_B_SPLINE_CURVE ( ( 1.000000000000000000, 0.9995183434654335564, 0.9995183434654335564, 1.000000000000000000 ) ) 
 REPRESENTATION_ITEM ( '' )  );
#5313 = DIRECTION ( 'NONE',  ( 0.000000000000000000, 1.000000000000000000, 0.000000000000000000 ) ) ;
#5314 = CARTESIAN_POINT ( 'NONE',  ( 24.33890690060549744, -16.42932864073580035, -53.53911138717730012 ) ) ;
#5315 = ORIENTED_EDGE ( 'NONE', *, *, #3726, .T. ) ;
#5316 = CARTESIAN_POINT ( 'NONE',  ( 53.36461225810830200, -49.03029623232499290, -26.93512695430979775 ) ) ;
#5317 = CARTESIAN_POINT ( 'NONE',  ( 14.28039018033829954, -50.95837531346739979, -21.66377081666569993 ) ) ;
#5318 = CARTESIAN_POINT ( 'NONE',  ( 12.14992171379115149, -22.52877759129744462, -64.45899891434670792 ) ) ;
#5319 = EDGE_CURVE ( 'NONE', #3978, #37534, #5044, .T. ) ;
#5320 = DIRECTION ( 'NONE',  ( -1.000000000000000000, 0.000000000000000000, 0.000000000000000000 ) ) ;
#5321 = CARTESIAN_POINT ( 'NONE',  ( 53.37798040714660175, 15.00501951321539984, -14.93908783775269988 ) ) ;
#5322 = EDGE_CURVE ( 'NONE', #27172, #14338, #5019, .T. ) ;
#5323 = AXIS2_PLACEMENT_3D ( 'NONE', #45286, #36899, #17502 ) ;
#5324 = ORIENTED_EDGE ( 'NONE', *, *, #12996, .T. ) ;
#5325 = CARTESIAN_POINT ( 'NONE',  ( -7.633825585628259525, -45.26999001540249878, -5.085140908233610091 ) ) ;
#5326 = ADVANCED_FACE ( 'NONE', ( #22009 ), #49573, .T. ) ;
#5327 = VECTOR ( 'NONE', #40021, 1000.000000000000000 ) ;
#5328 = CARTESIAN_POINT ( 'NONE',  ( 47.33274584257549833, 23.46610149159290160, -54.73778455475569871 ) ) ;
#5329 = CARTESIAN_POINT ( 'NONE',  ( 56.18863030605354680, -45.60033839355901364, -25.30081866562760595 ) ) ;
#5330 = CARTESIAN_POINT ( 'NONE',  ( 63.22343968446819673, 0.9036513197889520788, -62.20214363597960272 ) ) ;
#5331 = CARTESIAN_POINT ( 'NONE',  ( 56.52272905643124545, 15.01203539575427470, -26.27184597304366420 ) ) ;
#5332 = CARTESIAN_POINT ( 'NONE',  ( 11.31751849877900007, 34.00431797603069839, -17.44711658514470187 ) ) ;
#5333 = EDGE_CURVE ( 'NONE', #22521, #22272, #25801, .T. ) ;
#5334 = LINE ( 'NONE', #44378, #1806 ) ;
#5335 = CARTESIAN_POINT ( 'NONE',  ( 53.00700879704349688, 18.33567502363469970, -48.78176283131590196 ) ) ;
#5336 = DIRECTION ( 'NONE',  ( 0.000000000000000000, 0.000000000000000000, -1.000000000000000000 ) ) ;
#5337 = CARTESIAN_POINT ( 'NONE',  ( 59.93898548971230156, -46.07977442274060564, -47.78350827547860291 ) ) ;
#5338 = CARTESIAN_POINT ( 'NONE',  ( 52.88961653141840458, 18.37708373222320191, -27.85917056015219728 ) ) ;
#5339 = CARTESIAN_POINT ( 'NONE',  ( 52.47879378027149500, 21.24197845805030127, -54.47385978244439997 ) ) ;
#5340 = CARTESIAN_POINT ( 'NONE',  ( 63.49874256803619943, 1.370386981549569727, -69.01316122778010254 ) ) ;
#5341 = CARTESIAN_POINT ( 'NONE',  ( 15.24818525250952561, -8.849183378239496633, -47.91115446551594914 ) ) ;
#5342 = VERTEX_POINT ( 'NONE', #6310 ) ;
#5343 = FACE_OUTER_BOUND ( 'NONE', #9257, .T. ) ;
#5344 = CARTESIAN_POINT ( 'NONE',  ( 9.741373805871779368, 32.02484854115400026, -46.29737847346199686 ) ) ;
#5345 = DIRECTION ( 'NONE',  ( -1.000000000000000000, 0.000000000000000000, 0.000000000000000000 ) ) ;
#5346 = CARTESIAN_POINT ( 'NONE',  ( 12.79927192150049997, -8.608885486179000068, -81.23899999999999011 ) ) ;
#5347 = CARTESIAN_POINT ( 'NONE',  ( 17.83576269003119918, 20.28384221772149942, -75.35480091913980516 ) ) ;
#5348 = ORIENTED_EDGE ( 'NONE', *, *, #4133, .T. ) ;
#5349 = EDGE_LOOP ( 'NONE', ( #17131, #33679 ) ) ;
#5350 = AXIS2_PLACEMENT_3D ( 'NONE', #20904, #25082, #45029 ) ;
#5351 = DIRECTION ( 'NONE',  ( 0.000000000000000000, 0.000000000000000000, -1.000000000000000000 ) ) ;
#5352 = VERTEX_POINT ( 'NONE', #41425 ) ;
#5353 = EDGE_CURVE ( 'NONE', #5352, #23033, #18766, .T. ) ;
#5354 = CARTESIAN_POINT ( 'NONE',  ( 11.31507257915889930, -64.92605157093250057, -46.54990891655389618 ) ) ;
#5355 = CARTESIAN_POINT ( 'NONE',  ( 57.33744283413420106, -45.74625952484549885, -26.24889444639509861 ) ) ;
#5356 = CARTESIAN_POINT ( 'NONE',  ( 22.55493904458150212, -18.84709759249869876, -81.23899999999999011 ) ) ;
#5357 = CARTESIAN_POINT ( 'NONE',  ( 61.62976587840800136, 13.89047832419320017, -46.37201467644069908 ) ) ;
#5358 = CARTESIAN_POINT ( 'NONE',  ( 17.07096049057464526, 12.61358818065451182, -60.51477253168783221 ) ) ;
#5359 = VERTEX_POINT ( 'NONE', #26459 ) ;
#5360 = CARTESIAN_POINT ( 'NONE',  ( 21.94086349853619922, -19.61895903973029931, -69.03928461620259327 ) ) ;
#5361 = ORIENTED_EDGE ( 'NONE', *, *, #31501, .F. ) ;
#5362 = CARTESIAN_POINT ( 'NONE',  ( 48.13289152230240120, -45.11618894461150120, -9.279551874200048900 ) ) ;
#5363 = FACE_OUTER_BOUND ( 'NONE', #28462, .T. ) ;
#5364 = CYLINDRICAL_SURFACE ( 'NONE', #25948, 2.000000000000000444 ) ;
#5365 = ORIENTED_EDGE ( 'NONE', *, *, #34508, .F. ) ;
#5366 = CARTESIAN_POINT ( 'NONE',  ( 18.13393739769639978, 10.38381105532070059, -54.64999999999999858 ) ) ;
#5367 = CARTESIAN_POINT ( 'NONE',  ( 46.89485130532320056, -54.03863484889780011, -75.74144252524291687 ) ) ;
#5368 = DIRECTION ( 'NONE',  ( 0.000000000000000000, 0.000000000000000000, 1.000000000000000000 ) ) ;
#5369 = EDGE_CURVE ( 'NONE', #34827, #31635, #5791, .T. ) ;
#5370 = CARTESIAN_POINT ( 'NONE',  ( 52.39798347658840072, 14.77016143927119884, -14.07243307208769956 ) ) ;
#5371 = CARTESIAN_POINT ( 'NONE',  ( 16.13393739769620083, -15.61618894467929941, -21.14999999999999858 ) ) ;
#5372 = DIRECTION ( 'NONE',  ( 1.000000000000000000, 0.000000000000000000, -0.000000000000000000 ) ) ;
#5373 = CARTESIAN_POINT ( 'NONE',  ( 9.366931599644679807, -15.61636246440640008, -63.84717978381009118 ) ) ;
#5374 = CARTESIAN_POINT ( 'NONE',  ( 60.63521576136469804, 13.98548221933389968, -26.99365743681530105 ) ) ;
#5375 = CARTESIAN_POINT ( 'NONE',  ( 8.287157259014669819, -15.49457628754339922, -76.29243849297590430 ) ) ;
#5376 = ORIENTED_EDGE ( 'NONE', *, *, #46932, .F. ) ;
#5377 = DIRECTION ( 'NONE',  ( 8.462868000000000073E-18, -1.066343000000000058E-17, 1.000000000000000000 ) ) ;
#5378 = VECTOR ( 'NONE', #35312, 1000.000000000000000 ) ;
#5379 = LINE ( 'NONE', #33126, #5993 ) ;
#5380 = CARTESIAN_POINT ( 'NONE',  ( 28.28038400710291356, -22.62894316431776431, -34.79644660940672907 ) ) ;
#5381 = CARTESIAN_POINT ( 'NONE',  ( 72.72593655015040781, 1.394012070863599906, -68.94123343940819382 ) ) ;
#5382 = ADVANCED_FACE ( 'NONE', ( #42212 ), #38278, .T. ) ;
#5383 = B_SPLINE_CURVE_WITH_KNOTS ( 'NONE', 3,
 ( #17497, #29534, #9888, #37929, #33971, #22178, #2283, #41596, #1768, #50246, #14336, #30305, #46322, #2809, #46845, #3320, #42905, #7001 ),
 .UNSPECIFIED., .F., .F.,
 ( 4, 2, 2, 2, 2, 2, 2, 2, 4 ),
 ( 0.000000000000000000, 0.06249952337696731974, 0.1249990467539346395, 0.1874985701309019592, 0.2499980935078692790, 0.3124976168848365710, 0.3749971402618039185, 0.4374966636387712660, 0.4999961870157385579 ),
 .UNSPECIFIED. ) ;
#5384 = CARTESIAN_POINT ( 'NONE',  ( 20.11802686909307525, -8.703640737107740222, -43.17429654658235449 ) ) ;
#5385 = EDGE_CURVE ( 'NONE', #16578, #40267, #14165, .T. ) ;
#5386 = CARTESIAN_POINT ( 'NONE',  ( 48.86762024612250599, -53.93826904077799611, -54.76140763573010162 ) ) ;
#5387 = CARTESIAN_POINT ( 'NONE',  ( 43.91475033527959937, -43.54611815821230891, -5.093413304872340674 ) ) ;
#5388 = CIRCLE ( 'NONE', #26288, 1.500000000000001332 ) ;
#5389 = CARTESIAN_POINT ( 'NONE',  ( 8.254536426267019777, -16.37770113429971630, -34.47698882255479447 ) ) ;
#5390 = CARTESIAN_POINT ( 'NONE',  ( 18.53970998326800057, -51.57539031256270334, -74.98719232986280758 ) ) ;
#5391 = ORIENTED_EDGE ( 'NONE', *, *, #627, .T. ) ;
#5392 = AXIS2_PLACEMENT_3D ( 'NONE', #15260, #7908, #32749 ) ;
#5393 = CARTESIAN_POINT ( 'NONE',  ( 23.30168784358699696, -13.58393702039099971, -48.97940116656700127 ) ) ;
#5394 = CARTESIAN_POINT ( 'NONE',  ( 64.48466142462660855, 1.149538111077180069, -60.93632371623740340 ) ) ;
#5395 = ORIENTED_EDGE ( 'NONE', *, *, #7637, .F. ) ;
#5396 = DIRECTION ( 'NONE',  ( 0.000000000000000000, 0.000000000000000000, -1.000000000000000000 ) ) ;
#5397 = CARTESIAN_POINT ( 'NONE',  ( 61.07408082200849719, -45.63407273295089794, -47.69645918351529446 ) ) ;
#5398 = CARTESIAN_POINT ( 'NONE',  ( 22.90119541241246637, -15.61618911972255930, -40.84718082130915207 ) ) ;
#5399 = CARTESIAN_POINT ( 'NONE',  ( 20.63393739769599833, 10.38381105532070059, -35.14999999999999858 ) ) ;
#5401 = CARTESIAN_POINT ( 'NONE',  ( 50.03007040746459921, -48.61618894467930119, -78.14999999999999147 ) ) ;
#5400 = CARTESIAN_POINT ( 'NONE',  ( 43.62374791249758488, 8.690508226694738880, -68.48145595108481132 ) ) ;
#5402 = LINE ( 'NONE', #25802, #32634 ) ;
#5403 = DIRECTION ( 'NONE',  ( 0.3294064756441054120, -0.9441882088883177815, 9.436895709313929201E-16 ) ) ;
#5404 = ORIENTED_EDGE ( 'NONE', *, *, #51815, .F. ) ;
#5405 = EDGE_LOOP ( 'NONE', ( #44711, #13793, #9636, #25058 ) ) ;
#5406 = ORIENTED_EDGE ( 'NONE', *, *, #34703, .F. ) ;
#5407 = EDGE_LOOP ( 'NONE', ( #19021, #38205, #4099, #13285 ) ) ;
#5408 = CARTESIAN_POINT ( 'NONE',  ( 61.73009099606229455, -45.11618889822939593, -46.37193037902550685 ) ) ;
#5409 = CARTESIAN_POINT ( 'NONE',  ( 52.67030364760460515, -49.78282448137120042, -48.75888224404449289 ) ) ;
#5410 = CARTESIAN_POINT ( 'NONE',  ( 16.13393739769620083, -15.61618894467929941, 6.349999999999999645 ) ) ;
#5411 = CARTESIAN_POINT ( 'NONE',  ( 56.11441691986449598, -50.90435229196089750, -53.54520117640679899 ) ) ;
#5412 = B_SPLINE_CURVE_WITH_KNOTS ( 'NONE', 3,
 ( #28655, #25244, #41248, #5360, #24192, #21316, #40213, #4305, #16614, #20274, #48337 ),
 .UNSPECIFIED., .F., .F.,
 ( 4, 1, 1, 1, 1, 1, 1, 1, 4 ),
 ( 0.4999959824775806472, 0.5168334851326326085, 0.5960524161961817668, 0.6752713472598913524, 0.7544902783234405108, 0.8337092093871478760, 0.9129281404507014752, 0.9921470715144067309, 1.000000000000000000 ),
 .UNSPECIFIED. ) ;
#5413 = VERTEX_POINT ( 'NONE', #2367 ) ;
#5414 = ORIENTED_EDGE ( 'NONE', *, *, #7620, .T. ) ;
#5415 = ORIENTED_EDGE ( 'NONE', *, *, #6221, .T. ) ;
#5416 = CARTESIAN_POINT ( 'NONE',  ( 19.54188188357280964, -21.52912844502688117, -72.78610869383017246 ) ) ;
#5417 = CARTESIAN_POINT ( 'NONE',  ( -9.742541826421756923, 13.56590212943579488, -43.61116652808541971 ) ) ;
#5418 = CARTESIAN_POINT ( 'NONE',  ( 16.13393739769620083, -15.61618894467929941, -35.14999999999999858 ) ) ;
#5419 = AXIS2_PLACEMENT_3D ( 'NONE', #29638, #21776, #5810 ) ;
#5420 = CARTESIAN_POINT ( 'NONE',  ( 53.27996121806140195, -52.13308956689839846, -54.32024439625399737 ) ) ;
#5421 = CARTESIAN_POINT ( 'NONE',  ( 22.72480973293551898, -13.84493719928921784, -54.36948976686252877 ) ) ;
#5422 = EDGE_LOOP ( 'NONE', ( #23903, #31091, #17461, #14082 ) ) ;
#5423 = DIRECTION ( 'NONE',  ( 0.000000000000000000, 0.000000000000000000, -1.000000000000000000 ) ) ;
#5424 = CARTESIAN_POINT ( 'NONE',  ( 52.83096447931749395, -51.02617954204369966, -76.09006724408109790 ) ) ;
#5425 = CARTESIAN_POINT ( 'NONE',  ( 16.25549387145995084, -22.38225831564430734, -46.94710703770110882 ) ) ;
#5426 = CARTESIAN_POINT ( 'NONE',  ( 60.60271022049670364, 14.35607423084729994, -47.13139168423140291 ) ) ;
#5427 = ADVANCED_FACE ( 'NONE', ( #49820 ), #13911, .F. ) ;
#5428 = B_SPLINE_CURVE_WITH_KNOTS ( 'NONE', 3,
 ( #11974, #15895, #23212, #11199, #23979, #14860, #3076, #31337, #43168, #26905, #47871, #31592, #51543, #15640, #40002, #19043, #23470, #35808, #27929, #43931 ),
 .UNSPECIFIED., .F., .F.,
 ( 4, 2, 2, 2, 2, 2, 2, 2, 2, 4 ),
 ( 0.000000000000000000, 0.1775000000000006850, 0.3374999999999994671, 0.4374999999999980571, 0.4999999999999978906, 0.6249999999999994449, 0.7746634686404010317, 0.8753061185820656398, 0.9759487685237305810, 1.000000000000000000 ),
 .UNSPECIFIED. ) ;
#5429 = CARTESIAN_POINT ( 'NONE',  ( 8.288808833082619287, -15.41443316095459792, -61.02067868823729668 ) ) ;
#5430 = EDGE_CURVE ( 'NONE', #29238, #39800, #36692, .T. ) ;
#5431 = DIRECTION ( 'NONE',  ( 0.9441882088883221114, 0.3294064756440927000, 0.000000000000000000 ) ) ;
#5432 = CARTESIAN_POINT ( 'NONE',  ( 43.87445613097960262, 13.83391143939489965, -6.621204841358950155 ) ) ;
#5433 = AXIS2_PLACEMENT_3D ( 'NONE', #16911, #45209, #44426 ) ;
#5434 = CARTESIAN_POINT ( 'NONE',  ( 43.37850551083089812, -43.48449350341319786, -4.923475879740440320 ) ) ;
#5435 = EDGE_CURVE ( 'NONE', #16752, #3546, #16259, .T. ) ;
#5436 = CARTESIAN_POINT ( 'NONE',  ( 16.13393739769620083, -15.61618894467929941, -32.14999999999999858 ) ) ;
#5437 = CARTESIAN_POINT ( 'NONE',  ( 4.133937397696205274, -22.54439217495489700, -35.01561944896766931 ) ) ;
#5438 = CARTESIAN_POINT ( 'NONE',  ( 63.94153426497989301, 1.200157450721869967, -69.90579656221390792 ) ) ;
#5439 = CARTESIAN_POINT ( 'NONE',  ( 46.50691046839970255, 8.847764697030390479, -54.64999999999999858 ) ) ;
#5440 = CARTESIAN_POINT ( 'NONE',  ( 68.23802810435169874, 0.1965232615743089939, -18.38247172703000132 ) ) ;
#5441 = VERTEX_POINT ( 'NONE', #19642 ) ;
#5442 = CARTESIAN_POINT ( 'NONE',  ( 13.92281821510519890, -52.20693806470120535, -75.61048537065340724 ) ) ;
#5443 = LINE ( 'NONE', #1755, #26931 ) ;
#5444 = B_SPLINE_CURVE_WITH_KNOTS ( 'NONE', 3,
 ( #37575, #1941, #17921, #1681, #29698, #9811, #33892, #30738, #30480, #2978, #38360, #42821, #34930, #47521, #6917, #22868, #38889, #27326, #18434, #38629, #2454, #34408, #11107, #10848, #14770, #2721, #18952, #50930, #31500, #15027, #3234, #42562, #50422, #6653 ),
 .UNSPECIFIED., .F., .F.,
 ( 4, 2, 1, 1, 1, 1, 2, 2, 2, 2, 2, 2, 2, 2, 2, 2, 2, 2, 4 ),
 ( 0.4999993943104570904, 0.5004876761519508888, 0.5009759579934445206, 0.5019525216764315623, 0.5039056490424062007, 0.5078119037743555886, 0.5156244132382546974, 0.5312494321660528040, 0.5624994700216491283, 0.6249995457328421100, 0.6874996214440350917, 0.7499996971552280733, 0.8124997728664211660, 0.8437498107220176013, 0.8749998485776140367, 0.9062498864332106940, 0.9374999242888071294, 0.9687499621444035647, 1.000000000000000000 ),
 .UNSPECIFIED. ) ;
#5445 = CARTESIAN_POINT ( 'NONE',  ( 46.47536507427530239, -40.11920440292289669, -54.64999999999999858 ) ) ;
#5446 = CARTESIAN_POINT ( 'NONE',  ( 84.41931977240820117, 12.04917947078452301, -47.35294579213341848 ) ) ;
#5447 = CARTESIAN_POINT ( 'NONE',  ( 23.44327699831620038, -15.93920061306999791, -32.14999999999999858 ) ) ;
#5448 = CARTESIAN_POINT ( 'NONE',  ( 55.01976271995791024, -46.11948192427576032, -16.15584652683488898 ) ) ;
#5449 = EDGE_CURVE ( 'NONE', #41163, #49378, #23549, .T. ) ;
#5450 = CARTESIAN_POINT ( 'NONE',  ( 68.13393739769618662, -29.66618894467940137, -65.65000000000000568 ) ) ;
#5451 = VECTOR ( 'NONE', #2386, 1000.000000000000000 ) ;
#5453 = CARTESIAN_POINT ( 'NONE',  ( 9.120647901033246185, -11.85279051307570342, -44.66432580115215956 ) ) ;
#5452 = CARTESIAN_POINT ( 'NONE',  ( -18.28386310865111497, -15.61618894467930296, -82.14319696191608955 ) ) ;
#5454 = DIRECTION ( 'NONE',  ( 0.000000000000000000, 0.000000000000000000, -1.000000000000000000 ) ) ;
#5456 = DIRECTION ( 'NONE',  ( 0.3863301728269220581, -0.9223605572462000302, 0.000000000000000000 ) ) ;
#5455 = B_SPLINE_CURVE_WITH_KNOTS ( 'NONE', 3,
 ( #37782, #13431, #37264, #17351, #25962, #33316, #17608, #21002, #16829, #36999, #1876, #49073, #25442, #41973, #6070, #36727, #49329, #833, #9741, #32776, #25700, #12911, #1097, #17856, #13180, #29127, #28867, #44869 ),
 .UNSPECIFIED., .F., .F.,
 ( 4, 2, 2, 2, 2, 2, 2, 2, 2, 2, 1, 1, 1, 1, 2, 4 ),
 ( 0.000000000000000000, 0.06250046681096792234, 0.1250009336219358447, 0.1875014004329037531, 0.2500018672438716894, 0.3125023340548396256, 0.3750028008658075063, 0.4375032676767754425, 0.4687535010822594383, 0.4843786177850014085, 0.4921911761363723659, 0.4960974553120579555, 0.4980505948999007781, 0.4990271646938223005, 0.4995154495907830339, 0.5000037344877438228 ),
 .UNSPECIFIED. ) ;
#5457 = CARTESIAN_POINT ( 'NONE',  ( 48.08607070564750074, 23.01868680830909852, -54.70522948828759979 ) ) ;
#5458 = EDGE_LOOP ( 'NONE', ( #35408, #39333, #4578, #45817 ) ) ;
#5459 = CARTESIAN_POINT ( 'NONE',  ( 19.06574088075160134, -9.201589384987739706, -60.48364006133169823 ) ) ;
#5460 = ORIENTED_EDGE ( 'NONE', *, *, #30555, .T. ) ;
#5461 = DIRECTION ( 'NONE',  ( 0.000000000000000000, 0.000000000000000000, -1.000000000000000000 ) ) ;
#5462 = CARTESIAN_POINT ( 'NONE',  ( 65.01129443250870565, 1.391252479931859964, -61.03617692120100457 ) ) ;
#5463 = CARTESIAN_POINT ( 'NONE',  ( 12.72603136295543891, -21.52914872767418686, -43.11948669098642029 ) ) ;
#5465 = CARTESIAN_POINT ( 'NONE',  ( 53.72005416868749705, 17.35859260027000062, -26.34191669766340382 ) ) ;
#5464 = CARTESIAN_POINT ( 'NONE',  ( 83.94526921706011535, 13.29514832796600032, -47.24461768887499602 ) ) ;
#5466 = CARTESIAN_POINT ( 'NONE',  ( 19.62102412718670053, -21.74666892895760029, -64.78819959821109364 ) ) ;
#5467 = DIRECTION ( 'NONE',  ( 0.000000000000000000, 0.000000000000000000, -1.000000000000000000 ) ) ;
#5468 = CARTESIAN_POINT ( 'NONE',  ( 72.76779797359338886, 1.388189907116970101, -68.71367622713330547 ) ) ;
#5469 = B_SPLINE_SURFACE_WITH_KNOTS ( 'NONE', 3, 3, ( 
 ( #15197, #34317, #14418, #26454, #42469, #22523, #18857, #38535, #34842, #2631, #18603 ),
 ( #50585, #46927, #31410, #7851, #485, #4165, #47438, #11792, #24054, #47184, #23284 ),
 ( #19637, #3667, #51615, #12046, #12297, #7336, #15708, #44005, #27231, #8108, #39307 ),
 ( #31665, #19378, #11533, #27999, #40072, #47688, #20393, #27752, #35361, #51150, #20142 ),
 ( #27490, #11271, #32176, #36131, #35629, #39815, #23801, #24312, #236, #36380, #48192 ),
 ( #16221, #43749, #31923, #3925, #31156, #43497, #43249, #15969, #19885, #3410, #47945 ),
 ( #28256, #35876, #44256, #40330, #15460, #8363, #51360, #7599, #4423, #23543, #39561 ),
 ( #1273, #9654, #13588, #44516, #20652, #29043, #48717, #40582, #21171, #40842, #9138 ),
 ( #5722, #13091, #36637, #37176, #29297, #13337, #32692, #48451, #17514, #9407, #4941 ),
 ( #25094, #25608, #45298, #21676, #33486, #16474, #1528, #20916, #17264, #41106, #37687 ),
 ( #12556, #33224, #5216, #32429, #49242, #49500, #25355, #1012, #41358, #41613, #740 ),
 ( #29553, #45039, #5473, #16738, #24569, #28519, #36910, #8622, #12821, #21427, #37430 ),
 ( #4680, #45556, #28779, #44778, #8883, #24835, #17010, #32958, #48987, #22973, #41879 ),
 ( #30057, #13842, #34775, #18541, #22456, #38465, #10953, #5981, #10434, #22717, #50782 ),
 ( #6765, #2831, #14614, #26386, #34518, #22199, #33991, #18027, #37950, #2569, #30584 ),
 ( #14095, #46864, #17766, #29800, #26917, #21938, #18796, #26646, #46088, #50523, #14358 ),
 ( #42923, #2303, #46604, #2045, #30323, #1785, #42663, #50006, #34244, #10691, #33737 ),
 ( #6241, #42143, #26131, #38208, #38734, #14872, #45818, #18277, #30835, #49752, #7021 ) ),
 .UNSPECIFIED., .F., .F., .F.,
 ( 4, 2, 2, 2, 2, 2, 2, 2, 4 ),
 ( 4, 1, 1, 1, 1, 1, 1, 1, 4 ),
 ( -4.407659109999999858E-07, 0.02874937896918200106, 0.2125859696587990011, 0.3274838388398100264, 0.4366451184530800167, 0.4912257582597150396, 0.5785547819503310540, 0.7182812198553160110, 0.8732902369061590342 ),
 ( -4.407659119999999895E-07, 0.1250000000000000000, 0.2500000000000000000, 0.3750000000000000000, 0.5000000000000000000, 0.6250000000000000000, 0.7500000000000000000, 0.8750000000000000000, 1.000000000000000000 ),
 .UNSPECIFIED. ) ;
#5470 = DIRECTION ( 'NONE',  ( 0.000000000000000000, 0.000000000000000000, -1.000000000000000000 ) ) ;
#5471 = ORIENTED_EDGE ( 'NONE', *, *, #25109, .T. ) ;
#5472 = VERTEX_POINT ( 'NONE', #3415 ) ;
#5473 = CARTESIAN_POINT ( 'NONE',  ( 12.10148745386320002, -65.09303518706980185, -16.50605066007160104 ) ) ;
#5474 = CARTESIAN_POINT ( 'NONE',  ( 13.00893739769619906, 34.28605925116850273, -47.75434321273180416 ) ) ;
#5475 = CARTESIAN_POINT ( 'NONE',  ( -6.866062602303790285, -15.61618894467929941, -84.65000000000000568 ) ) ;
#5476 = CARTESIAN_POINT ( 'NONE',  ( 10.22106225561806880, -19.02424243086505129, -55.28615407388804215 ) ) ;
#5477 = CARTESIAN_POINT ( 'NONE',  ( 9.897519164466769936, -64.60056534484279211, -46.94956808900870016 ) ) ;
#5478 = VERTEX_POINT ( 'NONE', #47189 ) ;
#5479 = CARTESIAN_POINT ( 'NONE',  ( -3.724451274984229787, -49.27919138543109767, -38.36253275904599747 ) ) ;
#5480 = CARTESIAN_POINT ( 'NONE',  ( 16.13393739769620083, -15.61618894467929941, -35.14999999999999858 ) ) ;
#5481 = CYLINDRICAL_SURFACE ( 'NONE', #32307, 16.00000000000000000 ) ;
#5482 = CYLINDRICAL_SURFACE ( 'NONE', #9341, 1.999999999999997113 ) ;
#5483 = CARTESIAN_POINT ( 'NONE',  ( 59.32539931833549929, -3.119615929214149652, -15.67734707553489848 ) ) ;
#5484 = CARTESIAN_POINT ( 'NONE',  ( 50.77828552747430280, -50.74762180099720865, -76.14999999999999147 ) ) ;
#5485 = CARTESIAN_POINT ( 'NONE',  ( 57.24929578313069811, 19.38381105532069881, -53.91492796121699627 ) ) ;
#5486 = ORIENTED_EDGE ( 'NONE', *, *, #44191, .F. ) ;
#5487 = CARTESIAN_POINT ( 'NONE',  ( 53.34500566076300032, -49.01310193610010657, -26.65466145037910195 ) ) ;
#5488 = CARTESIAN_POINT ( 'NONE',  ( 68.13393739769819035, 19.47158195952289717, -70.40645085170196182 ) ) ;
#5489 = ORIENTED_EDGE ( 'NONE', *, *, #765, .F. ) ;
#5490 = CARTESIAN_POINT ( 'NONE',  ( 14.06321933549888570, -7.911099009402122739, -53.20899948581546113 ) ) ;
#5491 = LINE ( 'NONE', #37448, #37868 ) ;
#5492 = CONICAL_SURFACE ( 'NONE', #19729, 0.6299999999999991163, 0.7853981633974490562 ) ;
#5493 = CARTESIAN_POINT ( 'NONE',  ( 9.545302122914700149, -11.35278270015860080, -35.19530716149729699 ) ) ;
#5494 = AXIS2_PLACEMENT_3D ( 'NONE', #50990, #47839, #15092 ) ;
#5495 = ADVANCED_FACE ( 'NONE', ( #22783 ), #38401, .T. ) ;
#5496 = CARTESIAN_POINT ( 'NONE',  ( 13.92806294839289905, -51.20625126854269382, -22.96889535537080107 ) ) ;
#5497 = CARTESIAN_POINT ( 'NONE',  ( 55.90344875862429319, 19.41190792946789756, -75.71352352466739433 ) ) ;
#5498 = CARTESIAN_POINT ( 'NONE',  ( 46.62699164054490097, -53.28059046267329535, -76.10173089639540933 ) ) ;
#5499 = ORIENTED_EDGE ( 'NONE', *, *, #46177, .F. ) ;
#5500 = CARTESIAN_POINT ( 'NONE',  ( 56.28192901139959758, 14.29581952047969828, -17.75665406777029887 ) ) ;
#5501 = CARTESIAN_POINT ( 'NONE',  ( 56.94152844520889545, -50.61086428661570125, -53.44912207859540132 ) ) ;
#5502 = CARTESIAN_POINT ( 'NONE',  ( 52.66033724191510146, -49.78877526119400443, -48.73956177349010943 ) ) ;
#5503 = CARTESIAN_POINT ( 'NONE',  ( 16.03351556195739747, -22.66831448449759989, -37.35171219075489546 ) ) ;
#5504 = FACE_OUTER_BOUND ( 'NONE', #16358, .T. ) ;
#5505 = VERTEX_POINT ( 'NONE', #46933 ) ;
#5506 = CARTESIAN_POINT ( 'NONE',  ( 47.34726563384639775, 23.26222549619640034, -74.94563673128509151 ) ) ;
#5507 = CARTESIAN_POINT ( 'NONE',  ( 19.92389628699634940, -54.81363894426598904, -18.23936587176626745 ) ) ;
#5508 = CARTESIAN_POINT ( 'NONE',  ( 61.25267155084156201, -45.60875457951716072, -47.68505357991368498 ) ) ;
#5509 = CARTESIAN_POINT ( 'NONE',  ( 28.84982806847620296, -4.597856142697129833, -34.69901084462020435 ) ) ;
#5510 = AXIS2_PLACEMENT_3D ( 'NONE', #17511, #41353, #482 ) ;
#5511 = CARTESIAN_POINT ( 'NONE',  ( 16.37827341743040321, -23.85773112360640269, -79.99823436242610342 ) ) ;
#5512 = EDGE_CURVE ( 'NONE', #49694, #26020, #47443, .T. ) ;
#5513 = VECTOR ( 'NONE', #19362, 1000.000000000000000 ) ;
#5514 = CARTESIAN_POINT ( 'NONE',  ( 18.86789271246039945, 20.55440458018300021, -15.81497037201279987 ) ) ;
#5516 = CARTESIAN_POINT ( 'NONE',  ( 49.99435380674910334, -21.69248229676700390, -40.08896681911620163 ) ) ;
#5515 = CARTESIAN_POINT ( 'NONE',  ( 64.92520290936280958, 0.8850831926798620186, -60.57999765399179637 ) ) ;
#5517 = EDGE_CURVE ( 'NONE', #29730, #34663, #21727, .T. ) ;
#5518 = CYLINDRICAL_SURFACE ( 'NONE', #15944, 1.999999999999996891 ) ;
#5519 = CARTESIAN_POINT ( 'NONE',  ( 12.14979057282054242, -8.703674483741680845, -68.84100286263340251 ) ) ;
#5520 = CARTESIAN_POINT ( 'NONE',  ( -29.90021944857959824, -36.14291753250989814, -56.90940863684170381 ) ) ;
#5521 = VERTEX_POINT ( 'NONE', #15714 ) ;
#5522 = CARTESIAN_POINT ( 'NONE',  ( 52.72459160374280174, -49.72420427742829929, -48.48895090856409951 ) ) ;
#5523 = ORIENTED_EDGE ( 'NONE', *, *, #49275, .T. ) ;
#5524 = CARTESIAN_POINT ( 'NONE',  ( 61.49805056874480158, -45.11879423640499454, -27.42091738664879941 ) ) ;
#5525 = AXIS2_PLACEMENT_3D ( 'NONE', #48366, #4589, #40246 ) ;
#5526 = DIRECTION ( 'NONE',  ( 0.000000000000000000, 1.000000000000000000, 0.000000000000000000 ) ) ;
#5527 = CARTESIAN_POINT ( 'NONE',  ( 56.44557979832819683, 14.18613123430430001, -25.36404871676379713 ) ) ;
#5528 = CARTESIAN_POINT ( 'NONE',  ( 20.42372255482109722, -21.21442991862110006, -36.74469800168989764 ) ) ;
#5529 = DIRECTION ( 'NONE',  ( -0.2425356250363339128, 0.000000000000000000, -0.9701425001453316543 ) ) ;
#5530 = CARTESIAN_POINT ( 'NONE',  ( 52.70373694452960223, 18.51116282284399972, -48.64345963606820078 ) ) ;
#5531 = DIRECTION ( 'NONE',  ( 0.6415444970810859626, -0.4854844151940995167, 0.5939070136550161916 ) ) ;
#5532 = CARTESIAN_POINT ( 'NONE',  ( 72.31053544666039556, -43.38410770150959905, -12.49652231024070126 ) ) ;
#5533 = VECTOR ( 'NONE', #12798, 1000.000000000000000 ) ;
#5534 = ORIENTED_EDGE ( 'NONE', *, *, #8742, .F. ) ;
#5535 = CARTESIAN_POINT ( 'NONE',  ( 14.07085440528040010, -22.77512621944960003, -77.65665421159729931 ) ) ;
#5536 = CARTESIAN_POINT ( 'NONE',  ( 73.02809924467999281, 1.186515949276290227, -68.96459770949519452 ) ) ;
#5537 = CARTESIAN_POINT ( 'NONE',  ( 47.44122687894220292, -54.63357073524160512, -54.92718653334570433 ) ) ;
#5538 = CARTESIAN_POINT ( 'NONE',  ( 15.62246519096099107, -7.695412796532114186, -49.27188937755772002 ) ) ;
#5539 = CARTESIAN_POINT ( 'NONE',  ( 73.06808687136680192, 1.187415670095769871, -62.40340069948359769 ) ) ;
#5540 = LINE ( 'NONE', #20979, #6794 ) ;
#5541 = CARTESIAN_POINT ( 'NONE',  ( 71.48076113803239195, 1.264121749638659864, -60.84994802006399794 ) ) ;
#5542 = CARTESIAN_POINT ( 'NONE',  ( 28.13393739769619728, -22.54439217495490055, -47.64999999999999858 ) ) ;
#5543 = CARTESIAN_POINT ( 'NONE',  ( 71.53657551413809301, 1.402020837641559936, -61.10185970516889853 ) ) ;
#5544 = CARTESIAN_POINT ( 'NONE',  ( 15.09828667837113336, -23.52717655769652083, -72.04927324925495213 ) ) ;
#5545 = CARTESIAN_POINT ( 'NONE',  ( 64.84535060374950888, 1.263738073398980033, -70.48213147351589214 ) ) ;
#5546 = ORIENTED_EDGE ( 'NONE', *, *, #9537, .T. ) ;
#5547 = CARTESIAN_POINT ( 'NONE',  ( 14.05644111844239852, -51.15811488399830154, -22.83288692000170172 ) ) ;
#5548 = CARTESIAN_POINT ( 'NONE',  ( 68.13393739769618662, -2.032350560841069687, -29.09832030244572820 ) ) ;
#5549 = EDGE_LOOP ( 'NONE', ( #13561, #16421, #26281, #25041 ) ) ;
#5550 = CARTESIAN_POINT ( 'NONE',  ( 11.66017304635799867, -64.87584527432149173, -45.05114943332709743 ) ) ;
#5551 = CARTESIAN_POINT ( 'NONE',  ( 20.99558181260091061, -9.289996862630026442, -59.21596848997750584 ) ) ;
#5552 = CARTESIAN_POINT ( 'NONE',  ( 15.09845797924882760, -23.52719716851022724, -70.04933658504315019 ) ) ;
#5553 = CARTESIAN_POINT ( 'NONE',  ( 51.41399438364850027, 19.32188539444780062, -76.23672007490239366 ) ) ;
#5554 = ORIENTED_EDGE ( 'NONE', *, *, #8877, .F. ) ;
#5555 = FACE_OUTER_BOUND ( 'NONE', #17909, .T. ) ;
#5557 = DIRECTION ( 'NONE',  ( -1.000000000000000000, -8.673617379884043361E-16, 0.000000000000000000 ) ) ;
#5556 = VECTOR ( 'NONE', #17360, 1000.000000000000114 ) ;
#5558 = CARTESIAN_POINT ( 'NONE',  ( 14.06315832308397873, -7.911114717410128172, -43.20903977167234444 ) ) ;
#5559 = CARTESIAN_POINT ( 'NONE',  ( 19.78933351317860101, -23.00677750682039857, -54.14612557624229083 ) ) ;
#5560 = CIRCLE ( 'NONE', #23106, 16.00000000000000000 ) ;
#5561 = EDGE_CURVE ( 'NONE', #8299, #7479, #19126, .T. ) ;
#5562 = CARTESIAN_POINT ( 'NONE',  ( 46.03122142033570441, 13.88381105532070059, -7.582879021622040305 ) ) ;
#5563 = CARTESIAN_POINT ( 'NONE',  ( 45.33483351075369683, -38.08130543216955743, -63.64546632514639413 ) ) ;
#5564 = B_SPLINE_CURVE_WITH_KNOTS ( 'NONE', 3,
 ( #1338, #10238, #29864, #22264 ),
 .UNSPECIFIED., .F., .F.,
 ( 4, 4 ),
 ( 0.000000000000000000, 0.1813467805151689483 ),
 .UNSPECIFIED. ) ;
#5565 = ORIENTED_EDGE ( 'NONE', *, *, #27750, .T. ) ;
#5566 = CARTESIAN_POINT ( 'NONE',  ( 18.76585674228498135, 20.63639536069459268, -74.86151687926869158 ) ) ;
#5567 = CARTESIAN_POINT ( 'NONE',  ( 10.45489348174570132, -10.79382914828800111, -47.45674758581839825 ) ) ;
#5568 = CIRCLE ( 'NONE', #33180, 3.799999999999829736 ) ;
#5569 = CARTESIAN_POINT ( 'NONE',  ( 44.98357750381669007, 14.87860355809039881, -8.963129099644900677 ) ) ;
#5570 = AXIS2_PLACEMENT_3D ( 'NONE', #43637, #42609, #50721 ) ;
#5571 = CARTESIAN_POINT ( 'NONE',  ( 14.18747379400850051, 20.38364582413100123, -75.40982873507010709 ) ) ;
#5572 = CARTESIAN_POINT ( 'NONE',  ( 22.46012451160922652, -10.75454102864662609, -51.58399612945741808 ) ) ;
#5573 = LINE ( 'NONE', #583, #48223 ) ;
#5574 = CARTESIAN_POINT ( 'NONE',  ( 7.906922477136400396, -15.06942921146810122, -50.52879200675969429 ) ) ;
#5575 = ORIENTED_EDGE ( 'NONE', *, *, #10843, .T. ) ;
#5576 = CARTESIAN_POINT ( 'NONE',  ( 53.92255937822079659, -48.37029822198850582, -26.37636367547430183 ) ) ;
#5577 = CONICAL_SURFACE ( 'NONE', #30656, 36.50000000000000711, 0.1651486774146265213 ) ;
#5578 = CARTESIAN_POINT ( 'NONE',  ( 14.83504272149919956, -51.11618894083779452, -22.28508381815780126 ) ) ;
#5579 = CARTESIAN_POINT ( 'NONE',  ( 10.02064309493579941, 32.96920898343689998, -17.37848894768429986 ) ) ;
#5581 = EDGE_CURVE ( 'NONE', #6096, #5164, #44395, .T. ) ;
#5580 = CARTESIAN_POINT ( 'NONE',  ( 20.53618552854030099, -10.10594661162980046, -52.56174695496989102 ) ) ;
#5582 = CARTESIAN_POINT ( 'NONE',  ( 49.03396717343779443, 14.94208145987820124, -11.76399146459199940 ) ) ;
#5583 = VERTEX_POINT ( 'NONE', #43254 ) ;
#5584 = CARTESIAN_POINT ( 'NONE',  ( -7.434493659210470007, -45.51118646461110018, -5.423941065748909551 ) ) ;
#5585 = CARTESIAN_POINT ( 'NONE',  ( 47.46268832744230082, 23.38928987100490176, -54.95184613728230261 ) ) ;
#5586 = VECTOR ( 'NONE', #39667, 1000.000000000000000 ) ;
#5587 = CARTESIAN_POINT ( 'NONE',  ( 22.13393739769600188, 22.91950879131610108, -35.09469305598949518 ) ) ;
#5588 = CARTESIAN_POINT ( 'NONE',  ( 63.13746035244330557, 0.8910129994591549085, -62.32805707658469885 ) ) ;
#5589 = CARTESIAN_POINT ( 'NONE',  ( 61.05628869985170581, 14.11843175711090126, -46.88525980312950026 ) ) ;
#5590 = CARTESIAN_POINT ( 'NONE',  ( 10.98135320218699995, 33.83639044753279990, -17.57575610280199996 ) ) ;
#5591 = DIRECTION ( 'NONE',  ( 2.044963717693971196E-12, -0.08197919874685707931, 0.9966340406452226519 ) ) ;
#5592 = CARTESIAN_POINT ( 'NONE',  ( 52.96846354095290366, 18.35586996326500042, -48.76456332840299979 ) ) ;
#5593 = LINE ( 'NONE', #9526, #32519 ) ;
#5594 = CARTESIAN_POINT ( 'NONE',  ( 54.36655688846699519, -48.99971972129989695, -48.99196827366439777 ) ) ;
#5595 = CARTESIAN_POINT ( 'NONE',  ( 11.19961949155312553, 34.01496270439587732, -18.17421237848505911 ) ) ;
#5596 = CARTESIAN_POINT ( 'NONE',  ( 53.70964822437340302, 20.71768139653410046, -54.24308104583550261 ) ) ;
#5597 = CARTESIAN_POINT ( 'NONE',  ( 63.42025297602360467, 1.149536861557900247, -69.29926477292440268 ) ) ;
#5598 = CARTESIAN_POINT ( 'NONE',  ( 47.16461990496790690, 13.88381105532070059, -8.336227306136100523 ) ) ;
#5599 = ORIENTED_EDGE ( 'NONE', *, *, #5784, .F. ) ;
#5600 = DIRECTION ( 'NONE',  ( -1.000000000000000000, 0.000000000000000000, 0.000000000000000000 ) ) ;
#5601 = CARTESIAN_POINT ( 'NONE',  ( 10.14147289287149967, 31.98528096571020285, -45.99377946889909907 ) ) ;
#5602 = CARTESIAN_POINT ( 'NONE',  ( 45.82863309824571729, 13.88351055973502213, -7.494180813464123680 ) ) ;
#5603 = VECTOR ( 'NONE', #6358, 1000.000000000000114 ) ;
#5604 = CARTESIAN_POINT ( 'NONE',  ( 66.35712195075809916, -30.62653953495700065, -16.95628802592780104 ) ) ;
#5605 = DIRECTION ( 'NONE',  ( -0.6653150774959307734, 0.7465626883635315680, 0.000000000000000000 ) ) ;
#5606 = AXIS2_PLACEMENT_3D ( 'NONE', #37524, #21785, #6085 ) ;
#5607 = ORIENTED_EDGE ( 'NONE', *, *, #27539, .F. ) ;
#5608 = VERTEX_POINT ( 'NONE', #11797 ) ;
#5609 = CARTESIAN_POINT ( 'NONE',  ( 15.19691430481735139, 12.61358818065448695, -60.51477253168943804 ) ) ;
#5610 = ORIENTED_EDGE ( 'NONE', *, *, #48872, .F. ) ;
#5611 = CARTESIAN_POINT ( 'NONE',  ( 10.17097458880020078, -64.04334660451389993, -46.31317360413619610 ) ) ;
#5612 = CARTESIAN_POINT ( 'NONE',  ( 56.81616149493390111, -45.43712851969070243, -25.88809970019270068 ) ) ;
#5613 = CARTESIAN_POINT ( 'NONE',  ( 24.04470913566636625, -15.68475005675827916, -77.51042278623567938 ) ) ;
#5614 = DIRECTION ( 'NONE',  ( 1.000000000000000000, 0.000000000000000000, 0.000000000000000000 ) ) ;
#5615 = CARTESIAN_POINT ( 'NONE',  ( 61.63193477201050285, 13.93849808901580012, -46.83132799652889844 ) ) ;
#5616 = CARTESIAN_POINT ( 'NONE',  ( 63.61158869431360330, 1.412203896157240068, -62.26955982508579979 ) ) ;
#5617 = ORIENTED_EDGE ( 'NONE', *, *, #28660, .F. ) ;
#5618 = CARTESIAN_POINT ( 'NONE',  ( 45.76382685223779845, 6.896243026199304182, -61.50055243549356732 ) ) ;
#5619 = VERTEX_POINT ( 'NONE', #31161 ) ;
#5620 = CARTESIAN_POINT ( 'NONE',  ( 48.37455542296130062, -45.20184122439500385, -10.02357746685530060 ) ) ;
#5621 = CIRCLE ( 'NONE', #18995, 10.49999999999999822 ) ;
#5622 = EDGE_CURVE ( 'NONE', #39487, #20020, #16616, .T. ) ;
#5623 = DIRECTION ( 'NONE',  ( -1.000000000000000000, 0.000000000000000000, 0.000000000000000000 ) ) ;
#5624 = CARTESIAN_POINT ( 'NONE',  ( 63.34104417888273986, -63.11618894467939356, 11.14289321881345174 ) ) ;
#5625 = ADVANCED_FACE ( 'NONE', ( #39312 ), #43754, .F. ) ;
#5627 = EDGE_LOOP ( 'NONE', ( #12895, #24765 ) ) ;
#5626 =( BOUNDED_CURVE ( )  B_SPLINE_CURVE ( 3, ( #33716, #48963, #25588, #41593 ),
 .UNSPECIFIED., .F., .T. ) 
 B_SPLINE_CURVE_WITH_KNOTS ( ( 4, 4 ),
 ( 5.657409142292634030, 6.193758666985289985 ),
 .UNSPECIFIED. ) 
 CURVE ( )  GEOMETRIC_REPRESENTATION_ITEM ( )  RATIONAL_B_SPLINE_CURVE ( ( 1.000000000000000000, 0.9761707593066160094, 0.9761707593066160094, 1.000000000000000000 ) ) 
 REPRESENTATION_ITEM ( '' )  );
#5628 = EDGE_CURVE ( 'NONE', #17098, #1610, #15204, .T. ) ;
#5629 = CARTESIAN_POINT ( 'NONE',  ( 73.24758132965830271, 0.8838110553206740549, -68.78868353141480441 ) ) ;
#5630 = CARTESIAN_POINT ( 'NONE',  ( 46.99011664277529832, -54.32342547810879552, -75.47331621149609759 ) ) ;
#5631 = DIRECTION ( 'NONE',  ( 0.2260571801428030714, 0.000000000000000000, -0.9741140340359972782 ) ) ;
#5632 = AXIS2_PLACEMENT_3D ( 'NONE', #1117, #28622, #44621 ) ;
#5633 = EDGE_CURVE ( 'NONE', #29321, #48345, #50107, .T. ) ;
#5634 = CARTESIAN_POINT ( 'NONE',  ( 51.09737042232929838, 13.88381105524950065, -11.36023950572089802 ) ) ;
#5635 = DIRECTION ( 'NONE',  ( -1.000000000000000000, 0.000000000000000000, 0.000000000000000000 ) ) ;
#5636 = CARTESIAN_POINT ( 'NONE',  ( 9.443963076300310178, -17.25402591980700606, -63.77013741789689050 ) ) ;
#5637 = AXIS2_PLACEMENT_3D ( 'NONE', #28579, #37241, #17071 ) ;
#5638 = EDGE_CURVE ( 'NONE', #51719, #16095, #4261, .T. ) ;
#5639 = CARTESIAN_POINT ( 'NONE',  ( 57.64776587906369798, 14.05990909772789976, -25.94377082751820041 ) ) ;
#5640 = CARTESIAN_POINT ( 'NONE',  ( 15.64724003739100056, -7.783572915366379519, -76.76775207935759227 ) ) ;
#5641 = ORIENTED_EDGE ( 'NONE', *, *, #25101, .T. ) ;
#5642 = CARTESIAN_POINT ( 'NONE',  ( 61.75019796695539753, 13.88381105532070059, -46.37203261889099792 ) ) ;
#5643 = CARTESIAN_POINT ( 'NONE',  ( -10.53607080544539976, -41.37169853536430253, -4.264176651484540059 ) ) ;
#5644 = CARTESIAN_POINT ( 'NONE',  ( 16.13393739769609780, -15.61618894467929941, 8.449999999999999289 ) ) ;
#5646 = EDGE_CURVE ( 'NONE', #15133, #43823, #15975, .T. ) ;
#5645 = CARTESIAN_POINT ( 'NONE',  ( 72.96483387528880371, 0.9208623934721590354, -69.20867653485849758 ) ) ;
#5647 = CARTESIAN_POINT ( 'NONE',  ( 82.13853704237929776, -47.11618894467930119, -46.37203261889099792 ) ) ;
#5648 = CARTESIAN_POINT ( 'NONE',  ( 71.33393739770029640, 10.88381105532060111, -69.84999999999840270 ) ) ;
#5649 = CARTESIAN_POINT ( 'NONE',  ( 65.16938214696820353, 1.384887413063050188, -70.31636399389039127 ) ) ;
#5650 = CARTESIAN_POINT ( 'NONE',  ( 48.94619156065270005, -53.78419483245289712, -54.43336765931639576 ) ) ;
#5651 = DIRECTION ( 'NONE',  ( -1.000000000000000000, 0.000000000000000000, 0.000000000000000000 ) ) ;
#5652 = CARTESIAN_POINT ( 'NONE',  ( 76.69624363483841023, -43.19219574469177303, -14.37506098188831949 ) ) ;
#5653 = CARTESIAN_POINT ( 'NONE',  ( 18.84530626205710035, -51.72201361531850239, -74.35192203308130843 ) ) ;
#5654 = CYLINDRICAL_SURFACE ( 'NONE', #6410, 1.000000000000029976 ) ;
#5655 = VERTEX_POINT ( 'NONE', #51620 ) ;
#5656 = CARTESIAN_POINT ( 'NONE',  ( 12.93294630233359932, -8.888607629990449510, -56.42598068654719157 ) ) ;
#5657 = CARTESIAN_POINT ( 'NONE',  ( 64.00995881370980101, 1.028300555801489935, -61.29114157291949994 ) ) ;
#5658 = ORIENTED_EDGE ( 'NONE', *, *, #15743, .T. ) ;
#5659 = FACE_OUTER_BOUND ( 'NONE', #22129, .T. ) ;
#5660 = CARTESIAN_POINT ( 'NONE',  ( 60.92390599033139864, -45.64103330176020279, -47.67030853226700060 ) ) ;
#5661 = CARTESIAN_POINT ( 'NONE',  ( 21.66930937907060084, -19.98679716348209823, -75.05992337703780493 ) ) ;
#5662 = CARTESIAN_POINT ( 'NONE',  ( 21.74730038895833673, -21.19061166947408381, -61.75655418039362132 ) ) ;
#5664 = CARTESIAN_POINT ( 'NONE',  ( 15.19249895237996917, -8.626464141217111248, -54.30456343836949884 ) ) ;
#5663 = CARTESIAN_POINT ( 'NONE',  ( 44.68656668712876723, 8.775795761644557658, -63.33238661288917370 ) ) ;
#5665 = EDGE_CURVE ( 'NONE', #20377, #38000, #7604, .T. ) ;
#5666 = CYLINDRICAL_SURFACE ( 'NONE', #21768, 1.000000000000000444 ) ;
#5667 = CARTESIAN_POINT ( 'NONE',  ( 43.88907883820460398, -46.06587682131880257, -8.216673521218469389 ) ) ;
#5668 = ORIENTED_EDGE ( 'NONE', *, *, #16308, .T. ) ;
#5669 = EDGE_LOOP ( 'NONE', ( #45036, #37948, #7848, #18221, #47425 ) ) ;
#5670 = ORIENTED_EDGE ( 'NONE', *, *, #46381, .F. ) ;
#5671 = VERTEX_POINT ( 'NONE', #38803 ) ;
#5672 = CARTESIAN_POINT ( 'NONE',  ( 61.03994009699120227, -45.35937513829429690, -46.86322148818550204 ) ) ;
#5673 = FACE_OUTER_BOUND ( 'NONE', #5091, .T. ) ;
#5674 = CARTESIAN_POINT ( 'NONE',  ( 55.55115492324519266, -50.88452601480440052, -52.95812837848109211 ) ) ;
#5675 = AXIS2_PLACEMENT_3D ( 'NONE', #50524, #31094, #47123 ) ;
#5676 = ORIENTED_EDGE ( 'NONE', *, *, #17468, .F. ) ;
#5677 = ORIENTED_EDGE ( 'NONE', *, *, #2822, .F. ) ;
#5678 = CARTESIAN_POINT ( 'NONE',  ( 24.04490354837754396, -15.59228409935874637, -77.50671465413907413 ) ) ;
#5680 = CARTESIAN_POINT ( 'NONE',  ( 51.36789317581919789, -52.94755764699560530, -54.71052196913720422 ) ) ;
#5679 = VECTOR ( 'NONE', #27099, 1000.000000000000000 ) ;
#5681 = CARTESIAN_POINT ( 'NONE',  ( 14.36266333286323338, -9.025322607677731312, -53.86948819376841868 ) ) ;
#5682 = VERTEX_POINT ( 'NONE', #50847 ) ;
#5683 = CARTESIAN_POINT ( 'NONE',  ( 24.04456899842966067, -15.69869672982768982, -49.51098473570640124 ) ) ;
#5684 = CARTESIAN_POINT ( 'NONE',  ( 53.29069942456280273, -51.03998195050350262, -75.99878208018989767 ) ) ;
#5685 = EDGE_CURVE ( 'NONE', #29876, #13493, #3241, .T. ) ;
#5686 = CARTESIAN_POINT ( 'NONE',  ( 12.03477506705270095, -8.924132774964691706, -61.33755441249169849 ) ) ;
#5687 = CARTESIAN_POINT ( 'NONE',  ( -0.4410626023037970689, -22.87636857973879856, -35.14999999999999858 ) ) ;
#5688 = CARTESIAN_POINT ( 'NONE',  ( 41.29354876163589694, 13.54338451021459910, -5.375173354248380164 ) ) ;
#5689 = CARTESIAN_POINT ( 'NONE',  ( 42.08165231488229807, -44.23899420458050002, -4.969335818164180907 ) ) ;
#5690 = FACE_OUTER_BOUND ( 'NONE', #41235, .T. ) ;
#5691 = CARTESIAN_POINT ( 'NONE',  ( 16.13393739769620083, -15.61618894467929941, -35.14999999999999858 ) ) ;
#5692 = CARTESIAN_POINT ( 'NONE',  ( 63.92800470363879839, 1.456055302763120007, -69.58268673945899252 ) ) ;
#5693 = CARTESIAN_POINT ( 'NONE',  ( 22.14946380439831941, -18.71488146266838370, -32.99858898373786076 ) ) ;
#5694 = CARTESIAN_POINT ( 'NONE',  ( 65.95899839816510735, 0.8661402160289060070, -17.73196870731459995 ) ) ;
#5695 = ORIENTED_EDGE ( 'NONE', *, *, #7236, .F. ) ;
#5696 = CARTESIAN_POINT ( 'NONE',  ( 14.68717196201729891, -52.47980496485550361, -76.04476946176040997 ) ) ;
#5697 = CARTESIAN_POINT ( 'NONE',  ( 57.32763710804100299, 19.16690701097390104, -53.00790326582389866 ) ) ;
#5698 = DIRECTION ( 'NONE',  ( -0.2201775509773258865, 0.9741807197710415922, 0.04993767387456497786 ) ) ;
#5699 = DIRECTION ( 'NONE',  ( -0.7226652920947586045, -0.6911981449639438280, 0.000000000000000000 ) ) ;
#5700 = AXIS2_PLACEMENT_3D ( 'NONE', #25395, #14397, #21471 ) ;
#5701 = CARTESIAN_POINT ( 'NONE',  ( 23.21588883353000199, -14.35342990756280024, -32.14999999999999858 ) ) ;
#5702 = CARTESIAN_POINT ( 'NONE',  ( 47.77546308418789778, -54.44195670944800014, -54.82267176637049744 ) ) ;
#5703 = CARTESIAN_POINT ( 'NONE',  ( 21.11091583202307120, -9.437894192877843480, -45.22360369773933542 ) ) ;
#5704 = CARTESIAN_POINT ( 'NONE',  ( 47.91428909763650523, 23.15602325637470216, -54.91125936546870179 ) ) ;
#5705 = VERTEX_POINT ( 'NONE', #3155 ) ;
#5706 = CARTESIAN_POINT ( 'NONE',  ( 11.87323508191540000, -21.23659595402939715, -65.55365164940349132 ) ) ;
#5707 = ORIENTED_EDGE ( 'NONE', *, *, #19220, .F. ) ;
#5708 = CARTESIAN_POINT ( 'NONE',  ( 68.13393739769618662, -0.5161889446793590519, -81.65000000000000568 ) ) ;
#5709 = CARTESIAN_POINT ( 'NONE',  ( 14.36277100459635570, -22.20708315903983987, -43.03615330968553820 ) ) ;
#5711 = CARTESIAN_POINT ( 'NONE',  ( 52.90929476643909624, 18.25992211886340044, -27.14407627714519933 ) ) ;
#5710 = CARTESIAN_POINT ( 'NONE',  ( 84.20053740572899414, 12.88281201546480048, -47.28523898137510173 ) ) ;
#5712 = EDGE_CURVE ( 'NONE', #49951, #40988, #35103, .T. ) ;
#5713 = CARTESIAN_POINT ( 'NONE',  ( 15.81768230162860078, -8.570442610110308834, -77.93854215477199432 ) ) ;
#5714 = CARTESIAN_POINT ( 'NONE',  ( 82.13853704237929776, -45.64188066427789892, -47.72348187592560009 ) ) ;
#5715 = CARTESIAN_POINT ( 'NONE',  ( 57.50723796700749801, -45.11618894467940066, -17.93020416573320119 ) ) ;
#5716 = CARTESIAN_POINT ( 'NONE',  ( 56.48921795443543203, -46.16653356619494275, -26.24159223014568099 ) ) ;
#5717 = CARTESIAN_POINT ( 'NONE',  ( 53.63393739769619373, 21.88381105532059934, 17.35000000000000142 ) ) ;
#5718 = EDGE_CURVE ( 'NONE', #8182, #39508, #34183, .T. ) ;
#5719 = VERTEX_POINT ( 'NONE', #32696 ) ;
#5720 = ORIENTED_EDGE ( 'NONE', *, *, #26420, .F. ) ;
#5721 = EDGE_CURVE ( 'NONE', #40328, #51550, #26223, .T. ) ;
#5722 = CARTESIAN_POINT ( 'NONE',  ( 12.09990282912350068, -65.24532120969969640, -16.83009741455080288 ) ) ;
#5723 = CARTESIAN_POINT ( 'NONE',  ( 12.29700469235899973, 34.12962537319510403, -46.90718399448299891 ) ) ;
#5724 = DIRECTION ( 'NONE',  ( -1.062456999999999985E-16, -7.719205000000000365E-17, -1.000000000000000000 ) ) ;
#5725 = CARTESIAN_POINT ( 'NONE',  ( -26.88703640771693770, 10.64567781361937904, -56.26548710561206690 ) ) ;
#5726 = LINE ( 'NONE', #21431, #14238 ) ;
#5727 = EDGE_LOOP ( 'NONE', ( #41639, #51018, #5489, #36896 ) ) ;
#5728 = CARTESIAN_POINT ( 'NONE',  ( -3.808086725916260296, -49.05426427394600353, -38.11425470904319468 ) ) ;
#5729 = FACE_OUTER_BOUND ( 'NONE', #31231, .T. ) ;
#5730 = CARTESIAN_POINT ( 'NONE',  ( 52.74159186887090556, 18.44087211712770014, -48.34114423306549924 ) ) ;
#5731 = CARTESIAN_POINT ( 'NONE',  ( 59.22431762257839694, -3.120768426202699786, -15.66519454250340004 ) ) ;
#5732 = B_SPLINE_CURVE_WITH_KNOTS ( 'NONE', 3,
 ( #51339, #35605, #924, #16921, #3901, #35857, #32863, #3128, #31133, #39035, #51846, #35072, #12025, #15950, #31903, #47923, #27977, #47161, #25528, #25783, #25270, #50181, #38126, #41531, #41791, #22115, #1445, #33910 ),
 .UNSPECIFIED., .F., .F.,
 ( 4, 2, 2, 2, 2, 2, 2, 2, 2, 2, 2, 2, 2, 4 ),
 ( 0.000000000000000000, 0.03124990345073212078, 0.06249980690146424156, 0.09374971035219635540, 0.1249996138029284831, 0.1562495172536605970, 0.1874994207043927108, 0.2187493241551248246, 0.2499992276058569662, 0.2812491310565890523, 0.3124990345073211939, 0.3749988414087853106, 0.4374986483102494272, 0.4999984552117135994 ),
 .UNSPECIFIED. ) ;
#5733 = CARTESIAN_POINT ( 'NONE',  ( 51.34919179766620090, -49.60438797113280174, -76.46527068533909244 ) ) ;
#5734 = CARTESIAN_POINT ( 'NONE',  ( 56.48499257286630382, -50.43009329692559817, -52.75538019139929702 ) ) ;
#5735 = VERTEX_POINT ( 'NONE', #4685 ) ;
#5736 = CARTESIAN_POINT ( 'NONE',  ( 17.90525091854434692, -9.025334375736962400, -68.03615214762757546 ) ) ;
#5737 = CARTESIAN_POINT ( 'NONE',  ( 65.43393739769584272, 16.88381105531917825, -74.20000000000047180 ) ) ;
#5738 = ORIENTED_EDGE ( 'NONE', *, *, #33227, .F. ) ;
#5739 = CARTESIAN_POINT ( 'NONE',  ( 22.46009513736006369, -10.75450071354899428, -53.58400066563606856 ) ) ;
#5740 = CIRCLE ( 'NONE', #44223, 3.000000000000003997 ) ;
#5741 = CARTESIAN_POINT ( 'NONE',  ( 60.23130391297029718, 14.55066440145539985, -47.24246919202519734 ) ) ;
#5742 = EDGE_CURVE ( 'NONE', #33786, #48345, #12302, .T. ) ;
#5743 = CARTESIAN_POINT ( 'NONE',  ( 12.17215262800660014, -22.39047924184240301, -38.68094012829649841 ) ) ;
#5744 = CARTESIAN_POINT ( 'NONE',  ( 13.85787483888649874, -51.20742914540719681, -22.56068819944239934 ) ) ;
#5745 = CARTESIAN_POINT ( 'NONE',  ( 56.68181436161830078, 19.46489750539030084, -74.32030992971661476 ) ) ;
#5746 = TOROIDAL_SURFACE ( 'NONE', #39223, 18.00000000000000000, 2.000000000000000000 ) ;
#5747 = CARTESIAN_POINT ( 'NONE',  ( 47.63732208602310436, -54.52964753308490486, -74.36335264244719667 ) ) ;
#5748 = ORIENTED_EDGE ( 'NONE', *, *, #4296, .T. ) ;
#5749 = CARTESIAN_POINT ( 'NONE',  ( 55.49736661512110203, 14.70425851891470082, -16.59168144405439804 ) ) ;
#5750 = CARTESIAN_POINT ( 'NONE',  ( -21.86606260230379561, -15.61618894467929231, 6.349999999999999645 ) ) ;
#5751 = CARTESIAN_POINT ( 'NONE',  ( 56.94695455049200206, -50.48167892581339800, -53.05466020099660085 ) ) ;
#5752 = LINE ( 'NONE', #25897, #23854 ) ;
#5753 = DIRECTION ( 'NONE',  ( 0.7702700562048789834, 0.6377178376948009486, -1.693090112579540101E-15 ) ) ;
#5754 = CARTESIAN_POINT ( 'NONE',  ( 47.30207934339009768, 23.19015752006689723, -75.11580175282739447 ) ) ;
#5755 = CARTESIAN_POINT ( 'NONE',  ( 65.02006347151939281, 1.101170701158060039, -60.57405794295090118 ) ) ;
#5756 = CARTESIAN_POINT ( 'NONE',  ( 60.62539537963965586, -45.77966094345966042, -47.75584023230192088 ) ) ;
#5757 = CARTESIAN_POINT ( 'NONE',  ( 8.428886257399922144, -13.54533162025536441, -56.87566481798235429 ) ) ;
#5758 = CARTESIAN_POINT ( 'NONE',  ( 29.11900864776890074, -4.497910611074960485, -35.02873218748179340 ) ) ;
#5759 = CARTESIAN_POINT ( 'NONE',  ( 17.64603583078074678, -49.61617097760094452, -83.18933379702824027 ) ) ;
#5760 = CARTESIAN_POINT ( 'NONE',  ( 53.63393739769619373, -53.11618894467930119, 10.84999999999999964 ) ) ;
#5762 = CARTESIAN_POINT ( 'NONE',  ( 46.94493346192469119, -39.32255388986889955, -55.87925509191032347 ) ) ;
#5761 = CARTESIAN_POINT ( 'NONE',  ( 8.133937397696209715, 28.10308010054979988, -21.14999999999999858 ) ) ;
#5763 = CARTESIAN_POINT ( 'NONE',  ( 61.16115695917979878, 14.06348816002850022, -46.76869981922120445 ) ) ;
#5764 = CARTESIAN_POINT ( 'NONE',  ( 14.34417029198879945, -52.11618894467940066, -23.15000000000000213 ) ) ;
#5765 = CARTESIAN_POINT ( 'NONE',  ( -0.2991137081852789925, 30.89086735222949898, -48.78634498590000135 ) ) ;
#5766 = VERTEX_POINT ( 'NONE', #44522 ) ;
#5767 = CARTESIAN_POINT ( 'NONE',  ( 53.40532901998560789, -49.36081156069519693, -48.82229769749290682 ) ) ;
#5768 = ORIENTED_EDGE ( 'NONE', *, *, #43490, .F. ) ;
#5769 = VECTOR ( 'NONE', #18751, 1000.000000000000000 ) ;
#5770 = CARTESIAN_POINT ( 'NONE',  ( 61.33704255976599740, -45.11618898598639760, -27.03744896294960043 ) ) ;
#5771 = CARTESIAN_POINT ( 'NONE',  ( 23.93344121396042823, -16.98588554008669149, -65.84766514592809017 ) ) ;
#5772 = CARTESIAN_POINT ( 'NONE',  ( 13.64409289200350095, 19.76484905899049949, -21.86436953804059868 ) ) ;
#5773 = CARTESIAN_POINT ( 'NONE',  ( 56.30911185033799882, 14.37708950283650111, -25.70913536183260462 ) ) ;
#5774 = CARTESIAN_POINT ( 'NONE',  ( 22.15074124698030289, -19.29594846615139758, -48.62753766123279320 ) ) ;
#5776 = LINE ( 'NONE', #10491, #49224 ) ;
#5775 = AXIS2_PLACEMENT_3D ( 'NONE', #6244, #10174, #17771 ) ;
#5777 = CARTESIAN_POINT ( 'NONE',  ( 52.75373265657299982, 18.47785976625320004, -48.68700065433350233 ) ) ;
#5778 = CARTESIAN_POINT ( 'NONE',  ( 64.78392625511199299, 1.096932441169210071, -60.71856768636379797 ) ) ;
#5779 = CARTESIAN_POINT ( 'NONE',  ( 60.91431180673350809, -45.42519531869549354, -47.01365133320230427 ) ) ;
#5780 = CARTESIAN_POINT ( 'NONE',  ( 73.61871130914850880, -44.95982266748999479, -13.93477351660789942 ) ) ;
#5781 = ADVANCED_FACE ( 'NONE', ( #32181 ), #32434, .T. ) ;
#5782 = ORIENTED_EDGE ( 'NONE', *, *, #28170, .T. ) ;
#5783 = CARTESIAN_POINT ( 'NONE',  ( 15.67188839633519848, -8.180248852217671285, -76.54758917670659457 ) ) ;
#5784 = EDGE_CURVE ( 'NONE', #5413, #3924, #44991, .T. ) ;
#5785 = CARTESIAN_POINT ( 'NONE',  ( 73.11834175676820280, 0.9272522097098119254, -68.99005086130968323 ) ) ;
#5786 = CARTESIAN_POINT ( 'NONE',  ( 47.53365938598520302, -54.56237310633869697, -54.69765973086329325 ) ) ;
#5787 = LINE ( 'NONE', #49815, #9464 ) ;
#5788 = CARTESIAN_POINT ( 'NONE',  ( 72.85248830348810145, 1.369535599030039963, -62.52785204568030508 ) ) ;
#5789 = CARTESIAN_POINT ( 'NONE',  ( 10.81643727139639921, -64.95351341576260040, -17.63284883035869655 ) ) ;
#5790 = CARTESIAN_POINT ( 'NONE',  ( 71.58938403497960223, 1.005545696829380109, -60.75297091621269630 ) ) ;
#5791 = LINE ( 'NONE', #42474, #14115 ) ;
#5792 = CARTESIAN_POINT ( 'NONE',  ( 8.222290034161709116, -15.61613760572089937, -44.79233150823699816 ) ) ;
#5793 = DIRECTION ( 'NONE',  ( -0.05023550054956202326, 0.000000000000000000, -0.9987374001630934250 ) ) ;
#5794 = ORIENTED_EDGE ( 'NONE', *, *, #27742, .F. ) ;
#5795 = CARTESIAN_POINT ( 'NONE',  ( 65.00985940095789317, 1.385702546077159925, -70.29781821095090777 ) ) ;
#5796 = ORIENTED_EDGE ( 'NONE', *, *, #2459, .T. ) ;
#5797 = CARTESIAN_POINT ( 'NONE',  ( 8.799470649396189614, -63.19223985362448559, -46.67016919464409597 ) ) ;
#5798 = CARTESIAN_POINT ( 'NONE',  ( 17.92370450339619836, 19.88381105532299742, -74.14999999999999147 ) ) ;
#5799 = ORIENTED_EDGE ( 'NONE', *, *, #18962, .T. ) ;
#5800 = CARTESIAN_POINT ( 'NONE',  ( 0.1457841021255935343, -8.319710351909083812, -34.68167779225149161 ) ) ;
#5801 = CARTESIAN_POINT ( 'NONE',  ( 24.04464518807997919, -15.61618401921712618, -71.50767245506341396 ) ) ;
#5802 = CARTESIAN_POINT ( 'NONE',  ( 24.04493740294731552, -16.65173115070739840, -69.54933814134879810 ) ) ;
#5803 = CARTESIAN_POINT ( 'NONE',  ( 51.73525796840619506, 19.20063007591929960, -76.36782568579080532 ) ) ;
#5804 = ORIENTED_EDGE ( 'NONE', *, *, #46017, .T. ) ;
#5805 = FACE_OUTER_BOUND ( 'NONE', #42276, .T. ) ;
#5806 = DIRECTION ( 'NONE',  ( -0.7071067811865511255, -0.7071067811865440200, 0.000000000000000000 ) ) ;
#5807 = CARTESIAN_POINT ( 'NONE',  ( 23.13393739769620083, -2.337132753317950229, -39.64999999999999858 ) ) ;
#5808 = ADVANCED_FACE ( 'NONE', ( #4429 ), #20398, .T. ) ;
#5809 = CARTESIAN_POINT ( 'NONE',  ( 21.39045294677319831, -9.263885084012120075, -53.51237412773329538 ) ) ;
#5810 = DIRECTION ( 'NONE',  ( 1.000000000000000000, 0.000000000000000000, 0.000000000000000000 ) ) ;
#5811 = CARTESIAN_POINT ( 'NONE',  ( 45.70030952488608733, -38.12153290717493093, -61.81813589282543120 ) ) ;
#5812 = ADVANCED_FACE ( 'NONE', ( #40078 ), #39343, .T. ) ;
#5813 = ORIENTED_EDGE ( 'NONE', *, *, #21013, .F. ) ;
#5814 = AXIS2_PLACEMENT_3D ( 'NONE', #16238, #48733, #16492 ) ;
#5815 = CYLINDRICAL_SURFACE ( 'NONE', #50148, 0.9999999999999407141 ) ;
#5816 = CARTESIAN_POINT ( 'NONE',  ( 19.86268612959200297, -22.06623752585539933, -48.56581262070909588 ) ) ;
#5817 = VECTOR ( 'NONE', #14003, 1000.000000000000000 ) ;
#5818 = CIRCLE ( 'NONE', #48458, 0.5000000000000018874 ) ;
#5819 = CARTESIAN_POINT ( 'NONE',  ( 9.071496094108649544, -18.06536394266180068, -32.14999999999999858 ) ) ;
#5820 = CIRCLE ( 'NONE', #8314, 1.000000000000000888 ) ;
#5821 = CARTESIAN_POINT ( 'NONE',  ( 13.90784298899419902, 20.26946707534090208, -75.09610479291009710 ) ) ;
#5822 = CARTESIAN_POINT ( 'NONE',  ( 17.71568204744891517, -51.70197554413384466, -75.56421372420066973 ) ) ;
#5823 = CARTESIAN_POINT ( 'NONE',  ( 44.26786790321339993, -45.40684719649339485, -7.720938881823640187 ) ) ;
#5824 = CARTESIAN_POINT ( 'NONE',  ( 24.04493739770204641, -15.61617025106582446, -61.50767538883729912 ) ) ;
#5825 = CARTESIAN_POINT ( 'NONE',  ( 22.95508758428769625, -20.24810332654539735, -53.69754924930440154 ) ) ;
#5826 = ORIENTED_EDGE ( 'NONE', *, *, #51702, .F. ) ;
#5827 = CARTESIAN_POINT ( 'NONE',  ( 53.39205224544679851, -48.96840769728560616, -26.76104151705999712 ) ) ;
#5828 = B_SPLINE_CURVE_WITH_KNOTS ( 'NONE', 3,
 ( #16361, #4829, #24457, #17151, #33104, #48083, #7987, #20797, #632, #23938 ),
 .UNSPECIFIED., .F., .F.,
 ( 4, 1, 1, 1, 1, 1, 1, 4 ),
 ( 0.5000038964883081194, 0.5639822375181338110, 0.6432011685817549118, 0.7224200996453765677, 0.8016390307090128786, 0.8808579617726346456, 0.9600768928362556354, 1.000000000000000000 ),
 .UNSPECIFIED. ) ;
#5829 = CARTESIAN_POINT ( 'NONE',  ( 16.50882131665070318, -51.11266530063170421, -20.29200666522890018 ) ) ;
#5831 = DIRECTION ( 'NONE',  ( 0.000000000000000000, 0.000000000000000000, 1.000000000000000000 ) ) ;
#5830 = CARTESIAN_POINT ( 'NONE',  ( 10.88039558896599956, 33.80616322986560363, -17.65320609993409917 ) ) ;
#5832 = CARTESIAN_POINT ( 'NONE',  ( 9.367272718592845493, -14.60504838226429314, -69.89475711886211684 ) ) ;
#5833 = CARTESIAN_POINT ( 'NONE',  ( 51.35061793337657576, 19.88840392264928880, -50.03559567676038711 ) ) ;
#5834 = ORIENTED_EDGE ( 'NONE', *, *, #40349, .F. ) ;
#5835 = CARTESIAN_POINT ( 'NONE',  ( -3.971359608989250223, -47.88178280679790078, -4.564193690396530556 ) ) ;
#5836 = CARTESIAN_POINT ( 'NONE',  ( 47.49598700288770203, 23.35309783937709938, -54.68536711013020124 ) ) ;
#5837 = CARTESIAN_POINT ( 'NONE',  ( -11.80944000494499768, -34.05870648691990255, -45.03554556751409166 ) ) ;
#5838 = CARTESIAN_POINT ( 'NONE',  ( 63.47556362806851382, 1.384708701328919878, -62.55544205298410532 ) ) ;
#5839 = CARTESIAN_POINT ( 'NONE',  ( 60.80448350504249788, 14.25485008339019899, -47.16347503790071016 ) ) ;
#5840 = CARTESIAN_POINT ( 'NONE',  ( 11.90855646482910046, 33.99907130593510374, -16.85546526172750248 ) ) ;
#5841 = CARTESIAN_POINT ( 'NONE',  ( 52.23706089893619975, 18.52650580724129981, -77.18592072748609212 ) ) ;
#5842 = CARTESIAN_POINT ( 'NONE',  ( 52.89416328055860106, 18.39479795143680008, -48.70339646180270421 ) ) ;
#5843 = DIRECTION ( 'NONE',  ( 0.000000000000000000, -1.000000000000000000, 0.000000000000000000 ) ) ;
#5844 = CARTESIAN_POINT ( 'NONE',  ( 57.22447440519270145, -47.50261249455419232, -48.27822118512559513 ) ) ;
#5845 = CARTESIAN_POINT ( 'NONE',  ( 9.975091091254757458, -18.47606888634118150, -67.31448443351787603 ) ) ;
#5846 = EDGE_CURVE ( 'NONE', #49949, #41228, #10049, .T. ) ;
#5847 = CARTESIAN_POINT ( 'NONE',  ( 52.09210036518850018, 21.29014856838869818, -53.85655248009329910 ) ) ;
#5848 = CARTESIAN_POINT ( 'NONE',  ( 63.71146986217769381, 1.338416928215059976, -69.52371897276981372 ) ) ;
#5849 = CONICAL_SURFACE ( 'NONE', #19228, 20.98392344168889778, 0.7480182347898678419 ) ;
#5850 = LINE ( 'NONE', #1915, #23224 ) ;
#5851 = ORIENTED_EDGE ( 'NONE', *, *, #42422, .F. ) ;
#5852 = CARTESIAN_POINT ( 'NONE',  ( 71.25019707560579718, 0.9212109678634080590, -60.52272727272730179 ) ) ;
#5853 = CARTESIAN_POINT ( 'NONE',  ( 10.49390830983270106, 32.10632801932060687, -45.62647078093240083 ) ) ;
#5854 = DIRECTION ( 'NONE',  ( -1.000000000000000000, 0.000000000000000000, 0.000000000000000000 ) ) ;
#5855 = AXIS2_PLACEMENT_3D ( 'NONE', #22836, #18917, #31981 ) ;
#5856 = CARTESIAN_POINT ( 'NONE',  ( 65.81143242515639713, -32.80576248147190199, -18.80816254862149961 ) ) ;
#5857 = DIRECTION ( 'NONE',  ( -1.000000000000000000, 0.000000000000000000, 0.000000000000000000 ) ) ;
#5858 = VERTEX_POINT ( 'NONE', #36914 ) ;
#5859 = ORIENTED_EDGE ( 'NONE', *, *, #27076, .T. ) ;
#5860 = CARTESIAN_POINT ( 'NONE',  ( 8.222872596472118545, -15.61638977992110000, -80.50766849176289952 ) ) ;
#5861 = ORIENTED_EDGE ( 'NONE', *, *, #48203, .T. ) ;
#5862 = CARTESIAN_POINT ( 'NONE',  ( 11.09507093703399860, -63.56477272120999800, -44.34938846766090137 ) ) ;
#5863 = CARTESIAN_POINT ( 'NONE',  ( 56.86965732674089935, -45.75598051248179843, -26.16748850934180126 ) ) ;
#5864 = FACE_OUTER_BOUND ( 'NONE', #36642, .T. ) ;
#5865 = FACE_OUTER_BOUND ( 'NONE', #12472, .T. ) ;
#5866 = ORIENTED_EDGE ( 'NONE', *, *, #31602, .T. ) ;
#5867 = CARTESIAN_POINT ( 'NONE',  ( 46.52998719834516805, 6.974158363553319973, -57.66974223607722649 ) ) ;
#5868 = ORIENTED_EDGE ( 'NONE', *, *, #40978, .F. ) ;
#5869 = CARTESIAN_POINT ( 'NONE',  ( 50.84007792687270211, -45.59127768917590373, -12.55259730091349901 ) ) ;
#5870 = CARTESIAN_POINT ( 'NONE',  ( 8.672104946893240296, -18.33092530368449502, -34.68117512106212530 ) ) ;
#5871 = CARTESIAN_POINT ( 'NONE',  ( 15.72113303934720108, 19.87699618195869888, -21.50711442615470048 ) ) ;
#5872 = EDGE_CURVE ( 'NONE', #13261, #11543, #43105, .T. ) ;
#5873 = CARTESIAN_POINT ( 'NONE',  ( 50.95939078474919626, -32.48240620400619605, -76.37902184192930122 ) ) ;
#5874 = EDGE_LOOP ( 'NONE', ( #13827, #14612, #32067, #43067, #43760, #44425 ) ) ;
#5875 = CARTESIAN_POINT ( 'NONE',  ( 73.26121012496899709, 0.8838110553206759423, -68.76625967790960203 ) ) ;
#5876 = CARTESIAN_POINT ( 'NONE',  ( 47.08375996125450058, -54.42988687340879750, -75.29488275581999801 ) ) ;
#5877 = CARTESIAN_POINT ( 'NONE',  ( 61.59958201630909969, 13.73326013108119881, -10.58817094626940047 ) ) ;
#5878 = CARTESIAN_POINT ( 'NONE',  ( 50.90853148534860395, -50.90159658081540073, -76.14999999999999147 ) ) ;
#5879 = CARTESIAN_POINT ( 'NONE',  ( 52.59105628395929699, 20.91324755812640035, -53.43271834460720271 ) ) ;
#5880 = AXIS2_PLACEMENT_3D ( 'NONE', #47330, #11421, #27386 ) ;
#5881 = CIRCLE ( 'NONE', #31816, 1.999999999999996669 ) ;
#5882 = AXIS2_PLACEMENT_3D ( 'NONE', #5285, #48265, #16541 ) ;
#5883 = CARTESIAN_POINT ( 'NONE',  ( 52.46419965653649342, 19.96388597204279947, -75.99844946084689923 ) ) ;
#5884 = CARTESIAN_POINT ( 'NONE',  ( 57.36436529245580118, 14.21344931724819993, -26.07125751596730012 ) ) ;
#5885 = AXIS2_PLACEMENT_3D ( 'NONE', #20518, #17389, #36512 ) ;
#5886 = AXIS2_PLACEMENT_3D ( 'NONE', #41970, #2383, #5557 ) ;
#5887 = CARTESIAN_POINT ( 'NONE',  ( 22.12508014151499935, -10.54736691127049930, -71.06398904277699557 ) ) ;
#5888 = B_SPLINE_SURFACE_WITH_KNOTS ( 'NONE', 3, 3, ( 
 ( #1978, #30259, #10366, #24111, #20451, #48004, #8426, #12351, #35691, #3981, #28316, #35934, #8681 ),
 ( #44317, #27811, #4225, #48779, #546, #43811, #8167, #36441, #43560, #19699, #31984, #16028, #53 ),
 ( #24373, #24633, #3727, #12103, #40388, #23604, #4482, #51675, #15769, #28060, #31723, #7909, #16533 ),
 ( #44063, #16804, #40131, #47748, #48257, #32485, #48513, #23859, #7661, #28577, #12617, #20201, #36188 ),
 ( #20711, #44577, #32753, #40646, #27552, #4744, #298, #36702, #16280, #11856, #32234, #39882, #804 ),
 ( #39624, #19944, #5786, #41419, #21229, #25417, #17830, #17069, #49567, #1072, #33021, #37239, #5537 ),
 ( #9469, #21492, #1852, #21746, #24891, #36975, #49306, #13152, #5014, #37492, #25159, #13401, #29359 ),
 ( #29102, #44844, #12885, #40904, #37754, #33290, #1592, #33803, #45100, #33550, #1337, #25676, #45365 ),
 ( #41166, #17580, #13653, #49814, #45617, #41678, #29614, #9717, #13906, #17327, #9207, #49046, #5278 ),
 ( #28841, #8949, #20976, #40556, #28227, #40045, #24023, #43973, #28749, #36882, #36104, #16188, #983 ),
 ( #19858, #32929, #47913, #24804, #32661, #207, #28490, #20363, #24282, #48957, #8329, #8594, #8077 ),
 ( #20887, #40302, #24538, #4914, #32147, #16705, #48691, #4136, #12016, #48423, #48164, #461, #31896 ),
 ( #16982, #8854, #12266, #40815, #36609, #44229, #36350, #12793, #12524, #44748, #13060, #4647, #20621 ),
 ( #29013, #39787, #32401, #7822, #23774, #3893, #35849, #20111, #715, #4393, #51839, #16447, #44491 ),
 ( #15938, #27969, #37402, #25326, #9111, #33453, #33710, #13563, #37921, #10141, #21142, #14324, #1503 ),
 ( #29527, #13813, #2274, #29267, #2015, #13308, #45269, #45530, #45790, #29772, #49725, #9879, #38180 ) ),
 .UNSPECIFIED., .F., .F., .F.,
 ( 4, 2, 2, 2, 2, 2, 2, 4 ),
 ( 4, 1, 1, 1, 1, 1, 1, 1, 1, 1, 4 ),
 ( -1.191294110796560002, -0.9822786339451109461, -0.7434038032577410249, -0.5941070340781360315, -0.5194586494883330907, -0.4000212341446480191, -0.2089213695947530203, 0.003080042640286999919 ),
 ( 0.000000000000000000, 0.1000000000000000056, 0.2000000000000000111, 0.2999999999999999889, 0.4000000000000000222, 0.5000000000000000000, 0.5999999999999999778, 0.6999999999999999556, 0.8000000000000000444, 0.9000000000000000222, 1.000000000000000000 ),
 .UNSPECIFIED. ) ;
#5889 = ORIENTED_EDGE ( 'NONE', *, *, #18096, .T. ) ;
#5890 = CARTESIAN_POINT ( 'NONE',  ( 11.60944838831535897, -10.20586932579674944, -48.12548681540801709 ) ) ;
#5891 = CARTESIAN_POINT ( 'NONE',  ( 73.16133767175010405, 0.8879664753683469414, -62.37500410124779648 ) ) ;
#5892 = CARTESIAN_POINT ( 'NONE',  ( 75.41176871543700599, -41.13033092184089412, -13.09038441766009875 ) ) ;
#5893 = CARTESIAN_POINT ( 'NONE',  ( 72.69742484592399023, 1.402336724396409995, -68.91862208776170462 ) ) ;
#5894 = CARTESIAN_POINT ( 'NONE',  ( 3.987490788289483667, -22.62894316431776787, -34.79644660940672907 ) ) ;
#5895 = DIRECTION ( 'NONE',  ( -0.8660254037844390407, -0.4999999999999995004, -5.551115123125774074E-17 ) ) ;
#5896 = CARTESIAN_POINT ( 'NONE',  ( 19.54191009578054050, -21.52911156565832940, -78.78615145789616747 ) ) ;
#5897 = DIRECTION ( 'NONE',  ( -0.8090169943749453418, 0.5877852522924759127, 0.000000000000000000 ) ) ;
#5898 = CARTESIAN_POINT ( 'NONE',  ( 51.23914219048663909, -31.75230732063590011, -17.21756681101922126 ) ) ;
#5899 = EDGE_CURVE ( 'NONE', #6210, #27765, #13847, .T. ) ;
#5900 = CARTESIAN_POINT ( 'NONE',  ( 37.86285195093699940, -15.61618894467929763, 9.349999999999999645 ) ) ;
#5901 = CARTESIAN_POINT ( 'NONE',  ( 68.13393739769620083, 0.8838110553206759423, -65.65000000000000568 ) ) ;
#5902 = CIRCLE ( 'NONE', #35191, 3.000000000000003997 ) ;
#5903 = ORIENTED_EDGE ( 'NONE', *, *, #26068, .F. ) ;
#5904 = EDGE_CURVE ( 'NONE', #17310, #362, #46045, .T. ) ;
#5905 = CARTESIAN_POINT ( 'NONE',  ( 14.24329851705899941, -8.409790471005749168, -58.48567289420139304 ) ) ;
#5906 = EDGE_CURVE ( 'NONE', #11807, #12367, #5726, .T. ) ;
#5907 = CARTESIAN_POINT ( 'NONE',  ( 63.86181505067950326, 1.033004162168289941, -61.43684260791489748 ) ) ;
#5908 = ORIENTED_EDGE ( 'NONE', *, *, #984, .F. ) ;
#5909 = CARTESIAN_POINT ( 'NONE',  ( 60.61386341819070367, -45.76930238140869989, -47.73570512132659616 ) ) ;
#5910 = CARTESIAN_POINT ( 'NONE',  ( 9.367848958511704183, -14.88152289001418715, -73.88173930325579875 ) ) ;
#5911 = CARTESIAN_POINT ( 'NONE',  ( 22.38196252458151037, -20.47457147835186575, -61.71802975325617524 ) ) ;
#5913 = CARTESIAN_POINT ( 'NONE',  ( 8.222623404330700936, -15.61601543569009820, -34.79233150823699816 ) ) ;
#5912 = CARTESIAN_POINT ( 'NONE',  ( 45.05098064268191393, 8.801720613440462415, -61.56528120495866574 ) ) ;
#5914 = EDGE_CURVE ( 'NONE', #34588, #5583, #43532, .T. ) ;
#5915 = CARTESIAN_POINT ( 'NONE',  ( 71.33393739769790898, 11.38381099282070075, -62.44999999999869544 ) ) ;
#5916 = CARTESIAN_POINT ( 'NONE',  ( 45.01569400174280133, -46.01157251195749609, -8.915078500992239086 ) ) ;
#5917 = ORIENTED_EDGE ( 'NONE', *, *, #35453, .T. ) ;
#5918 = VERTEX_POINT ( 'NONE', #49756 ) ;
#5919 = ORIENTED_EDGE ( 'NONE', *, *, #13821, .F. ) ;
#5920 = CARTESIAN_POINT ( 'NONE',  ( 61.39588016320150388, -45.18041509599279948, -46.37196697359190267 ) ) ;
#5922 = CARTESIAN_POINT ( 'NONE',  ( 53.36596843580329619, -49.48455262995090465, -49.20806672364570034 ) ) ;
#5921 = VECTOR ( 'NONE', #37323, 1000.000000000000000 ) ;
#5923 = CARTESIAN_POINT ( 'NONE',  ( 61.09347322899138533, 14.24408283890917204, -47.46698883568873129 ) ) ;
#5924 =( BOUNDED_CURVE ( )  B_SPLINE_CURVE ( 3, ( #20149, #12055, #24319, #44265 ),
 .UNSPECIFIED., .F., .T. ) 
 B_SPLINE_CURVE_WITH_KNOTS ( ( 4, 4 ),
 ( 0.9533855775336180782, 1.098605931781428069 ),
 .UNSPECIFIED. ) 
 CURVE ( )  GEOMETRIC_REPRESENTATION_ITEM ( )  RATIONAL_B_SPLINE_CURVE ( ( 1.000000000000000000, 0.9982433593817650053, 0.9982433593817650053, 1.000000000000000000 ) ) 
 REPRESENTATION_ITEM ( '' )  );
#5925 = CARTESIAN_POINT ( 'NONE',  ( 17.63393739769620083, -32.58675169315650066, -35.14999999999999858 ) ) ;
#5926 = AXIS2_PLACEMENT_3D ( 'NONE', #17050, #33004, #29083 ) ;
#5927 = ORIENTED_EDGE ( 'NONE', *, *, #45444, .F. ) ;
#5928 = CIRCLE ( 'NONE', #35204, 6.099999999999994316 ) ;
#5929 = ORIENTED_EDGE ( 'NONE', *, *, #16241, .T. ) ;
#5930 = LINE ( 'NONE', #2255, #10981 ) ;
#5931 = CARTESIAN_POINT ( 'NONE',  ( 51.82317580592130213, -52.75362460619960103, -54.60923380648279846 ) ) ;
#5932 = ADVANCED_FACE ( 'NONE', ( #2306 ), #34248, .T. ) ;
#5933 = PLANE ( 'NONE',  #23392 ) ;
#5934 = ORIENTED_EDGE ( 'NONE', *, *, #10066, .T. ) ;
#5935 = B_SPLINE_CURVE_WITH_KNOTS ( 'NONE', 3,
 ( #49435, #42340, #1723, #46019, #18480, #22397, #33417, #26585 ),
 .UNSPECIFIED., .F., .F.,
 ( 4, 2, 2, 4 ),
 ( 0.08616863070422620119, 0.1028498217474689974, 0.1208689123377440083, 0.1272047750358668849 ),
 .UNSPECIFIED. ) ;
#5936 = CARTESIAN_POINT ( 'NONE',  ( 15.98649569970556072, 19.77667957984293423, -15.66524362255343839 ) ) ;
#5937 = CARTESIAN_POINT ( 'NONE',  ( 52.48374445785739795, -50.75964131328780127, -76.33825989612010687 ) ) ;
#5938 = CARTESIAN_POINT ( 'NONE',  ( 7.441840577107678101, -61.50537939366137152, -19.49871569355901002 ) ) ;
#5939 = CARTESIAN_POINT ( 'NONE',  ( 20.40563007449969746, -9.032923093559031003, -73.69570765841629623 ) ) ;
#5940 = CARTESIAN_POINT ( 'NONE',  ( 51.67587649748560352, 17.38381105532069881, -77.01363636363639387 ) ) ;
#5941 = CARTESIAN_POINT ( 'NONE',  ( 41.30531720498969861, 13.54650839412840035, -5.382424522816090295 ) ) ;
#5942 = CARTESIAN_POINT ( 'NONE',  ( 42.13038056454769986, -43.33336100108030564, -3.383138906590309691 ) ) ;
#5943 = CARTESIAN_POINT ( 'NONE',  ( -21.36606260230379917, -63.11618894467929408, 16.35000000000000142 ) ) ;
#5944 = CARTESIAN_POINT ( 'NONE',  ( -31.07316938349034885, -53.11618894467930119, 11.14289321881345352 ) ) ;
#5945 = EDGE_CURVE ( 'NONE', #32513, #43185, #10797, .T. ) ;
#5946 = CARTESIAN_POINT ( 'NONE',  ( 64.45072088349949979, 1.390546226751929959, -70.11984532146888682 ) ) ;
#5947 = CYLINDRICAL_SURFACE ( 'NONE', #7153, 5.999999999999998224 ) ;
#5948 = CARTESIAN_POINT ( 'NONE',  ( 67.51508810499439051, 1.181331450973390096, -18.81107296211990132 ) ) ;
#5949 = ORIENTED_EDGE ( 'NONE', *, *, #49532, .T. ) ;
#5950 = CARTESIAN_POINT ( 'NONE',  ( 15.05440318628160057, -53.11618894467930119, -76.14999999999999147 ) ) ;
#5951 = FACE_OUTER_BOUND ( 'NONE', #31352, .T. ) ;
#5952 =( GEOMETRIC_REPRESENTATION_CONTEXT ( 3 ) GLOBAL_UNCERTAINTY_ASSIGNED_CONTEXT ( ( #51007 ) ) GLOBAL_UNIT_ASSIGNED_CONTEXT ( ( #47775, #40161, #40672 ) ) REPRESENTATION_CONTEXT ( 'NONE', 'WORKASPACE' ) );
#5953 = CARTESIAN_POINT ( 'NONE',  ( 46.19857506040184347, -40.10460585432269909, -55.99493465955088567 ) ) ;
#5954 = DIRECTION ( 'NONE',  ( 0.000000000000000000, 0.000000000000000000, -1.000000000000000000 ) ) ;
#5955 = AXIS2_PLACEMENT_3D ( 'NONE', #4050, #36008, #43887 ) ;
#5956 = CARTESIAN_POINT ( 'NONE',  ( 46.65068702493330477, -53.59610475534989860, -76.01748491306379663 ) ) ;
#5957 = VECTOR ( 'NONE', #34067, 1000.000000000000114 ) ;
#5958 = CARTESIAN_POINT ( 'NONE',  ( 63.18115153217100755, 0.8966068345641440285, -69.03681046574699565 ) ) ;
#5959 = CARTESIAN_POINT ( 'NONE',  ( 47.77308976098110094, -54.47805619242490138, -55.14252499832750232 ) ) ;
#5960 = CARTESIAN_POINT ( 'NONE',  ( 16.65420337941495887, 19.88381105532299387, -21.07727733026571926 ) ) ;
#5961 = CYLINDRICAL_SURFACE ( 'NONE', #46865, 0.4999999999999997224 ) ;
#5962 = CARTESIAN_POINT ( 'NONE',  ( 48.19528691875230209, 22.98443981604779651, -54.75792617359909542 ) ) ;
#5963 = ORIENTED_EDGE ( 'NONE', *, *, #36112, .F. ) ;
#5964 = EDGE_CURVE ( 'NONE', #18453, #24585, #14361, .T. ) ;
#5965 = CARTESIAN_POINT ( 'NONE',  ( 21.80209328419340054, -11.41921765328320149, -76.64430199831019763 ) ) ;
#5966 = EDGE_CURVE ( 'NONE', #5359, #1409, #25869, .T. ) ;
#5967 = ORIENTED_EDGE ( 'NONE', *, *, #18128, .T. ) ;
#5968 = DIRECTION ( 'NONE',  ( 0.000000000000000000, 0.000000000000000000, -1.000000000000000000 ) ) ;
#5969 = DIRECTION ( 'NONE',  ( 0.000000000000000000, 0.000000000000000000, 1.000000000000000000 ) ) ;
#5970 = CARTESIAN_POINT ( 'NONE',  ( 13.88443978363230613, 19.02525189127405625, -20.90776614285195834 ) ) ;
#5972 = CARTESIAN_POINT ( 'NONE',  ( 72.33393739769618946, 10.88381105532070059, -68.84999999999999432 ) ) ;
#5971 = CARTESIAN_POINT ( 'NONE',  ( 82.72635976414500192, 13.93234363556419986, -46.96146434100139544 ) ) ;
#5973 = CARTESIAN_POINT ( 'NONE',  ( 9.490404654256218819, -17.98389487732099923, -73.34384415308200289 ) ) ;
#5975 = EDGE_CURVE ( 'NONE', #28663, #50827, #47643, .T. ) ;
#5974 = DIRECTION ( 'NONE',  ( 0.000000000000000000, 0.000000000000000000, 1.000000000000000000 ) ) ;
#5976 = CARTESIAN_POINT ( 'NONE',  ( 57.29927415537260060, -45.11618894467940066, -16.93367793570499558 ) ) ;
#5977 = CARTESIAN_POINT ( 'NONE',  ( 56.36054294385242258, -46.08205199474749492, -26.17081565480442151 ) ) ;
#5978 = CARTESIAN_POINT ( 'NONE',  ( 51.96093394445609448, -33.40751490558020009, -77.41818406554270382 ) ) ;
#5979 = VERTEX_POINT ( 'NONE', #9412 ) ;
#5980 = ORIENTED_EDGE ( 'NONE', *, *, #11423, .F. ) ;
#5981 = CARTESIAN_POINT ( 'NONE',  ( 11.96713421143980050, -64.86694020486450540, -16.19173486066560130 ) ) ;
#5982 = CARTESIAN_POINT ( 'NONE',  ( 23.01789209736645603, -11.61359716709991119, -39.34022659375048647 ) ) ;
#5983 = CYLINDRICAL_SURFACE ( 'NONE', #24291, 0.4999999999999982236 ) ;
#5984 = CARTESIAN_POINT ( 'NONE',  ( 11.24959018551579959, -65.20486053971309559, -47.30001788089079895 ) ) ;
#5985 = EDGE_LOOP ( 'NONE', ( #48972, #30833, #28071, #13920 ) ) ;
#5986 = CARTESIAN_POINT ( 'NONE',  ( -3.781020702776450193, -49.21259983685390438, -38.25262466549630602 ) ) ;
#5987 = CARTESIAN_POINT ( 'NONE',  ( 28.13393739769619728, -8.687985714403851034, -47.64999999999999858 ) ) ;
#5988 = CARTESIAN_POINT ( 'NONE',  ( 52.08657362407299729, 19.57909417788119910, -50.79540346422049879 ) ) ;
#5989 = CARTESIAN_POINT ( 'NONE',  ( 63.55185157652021388, -1.570504493222709907, -16.28098074310999621 ) ) ;
#5990 = EDGE_CURVE ( 'NONE', #18792, #24734, #29557, .T. ) ;
#5991 = CARTESIAN_POINT ( 'NONE',  ( 51.78079136204299715, -50.15135418014879320, -76.50453849984249644 ) ) ;
#5992 = CARTESIAN_POINT ( 'NONE',  ( 58.95041639152130131, -47.63872770396720568, -49.67920619127879434 ) ) ;
#5993 = VECTOR ( 'NONE', #25522, 1000.000000000000000 ) ;
#5994 = ORIENTED_EDGE ( 'NONE', *, *, #18197, .T. ) ;
#5995 = CARTESIAN_POINT ( 'NONE',  ( 24.04488894642461005, -15.58382787379838774, -33.79102812862304006 ) ) ;
#5997 = CARTESIAN_POINT ( 'NONE',  ( 65.43393739769578588, 16.88381105532129922, -71.50000000000000000 ) ) ;
#5996 = CIRCLE ( 'NONE', #35274, 3.800000000000001155 ) ;
#5998 = ORIENTED_EDGE ( 'NONE', *, *, #39733, .T. ) ;
#5999 = CARTESIAN_POINT ( 'NONE',  ( 12.13393739769600010, -55.41568642894409180, -74.14999999999999147 ) ) ;
#6000 = LINE ( 'NONE', #37707, #33693 ) ;
#6001 = AXIS2_PLACEMENT_3D ( 'NONE', #1738, #21892, #22148 ) ;
#6002 = CARTESIAN_POINT ( 'NONE',  ( 21.52278304119420227, -10.21091847863399948, -31.76248681540709384 ) ) ;
#6003 = CARTESIAN_POINT ( 'NONE',  ( 13.38188356245069954, -50.84254990746399727, -21.60457932969460160 ) ) ;
#6004 = CARTESIAN_POINT ( 'NONE',  ( 53.99619597978309571, 19.44063915672739995, -76.54984132165219535 ) ) ;
#6005 = CARTESIAN_POINT ( 'NONE',  ( 46.86233940950339871, -53.56483039667740087, -75.98411709232810551 ) ) ;
#6006 = ORIENTED_EDGE ( 'NONE', *, *, #51280, .T. ) ;
#6007 = CARTESIAN_POINT ( 'NONE',  ( 55.06067154038679945, 14.25733030481009855, -15.42310526391529990 ) ) ;
#6008 = CARTESIAN_POINT ( 'NONE',  ( 47.65800422766920263, 23.29553884563950206, -55.16662536789920068 ) ) ;
#6009 = CARTESIAN_POINT ( 'NONE',  ( 56.94659880849959421, -50.63911411607320190, -53.72521300055049664 ) ) ;
#6010 = EDGE_CURVE ( 'NONE', #35235, #7036, #30326, .T. ) ;
#6011 = DIRECTION ( 'NONE',  ( 0.000000000000000000, -1.000000000000000000, 0.000000000000000000 ) ) ;
#6012 = DIRECTION ( 'NONE',  ( -0.4412403921425845921, 0.5329539830406733181, -0.7219882050995984901 ) ) ;
#6013 = ORIENTED_EDGE ( 'NONE', *, *, #48750, .T. ) ;
#6014 = ADVANCED_FACE ( 'NONE', ( #14098 ), #48338, .T. ) ;
#6015 = CARTESIAN_POINT ( 'NONE',  ( 47.27618702399679762, 22.86794904519689808, -75.52157719890340104 ) ) ;
#6016 = CARTESIAN_POINT ( 'NONE',  ( 20.03241719490254624, -55.12469585795458471, -18.94537924066331414 ) ) ;
#6017 = APPLICATION_CONTEXT ( 'automotive_design' ) ;
#6018 = CARTESIAN_POINT ( 'NONE',  ( 75.13751216009411849, -27.93201665058723293, -11.73726326173032852 ) ) ;
#6019 = CARTESIAN_POINT ( 'NONE',  ( 13.00893747662790112, -65.51843693869379592, -23.32157303180050079 ) ) ;
#6020 = CYLINDRICAL_SURFACE ( 'NONE', #37373, 2.000000000000003997 ) ;
#6021 = DIRECTION ( 'NONE',  ( -0.1686178020941689892, 0.6660492713794449182, 0.7265992051412129005 ) ) ;
#6022 = DIRECTION ( 'NONE',  ( 2.375726999999999900E-16, -1.726067000000000108E-16, 1.000000000000000000 ) ) ;
#6024 = CARTESIAN_POINT ( 'NONE',  ( 46.36678673786003202, -40.25856219554008675, -54.59816767677268956 ) ) ;
#6023 = DIRECTION ( 'NONE',  ( -1.000000000000000000, -1.681650659181820092E-11, -3.734562218117174162E-22 ) ) ;
#6025 = CARTESIAN_POINT ( 'NONE',  ( 61.08444520316569282, 14.10367956201559991, -46.85801524881159708 ) ) ;
#6026 = CARTESIAN_POINT ( 'NONE',  ( -0.4230338164521119659, 31.94242356383909964, -49.86202923830639833 ) ) ;
#6027 = ORIENTED_EDGE ( 'NONE', *, *, #12526, .T. ) ;
#6028 = EDGE_CURVE ( 'NONE', #49041, #49436, #33307, .T. ) ;
#6029 = AXIS2_PLACEMENT_3D ( 'NONE', #16155, #4100, #15137 ) ;
#6030 = CARTESIAN_POINT ( 'NONE',  ( 52.70374190456139729, -49.74353769694130278, -48.64347189729229370 ) ) ;
#6031 = AXIS2_PLACEMENT_3D ( 'NONE', #43428, #3852, #8033 ) ;
#6032 = ORIENTED_EDGE ( 'NONE', *, *, #35622, .T. ) ;
#6033 = CARTESIAN_POINT ( 'NONE',  ( 46.38583315129304907, 9.012427395117848405, -54.56778683011410891 ) ) ;
#6034 = DIRECTION ( 'NONE',  ( 0.000000000000000000, -1.000000000000000000, 0.000000000000000000 ) ) ;
#6035 = CARTESIAN_POINT ( 'NONE',  ( 13.38497028141870082, 19.86898531093049769, -21.91519145123350043 ) ) ;
#6036 = CARTESIAN_POINT ( 'NONE',  ( 56.20448449522419310, 14.46648588902639965, -25.71422073399899944 ) ) ;
#6037 = CARTESIAN_POINT ( 'NONE',  ( 9.181343238418110175, -16.80109111490159890, -43.39908821103389869 ) ) ;
#6038 = CYLINDRICAL_SURFACE ( 'NONE', #1482, 6.766999999999998572 ) ;
#6040 = EDGE_CURVE ( 'NONE', #46863, #12957, #2448, .T. ) ;
#6039 = CARTESIAN_POINT ( 'NONE',  ( 53.35046855971329194, 18.18352159517930389, -49.00406222516500065 ) ) ;
#6041 = CARTESIAN_POINT ( 'NONE',  ( 64.95388650200960967, 1.388313565858570131, -61.02265534841509975 ) ) ;
#6042 = CARTESIAN_POINT ( 'NONE',  ( 60.86251426101320305, -45.45233350416659590, -47.00312498071580336 ) ) ;
#6043 = CARTESIAN_POINT ( 'NONE',  ( -1.266062602303798856, -15.61618894467929941, -6.649999999999999467 ) ) ;
#6044 = VERTEX_POINT ( 'NONE', #563 ) ;
#6045 = CARTESIAN_POINT ( 'NONE',  ( 21.37225650031859914, -20.91399106607289937, -71.31913972650760059 ) ) ;
#6046 = CARTESIAN_POINT ( 'NONE',  ( 73.01377481872879116, 1.100585178972000033, -69.07860007646939948 ) ) ;
#6047 = CARTESIAN_POINT ( 'NONE',  ( 12.42940066044197422, -8.592417990221209223, -49.13779373100693704 ) ) ;
#6048 = CARTESIAN_POINT ( 'NONE',  ( 73.20448466830819712, 0.9214125008369580261, -62.44212918470660156 ) ) ;
#6049 = FACE_OUTER_BOUND ( 'NONE', #27689, .T. ) ;
#6050 = CARTESIAN_POINT ( 'NONE',  ( 71.54199927891758648, 1.099344084866040072, -60.75649936161010345 ) ) ;
#6051 = CARTESIAN_POINT ( 'NONE',  ( 57.50723796702470025, 15.88381105532069704, -17.93019253464870033 ) ) ;
#6052 = CARTESIAN_POINT ( 'NONE',  ( 22.89932169800278317, -15.45644993449541715, -62.44531429522186272 ) ) ;
#6053 = CARTESIAN_POINT ( 'NONE',  ( 11.56113406461153126, -22.12597267880275353, -46.20275904408111245 ) ) ;
#6054 = CARTESIAN_POINT ( 'NONE',  ( 64.95585434546930514, 1.326578174762039986, -70.44621455782281316 ) ) ;
#6055 = ORIENTED_EDGE ( 'NONE', *, *, #14626, .T. ) ;
#6056 = CARTESIAN_POINT ( 'NONE',  ( 8.962063992902059795, -63.18440697733050371, -46.63297166286719886 ) ) ;
#6057 = CARTESIAN_POINT ( 'NONE',  ( 11.27231506636646330, -9.289981607459157686, -47.08399875780654043 ) ) ;
#6058 = ORIENTED_EDGE ( 'NONE', *, *, #30272, .T. ) ;
#6059 = CARTESIAN_POINT ( 'NONE',  ( 20.63393739769599833, 10.38381105532070059, -34.64999999999999858 ) ) ;
#6060 = CARTESIAN_POINT ( 'NONE',  ( 84.44421850426766696, 12.09119830389948014, -47.46023813347235176 ) ) ;
#6061 = CARTESIAN_POINT ( 'NONE',  ( 18.20467564891351131, -23.32127245094282131, -69.92433697411958349 ) ) ;
#6062 = CARTESIAN_POINT ( 'NONE',  ( 52.15433714350280070, 18.66469978627599957, -76.93549836835239830 ) ) ;
#6063 = EDGE_LOOP ( 'NONE', ( #16722, #47120, #47886, #26331 ) ) ;
#6064 = DIRECTION ( 'NONE',  ( 0.000000000000000000, -1.000000000000000000, 0.000000000000000000 ) ) ;
#6065 = B_SPLINE_SURFACE_WITH_KNOTS ( 'NONE', 3, 3, ( 
 ( #27588, #85, #15555, #51458, #31510, #26815, #47529, #7698, #30999 ),
 ( #43593, #19732, #47781, #15033, #43085, #39147, #51707, #15801, #31763 ),
 ( #23892, #9247, #329, #5310, #48812, #4779, #32014, #12385, #28093 ),
 ( #44099, #13186, #12650, #32785, #841, #37007, #4512, #45136, #40940 ),
 ( #20231, #28610, #32269, #5050, #36734, #8458, #33056, #44877, #20747 ),
 ( #28874, #49082, #16836, #8980, #24926, #21009, #44611, #44352, #21263 ),
 ( #29135, #25194, #4260, #1105, #41201, #17103, #37270, #1371, #48039 ),
 ( #12138, #8199, #40166, #24144, #16313, #36219, #48290, #28350, #24407 ),
 ( #40419, #20484, #36475, #581, #16565, #32520, #48549, #8717, #40679 ),
 ( #13438, #46183, #45398, #5571, #25707, #25450, #49848, #33323, #37790 ),
 ( #42504, #1886, #17865, #33835, #22298, #29396, #33584, #49340, #18375 ),
 ( #29897, #46446, #41980, #37523, #5821, #26490, #34088, #49601, #6083 ),
 ( #41712, #50366, #10271, #14452, #22037, #17616, #30421, #1625, #2392 ),
 ( #45652, #21783, #26233, #13941, #6593, #42240, #10531, #38305, #9503 ),
 ( #41451, #45916, #13687, #14197, #22557, #38572, #17358, #25969, #10008 ),
 ( #38051, #21527, #29647, #9752, #2143, #18124, #50097, #30167, #6338 ) ),
 .UNSPECIFIED., .F., .F., .F.,
 ( 4, 2, 2, 2, 2, 2, 2, 4 ),
 ( 4, 1, 1, 1, 1, 1, 4 ),
 ( -1.570796326794899889, -1.295906969605790104, -0.9817477042468110149, -0.7853981633974489451, -0.6872233929727680213, -0.5301437602932779214, -0.2788163480060940058, 2.850064270699999782E-05 ),
 ( -2.850064270699999782E-05, 0.1666666666666670182, 0.3333333333333329818, 0.5000000000000000000, 0.6666666666666670737, 0.8333333333333330373, 1.000028500642649920 ),
 .UNSPECIFIED. ) ;
#6066 = LINE ( 'NONE', #42751, #35952 ) ;
#6067 = CARTESIAN_POINT ( 'NONE',  ( 64.93393739769619799, 11.38381105532070059, -69.34999999999999432 ) ) ;
#6068 = DIRECTION ( 'NONE',  ( 0.000000000000000000, 0.000000000000000000, -1.000000000000000000 ) ) ;
#6069 = CARTESIAN_POINT ( 'NONE',  ( 17.35874840962710053, -23.76987265457309917, -52.24487123071529027 ) ) ;
#6070 = CARTESIAN_POINT ( 'NONE',  ( 22.11375918210443459, -12.33543082924636280, -56.29291989957688003 ) ) ;
#6071 = CARTESIAN_POINT ( 'NONE',  ( 45.74966035014026744, -38.12695882478442400, -61.57138523371202865 ) ) ;
#6072 = ORIENTED_EDGE ( 'NONE', *, *, #48527, .T. ) ;
#6073 = AXIS2_PLACEMENT_3D ( 'NONE', #36992, #821, #16551 ) ;
#6074 =( BOUNDED_CURVE ( )  B_SPLINE_CURVE ( 3, ( #43652, #31310, #28671, #41002 ),
 .UNSPECIFIED., .F., .T. ) 
 B_SPLINE_CURVE_WITH_KNOTS ( ( 4, 4 ),
 ( 1.485879941667409998, 1.508255586718169949 ),
 .UNSPECIFIED. ) 
 CURVE ( )  GEOMETRIC_REPRESENTATION_ITEM ( )  RATIONAL_B_SPLINE_CURVE ( ( 1.000000000000000000, 0.9999582779775693098, 0.9999582779775693098, 1.000000000000000000 ) ) 
 REPRESENTATION_ITEM ( '' )  );
#6075 = CARTESIAN_POINT ( 'NONE',  ( 18.86789271228450104, 20.55440457967890211, -74.14999999999999147 ) ) ;
#6076 = CARTESIAN_POINT ( 'NONE',  ( 17.09013251674910450, -8.227522982582710753, -47.77362331007289953 ) ) ;
#6077 = AXIS2_PLACEMENT_3D ( 'NONE', #6782, #46622, #10711 ) ;
#6078 = CARTESIAN_POINT ( 'NONE',  ( 52.69474619017670136, -49.76773528829180293, -48.79529908194029986 ) ) ;
#6079 = CIRCLE ( 'NONE', #49598, 39.00000000000000711 ) ;
#6080 = ADVANCED_FACE ( 'NONE', ( #25176 ), #49320, .T. ) ;
#6081 = CARTESIAN_POINT ( 'NONE',  ( 8.943693940708850931, -14.83288028135000047, -32.14999999999999858 ) ) ;
#6082 = EDGE_CURVE ( 'NONE', #16397, #24197, #50968, .T. ) ;
#6083 = CARTESIAN_POINT ( 'NONE',  ( 13.55697919800630125, 20.68059730019900044, -75.01675372117850316 ) ) ;
#6084 = EDGE_CURVE ( 'NONE', #21662, #15955, #41434, .T. ) ;
#6085 = DIRECTION ( 'NONE',  ( 0.7165155114351262622, 0.6975711590030506670, 0.000000000000000000 ) ) ;
#6086 = CARTESIAN_POINT ( 'NONE',  ( 40.91146328487249662, -45.10909871309650754, -5.616201299875400288 ) ) ;
#6087 = CARTESIAN_POINT ( 'NONE',  ( 8.222268241235530795, -15.61616536502389962, -60.50766849176299900 ) ) ;
#6088 = CARTESIAN_POINT ( 'NONE',  ( 10.88887983203600029, -9.254420963851531567, -64.78819959821119312 ) ) ;
#6089 = ORIENTED_EDGE ( 'NONE', *, *, #42242, .T. ) ;
#6090 = CARTESIAN_POINT ( 'NONE',  ( 52.71775171463769993, -49.71300855879460556, -27.79849493049370324 ) ) ;
#6091 = CARTESIAN_POINT ( 'NONE',  ( 53.75292032863279701, -50.98834292138020174, -75.91908533967558981 ) ) ;
#6093 = CARTESIAN_POINT ( 'NONE',  ( -21.36606260230379917, -53.11618894467930119, 16.35000000000000142 ) ) ;
#6092 = CARTESIAN_POINT ( 'NONE',  ( 11.31966774034260048, 33.55174231454390110, -16.38775631906590036 ) ) ;
#6094 = CARTESIAN_POINT ( 'NONE',  ( -12.09840336385581949, 8.995683791603443780, -20.56421356237309794 ) ) ;
#6095 = DIRECTION ( 'NONE',  ( 0.000000000000000000, -1.000000000000000000, 0.000000000000000000 ) ) ;
#6096 = VERTEX_POINT ( 'NONE', #37506 ) ;
#6097 = CARTESIAN_POINT ( 'NONE',  ( -10.42673545829310022, -42.80093869873649481, -6.039852268628239429 ) ) ;
#6098 = CARTESIAN_POINT ( 'NONE',  ( 47.44708028012349388, 23.39794963804610006, -54.93391004409950540 ) ) ;
#6099 = DIRECTION ( 'NONE',  ( 0.3281607301299682700, -0.6263469766835021435, 0.7071067811865493491 ) ) ;
#6100 = CARTESIAN_POINT ( 'NONE',  ( 63.29194469617720387, 1.263903724274369811, -62.37965189720969761 ) ) ;
#6101 = DIRECTION ( 'NONE',  ( 1.000000000000000000, 0.000000000000000000, 0.000000000000000000 ) ) ;
#6102 = CARTESIAN_POINT ( 'NONE',  ( 11.46543043511809934, 33.89017917862779683, -16.91315252355219911 ) ) ;
#6103 = CARTESIAN_POINT ( 'NONE',  ( 7.695097139525095109, 29.51999919305320219, -20.68192065308967997 ) ) ;
#6105 = ADVANCED_FACE ( 'NONE', ( #24650 ), #9223, .T. ) ;
#6104 = CYLINDRICAL_SURFACE ( 'NONE', #24182, 2.999999999999994227 ) ;
#6106 = DIRECTION ( 'NONE',  ( -0.7226652920947586045, 0.6911981449639438280, 0.000000000000000000 ) ) ;
#6107 = CARTESIAN_POINT ( 'NONE',  ( 58.40586952783630181, -46.88396992412620534, -48.04164431124769408 ) ) ;
#6108 = CARTESIAN_POINT ( 'NONE',  ( 52.93425510534450495, 18.32883259169719992, -27.73986516523889989 ) ) ;
#6109 = CARTESIAN_POINT ( 'NONE',  ( 55.99237516468339493, 19.62876559806929677, -53.22104904766129607 ) ) ;
#6110 = CIRCLE ( 'NONE', #219, 13.50000000000000178 ) ;
#6111 = CARTESIAN_POINT ( 'NONE',  ( 63.38185292195529286, 1.308647200627810259, -68.98304916495260386 ) ) ;
#6112 = DIRECTION ( 'NONE',  ( 1.965094753941435058E-11, -1.000000000000000000, 0.000000000000000000 ) ) ;
#6113 = CARTESIAN_POINT ( 'NONE',  ( 15.09836673641149574, -23.52718614182695944, -76.04935793674373201 ) ) ;
#6114 = CARTESIAN_POINT ( 'NONE',  ( 31.69621505884970247, -15.61618894405949654, -8.049999999868621359 ) ) ;
#6115 = CARTESIAN_POINT ( 'NONE',  ( 10.76969664418740003, 31.91660660290840212, -45.20603937285839891 ) ) ;
#6116 = CIRCLE ( 'NONE', #31183, 35.00000000000000000 ) ;
#6117 = CARTESIAN_POINT ( 'NONE',  ( 72.72470740462131289, 1.321111291668189747, -62.02365098255700104 ) ) ;
#6118 = CARTESIAN_POINT ( 'NONE',  ( 67.51507903343110684, -32.41370693817690096, -18.81106344304309985 ) ) ;
#6119 = CARTESIAN_POINT ( 'NONE',  ( 18.86790430670709995, 20.55443781750869903, -74.14994299942661371 ) ) ;
#6120 = ORIENTED_EDGE ( 'NONE', *, *, #32590, .T. ) ;
#6121 = ORIENTED_EDGE ( 'NONE', *, *, #34664, .F. ) ;
#6122 = CARTESIAN_POINT ( 'NONE',  ( 20.99566267773841943, -21.94231647796216933, -79.79933649795523820 ) ) ;
#6123 = CARTESIAN_POINT ( 'NONE',  ( 50.86235438802759745, -0.06463905938872580026, -16.68603828160338765 ) ) ;
#6124 = ORIENTED_EDGE ( 'NONE', *, *, #1633, .F. ) ;
#6125 = CARTESIAN_POINT ( 'NONE',  ( 11.24623595844510149, -64.51626478753739491, -45.52110913008969817 ) ) ;
#6126 = CARTESIAN_POINT ( 'NONE',  ( 56.22872378878379607, -46.03156578494489537, -26.06926613992889941 ) ) ;
#6127 = CARTESIAN_POINT ( 'NONE',  ( 11.97527466958848130, -21.02751549615875959, -45.16117179432525575 ) ) ;
#6128 = CARTESIAN_POINT ( 'NONE',  ( 2.419685150592402856, -25.83699066625585417, -35.06583844469938072 ) ) ;
#6129 = ORIENTED_EDGE ( 'NONE', *, *, #12829, .T. ) ;
#6130 = FACE_OUTER_BOUND ( 'NONE', #42871, .T. ) ;
#6131 = CARTESIAN_POINT ( 'NONE',  ( 45.86773870069588810, 6.907491052131607745, -60.98097754236641777 ) ) ;
#6132 = ORIENTED_EDGE ( 'NONE', *, *, #18335, .F. ) ;
#6133 = CARTESIAN_POINT ( 'NONE',  ( 50.02848935589319979, -45.20415504953729879, -11.19050354007790027 ) ) ;
#6134 = TOROIDAL_SURFACE ( 'NONE', #32867, 25.10000000000000142, 4.000000000000050626 ) ;
#6135 = B_SPLINE_CURVE_WITH_KNOTS ( 'NONE', 3,
 ( #47102, #42120, #30817, #42904, #10672, #46844, #21920, #38973, #10931, #37928, #6220, #22177, #26628, #38188, #2282, #50245 ),
 .UNSPECIFIED., .F., .F.,
 ( 4, 2, 2, 2, 2, 2, 2, 4 ),
 ( 0.000000000000000000, 0.2085309826310009773, 0.3750000003143186822, 0.5000000002514550790, 0.5625000002200234439, 0.6625000001697317620, 0.8225000000892668250, 1.000000000000000000 ),
 .UNSPECIFIED. ) ;
#6136 = CARTESIAN_POINT ( 'NONE',  ( 23.56187535230263208, -18.44086820948935923, -33.90806464902174611 ) ) ;
#6137 = CARTESIAN_POINT ( 'NONE',  ( 15.80909573685769942, 19.88381431121090159, -21.61146777486800019 ) ) ;
#6138 = CARTESIAN_POINT ( 'NONE',  ( 0.5406133260286609676, 12.32747302715160131, -20.15000000000000213 ) ) ;
#6139 = CARTESIAN_POINT ( 'NONE',  ( 57.24929578595760660, -52.61618894467940066, -74.14999999999999147 ) ) ;
#6140 = CARTESIAN_POINT ( 'NONE',  ( 47.13698192568809731, -54.70277146169920712, -74.81178025453719727 ) ) ;
#6141 = CARTESIAN_POINT ( 'NONE',  ( 43.46129097223089843, 12.31710076222960026, -4.984571623251230044 ) ) ;
#6142 = LINE ( 'NONE', #38111, #7144 ) ;
#6143 = EDGE_CURVE ( 'NONE', #51495, #11933, #14152, .T. ) ;
#6144 = VECTOR ( 'NONE', #22449, 1000.000000000000227 ) ;
#6145 = DIRECTION ( 'NONE',  ( -0.5877852522924764678, 0.8090169943749450088, 0.000000000000000000 ) ) ;
#6146 = TOROIDAL_SURFACE ( 'NONE', #40430, 14.50000000000000000, 1.500000000000000000 ) ;
#6147 = AXIS2_PLACEMENT_3D ( 'NONE', #5480, #9416, #37437 ) ;
#6148 = CARTESIAN_POINT ( 'NONE',  ( 52.36927096055270425, 20.10938754437729870, -75.93037474112890095 ) ) ;
#6149 = CARTESIAN_POINT ( 'NONE',  ( 59.73986354666979537, 13.88378808363800054, -26.01995814806780061 ) ) ;
#6150 = CARTESIAN_POINT ( 'NONE',  ( 8.295765907398179095, -16.00324949790340057, -70.27179973214080633 ) ) ;
#6151 = ORIENTED_EDGE ( 'NONE', *, *, #37627, .T. ) ;
#6152 = FACE_OUTER_BOUND ( 'NONE', #887, .T. ) ;
#6153 = CARTESIAN_POINT ( 'NONE',  ( -10.89909870438290085, -41.47166246998200023, -4.617948214634860271 ) ) ;
#6154 = DIRECTION ( 'NONE',  ( 0.3535533905932738974, -0.6123724356957941373, 0.7071067811865477948 ) ) ;
#6155 = CARTESIAN_POINT ( 'NONE',  ( 72.73111481579618953, 1.374525224580429805, -69.09669985268870107 ) ) ;
#6156 = CARTESIAN_POINT ( 'NONE',  ( 2.404741263826640107, -5.380232784273969671, -35.14999999999999858 ) ) ;
#6157 = FACE_OUTER_BOUND ( 'NONE', #43264, .T. ) ;
#6158 = CARTESIAN_POINT ( 'NONE',  ( 11.89321892211240161, 34.20364954171930094, -18.17421237891140251 ) ) ;
#6159 = CARTESIAN_POINT ( 'NONE',  ( 42.25542674435120460, 12.11009477977519921, -3.898748442682229864 ) ) ;
#6161 = ADVANCED_FACE ( 'NONE', ( #44593 ), #4497, .T. ) ;
#6160 = CARTESIAN_POINT ( 'NONE',  ( 15.09829761739486464, -7.705200025808673914, -59.25071220949133988 ) ) ;
#6162 = CARTESIAN_POINT ( 'NONE',  ( 54.17308944977700236, 19.38381105532069881, -77.01198594365929750 ) ) ;
#6163 = AXIS2_PLACEMENT_3D ( 'NONE', #16726, #32681, #41096 ) ;
#6164 = CARTESIAN_POINT ( 'NONE',  ( 75.63614713166808201, -43.36095494122034921, -13.45287883108393956 ) ) ;
#6165 = ADVANCED_FACE ( 'NONE', ( #49061 ), #28348, .F. ) ;
#6166 = FACE_OUTER_BOUND ( 'NONE', #34808, .T. ) ;
#6167 = ORIENTED_EDGE ( 'NONE', *, *, #21582, .F. ) ;
#6168 = CARTESIAN_POINT ( 'NONE',  ( 9.397791606579609436, -12.43326038450650017, -54.20785061676589578 ) ) ;
#6169 = CARTESIAN_POINT ( 'NONE',  ( 63.83278432315639606, 1.031856533264720266, -61.46648470735859604 ) ) ;
#6170 = ORIENTED_EDGE ( 'NONE', *, *, #8917, .F. ) ;
#6171 = CARTESIAN_POINT ( 'NONE',  ( 22.72481146437324639, -17.38743204429671607, -68.53615134654430108 ) ) ;
#6172 = CARTESIAN_POINT ( 'NONE',  ( 60.89859637212030918, -45.70159618970230042, -47.74371479433310128 ) ) ;
#6173 = CARTESIAN_POINT ( 'NONE',  ( 17.86626912417429836, -8.779407102036641319, -74.42617192852868868 ) ) ;
#6174 = CARTESIAN_POINT ( 'NONE',  ( 16.21641506526469101, -23.52682115103659655, -62.00435319991119343 ) ) ;
#6176 = CARTESIAN_POINT ( 'NONE',  ( 21.48628740521284541, -11.02326954940455828, -54.62143916262400012 ) ) ;
#6175 = CARTESIAN_POINT ( 'NONE',  ( 44.33333018168126216, 8.749049325578242886, -65.04467465255862635 ) ) ;
#6177 = B_SPLINE_CURVE_WITH_KNOTS ( 'NONE', 3,
 ( #27669, #39736, #51785, #3840, #50761, #31331, #51017, #34755, #15115, #47103, #35282, #19813, #15888, #14855, #27154, #31842, #7256, #39225 ),
 .UNSPECIFIED., .F., .F.,
 ( 4, 2, 2, 2, 2, 2, 2, 2, 4 ),
 ( 0.5000000032664997374, 0.5625000028581871314, 0.6250000024498745255, 0.6875000020415620305, 0.7500000016332494246, 0.8125000012249370407, 0.8750000008166247678, 0.9375000004083123839, 1.000000000000000000 ),
 .UNSPECIFIED. ) ;
#6178 = LINE ( 'NONE', #34454, #9231 ) ;
#6179 = DIRECTION ( 'NONE',  ( -1.000000000000000000, 0.000000000000000000, 0.000000000000000000 ) ) ;
#6180 = ORIENTED_EDGE ( 'NONE', *, *, #45974, .T. ) ;
#6181 = EDGE_LOOP ( 'NONE', ( #32885, #27780, #3665, #5247, #43447, #46871 ) ) ;
#6182 = ORIENTED_EDGE ( 'NONE', *, *, #12178, .F. ) ;
#6183 = ORIENTED_EDGE ( 'NONE', *, *, #49170, .T. ) ;
#6184 = CARTESIAN_POINT ( 'NONE',  ( -22.74221626195645385, -18.63195909012526741, -54.69355302056131052 ) ) ;
#6185 = CARTESIAN_POINT ( 'NONE',  ( -11.36606260230380094, -15.61618894467929941, -54.64999999999999858 ) ) ;
#6186 = CIRCLE ( 'NONE', #27893, 1.000000000000000888 ) ;
#6187 = CARTESIAN_POINT ( 'NONE',  ( 82.57794276518897902, -45.19659166770669145, -47.00700528987445637 ) ) ;
#6188 = VECTOR ( 'NONE', #21122, 1000.000000000000114 ) ;
#6189 = ORIENTED_EDGE ( 'NONE', *, *, #23864, .F. ) ;
#6190 = VERTEX_POINT ( 'NONE', #40920 ) ;
#6191 = CARTESIAN_POINT ( 'NONE',  ( 9.367206039829609310, -15.61603166621950045, -73.45282021618999124 ) ) ;
#6192 = B_SPLINE_CURVE_WITH_KNOTS ( 'NONE', 3,
 ( #40773, #28970, #9342, #16664, #21360, #20841, #25019, #48918, #17452, #9071, #33416 ),
 .UNSPECIFIED., .F., .F.,
 ( 4, 1, 1, 1, 1, 1, 1, 1, 4 ),
 ( 0.000000000000000000, 0.001354414506361919807, 0.08057334556998355102, 0.1597922766336074829, 0.2390112076972449318, 0.3182301387608665322, 0.3974490698244904641, 0.4766680008880465058, 0.5000038607551413605 ),
 .UNSPECIFIED. ) ;
#6193 = CARTESIAN_POINT ( 'NONE',  ( 53.79565702846219466, -51.91342281481009735, -54.22862211494859963 ) ) ;
#6194 = CARTESIAN_POINT ( 'NONE',  ( 12.89365889624202133, -8.399591182479161589, -80.87333339708158064 ) ) ;
#6195 = ORIENTED_EDGE ( 'NONE', *, *, #5846, .T. ) ;
#6196 = CARTESIAN_POINT ( 'NONE',  ( 24.03121162336080019, -16.09189990580818730, -49.52681125393587536 ) ) ;
#6197 = CARTESIAN_POINT ( 'NONE',  ( 53.99629484594630213, -50.67301330453769737, -76.54982658320740541 ) ) ;
#6198 = CARTESIAN_POINT ( 'NONE',  ( 60.86321315385399799, 14.29876455231970134, -47.42926630397769827 ) ) ;
#6199 = CARTESIAN_POINT ( 'NONE',  ( 19.10341123310410083, -8.351963402172360773, -71.63601545076220134 ) ) ;
#6200 = DIRECTION ( 'NONE',  ( -0.000000000000000000, 1.000000000000000000, 0.000000000000000000 ) ) ;
#6201 = TOROIDAL_SURFACE ( 'NONE', #36286, 38.50000000000000000, 0.5000000000000000000 ) ;
#6202 = CARTESIAN_POINT ( 'NONE',  ( 41.35566246811119839, 13.52648421961340119, -5.363889536437749683 ) ) ;
#6203 = EDGE_CURVE ( 'NONE', #38000, #36938, #21822, .T. ) ;
#6204 = CARTESIAN_POINT ( 'NONE',  ( 41.46604536830830057, -44.03292034146659972, -4.103344335168969792 ) ) ;
#6205 = DIRECTION ( 'NONE',  ( 0.000000000000000000, 0.000000000000000000, -1.000000000000000000 ) ) ;
#6206 = CARTESIAN_POINT ( 'NONE',  ( -11.32734370190460105, 10.64934056395049922, -6.430192534648650593 ) ) ;
#6207 = CARTESIAN_POINT ( 'NONE',  ( 64.41724364727048169, 1.057016615258209891, -70.35216550789259315 ) ) ;
#6208 = CARTESIAN_POINT ( 'NONE',  ( 46.86113300846039920, 8.401293227643240158, -54.33266508569499820 ) ) ;
#6209 = CARTESIAN_POINT ( 'NONE',  ( 8.643744238043749917, -48.75525398023999912, -35.14999999999999858 ) ) ;
#6210 = VERTEX_POINT ( 'NONE', #2377 ) ;
#6211 = LINE ( 'NONE', #47846, #13804 ) ;
#6212 = AXIS2_PLACEMENT_3D ( 'NONE', #25483, #5600, #1917 ) ;
#6213 = CARTESIAN_POINT ( 'NONE',  ( 57.26339702283340216, 19.38381105532069881, -53.86342145260750414 ) ) ;
#6214 = DIRECTION ( 'NONE',  ( 0.000000000000000000, 0.000000000000000000, -1.000000000000000000 ) ) ;
#6215 = DIRECTION ( 'NONE',  ( 0.7071067811865473507, 0.7071067811865476838, 0.000000000000000000 ) ) ;
#6216 = CYLINDRICAL_SURFACE ( 'NONE', #39764, 0.4999999999999967248 ) ;
#6217 = CARTESIAN_POINT ( 'NONE',  ( 63.50007682179899149, 1.388189907116970101, -68.71367622713330547 ) ) ;
#6218 = CARTESIAN_POINT ( 'NONE',  ( 48.05932801370259710, -54.34400791176139478, -55.06214228100389363 ) ) ;
#6219 = LINE ( 'NONE', #17242, #8888 ) ;
#6220 = CARTESIAN_POINT ( 'NONE',  ( -8.399016668315434586, -44.63805185223194627, -5.182633195203329102 ) ) ;
#6221 = EDGE_CURVE ( 'NONE', #30405, #20085, #18352, .T. ) ;
#6222 = CARTESIAN_POINT ( 'NONE',  ( 48.00082595223879878, 23.13732979179570037, -55.05693380849600516 ) ) ;
#6223 = ORIENTED_EDGE ( 'NONE', *, *, #14256, .F. ) ;
#6224 = CARTESIAN_POINT ( 'NONE',  ( 12.00938018391109985, -9.895123749747108732, -70.14834965109328380 ) ) ;
#6225 =( BOUNDED_CURVE ( )  B_SPLINE_CURVE ( 3, ( #45736, #26313, #25785, #34169 ),
 .UNSPECIFIED., .F., .T. ) 
 B_SPLINE_CURVE_WITH_KNOTS ( ( 4, 4 ),
 ( 0.6960202569534489347, 0.7967575818190610892 ),
 .UNSPECIFIED. ) 
 CURVE ( )  GEOMETRIC_REPRESENTATION_ITEM ( )  RATIONAL_B_SPLINE_CURVE ( ( 1.000000000000000000, 0.9991545113881226126, 0.9991545113881226126, 1.000000000000000000 ) ) 
 REPRESENTATION_ITEM ( '' )  );
#6226 = ORIENTED_EDGE ( 'NONE', *, *, #32012, .F. ) ;
#6227 = CARTESIAN_POINT ( 'NONE',  ( 71.31202044992319600, 1.326578174762039986, -70.44621455782281316 ) ) ;
#6228 = CARTESIAN_POINT ( 'NONE',  ( 51.13393739769659874, -50.61618894467899565, 16.85000000000000142 ) ) ;
#6229 = CARTESIAN_POINT ( 'NONE',  ( 61.28610861176739633, -45.23040055550220018, -28.15000000000000213 ) ) ;
#6230 = CARTESIAN_POINT ( 'NONE',  ( 15.41380632618001023, 19.54070139485968838, -20.47803115614054192 ) ) ;
#6232 = CARTESIAN_POINT ( 'NONE',  ( 53.10197615768310442, 18.04954227246929932, -26.94626597811889823 ) ) ;
#6231 = CARTESIAN_POINT ( 'NONE',  ( 82.61657258396949999, 14.02918563699070020, -47.17378930654919600 ) ) ;
#6233 = CARTESIAN_POINT ( 'NONE',  ( 9.165464470679451026, -16.70382112609910052, -75.40353636073618304 ) ) ;
#6234 = DIRECTION ( 'NONE',  ( -0.8090169943749466741, -0.5877852522924741363, 0.000000000000000000 ) ) ;
#6235 = CARTESIAN_POINT ( 'NONE',  ( 71.54045699608259667, 0.8986939045430389905, -70.58925035374331003 ) ) ;
#6236 = CARTESIAN_POINT ( 'NONE',  ( 22.84664670202137771, -16.49985376298375073, -40.49448084163965689 ) ) ;
#6237 = ORIENTED_EDGE ( 'NONE', *, *, #16974, .T. ) ;
#6238 = CARTESIAN_POINT ( 'NONE',  ( 53.63393739769619373, 30.88381105532059934, 16.35000000000000142 ) ) ;
#6239 = ORIENTED_EDGE ( 'NONE', *, *, #20506, .F. ) ;
#6240 = ORIENTED_EDGE ( 'NONE', *, *, #33653, .T. ) ;
#6241 = CARTESIAN_POINT ( 'NONE',  ( 12.36320305068320025, -64.54682834576858852, -15.76422791927960176 ) ) ;
#6242 = DIRECTION ( 'NONE',  ( -0.8224686640529101922, -0.3976080002595576146, -0.4067593573362719428 ) ) ;
#6243 = CARTESIAN_POINT ( 'NONE',  ( -18.43768031504481897, 21.20943201602872108, -54.46295789858282888 ) ) ;
#6244 = CARTESIAN_POINT ( 'NONE',  ( 68.13393739769618662, -29.66618894467940137, -90.65000000000000568 ) ) ;
#6245 = ORIENTED_EDGE ( 'NONE', *, *, #24996, .F. ) ;
#6246 = ORIENTED_EDGE ( 'NONE', *, *, #1104, .T. ) ;
#6247 = CARTESIAN_POINT ( 'NONE',  ( -22.53151229193539962, -21.50213485567750027, -54.59180516875479583 ) ) ;
#6248 = CARTESIAN_POINT ( 'NONE',  ( 30.63393739769620083, -15.61618894467929941, -7.139181489322110608 ) ) ;
#6249 = CARTESIAN_POINT ( 'NONE',  ( 52.61152491900050165, -49.81922436508880025, -48.60684586696110188 ) ) ;
#6250 = AXIS2_PLACEMENT_3D ( 'NONE', #31381, #32146, #39024 ) ;
#6251 = CARTESIAN_POINT ( 'NONE',  ( 51.62687445589580193, 19.67932366877230166, -50.32393917942640371 ) ) ;
#6252 = CARTESIAN_POINT ( 'NONE',  ( 59.93069137380890510, -2.467633955725609951, -15.76379753216029833 ) ) ;
#6253 = CARTESIAN_POINT ( 'NONE',  ( 51.30775049128980214, -48.61618637183489966, -76.60305691058019306 ) ) ;
#6254 = CARTESIAN_POINT ( 'NONE',  ( 61.25350616478739596, -45.59157681858799549, -47.66860495335490100 ) ) ;
#6255 = CIRCLE ( 'NONE', #5392, 24.90000000000000213 ) ;
#6256 = ORIENTED_EDGE ( 'NONE', *, *, #28990, .F. ) ;
#6257 = CARTESIAN_POINT ( 'NONE',  ( 52.56521993351449851, -49.86179673305689874, -28.15000000000000213 ) ) ;
#6258 = CARTESIAN_POINT ( 'NONE',  ( 68.13393739769630031, 16.88381105531719939, -74.20000000000000284 ) ) ;
#6259 = VERTEX_POINT ( 'NONE', #21761 ) ;
#6260 = CARTESIAN_POINT ( 'NONE',  ( 11.27222774357445978, -9.290047668763994793, -53.08399909254191584 ) ) ;
#6261 = CARTESIAN_POINT ( 'NONE',  ( 54.46258938185140153, -45.11618894467940066, -13.50670374307950006 ) ) ;
#6262 = CARTESIAN_POINT ( 'NONE',  ( 23.47482255641189752, -18.39074344551899642, -46.12751964827670292 ) ) ;
#6263 = CARTESIAN_POINT ( 'NONE',  ( 13.48683992790079955, -51.30121652062240400, -22.27491888996000213 ) ) ;
#6264 = CARTESIAN_POINT ( 'NONE',  ( 54.99824089832750218, 19.63007236206330219, -75.56194783846839869 ) ) ;
#6265 = EDGE_CURVE ( 'NONE', #35016, #11240, #31701, .T. ) ;
#6266 = CARTESIAN_POINT ( 'NONE',  ( 47.61801185652239354, -54.54486410850540068, -74.17413012813480577 ) ) ;
#6267 = CARTESIAN_POINT ( 'NONE',  ( 56.07276868759860378, 14.18019669060810095, -16.47680628068019715 ) ) ;
#6269 = EDGE_CURVE ( 'NONE', #16151, #22139, #14432, .T. ) ;
#6268 = CARTESIAN_POINT ( 'NONE',  ( 10.98008937475129976, 32.20858435228970507, -44.74889856825390666 ) ) ;
#6270 = EDGE_CURVE ( 'NONE', #6972, #6855, #29207, .T. ) ;
#6271 = CARTESIAN_POINT ( 'NONE',  ( 56.73072851771979686, -50.34974087631989903, -52.75329813171639870 ) ) ;
#6272 = CARTESIAN_POINT ( 'NONE',  ( 21.45406565774140262, -10.98598436268509992, -38.61921508777290057 ) ) ;
#6273 = DIRECTION ( 'NONE',  ( 0.000000000000000000, 1.000000000000000000, 0.000000000000000000 ) ) ;
#6274 = ADVANCED_FACE ( 'NONE', ( #45632 ), #33373, .F. ) ;
#6275 = EDGE_LOOP ( 'NONE', ( #2573, #30372, #1834, #9532 ) ) ;
#6276 = CARTESIAN_POINT ( 'NONE',  ( 46.40342216745409587, 21.74594192202859944, -76.14871748185780120 ) ) ;
#6277 = LINE ( 'NONE', #41651, #9180 ) ;
#6278 = CARTESIAN_POINT ( 'NONE',  ( 75.28824676885817269, -36.05057910978030122, -12.47240171960510580 ) ) ;
#6279 = CARTESIAN_POINT ( 'NONE',  ( 12.58400818661273668, -65.44616333973714006, -23.49836544046852893 ) ) ;
#6280 = CARTESIAN_POINT ( 'NONE',  ( 0.3209249304026170480, -23.01378514180129997, -34.64999999999999858 ) ) ;
#6281 = ADVANCED_FACE ( 'NONE', ( #46424 ), #13922, .T. ) ;
#6282 = DIRECTION ( 'NONE',  ( -1.000000000000000000, 0.000000000000000000, 0.000000000000000000 ) ) ;
#6283 = CARTESIAN_POINT ( 'NONE',  ( 82.13853704237929776, 14.41952981576026005, -47.73442046593409316 ) ) ;
#6284 = CARTESIAN_POINT ( 'NONE',  ( -18.22323072929020071, 2.939837993609400346, -50.61277379763759399 ) ) ;
#6286 = CARTESIAN_POINT ( 'NONE',  ( 42.77811245501010262, -37.70056812138489732, -76.42740052126559647 ) ) ;
#6285 = DIRECTION ( 'NONE',  ( -1.000000000000000000, 6.785502314117012559E-28, 1.822422554782380175E-11 ) ) ;
#6287 = CARTESIAN_POINT ( 'NONE',  ( 19.55461702279360026, -22.74941205225439944, -32.14999999999999858 ) ) ;
#6288 = EDGE_CURVE ( 'NONE', #32498, #32056, #44263, .T. ) ;
#6289 = CARTESIAN_POINT ( 'NONE',  ( -18.46512919571819822, 21.18267207168980093, -54.23003070569360062 ) ) ;
#6290 = ORIENTED_EDGE ( 'NONE', *, *, #3756, .F. ) ;
#6291 = CARTESIAN_POINT ( 'NONE',  ( 52.65923618566689868, -49.77350477033189691, -48.49072211711909830 ) ) ;
#6292 = ORIENTED_EDGE ( 'NONE', *, *, #24812, .T. ) ;
#6293 = DIRECTION ( 'NONE',  ( 0.6911981449639417185, -0.7226652920947607139, 0.000000000000000000 ) ) ;
#6294 = CARTESIAN_POINT ( 'NONE',  ( 23.83903833740709288, -17.68686109898874292, -73.87566485239436531 ) ) ;
#6295 = CARTESIAN_POINT ( 'NONE',  ( 13.50106276864140042, 20.05783398961539632, -22.28116795780599801 ) ) ;
#6296 = CARTESIAN_POINT ( 'NONE',  ( 57.59065840064920394, 13.88420960100420132, -25.33983012720019801 ) ) ;
#6297 = CARTESIAN_POINT ( 'NONE',  ( 22.28429397680109858, -12.16428039338680023, -42.29002317614330053 ) ) ;
#6298 = DIRECTION ( 'NONE',  ( 1.000000000000000000, 2.460964292799963328E-14, 0.000000000000000000 ) ) ;
#6299 = CARTESIAN_POINT ( 'NONE',  ( 52.65272527767510269, 18.55395787694629917, -48.66231656572949760 ) ) ;
#6300 = CARTESIAN_POINT ( 'NONE',  ( 18.30559885472430182, -8.906037589390139786, -80.44681068936390034 ) ) ;
#6301 = DIRECTION ( 'NONE',  ( 1.000000000000000000, 0.000000000000000000, 0.000000000000000000 ) ) ;
#6302 = ORIENTED_EDGE ( 'NONE', *, *, #26165, .F. ) ;
#6303 = CARTESIAN_POINT ( 'NONE',  ( 21.01363834691890276, -21.76234764997069959, -35.57390792627550269 ) ) ;
#6304 = B_SPLINE_CURVE_WITH_KNOTS ( 'NONE', 3,
 ( #19091, #51072, #15172, #7309, #39276, #3896, #19860, #717 ),
 .UNSPECIFIED., .F., .F.,
 ( 4, 2, 2, 4 ),
 ( 0.000000000000000000, 0.1753589473978111879, 0.6151675087881982584, 1.000000000000000000 ),
 .UNSPECIFIED. ) ;
#6305 = CARTESIAN_POINT ( 'NONE',  ( 72.86479754607628934, 1.326666718054979821, -68.96486503246650557 ) ) ;
#6306 = DIRECTION ( 'NONE',  ( -0.4640893551880601597, -0.8857883891771953788, 0.000000000000000000 ) ) ;
#6307 = CARTESIAN_POINT ( 'NONE',  ( 72.80030139158668590, 1.384887413063060180, -62.68544474927200127 ) ) ;
#6308 = CARTESIAN_POINT ( 'NONE',  ( 11.78673863892869988, -65.42703615493769576, -17.91922926161289809 ) ) ;
#6309 = CARTESIAN_POINT ( 'NONE',  ( 23.24148394091319858, 16.60930999848680401, -54.64999999999999858 ) ) ;
#6310 = CARTESIAN_POINT ( 'NONE',  ( 14.13393739769640156, 6.292713355527309815, -54.64999999999999858 ) ) ;
#6311 = CARTESIAN_POINT ( 'NONE',  ( 11.41477078611200824, -10.71002323189214778, -61.70916163504242036 ) ) ;
#6312 = ADVANCED_FACE ( 'NONE', ( #6575 ), #10512, .T. ) ;
#6313 = DIRECTION ( 'NONE',  ( 1.000000000000000000, 0.000000000000000000, 0.000000000000000000 ) ) ;
#6314 = CARTESIAN_POINT ( 'NONE',  ( 65.09799605061500927, 1.383357884654609959, -70.32891903079600127 ) ) ;
#6315 = ORIENTED_EDGE ( 'NONE', *, *, #17221, .T. ) ;
#6316 = CIRCLE ( 'NONE', #13018, 0.5000000000000004441 ) ;
#6317 = CARTESIAN_POINT ( 'NONE',  ( 10.77067511104800168, -63.19718398965360251, -45.20499083143030106 ) ) ;
#6318 = PLANE ( 'NONE',  #35249 ) ;
#6319 = ORIENTED_EDGE ( 'NONE', *, *, #47508, .T. ) ;
#6320 = DIRECTION ( 'NONE',  ( 0.000000000000000000, 0.000000000000000000, -1.000000000000000000 ) ) ;
#6321 = CARTESIAN_POINT ( 'NONE',  ( 57.12444641451660488, 19.38683328975340103, -53.89324253205270310 ) ) ;
#6322 = CARTESIAN_POINT ( 'NONE',  ( 53.11717555236790389, 19.14142822879220063, -77.21703359850030779 ) ) ;
#6323 = ORIENTED_EDGE ( 'NONE', *, *, #16495, .T. ) ;
#6324 = FACE_OUTER_BOUND ( 'NONE', #35678, .T. ) ;
#6325 = DIRECTION ( 'NONE',  ( -0.4439767838697923907, -0.8960382890170686121, 0.000000000000000000 ) ) ;
#6326 = CARTESIAN_POINT ( 'NONE',  ( -0.007164427059776000244, -27.04615419348650107, -34.77269723891829756 ) ) ;
#6327 = CARTESIAN_POINT ( 'NONE',  ( 8.903861523391762844, -18.89162002862403256, -66.37230234641415905 ) ) ;
#6328 = CARTESIAN_POINT ( 'NONE',  ( 7.922553350839290687, -14.87060723154609931, -66.82115454642119801 ) ) ;
#6329 = CARTESIAN_POINT ( 'NONE',  ( 8.428889365030967085, -17.68705757020854819, -48.42433527398944904 ) ) ;
#6330 = CARTESIAN_POINT ( 'NONE',  ( 45.95646501821028806, -38.14902966602224410, -60.53732341105824588 ) ) ;
#6331 = DIRECTION ( 'NONE',  ( 1.000000000000000000, 0.000000000000000000, 0.000000000000000000 ) ) ;
#6332 = VERTEX_POINT ( 'NONE', #34595 ) ;
#6333 = CARTESIAN_POINT ( 'NONE',  ( 56.64397300593279994, -46.12966333012919762, -26.25586768246660085 ) ) ;
#6334 = CARTESIAN_POINT ( 'NONE',  ( 23.10304989619800153, -18.25022857770899876, -46.34768255092769351 ) ) ;
#6335 = CARTESIAN_POINT ( 'NONE',  ( 9.170124594752591562, -18.41179469585090089, -32.14999999999999858 ) ) ;
#6336 = ADVANCED_FACE ( 'NONE', ( #18103 ), #41963, .T. ) ;
#6337 = LINE ( 'NONE', #38304, #50151 ) ;
#6338 = CARTESIAN_POINT ( 'NONE',  ( 13.39997048867730101, 20.55443781750869903, -74.14994299942661371 ) ) ;
#6339 = DIRECTION ( 'NONE',  ( 1.000000000000000000, 0.000000000000000000, 0.000000000000000000 ) ) ;
#6340 = B_SPLINE_CURVE_WITH_KNOTS ( 'NONE', 3,
 ( #30871, #47155, #46898, #10988, #42958, #7056, #39027, #3122 ),
 .UNSPECIFIED., .F., .F.,
 ( 4, 2, 2, 4 ),
 ( -0.1329710036333066059, -0.1164701438935569905, -0.09932952752691590059, -0.09339196852977180163 ),
 .UNSPECIFIED. ) ;
#6341 = CARTESIAN_POINT ( 'NONE',  ( 44.70608228162969766, -45.11482979815730232, -7.106782871617689956 ) ) ;
#6342 = CARTESIAN_POINT ( 'NONE',  ( 44.84924418339111440, -33.99486860111965569, -61.59306135713902108 ) ) ;
#6343 = CIRCLE ( 'NONE', #41456, 40.00000000000000711 ) ;
#6344 = CARTESIAN_POINT ( 'NONE',  ( 9.794802990449738900, -10.34379900501819982, -62.72850739055710534 ) ) ;
#6345 = VERTEX_POINT ( 'NONE', #25690 ) ;
#6346 = CARTESIAN_POINT ( 'NONE',  ( 53.72142583261089754, -48.59959933175579749, -26.50701750644289945 ) ) ;
#6347 = AXIS2_PLACEMENT_3D ( 'NONE', #38247, #38509, #2340 ) ;
#6348 = CARTESIAN_POINT ( 'NONE',  ( 55.25034777390520446, -50.83736373112089524, -75.46481584694240041 ) ) ;
#6350 = CARTESIAN_POINT ( 'NONE',  ( 42.04585206398351716, -39.76929823994083790, -76.11101280728998120 ) ) ;
#6349 = CARTESIAN_POINT ( 'NONE',  ( 3.293849930124880032, 24.23711703498809911, -8.836877851435611220 ) ) ;
#6351 = CARTESIAN_POINT ( 'NONE',  ( 63.40197747243239945, 1.383811055320669947, -68.52599601131950635 ) ) ;
#6352 = LINE ( 'NONE', #41727, #47382 ) ;
#6353 = EDGE_LOOP ( 'NONE', ( #16666, #46938, #49691, #41600, #25301, #41039, #39290 ) ) ;
#6354 = CARTESIAN_POINT ( 'NONE',  ( 23.24148394091319858, 16.60930999848680401, -54.64999999999999858 ) ) ;
#6355 = CARTESIAN_POINT ( 'NONE',  ( 47.40902048891640419, 23.41821873921709951, -54.79940014147959459 ) ) ;
#6356 = DIRECTION ( 'NONE',  ( -1.649757730820868427E-30, -1.000000000000000000, -1.919972818367709724E-16 ) ) ;
#6357 = CARTESIAN_POINT ( 'NONE',  ( 63.25162284297759641, 1.007912009470880221, -62.17370354086050099 ) ) ;
#6358 = DIRECTION ( 'NONE',  ( 0.3294064756441338893, 0.9441882088883076785, 0.000000000000000000 ) ) ;
#6359 = CARTESIAN_POINT ( 'NONE',  ( 11.16919178478540076, 33.86141759158169862, -17.21576959522939987 ) ) ;
#6360 = CARTESIAN_POINT ( 'NONE',  ( 16.13393739769620083, -15.61618894467929941, -54.64999999999999858 ) ) ;
#6361 = CARTESIAN_POINT ( 'NONE',  ( 53.05172804014560484, 18.31224535922569885, -48.80720635444740196 ) ) ;
#6362 = CARTESIAN_POINT ( 'NONE',  ( 19.16183572673343960, 24.26821873444684741, -75.85379901496348509 ) ) ;
#6363 = CARTESIAN_POINT ( 'NONE',  ( 59.94009989542160355, -46.08106328245670369, -47.78644945012640477 ) ) ;
#6364 = CARTESIAN_POINT ( 'NONE',  ( 53.32548350150899807, 17.93821637278129799, -27.25266754418050041 ) ) ;
#6365 = CARTESIAN_POINT ( 'NONE',  ( 63.34671918778160205, 1.229987731989950150, -69.08683410666979796 ) ) ;
#6366 = CARTESIAN_POINT ( 'NONE',  ( 53.16274087092459411, 18.32513333159890223, -49.15255084583340306 ) ) ;
#6367 = FACE_OUTER_BOUND ( 'NONE', #50811, .T. ) ;
#6368 = CYLINDRICAL_SURFACE ( 'NONE', #51403, 0.4999999999999991118 ) ;
#6369 = CARTESIAN_POINT ( 'NONE',  ( 10.97944215675429902, 32.11615974706089816, -44.74438178823580614 ) ) ;
#6370 = CARTESIAN_POINT ( 'NONE',  ( 72.98301648142211207, 1.028860820852099955, -62.13042434682570558 ) ) ;
#6371 = EDGE_CURVE ( 'NONE', #46602, #12186, #19974, .T. ) ;
#6372 = FACE_OUTER_BOUND ( 'NONE', #25230, .T. ) ;
#6373 = VECTOR ( 'NONE', #12090, 1000.000000000000000 ) ;
#6374 = CARTESIAN_POINT ( 'NONE',  ( 12.89365889624202133, -8.399591182479161589, -80.87333339708158064 ) ) ;
#6375 = VERTEX_POINT ( 'NONE', #30142 ) ;
#6376 = EDGE_CURVE ( 'NONE', #41771, #11158, #46164, .T. ) ;
#6377 = ORIENTED_EDGE ( 'NONE', *, *, #48561, .T. ) ;
#6378 = CARTESIAN_POINT ( 'NONE',  ( 56.46340970881719556, 19.25363520061540257, -52.83593731267799143 ) ) ;
#6379 = CARTESIAN_POINT ( 'NONE',  ( 76.51288141920070984, -2.167259785322154908, -13.28292618809263992 ) ) ;
#6380 = EDGE_LOOP ( 'NONE', ( #21760, #44150, #26869, #36844 ) ) ;
#6381 = CARTESIAN_POINT ( 'NONE',  ( 11.21372797129970067, -64.10201777544770607, -44.24198874234829759 ) ) ;
#6382 = CARTESIAN_POINT ( 'NONE',  ( 57.66457883666589623, -45.12239002789189612, -25.34735987882629971 ) ) ;
#6383 = CARTESIAN_POINT ( 'NONE',  ( 23.78923512644315608, -17.67736616603236044, -77.59138855168500015 ) ) ;
#6384 = EDGE_CURVE ( 'NONE', #45182, #27942, #8268, .T. ) ;
#6385 = DIRECTION ( 'NONE',  ( 0.000000000000000000, 0.7071067811865463515, -0.7071067811865487940 ) ) ;
#6386 =( BOUNDED_CURVE ( )  B_SPLINE_CURVE ( 2, ( #18509, #22164, #38176 ),
 .UNSPECIFIED., .F., .T. ) 
 B_SPLINE_CURVE_WITH_KNOTS ( ( 3, 3 ),
 ( 1.104980434577240045, 2.168627590050209886 ),
 .UNSPECIFIED. ) 
 CURVE ( )  GEOMETRIC_REPRESENTATION_ITEM ( )  RATIONAL_B_SPLINE_CURVE ( ( 1.323085463760220071, 1.425426480542949959, 1.425426480542949959 ) ) 
 REPRESENTATION_ITEM ( '' )  );
#6387 = DIRECTION ( 'NONE',  ( 0.000000000000000000, 1.000000000000000000, 0.000000000000000000 ) ) ;
#6388 = ORIENTED_EDGE ( 'NONE', *, *, #45322, .F. ) ;
#6389 = DIRECTION ( 'NONE',  ( 0.000000000000000000, -1.000000000000000000, 0.000000000000000000 ) ) ;
#6390 = CARTESIAN_POINT ( 'NONE',  ( 46.13676306618652490, 6.935121276559664594, -59.63581676699643452 ) ) ;
#6391 = CIRCLE ( 'NONE', #4686, 2.000000000000001776 ) ;
#6392 = CARTESIAN_POINT ( 'NONE',  ( -11.00338044706756335, 12.40696740781548790, -44.69336853459499537 ) ) ;
#6393 = ORIENTED_EDGE ( 'NONE', *, *, #33775, .F. ) ;
#6394 = CARTESIAN_POINT ( 'NONE',  ( 53.45824824194160385, -46.01483040506809630, -14.86313069892749894 ) ) ;
#6395 = CIRCLE ( 'NONE', #5570, 151.2593554377170051 ) ;
#6396 = DIRECTION ( 'NONE',  ( 2.448986521869468475E-28, 2.813979115193090436E-11, -1.000000000000000000 ) ) ;
#6397 = CARTESIAN_POINT ( 'NONE',  ( 15.85308752007499855, 19.88381105299019680, -21.66365682949070148 ) ) ;
#6398 = DIRECTION ( 'NONE',  ( 1.000000000000000000, 0.000000000000000000, 0.000000000000000000 ) ) ;
#6399 = CARTESIAN_POINT ( 'NONE',  ( 20.92839437590340879, -20.39170135171949028, -46.70218316016916305 ) ) ;
#6400 = DIRECTION ( 'NONE',  ( 0.6522074047277899300, 0.2731766849828906607, 0.7071067811865471286 ) ) ;
#6401 = CARTESIAN_POINT ( 'NONE',  ( 47.18937032989539659, -54.36132375060520161, -75.29143818916560349 ) ) ;
#6402 = CARTESIAN_POINT ( 'NONE',  ( 61.35257612535340144, 13.88381105527380122, -11.49664314637620066 ) ) ;
#6403 = EDGE_CURVE ( 'NONE', #45454, #611, #25639, .T. ) ;
#6404 = CYLINDRICAL_SURFACE ( 'NONE', #51856, 2.000000000000070610 ) ;
#6406 = AXIS2_PLACEMENT_3D ( 'NONE', #34091, #46189, #6868 ) ;
#6405 = CARTESIAN_POINT ( 'NONE',  ( 52.20740535868720400, 20.17246182719640046, -75.93239680710080108 ) ) ;
#6407 = CARTESIAN_POINT ( 'NONE',  ( 58.63648023476770277, 14.01916632703320076, -26.11532393003080088 ) ) ;
#6408 = CARTESIAN_POINT ( 'NONE',  ( 23.70898548626439961, -12.36021487155560017, -37.37844945019890019 ) ) ;
#6409 = VERTEX_POINT ( 'NONE', #22538 ) ;
#6410 = AXIS2_PLACEMENT_3D ( 'NONE', #33405, #13518, #42327 ) ;
#6411 = CARTESIAN_POINT ( 'NONE',  ( 13.00893747662790112, -65.51843693869379592, -23.32157303180050079 ) ) ;
#6412 = CARTESIAN_POINT ( 'NONE',  ( -8.213039659533700743, -43.95837968899080295, -4.510005153980579884 ) ) ;
#6413 = CARTESIAN_POINT ( 'NONE',  ( 76.50235723590930093, 0.4624019994698309599, -13.23610440576140057 ) ) ;
#6414 = CARTESIAN_POINT ( 'NONE',  ( 75.10386764943962135, 13.78341926604215750, -14.70942033535232873 ) ) ;
#6415 = CARTESIAN_POINT ( 'NONE',  ( 75.47966807050509885, -43.37310274687460065, -13.40512917118210012 ) ) ;
#6416 = CARTESIAN_POINT ( 'NONE',  ( 13.10603906833544485, -55.50059662380513004, -75.85379901477443809 ) ) ;
#6417 = DIRECTION ( 'NONE',  ( -0.3863301728269312174, 0.9223605572461961444, 0.000000000000000000 ) ) ;
#6418 = AXIS2_PLACEMENT_3D ( 'NONE', #36891, #11773, #47924 ) ;
#6419 = CARTESIAN_POINT ( 'NONE',  ( 82.54642784563390023, -45.59022060583280478, -47.66712544853100297 ) ) ;
#6420 = DIRECTION ( 'NONE',  ( 0.5721078732755749963, -0.8201783838507928914, 0.000000000000000000 ) ) ;
#6421 = CARTESIAN_POINT ( 'NONE',  ( 42.98728576789530109, 11.64384254154439979, -4.202726304293560311 ) ) ;
#6422 = CARTESIAN_POINT ( 'NONE',  ( 9.807687359717487396, -10.75461966244250611, -59.00069697328734009 ) ) ;
#6423 = DIRECTION ( 'NONE',  ( 0.000000000000000000, -0.7071067811865475727, 0.7071067811865475727 ) ) ;
#6424 = AXIS2_PLACEMENT_3D ( 'NONE', #33415, #21611, #46016 ) ;
#6425 = CARTESIAN_POINT ( 'NONE',  ( 68.13393739769790614, -49.95860450174320277, -71.35146707679190570 ) ) ;
#6426 = CARTESIAN_POINT ( 'NONE',  ( 22.68450600391640393, -17.37075470328159454, -62.53615866583844962 ) ) ;
#6427 = FACE_OUTER_BOUND ( 'NONE', #20760, .T. ) ;
#6428 = EDGE_LOOP ( 'NONE', ( #22399, #3553, #6431, #13915 ) ) ;
#6429 = CARTESIAN_POINT ( 'NONE',  ( 8.695472295357721038, -16.03563054923700193, -54.04941275463870198 ) ) ;
#6430 = CARTESIAN_POINT ( 'NONE',  ( 63.75074504544879517, 1.428542319231299818, -61.92421027702900460 ) ) ;
#6431 = ORIENTED_EDGE ( 'NONE', *, *, #23738, .F. ) ;
#6432 = CARTESIAN_POINT ( 'NONE',  ( 9.366945217436017046, -16.50204441428810753, -69.41115344938793896 ) ) ;
#6433 = DIRECTION ( 'NONE',  ( 1.000000000000000000, 0.000000000000000000, 0.000000000000000000 ) ) ;
#6434 = CARTESIAN_POINT ( 'NONE',  ( 16.13393739769620083, -15.61618894467929941, -41.53556505950739819 ) ) ;
#6435 = CARTESIAN_POINT ( 'NONE',  ( 19.25005220832321129, -22.90603194472208770, -61.87906973423940826 ) ) ;
#6436 = CARTESIAN_POINT ( 'NONE',  ( 45.76614692253087924, 8.847677250480378675, -58.09469284861464189 ) ) ;
#6437 = CARTESIAN_POINT ( 'NONE',  ( 22.90093381512099668, -15.61618921778096336, -54.45281771551935890 ) ) ;
#6438 = DIRECTION ( 'NONE',  ( -9.834501533011740460E-16, -2.054487543405499690E-16, -1.000000000000000000 ) ) ;
#6439 = VERTEX_POINT ( 'NONE', #42746 ) ;
#6440 = EDGE_CURVE ( 'NONE', #42352, #37266, #12462, .T. ) ;
#6441 = ORIENTED_EDGE ( 'NONE', *, *, #48433, .F. ) ;
#6442 = CIRCLE ( 'NONE', #8076, 1.000000000000000888 ) ;
#6443 = VERTEX_POINT ( 'NONE', #33565 ) ;
#6444 = FACE_OUTER_BOUND ( 'NONE', #20375, .T. ) ;
#6445 = CARTESIAN_POINT ( 'NONE',  ( 61.27924359309639613, -45.29619558891289444, -47.09340982550319410 ) ) ;
#6446 = EDGE_CURVE ( 'NONE', #37842, #44438, #13666, .T. ) ;
#6447 = CARTESIAN_POINT ( 'NONE',  ( -11.01912895885372379, -43.80691297044756283, -44.70832929457024107 ) ) ;
#6448 = CIRCLE ( 'NONE', #39889, 7.599999999999996092 ) ;
#6449 = ORIENTED_EDGE ( 'NONE', *, *, #24701, .F. ) ;
#6450 = VERTEX_POINT ( 'NONE', #23050 ) ;
#6451 = DIRECTION ( 'NONE',  ( 0.8660254037844431485, 0.4999999999999921174, 0.000000000000000000 ) ) ;
#6452 = DIRECTION ( 'NONE',  ( 0.000000000000000000, 0.000000000000000000, -1.000000000000000000 ) ) ;
#6453 = ORIENTED_EDGE ( 'NONE', *, *, #27725, .T. ) ;
#6454 = CARTESIAN_POINT ( 'NONE',  ( 23.98909829869109700, -16.57502267198761103, -49.54631662027205152 ) ) ;
#6455 = CARTESIAN_POINT ( 'NONE',  ( 51.62681347090829576, -50.36479533742150494, -76.35210449998979243 ) ) ;
#6456 = CARTESIAN_POINT ( 'NONE',  ( 60.60289840739719835, 14.37099682994570138, -47.31448087610870346 ) ) ;
#6457 = CIRCLE ( 'NONE', #32334, 0.5000000000000004441 ) ;
#6458 = CARTESIAN_POINT ( 'NONE',  ( 17.69277123176280142, -23.30753373288560226, -78.44884352223360224 ) ) ;
#6459 = EDGE_CURVE ( 'NONE', #20583, #18282, #43508, .T. ) ;
#6460 = CARTESIAN_POINT ( 'NONE',  ( 2.452285341914097305, -5.552263267694091731, -34.81767276520685073 ) ) ;
#6461 = CARTESIAN_POINT ( 'NONE',  ( 43.02889804305800681, 14.13343854988660020, -6.968343944726750117 ) ) ;
#6462 = EDGE_CURVE ( 'NONE', #45513, #30141, #33697, .T. ) ;
#6463 = CARTESIAN_POINT ( 'NONE',  ( 40.87457736023439736, -44.61120891011739786, -4.704571543260979816 ) ) ;
#6464 = DIRECTION ( 'NONE',  ( 1.000000000000000000, 0.000000000000000000, 0.000000000000000000 ) ) ;
#6465 = CARTESIAN_POINT ( 'NONE',  ( 66.28198996516779573, 1.842642050337383264, -19.91063246777952855 ) ) ;
#6466 = CARTESIAN_POINT ( 'NONE',  ( 64.45078520382470799, 1.153637615392060223, -70.33899815792979382 ) ) ;
#6467 = CARTESIAN_POINT ( 'NONE',  ( 46.72523890439229888, 8.574345336337970025, -54.52047978925480010 ) ) ;
#6468 = CARTESIAN_POINT ( 'NONE',  ( 17.87263216484612727, -51.26000751223833163, -74.91995119714192697 ) ) ;
#6469 = CARTESIAN_POINT ( 'NONE',  ( 20.97057552888700016, -21.79629248516249973, -51.57613200112659513 ) ) ;
#6470 = ORIENTED_EDGE ( 'NONE', *, *, #4848, .F. ) ;
#6471 = CARTESIAN_POINT ( 'NONE',  ( 57.55751162087899786, 18.85811933572209753, -52.57651812407429759 ) ) ;
#6472 = CARTESIAN_POINT ( 'NONE',  ( 45.76880525768196861, -40.08018765987725374, -58.08188677919342524 ) ) ;
#6473 = CARTESIAN_POINT ( 'NONE',  ( 64.93393739769619799, 11.38381105532070059, -68.84999999999999432 ) ) ;
#6474 = CARTESIAN_POINT ( 'NONE',  ( 46.77994874552049254, -53.89178638932320098, -75.86501933388160523 ) ) ;
#6475 = CARTESIAN_POINT ( 'NONE',  ( 63.15932386229340523, 0.8936201581567889685, -69.00461532610479765 ) ) ;
#6476 = B_SPLINE_CURVE_WITH_KNOTS ( 'NONE', 3,
 ( #21955, #38752, #5995, #6778, #30850, #50019, #10187, #30597, #2318, #46880, #46618, #2846, #26660, #33754, #10449, #26147, #14109, #2064, #18290, #34262, #10967, #21695, #30339, #50286, #46362, #26402, #26933, #18040, #1799, #42423, #42938, #6513, #22473, #37703, #37965 ),
 .UNSPECIFIED., .F., .F.,
 ( 4, 2, 1, 2, 2, 2, 2, 2, 2, 2, 2, 2, 2, 2, 2, 2, 2, 4 ),
 ( 0.5000036731825925340, 0.5039098944858534379, 0.5078161157891143418, 0.5156285583956361496, 0.5312534436086802092, 0.5625032140347683285, 0.6250027548869443450, 0.6875022957391202505, 0.7187520661652082588, 0.7500018365912961560, 0.7812516070173841642, 0.8125013774434721725, 0.8437511478695601808, 0.8750009182956480780, 0.9062506887217359752, 0.9375004591478239835, 0.9687502295739119917, 1.000000000000000000 ),
 .UNSPECIFIED. ) ;
#6477 = CARTESIAN_POINT ( 'NONE',  ( 13.13393739769619906, -63.52234721269329754, -46.39999999999999858 ) ) ;
#6478 = CARTESIAN_POINT ( 'NONE',  ( 9.367202679915338948, -15.61634672871210050, -75.45282021618999124 ) ) ;
#6479 = B_SPLINE_CURVE_WITH_KNOTS ( 'NONE', 3,
 ( #11352, #23117, #39135, #51442, #19198, #15538, #27831, #7930, #31490, #20218, #47515, #35184, #19718, #23879, #39903, #11610, #11100, #51186 ),
 .UNSPECIFIED., .F., .F.,
 ( 4, 2, 2, 2, 2, 2, 2, 2, 4 ),
 ( 0.4999969675811580805, 0.5624973466335132510, 0.6249977256858685326, 0.6874981047382237032, 0.7499984837905790958, 0.8124988628429342663, 0.8749992418952895479, 0.9374996209476447184, 1.000000000000000000 ),
 .UNSPECIFIED. ) ;
#6480 = CARTESIAN_POINT ( 'NONE',  ( 48.25999128426249740, 23.03781136496079895, -55.22775327136439927 ) ) ;
#6481 = VERTEX_POINT ( 'NONE', #47701 ) ;
#6482 = CARTESIAN_POINT ( 'NONE',  ( 12.38873293430890143, -9.639902246245529938, -76.16898841192839598 ) ) ;
#6483 = EDGE_LOOP ( 'NONE', ( #29569, #39127, #11789, #48336, #5565 ) ) ;
#6484 = CARTESIAN_POINT ( 'NONE',  ( 71.47612964547808190, 0.8925687589132640376, -70.63296852923029689 ) ) ;
#6485 = CARTESIAN_POINT ( 'NONE',  ( 16.13393739769620083, -15.61618894467929941, -28.45282021618999835 ) ) ;
#6486 = AXIS2_PLACEMENT_3D ( 'NONE', #9350, #25295, #21368 ) ;
#6487 = CARTESIAN_POINT ( 'NONE',  ( 57.34776335324270491, 14.57942837581910034, -26.27178905609630277 ) ) ;
#6488 = DIRECTION ( 'NONE',  ( 1.000000000000000000, 0.000000000000000000, 0.000000000000000000 ) ) ;
#6490 = CARTESIAN_POINT ( 'NONE',  ( 54.12395466776580122, 16.89186266783300283, -26.13497438140159801 ) ) ;
#6489 = DIRECTION ( 'NONE',  ( 1.000000000000000000, 0.000000000000000000, 0.000000000000000000 ) ) ;
#6491 = CARTESIAN_POINT ( 'NONE',  ( 19.21648360630749863, -21.95972640956449951, -70.80883835904629109 ) ) ;
#6492 = DIRECTION ( 'NONE',  ( -0.3294064756440908681, 0.9441882088883227775, 0.000000000000000000 ) ) ;
#6493 = CARTESIAN_POINT ( 'NONE',  ( 24.04513930477782679, -15.61618913701998146, -67.79233342760500136 ) ) ;
#6494 = CARTESIAN_POINT ( 'NONE',  ( 9.366915451059274034, -16.50182680598841500, -41.41114337331676154 ) ) ;
#6495 = ORIENTED_EDGE ( 'NONE', *, *, #16968, .T. ) ;
#6496 = CARTESIAN_POINT ( 'NONE',  ( 16.13393739769620083, -15.61618894467929941, -84.65000000000000568 ) ) ;
#6497 = ORIENTED_EDGE ( 'NONE', *, *, #11152, .T. ) ;
#6498 = EDGE_CURVE ( 'NONE', #2490, #36299, #19160, .T. ) ;
#6499 = ORIENTED_EDGE ( 'NONE', *, *, #37214, .T. ) ;
#6500 = CARTESIAN_POINT ( 'NONE',  ( 16.13393739769620083, -15.61618894467929941, -32.14999999999999858 ) ) ;
#6501 = CARTESIAN_POINT ( 'NONE',  ( 54.53727200435603351, 14.79464053051451700, -15.67785519347521550 ) ) ;
#6502 = CARTESIAN_POINT ( 'NONE',  ( 9.366948908879642488, -16.50207144407324478, -55.41115368061451107 ) ) ;
#6503 = DIRECTION ( 'NONE',  ( 0.9200120562340476926, 0.3918900565005438708, 0.000000000000000000 ) ) ;
#6504 = ORIENTED_EDGE ( 'NONE', *, *, #10284, .F. ) ;
#6505 = ORIENTED_EDGE ( 'NONE', *, *, #51156, .T. ) ;
#6506 = CARTESIAN_POINT ( 'NONE',  ( 49.72648160330989953, 22.41435850158119791, -55.11972614036179863 ) ) ;
#6507 = CARTESIAN_POINT ( 'NONE',  ( 64.43393739769710749, 11.38381105532080184, -69.34999999999971010 ) ) ;
#6508 = CARTESIAN_POINT ( 'NONE',  ( 53.46099711234219143, 18.11456714212909702, -49.02220847068660703 ) ) ;
#6509 = CARTESIAN_POINT ( 'NONE',  ( 65.46589392415390307, -1.325377498103930130, -16.55434372537479959 ) ) ;
#6510 = CARTESIAN_POINT ( 'NONE',  ( 51.59667043160109756, -49.96101828097980047, -76.48753601724520479 ) ) ;
#6511 = CARTESIAN_POINT ( 'NONE',  ( 57.25062957476220049, -50.11783017573850429, -52.59164223185749876 ) ) ;
#6512 = ORIENTED_EDGE ( 'NONE', *, *, #44916, .T. ) ;
#6513 = CARTESIAN_POINT ( 'NONE',  ( 8.944826496811360883, -12.20469241501894331, -32.93351229774626887 ) ) ;
#6514 = CARTESIAN_POINT ( 'NONE',  ( 69.22748654599826068, 19.47158195952029303, -72.59354914830210248 ) ) ;
#6515 = VERTEX_POINT ( 'NONE', #35111 ) ;
#6516 = CARTESIAN_POINT ( 'NONE',  ( 9.543102507195031947, -13.84480207404790342, -51.53615333421284106 ) ) ;
#6517 = PLANE ( 'NONE',  #17772 ) ;
#6518 = CARTESIAN_POINT ( 'NONE',  ( 23.21194978661330310, -12.22672169835309930, -47.87033613167638890 ) ) ;
#6519 = CARTESIAN_POINT ( 'NONE',  ( 12.99344367413189971, -50.62396699225990204, -21.36723036234760187 ) ) ;
#6520 = CARTESIAN_POINT ( 'NONE',  ( 54.17122153902240456, 19.43792079591710120, -76.49428706740339123 ) ) ;
#6521 = EDGE_CURVE ( 'NONE', #45038, #50570, #24539, .T. ) ;
#6522 = CARTESIAN_POINT ( 'NONE',  ( 47.47118984295180155, -54.42867273149169449, -74.94873378728740931 ) ) ;
#6523 = CARTESIAN_POINT ( 'NONE',  ( 55.61922199844690340, 13.90021221559030096, -14.76093055395720022 ) ) ;
#6524 = CARTESIAN_POINT ( 'NONE',  ( 8.815605938792600682, 32.05029769220720226, -46.67186391141279955 ) ) ;
#6525 = CARTESIAN_POINT ( 'NONE',  ( 56.77163879080330133, -50.67344205490699949, -53.71547587233740018 ) ) ;
#6526 = CARTESIAN_POINT ( 'NONE',  ( 11.60944838831639991, -10.20586932579799821, -48.12548681540710049 ) ) ;
#6527 = LINE ( 'NONE', #22489, #40211 ) ;
#6528 = VERTEX_POINT ( 'NONE', #40086 ) ;
#6529 = CARTESIAN_POINT ( 'NONE',  ( 46.35275103504439898, 21.67755452994670406, -76.14999999999999147 ) ) ;
#6530 = CARTESIAN_POINT ( 'NONE',  ( 64.84562941585738827, 1.096044978595170027, -60.67935125044880351 ) ) ;
#6531 = CARTESIAN_POINT ( 'NONE',  ( -12.18284927255036543, -15.61618894467929763, 6.072546842075589701 ) ) ;
#6532 = CARTESIAN_POINT ( 'NONE',  ( 12.14991910881904502, -8.703601772961780725, -57.12566474721839427 ) ) ;
#6533 = DIRECTION ( 'NONE',  ( 0.000000000000000000, 0.000000000000000000, 1.000000000000000000 ) ) ;
#6534 = FACE_OUTER_BOUND ( 'NONE', #35123, .T. ) ;
#6535 = CARTESIAN_POINT ( 'NONE',  ( 82.32429372338799567, 14.20864740965710027, -47.46868296552500510 ) ) ;
#6536 = CARTESIAN_POINT ( 'NONE',  ( -9.411761488291968902, 14.27370694945600071, -43.11785523033920242 ) ) ;
#6538 = CARTESIAN_POINT ( 'NONE',  ( 45.56286034474006641, -39.21681118499099483, -62.73037012550634017 ) ) ;
#6537 = DIRECTION ( 'NONE',  ( 0.000000000000000000, 0.000000000000000000, -1.000000000000000000 ) ) ;
#6539 = CARTESIAN_POINT ( 'NONE',  ( 23.99634207538090891, -14.71164246568921641, -71.47121910958560420 ) ) ;
#6540 = CARTESIAN_POINT ( 'NONE',  ( 22.46009814471073440, -10.75450484369422455, -69.29933762258028196 ) ) ;
#6541 = CARTESIAN_POINT ( 'NONE',  ( -33.78933650424870194, -10.75740117049570088, -57.07866011716559740 ) ) ;
#6542 = ORIENTED_EDGE ( 'NONE', *, *, #37627, .F. ) ;
#6543 = CARTESIAN_POINT ( 'NONE',  ( 53.23189944373280014, -49.47193143504960489, -48.99600315007679541 ) ) ;
#6544 = ORIENTED_EDGE ( 'NONE', *, *, #47166, .T. ) ;
#6545 = CARTESIAN_POINT ( 'NONE',  ( 46.82732515567090559, 9.047176644529985268, -52.37284531381663299 ) ) ;
#6546 = CARTESIAN_POINT ( 'NONE',  ( 10.22109612992661098, -12.20807755088076441, -41.61948678692156278 ) ) ;
#6547 = CARTESIAN_POINT ( 'NONE',  ( 14.30978967243790123, 19.88381105581349573, -22.40422843537270126 ) ) ;
#6548 = CARTESIAN_POINT ( 'NONE',  ( 55.97700001955439575, 14.61467643665769955, -25.52897050747419883 ) ) ;
#6549 = CARTESIAN_POINT ( 'NONE',  ( 9.459240049790720306, -13.33781803315300074, -43.55752607316119906 ) ) ;
#6550 = CARTESIAN_POINT ( 'NONE',  ( 28.63604668330589931, -26.55449506982230190, -34.65000333679609668 ) ) ;
#6551 = CARTESIAN_POINT ( 'NONE',  ( 52.95534730618609842, 18.39748524797530038, -49.01774095212640248 ) ) ;
#6552 = CARTESIAN_POINT ( 'NONE',  ( 55.36019775732630421, -46.03750363997700390, -16.50346971581090116 ) ) ;
#6553 = CARTESIAN_POINT ( 'NONE',  ( 15.19691430481782568, -43.84596607001308399, -60.51477253168710035 ) ) ;
#6554 = ORIENTED_EDGE ( 'NONE', *, *, #31874, .T. ) ;
#6555 = EDGE_CURVE ( 'NONE', #14404, #260, #47703, .T. ) ;
#6556 = CARTESIAN_POINT ( 'NONE',  ( 21.72913965751709853, -21.11895732567419870, -39.53485447945639919 ) ) ;
#6557 = EDGE_CURVE ( 'NONE', #3678, #37798, #37656, .T. ) ;
#6558 = CARTESIAN_POINT ( 'NONE',  ( 59.77423841227909662, 14.93359823389899788, -47.80915357183090464 ) ) ;
#6559 = CARTESIAN_POINT ( 'NONE',  ( 9.469557471980332153, 33.05699343178789462, -46.83899467929160210 ) ) ;
#6560 = CARTESIAN_POINT ( 'NONE',  ( 72.81285642849219641, 1.383357884654609959, -62.61405865291869333 ) ) ;
#6561 = CARTESIAN_POINT ( 'NONE',  ( 10.64977475910500004, -64.85626261263139725, -18.05902683592860214 ) ) ;
#6563 = EDGE_CURVE ( 'NONE', #40270, #5090, #32439, .T. ) ;
#6562 = CARTESIAN_POINT ( 'NONE',  ( 52.60295254337715676, -49.82768164818063639, -48.60889610034470110 ) ) ;
#6564 = DIRECTION ( 'NONE',  ( 0.8229030450105319083, 0.000000000000000000, 0.5681818181818162339 ) ) ;
#6565 = CARTESIAN_POINT ( 'NONE',  ( 16.57903057602875663, -8.841341571868987614, -61.97366626368047093 ) ) ;
#6566 = AXIS2_PLACEMENT_3D ( 'NONE', #35315, #8059, #23756 ) ;
#6567 = CARTESIAN_POINT ( 'NONE',  ( 23.78210164868285048, -17.70463183224734038, -45.59262049459194799 ) ) ;
#6568 = EDGE_CURVE ( 'NONE', #9565, #38690, #21180, .T. ) ;
#6569 = ORIENTED_EDGE ( 'NONE', *, *, #50685, .F. ) ;
#6570 = CARTESIAN_POINT ( 'NONE',  ( 64.86358929490600644, 1.263903724274369811, -70.49199270151910923 ) ) ;
#6571 = VERTEX_POINT ( 'NONE', #40591 ) ;
#6572 = CARTESIAN_POINT ( 'NONE',  ( 10.77295366634669804, -63.31447053344770381, -45.20535261670850247 ) ) ;
#6573 = CYLINDRICAL_SURFACE ( 'NONE', #23511, 0.4999999999999967248 ) ;
#6574 = ORIENTED_EDGE ( 'NONE', *, *, #3892, .F. ) ;
#6575 = FACE_OUTER_BOUND ( 'NONE', #7737, .T. ) ;
#6576 = CARTESIAN_POINT ( 'NONE',  ( 57.28774565042520095, 19.34651099262390161, -53.44461253008790180 ) ) ;
#6577 = CARTESIAN_POINT ( 'NONE',  ( 52.98832975904100095, 19.18558910406980189, -76.96373677364138643 ) ) ;
#6578 = ORIENTED_EDGE ( 'NONE', *, *, #30028, .T. ) ;
#6579 = CYLINDRICAL_SURFACE ( 'NONE', #29960, 39.00000000000000711 ) ;
#6580 = CARTESIAN_POINT ( 'NONE',  ( 60.14150383576895109, 15.95610133017432908, -49.41068029984030119 ) ) ;
#6581 = CARTESIAN_POINT ( 'NONE',  ( 21.34899891482215395, -19.99345227585487095, -32.67494819118432048 ) ) ;
#6582 = EDGE_CURVE ( 'NONE', #12303, #18612, #48996, .T. ) ;
#6583 = CARTESIAN_POINT ( 'NONE',  ( 8.222928256549737469, -14.58070839043696409, -68.83399830554878918 ) ) ;
#6584 = CARTESIAN_POINT ( 'NONE',  ( 12.33875874437710074, -22.93597986008980172, -64.44458661451268711 ) ) ;
#6585 = CARTESIAN_POINT ( 'NONE',  ( 16.13393739769620083, -15.61618894467929941, -18.58999999999999986 ) ) ;
#6586 = CARTESIAN_POINT ( 'NONE',  ( 44.68164263780834489, -38.00422853341399332, -66.91141490620562138 ) ) ;
#6587 = ADVANCED_FACE ( 'NONE', ( #37187 ), #498, .T. ) ;
#6588 = ORIENTED_EDGE ( 'NONE', *, *, #37815, .F. ) ;
#6589 = CARTESIAN_POINT ( 'NONE',  ( 74.93037295002240228, -43.11618894467930119, -15.31098073120859837 ) ) ;
#6590 = CARTESIAN_POINT ( 'NONE',  ( 14.93875137453389890, -22.96997872785800254, -50.78394269049049825 ) ) ;
#6591 = CARTESIAN_POINT ( 'NONE',  ( 8.946858529655370873, -17.52974850216140013, -32.14999999999999858 ) ) ;
#6592 = CARTESIAN_POINT ( 'NONE',  ( 50.95182575631829991, 19.71852405838109945, -76.14999999999999147 ) ) ;
#6593 = CARTESIAN_POINT ( 'NONE',  ( 13.78212824785540036, 20.09246212084070038, -74.56515407679870577 ) ) ;
#6594 = CARTESIAN_POINT ( 'NONE',  ( 57.24929578595760660, 21.38381105532069881, -63.99406948319570887 ) ) ;
#6595 = CARTESIAN_POINT ( 'NONE',  ( 41.35125392209459960, -44.98027078473889873, -5.668951409370400540 ) ) ;
#6596 = DIRECTION ( 'NONE',  ( 0.000000000000000000, 0.000000000000000000, 1.000000000000000000 ) ) ;
#6597 = VECTOR ( 'NONE', #49962, 999.9999999999998863 ) ;
#6598 = ADVANCED_FACE ( 'NONE', ( #36921 ), #33236, .T. ) ;
#6600 = VECTOR ( 'NONE', #19896, 1000.000000000000000 ) ;
#6599 = CARTESIAN_POINT ( 'NONE',  ( 20.04006244057629971, -8.354997041254607737, -67.16476753011970402 ) ) ;
#6601 = ORIENTED_EDGE ( 'NONE', *, *, #39218, .F. ) ;
#6602 = CARTESIAN_POINT ( 'NONE',  ( 52.67941827447170056, -49.73994065207369886, -27.56303321415330032 ) ) ;
#6603 = CARTESIAN_POINT ( 'NONE',  ( 54.78812434636329698, -50.98684819909150434, -75.45670350304489205 ) ) ;
#6605 = CARTESIAN_POINT ( 'NONE',  ( 16.13393739769599833, 14.38381105532070059, -62.64999999999999858 ) ) ;
#6604 = CARTESIAN_POINT ( 'NONE',  ( 10.28185505973059932, 33.24230909050100280, -17.86151643087199758 ) ) ;
#6606 = FACE_OUTER_BOUND ( 'NONE', #37621, .T. ) ;
#6607 = CARTESIAN_POINT ( 'NONE',  ( 6.187261889072820154, -46.71083452957879700, -20.15000000000000213 ) ) ;
#6608 = ORIENTED_EDGE ( 'NONE', *, *, #12294, .F. ) ;
#6609 = CARTESIAN_POINT ( 'NONE',  ( -10.89082349597999944, -42.33811146364660516, -6.201050197583099610 ) ) ;
#6610 = CARTESIAN_POINT ( 'NONE',  ( 47.48653415169840031, 23.37519123828230150, -54.89669719852860652 ) ) ;
#6611 = CARTESIAN_POINT ( 'NONE',  ( 24.04460285965960864, -15.61618860597671876, -65.79233133698019742 ) ) ;
#6612 = LINE ( 'NONE', #7389, #19300 ) ;
#6613 = CARTESIAN_POINT ( 'NONE',  ( 20.63393739769598767, 10.38381105532070414, -35.01561944896766931 ) ) ;
#6614 = CARTESIAN_POINT ( 'NONE',  ( 11.91426296011000119, 33.88532756217980335, -16.60966417100599912 ) ) ;
#6615 = CARTESIAN_POINT ( 'NONE',  ( 7.853097003783789276, 29.28805065900050053, -20.86915960608759946 ) ) ;
#6616 = CARTESIAN_POINT ( 'NONE',  ( 52.83464909576289159, 18.42637314819869943, -48.65907448191860141 ) ) ;
#6617 = LINE ( 'NONE', #45421, #48424 ) ;
#6618 = DIRECTION ( 'NONE',  ( 0.000000000000000000, 1.000000000000000000, 0.000000000000000000 ) ) ;
#6619 = CARTESIAN_POINT ( 'NONE',  ( 53.37647868240819804, 17.93233224264670156, -27.30365310598189765 ) ) ;
#6620 = CYLINDRICAL_SURFACE ( 'NONE', #22946, 0.5000000000000006661 ) ;
#6621 = EDGE_CURVE ( 'NONE', #4309, #5342, #23944, .T. ) ;
#6622 = CARTESIAN_POINT ( 'NONE',  ( 11.10574934303680017, -63.48107579820671020, -44.26157399421149563 ) ) ;
#6623 = CARTESIAN_POINT ( 'NONE',  ( 52.77399500191609860, 18.49248106158579930, -48.90117827005099826 ) ) ;
#6624 = CARTESIAN_POINT ( 'NONE',  ( 18.13393739769639268, 10.38381105532070414, -35.01561944896763379 ) ) ;
#6625 = CARTESIAN_POINT ( 'NONE',  ( 71.36046776202630326, 0.9940423591679348192, -60.60059430635039490 ) ) ;
#6626 = CARTESIAN_POINT ( 'NONE',  ( 11.10574934303680017, 32.24869790884810072, -44.26157399421149563 ) ) ;
#6627 = CARTESIAN_POINT ( 'NONE',  ( 72.94959658490671472, 1.034647430441060001, -62.08420298997459952 ) ) ;
#6628 = CIRCLE ( 'NONE', #21663, 5.999999999999998224 ) ;
#6629 = CARTESIAN_POINT ( 'NONE',  ( 65.13922429466639130, -32.18685348281329794, -17.74407301686150262 ) ) ;
#6630 = EDGE_CURVE ( 'NONE', #4963, #2182, #36440, .T. ) ;
#6631 = CARTESIAN_POINT ( 'NONE',  ( 12.18502445233735187, 24.18831204814821945, -74.66535148663518839 ) ) ;
#6632 = VERTEX_POINT ( 'NONE', #4955 ) ;
#6633 = ORIENTED_EDGE ( 'NONE', *, *, #12073, .F. ) ;
#6634 = FACE_OUTER_BOUND ( 'NONE', #44763, .T. ) ;
#6635 = CARTESIAN_POINT ( 'NONE',  ( 48.94724833445295076, -2.939553391498948898, -15.65000000114250334 ) ) ;
#6636 = VERTEX_POINT ( 'NONE', #20925 ) ;
#6637 = CARTESIAN_POINT ( 'NONE',  ( 11.39881522676340175, -64.71865303079098908, -45.74527777199200784 ) ) ;
#6638 = CARTESIAN_POINT ( 'NONE',  ( 56.54952170946580736, -45.45011454905849746, -25.70425748956289880 ) ) ;
#6639 = PLANE ( 'NONE',  #29466 ) ;
#6640 = CIRCLE ( 'NONE', #29203, 2.000000000000001332 ) ;
#6641 = CARTESIAN_POINT ( 'NONE',  ( 63.47971227208819300, 1.385888765344509999, -68.65207957385619864 ) ) ;
#6642 = ORIENTED_EDGE ( 'NONE', *, *, #45969, .F. ) ;
#6643 = DIRECTION ( 'NONE',  ( -0.7071067811865475727, 0.000000000000000000, 0.7071067811865475727 ) ) ;
#6644 = VECTOR ( 'NONE', #4256, 1000.000000000000000 ) ;
#6645 = CARTESIAN_POINT ( 'NONE',  ( 46.79883821287099721, 6.999256669433407296, -56.32544524183283841 ) ) ;
#6646 = EDGE_CURVE ( 'NONE', #25231, #14553, #48465, .T. ) ;
#6647 = CARTESIAN_POINT ( 'NONE',  ( 12.26871351663039889, 34.23561203028980060, -22.61095353172289890 ) ) ;
#6648 = ORIENTED_EDGE ( 'NONE', *, *, #12738, .F. ) ;
#6649 = CARTESIAN_POINT ( 'NONE',  ( 48.26658354509820725, -45.11618894467940066, -9.084211283098401424 ) ) ;
#6650 = CYLINDRICAL_SURFACE ( 'NONE', #25441, 0.4999999999999967248 ) ;
#6651 = AXIS2_PLACEMENT_3D ( 'NONE', #39876, #2945, #31718 ) ;
#6652 = CARTESIAN_POINT ( 'NONE',  ( 16.65429250104310199, 19.88381105411679783, -20.30769847209329981 ) ) ;
#6653 = CARTESIAN_POINT ( 'NONE',  ( 9.366715917462860475, -15.61603296970410071, -51.45282021618999835 ) ) ;
#6654 = EDGE_CURVE ( 'NONE', #7479, #9073, #41115, .T. ) ;
#6655 = CARTESIAN_POINT ( 'NONE',  ( 22.88143834593734027, -16.17571944551308860, -46.47913774983016566 ) ) ;
#6656 = CARTESIAN_POINT ( 'NONE',  ( -0.007164378094141890356, 19.48649803870589992, -34.77269719633950018 ) ) ;
#6657 = CARTESIAN_POINT ( 'NONE',  ( 46.61365481427139912, -53.40542986336679832, -76.07618347743780873 ) ) ;
#6658 = CARTESIAN_POINT ( 'NONE',  ( 60.84977283502919931, 12.51329875045430029, -9.366796605703170187 ) ) ;
#6659 = FACE_OUTER_BOUND ( 'NONE', #45429, .T. ) ;
#6660 = CARTESIAN_POINT ( 'NONE',  ( 53.38272065464079930, 20.08420318064650090, -75.68264751698761472 ) ) ;
#6661 = CARTESIAN_POINT ( 'NONE',  ( 24.04465145034966156, -15.61618865458276595, -39.79233592887338489 ) ) ;
#6662 = EDGE_CURVE ( 'NONE', #2811, #17149, #14640, .T. ) ;
#6663 = CARTESIAN_POINT ( 'NONE',  ( 10.80048316119169982, -9.328284477191109758, -32.78375144850900114 ) ) ;
#6664 = EDGE_LOOP ( 'NONE', ( #3512, #33094, #35932, #24447, #30271, #49934 ) ) ;
#6666 = EDGE_CURVE ( 'NONE', #22911, #3350, #28529, .T. ) ;
#6665 = CARTESIAN_POINT ( 'NONE',  ( -31.07316938349034885, -53.11618894467940066, 17.05710678118654755 ) ) ;
#6667 = CARTESIAN_POINT ( 'NONE',  ( 4.986282691042689841, -58.88488589497760728, -12.65546072889769924 ) ) ;
#6668 = CARTESIAN_POINT ( 'NONE',  ( 75.73654537959819777, -5.923657072368180287, -11.84124065471690024 ) ) ;
#6669 = CARTESIAN_POINT ( 'NONE',  ( 75.07825548516527192, 13.81215145325568550, -14.79904531683525626 ) ) ;
#6670 = CARTESIAN_POINT ( 'NONE',  ( 75.19651472130358627, -44.95919067516332035, -14.38756988197933495 ) ) ;
#6671 = VECTOR ( 'NONE', #469, 1000.000000000000000 ) ;
#6672 = CONICAL_SURFACE ( 'NONE', #44290, 0.7350000000000010969, 0.06981317007977388966 ) ;
#6673 = CARTESIAN_POINT ( 'NONE',  ( 12.75813532167091324, -55.47348756089835575, -75.58682750841406062 ) ) ;
#6674 = AXIS2_PLACEMENT_3D ( 'NONE', #39344, #14712, #3445 ) ;
#6675 = CARTESIAN_POINT ( 'NONE',  ( 29.99034385824719706, -15.61618894467929941, -32.14999999999999858 ) ) ;
#6676 = CARTESIAN_POINT ( 'NONE',  ( 63.16529205807979963, 1.278021359705829862, -62.63015105704829466 ) ) ;
#6677 = LINE ( 'NONE', #10613, #39044 ) ;
#6678 = AXIS2_PLACEMENT_3D ( 'NONE', #13966, #34112, #29920 ) ;
#6679 = CARTESIAN_POINT ( 'NONE',  ( 40.36721523011259904, 13.65407319109449880, -4.296538310234210734 ) ) ;
#6680 = DIRECTION ( 'NONE',  ( 0.000000000000000000, -1.000000000000000000, 0.000000000000000000 ) ) ;
#6681 = CARTESIAN_POINT ( 'NONE',  ( 10.03166977892449552, -53.91985561451862452, -34.73809820100212420 ) ) ;
#6682 = FACE_OUTER_BOUND ( 'NONE', #11968, .T. ) ;
#6683 = VECTOR ( 'NONE', #4868, 1000.000000000000000 ) ;
#6684 = CARTESIAN_POINT ( 'NONE',  ( 22.84664696149711105, -16.49985153785048908, -62.49449331979504052 ) ) ;
#6685 = CARTESIAN_POINT ( 'NONE',  ( 17.83683460335419824, -52.03647206054819918, -75.81086730487160708 ) ) ;
#6686 = CARTESIAN_POINT ( 'NONE',  ( 58.84619698805219912, -43.44629174156790441, -8.775524122719259523 ) ) ;
#6687 = ORIENTED_EDGE ( 'NONE', *, *, #37574, .T. ) ;
#6688 = EDGE_CURVE ( 'NONE', #26597, #44905, #19972, .T. ) ;
#6689 = CARTESIAN_POINT ( 'NONE',  ( 13.70954523500570055, -22.66097545527179946, -51.67284482273019819 ) ) ;
#6690 =( BOUNDED_CURVE ( )  B_SPLINE_CURVE ( 3, ( #7353, #31682, #3426, #28017 ),
 .UNSPECIFIED., .F., .T. ) 
 B_SPLINE_CURVE_WITH_KNOTS ( ( 4, 4 ),
 ( 0.7853981633974506105, 1.570796326794898334 ),
 .UNSPECIFIED. ) 
 CURVE ( )  GEOMETRIC_REPRESENTATION_ITEM ( )  RATIONAL_B_SPLINE_CURVE ( ( 1.000000000000000000, 0.9492530216741912330, 0.9492530216741912330, 1.000000000000000000 ) ) 
 REPRESENTATION_ITEM ( '' )  );
#6691 = CARTESIAN_POINT ( 'NONE',  ( 63.72050982575409961, 1.191618978581419963, -61.62625993902970123 ) ) ;
#6692 = VERTEX_POINT ( 'NONE', #14625 ) ;
#6693 = CARTESIAN_POINT ( 'NONE',  ( 15.24817145470214719, -22.38319284411442212, -68.99448578136716037 ) ) ;
#6694 = CARTESIAN_POINT ( 'NONE',  ( 60.41799884498819750, -45.84359652593190049, -47.74079192425810447 ) ) ;
#6695 = CARTESIAN_POINT ( 'NONE',  ( 56.17779366879769753, 14.41653637947479893, -28.15000000000000213 ) ) ;
#6696 = CARTESIAN_POINT ( 'NONE',  ( 29.63393739769620083, -15.61618894467929941, 4.349999999999999645 ) ) ;
#6697 = CARTESIAN_POINT ( 'NONE',  ( 9.074293494951078287, -16.25319589821559774, -81.23899999999999011 ) ) ;
#6698 = CARTESIAN_POINT ( 'NONE',  ( 41.19621318014409894, -45.49641962229259917, -6.107574381499630611 ) ) ;
#6699 = EDGE_CURVE ( 'NONE', #40057, #15227, #26666, .T. ) ;
#6700 = ORIENTED_EDGE ( 'NONE', *, *, #48595, .F. ) ;
#6701 = ORIENTED_EDGE ( 'NONE', *, *, #1133, .F. ) ;
#6702 = ORIENTED_EDGE ( 'NONE', *, *, #26777, .T. ) ;
#6703 = CARTESIAN_POINT ( 'NONE',  ( 55.55365133010059964, -45.11618894467940066, -14.32025150907159983 ) ) ;
#6704 = CARTESIAN_POINT ( 'NONE',  ( 61.39588726022179799, -45.18041116279739811, -46.45920956806440216 ) ) ;
#6705 = CARTESIAN_POINT ( 'NONE',  ( 82.46534343335889616, -45.09316689051424731, -46.44242255414575737 ) ) ;
#6706 = ORIENTED_EDGE ( 'NONE', *, *, #1153, .T. ) ;
#6707 = CARTESIAN_POINT ( 'NONE',  ( 10.05068326232998288, -12.54826803111968303, -79.60166762876662006 ) ) ;
#6708 = ORIENTED_EDGE ( 'NONE', *, *, #13673, .T. ) ;
#6709 = CARTESIAN_POINT ( 'NONE',  ( 20.11809143863368377, -8.703679352620326881, -63.45899965378977470 ) ) ;
#6710 = CIRCLE ( 'NONE', #43518, 21.72891455324079857 ) ;
#6711 = CARTESIAN_POINT ( 'NONE',  ( -0.007164427059766999631, 19.48649803864789831, -34.77269723891829756 ) ) ;
#6712 = AXIS2_PLACEMENT_3D ( 'NONE', #2441, #2711, #8122 ) ;
#6713 = AXIS2_PLACEMENT_3D ( 'NONE', #15930, #23766, #27453 ) ;
#6714 = ORIENTED_EDGE ( 'NONE', *, *, #31813, .F. ) ;
#6715 = CARTESIAN_POINT ( 'NONE',  ( 0.3209249304026170480, -46.25141913721060405, -34.64999999999999858 ) ) ;
#6716 = CARTESIAN_POINT ( 'NONE',  ( 51.15928635398449842, -50.96517669477629653, -76.15045079391039451 ) ) ;
#6717 = VECTOR ( 'NONE', #30262, 1000.000000000000000 ) ;
#6718 = CARTESIAN_POINT ( 'NONE',  ( 60.32710813244079873, 14.50229188127310032, -47.29630948315320182 ) ) ;
#6719 = CIRCLE ( 'NONE', #11735, 6.100000000000001421 ) ;
#6720 = CARTESIAN_POINT ( 'NONE',  ( 61.75019796695539753, 14.88381105532069881, -37.26101630944549470 ) ) ;
#6721 = CARTESIAN_POINT ( 'NONE',  ( 40.73531874280419629, -44.64268826760660147, -4.523453480819620509 ) ) ;
#6722 = B_SPLINE_CURVE_WITH_KNOTS ( 'NONE', 3,
 ( #37566, #37055, #1151, #49387, #18170, #17148, #44923, #9024, #37314, #33884, #49895, #24968, #13483, #5100, #25499, #41502, #5616, #10057, #1675, #26017 ),
 .UNSPECIFIED., .F., .F.,
 ( 4, 2, 2, 2, 2, 2, 2, 2, 2, 4 ),
 ( 0.000000000000000000, 0.08842663233073849716, 0.2261948956704462055, 0.3749999999999999445, 0.4999999999999988898, 0.5624999999999988898, 0.6624999999999995337, 0.7983826544642954604, 0.9363829142756890933, 1.000000000000000000 ),
 .UNSPECIFIED. ) ;
#6723 = DIRECTION ( 'NONE',  ( 0.000000000000000000, -1.000000000000000000, 0.000000000000000000 ) ) ;
#6724 = CARTESIAN_POINT ( 'NONE',  ( -3.308601418378690262, 17.32579908435650040, -5.270794404415338974 ) ) ;
#6725 = CARTESIAN_POINT ( 'NONE',  ( 64.48795401538340855, 1.045503847279079856, -70.40650121518619642 ) ) ;
#6726 = CARTESIAN_POINT ( 'NONE',  ( 22.78736197255772922, -17.44565462478292872, -42.93322834753961814 ) ) ;
#6727 = CARTESIAN_POINT ( 'NONE',  ( 16.13393739769620083, -15.61618894467929941, -9.721247897589949005 ) ) ;
#6728 = CARTESIAN_POINT ( 'NONE',  ( 8.836122779856628640, -12.73024889214359945, -48.40737475858179550 ) ) ;
#6729 = ORIENTED_EDGE ( 'NONE', *, *, #26096, .F. ) ;
#6731 = ADVANCED_FACE ( 'NONE', ( #34258 ), #40379, .T. ) ;
#6730 = CARTESIAN_POINT ( 'NONE',  ( 14.53574929604680044, -52.38593004734789815, -75.99067819366339904 ) ) ;
#6732 = CARTESIAN_POINT ( 'NONE',  ( 51.64361810415240939, 19.75411576426495586, 11.97999999999999865 ) ) ;
#6733 = CARTESIAN_POINT ( 'NONE',  ( 11.89321892218980103, -65.43602743108449715, -22.25048313876769868 ) ) ;
#6734 = EDGE_CURVE ( 'NONE', #47505, #18529, #12768, .T. ) ;
#6735 = CARTESIAN_POINT ( 'NONE',  ( 45.50949004153680733, -40.06418272001256042, -59.34096905993463622 ) ) ;
#6736 = CARTESIAN_POINT ( 'NONE',  ( 16.13393739769620083, -15.61618894467929941, -81.65000000000000568 ) ) ;
#6737 = CARTESIAN_POINT ( 'NONE',  ( 20.98195727178219983, -10.76281971865039999, -32.14999999999999858 ) ) ;
#6738 = CARTESIAN_POINT ( 'NONE',  ( 16.13393739769620083, -15.61618894467929941, -32.14999999999999858 ) ) ;
#6739 = CARTESIAN_POINT ( 'NONE',  ( 65.27736602627911111, 1.383811055320669947, -70.34999999999999432 ) ) ;
#6740 = CARTESIAN_POINT ( 'NONE',  ( 47.86038305415719663, -54.40158572345529819, -54.84188222968870008 ) ) ;
#6741 = DIRECTION ( 'NONE',  ( 0.000000000000000000, 0.000000000000000000, -1.000000000000000000 ) ) ;
#6742 = CARTESIAN_POINT ( 'NONE',  ( 17.32262310423930174, -8.664240623128923957, -36.40108501799142005 ) ) ;
#6743 = CARTESIAN_POINT ( 'NONE',  ( 47.79491795492819506, 23.18827802853950004, -54.76904050233790144 ) ) ;
#6744 = CIRCLE ( 'NONE', #51113, 14.50000000000000178 ) ;
#6745 = ORIENTED_EDGE ( 'NONE', *, *, #35259, .F. ) ;
#6746 = CARTESIAN_POINT ( 'NONE',  ( 23.08438461476639958, -16.81362063674830054, -74.90148551491040507 ) ) ;
#6747 = ORIENTED_EDGE ( 'NONE', *, *, #16591, .F. ) ;
#6748 = CARTESIAN_POINT ( 'NONE',  ( 71.25801539443460797, 1.385702546077159925, -70.29781821095090777 ) ) ;
#6749 = AXIS2_PLACEMENT_3D ( 'NONE', #954, #16951, #41046 ) ;
#6750 = DIRECTION ( 'NONE',  ( 0.000000000000000000, -1.000000000000000000, 0.000000000000000000 ) ) ;
#6751 = DIRECTION ( 'NONE',  ( 0.000000000000000000, 0.000000000000000000, -1.000000000000000000 ) ) ;
#6753 = DIRECTION ( 'NONE',  ( 0.000000000000000000, 0.000000000000000000, -1.000000000000000000 ) ) ;
#6752 = CARTESIAN_POINT ( 'NONE',  ( 84.44784216359251161, 11.88381105532070059, -47.47585302082339354 ) ) ;
#6754 = VECTOR ( 'NONE', #41439, 1000.000000000000000 ) ;
#6755 = AXIS2_PLACEMENT_3D ( 'NONE', #25183, #30152, #50353 ) ;
#6756 = DIRECTION ( 'NONE',  ( 0.000000000000000000, 0.000000000000000000, 1.000000000000000000 ) ) ;
#6757 = CARTESIAN_POINT ( 'NONE',  ( 71.62484648860579739, 0.9098571636355720083, -70.52991329011129551 ) ) ;
#6758 = DIRECTION ( 'NONE',  ( 0.000000000000000000, 0.000000000000000000, -1.000000000000000000 ) ) ;
#6759 = EDGE_CURVE ( 'NONE', #19317, #51151, #23324, .T. ) ;
#6760 = B_SPLINE_SURFACE_WITH_KNOTS ( 'NONE', 3, 3, ( 
 ( #9613, #32914, #25046, #49201, #33440, #13549, #5426, #45516, #45773, #9865, #44733, #4900, #13293, #41063, #24789, #25819 ),
 ( #21896, #41831, #16691, #5175, #48673, #32648, #12777, #8838, #45259, #41571, #40797, #21130, #25313, #38419, #22928, #46559 ),
 ( #30280, #38162, #10910, #42620, #14311, #38948, #50731, #10649, #18753, #6976, #26872, #46038, #2518, #6718, #14830, #50481 ),
 ( #50989, #22673, #30536, #26604, #26087, #3038, #42879, #46300, #6456, #10387, #19012, #34988, #47078, #15089, #10129, #38693 ),
 ( #43140, #2260, #34200, #2782, #34729, #30794, #7232, #26343, #42355, #22416, #46820, #31055, #14054, #18500, #11166, #33947 ),
 ( #27134, #30015, #42095, #34471, #6198, #18235, #37907, #2000, #17980, #49964, #22153, #50222, #14571, #36025, #20029, #39462 ),
 ( #24201, #16111, #31821, #43392, #7487, #16372, #136, #28408, #40227, #23182, #44416, #23439, #47585, #19532, #39199, #3559 ),
 ( #43901, #11941, #3294, #7996, #4316, #23948, #7751, #39968, #32327, #35520, #32073, #51510, #15610, #23698, #4063, #48091 ),
 ( #27647, #48348, #31564, #27898, #28150, #19273, #35258, #12443, #44154, #11680, #39713, #20285, #43650, #3817, #51258, #15353 ),
 ( #19786, #35778, #31305, #36278, #12190, #8250, #386, #47334, #27390, #47838, #51761, #11426, #15861, #49658, #13497, #907 ),
 ( #32581, #25509, #16901, #9558, #21323, #13749, #24465, #44672, #17413, #8518, #8775, #13239, #5115, #28932, #41257, #45195 ) ),
 .UNSPECIFIED., .F., .F., .F.,
 ( 4, 1, 1, 1, 1, 1, 1, 1, 4 ),
 ( 4, 2, 2, 2, 2, 2, 2, 4 ),
 ( 0.000000000000000000, 0.1250000000000000000, 0.2500000000000000000, 0.3750000000000000000, 0.5000000000000000000, 0.6250000000000000000, 0.7500000000000000000, 0.8750000000000000000, 1.000000000000000000 ),
 ( 0.000000000000000000, 0.1402455969909039979, 0.3005262792662219962, 0.4007017056882959949, 0.4507894188993329943, 0.5309297600369919934, 0.6591543058572471026, 0.8014034113765919898 ),
 .UNSPECIFIED. ) ;
#6761 = ORIENTED_EDGE ( 'NONE', *, *, #4784, .F. ) ;
#6762 = CARTESIAN_POINT ( 'NONE',  ( 11.51160566532330165, 19.89559162839070083, -21.14999999999999858 ) ) ;
#6763 = ORIENTED_EDGE ( 'NONE', *, *, #1106, .T. ) ;
#6764 = VERTEX_POINT ( 'NONE', #44468 ) ;
#6765 = CARTESIAN_POINT ( 'NONE',  ( 12.24533245415720017, -64.90027884028160088, -16.17634614696339668 ) ) ;
#6766 = CARTESIAN_POINT ( 'NONE',  ( 29.12893361417137328, -4.494242171482554227, -35.06842082984485387 ) ) ;
#6767 = CARTESIAN_POINT ( 'NONE',  ( 76.46365438545950610, -25.95764364605460983, -13.07079957363982814 ) ) ;
#6768 = CARTESIAN_POINT ( 'NONE',  ( 12.89950475509210115, -65.51158420262359527, -47.71261340485989422 ) ) ;
#6769 = VERTEX_POINT ( 'NONE', #40535 ) ;
#6770 = EDGE_LOOP ( 'NONE', ( #25594, #32626, #41467, #33041 ) ) ;
#6771 = CARTESIAN_POINT ( 'NONE',  ( 71.62064552848029564, 0.9479899806831150189, -60.76708149872590070 ) ) ;
#6772 = DIRECTION ( 'NONE',  ( 0.000000000000000000, 0.000000000000000000, 1.000000000000000000 ) ) ;
#6773 = CARTESIAN_POINT ( 'NONE',  ( 47.68692968653899555, 23.40598529524750049, -55.28501249849080068 ) ) ;
#6774 = CARTESIAN_POINT ( 'NONE',  ( 64.67926456151019465, 0.3460283776947450374, -17.08790319438210048 ) ) ;
#6775 = CARTESIAN_POINT ( 'NONE',  ( 51.86152422305890042, -49.39855420986879864, -77.00280416433220410 ) ) ;
#6776 = CARTESIAN_POINT ( 'NONE',  ( 56.78254564749959599, -50.61158444988599570, -53.13069165659919690 ) ) ;
#6777 = VERTEX_POINT ( 'NONE', #48143 ) ;
#6778 = CARTESIAN_POINT ( 'NONE',  ( 24.04468094043696880, -15.55032358031935047, -33.78968039492959718 ) ) ;
#6779 = CARTESIAN_POINT ( 'NONE',  ( 15.09849799342586607, -23.52720200456179711, -48.33399909089389723 ) ) ;
#6780 = ORIENTED_EDGE ( 'NONE', *, *, #42246, .F. ) ;
#6781 = CARTESIAN_POINT ( 'NONE',  ( 17.90524838325329071, -9.025333659381530538, -52.03615204234977654 ) ) ;
#6782 = CARTESIAN_POINT ( 'NONE',  ( 14.13393739769649926, 18.32493655227499829, -34.64999999999999858 ) ) ;
#6783 = CARTESIAN_POINT ( 'NONE',  ( 21.25937865767100021, -21.55896602969010090, -46.28595751040398909 ) ) ;
#6784 = CARTESIAN_POINT ( 'NONE',  ( 13.79398456934750072, -51.11484069242550277, -22.16948675641290123 ) ) ;
#6786 = CARTESIAN_POINT ( 'NONE',  ( 54.67587076525569501, 19.38381105532069881, -76.72550994220580378 ) ) ;
#6785 = B_SPLINE_CURVE_WITH_KNOTS ( 'NONE', 3,
 ( #49421, #25533, #13517, #28690, #17183, #5134, #20828, #36825, #21090, #5652, #6947, #14283, #30507, #17946, #29725, #33914, #18721, #46004, #38388, #10877, #42850, #41796, #46530, #22899, #18466, #34171, #34439, #38916, #22384, #10619, #49932, #50449, #18205, #50189, #50700, #45739, #3007, #21865, #10356, #6164, #26573, #26840 ),
 .UNSPECIFIED., .F., .F.,
 ( 4, 2, 2, 1, 1, 2, 2, 2, 2, 1, 1, 2, 2, 2, 2, 1, 1, 2, 2, 2, 1, 1, 2, 2, 4 ),
 ( 0.000000000000000000, 0.1250000000000936196, 0.1875000000001387224, 0.2187500000001632583, 0.2343750000001697253, 0.2421875000001709188, 0.2500000000001720846, 0.3750000000001643685, 0.4375000000001614819, 0.4687500000001668110, 0.4843750000001631473, 0.4921875000001623701, 0.5000000000001615375, 0.6250000000001039169, 0.6875000000000743849, 0.7187500000000507372, 0.7343750000000396350, 0.7421875000000440759, 0.7500000000000484057, 0.8125000000000045519, 0.8437499999999744649, 0.8593749999999678035, 0.8671874999999650280, 0.8749999999999622524, 1.000000000000000000 ),
 .UNSPECIFIED. ) ;
#6787 = CARTESIAN_POINT ( 'NONE',  ( 46.70520323956110076, -53.35084480228680093, -76.07728942632040514 ) ) ;
#6788 = CARTESIAN_POINT ( 'NONE',  ( 57.24436406277250455, 13.89534489142819851, -17.69598351972189931 ) ) ;
#6789 = CARTESIAN_POINT ( 'NONE',  ( 10.74314122376619984, -11.06845590621349906, -78.07024275745519049 ) ) ;
#6790 = CARTESIAN_POINT ( 'NONE',  ( 56.56050783365309798, -50.71580908316560254, -53.48830978476309639 ) ) ;
#6791 = AXIS2_PLACEMENT_3D ( 'NONE', #10995, #10217, #22244 ) ;
#6792 = CARTESIAN_POINT ( 'NONE',  ( 14.74159083669250059, -8.702150310963681079, -48.28392467753440087 ) ) ;
#6793 = CARTESIAN_POINT ( 'NONE',  ( 12.72586417107244827, -9.703323737910269031, -43.78612585668066970 ) ) ;
#6794 = VECTOR ( 'NONE', #13155, 1000.000000000000000 ) ;
#6795 = ORIENTED_EDGE ( 'NONE', *, *, #21797, .T. ) ;
#6797 = ADVANCED_FACE ( 'NONE', ( #20598 ), #9183, .T. ) ;
#6796 = CARTESIAN_POINT ( 'NONE',  ( 47.42018403062719756, 23.12668429572390139, -75.11910893338719575 ) ) ;
#6798 = CARTESIAN_POINT ( 'NONE',  ( 64.84324960441189489, 0.8888742037077609348, -60.63285689971630177 ) ) ;
#6799 = CARTESIAN_POINT ( 'NONE',  ( 14.06334000076352098, -7.911067765953196051, -50.92433393874132008 ) ) ;
#6800 = CARTESIAN_POINT ( 'NONE',  ( 44.45072406794265163, -15.61618894467929408, 6.072546842075589701 ) ) ;
#6801 = CARTESIAN_POINT ( 'NONE',  ( 8.942935310824880801, -49.33243882768289978, -34.64999999999999858 ) ) ;
#6802 = DIRECTION ( 'NONE',  ( 0.1961161351381840445, 0.000000000000000000, 0.9805806756909201116 ) ) ;
#6803 = FACE_OUTER_BOUND ( 'NONE', #33110, .T. ) ;
#6804 = CARTESIAN_POINT ( 'NONE',  ( -21.98676283070069815, -6.896957895883470080, -53.98713251066509855 ) ) ;
#6806 = CARTESIAN_POINT ( 'NONE',  ( -0.03447620312152738231, -22.81072779144790275, -34.79644660940672907 ) ) ;
#6805 = CARTESIAN_POINT ( 'NONE',  ( 53.82997852138471018, 19.36722236602833291, -77.06221308720526508 ) ) ;
#6807 = DIRECTION ( 'NONE',  ( 0.000000000000000000, 0.000000000000000000, 1.000000000000000000 ) ) ;
#6808 = DIRECTION ( 'NONE',  ( 0.000000000000000000, 0.000000000000000000, 1.000000000000000000 ) ) ;
#6809 = CARTESIAN_POINT ( 'NONE',  ( -32.94143001319760344, -10.86309130919419985, -56.02216466475820056 ) ) ;
#6810 = ORIENTED_EDGE ( 'NONE', *, *, #42522, .F. ) ;
#6811 = CARTESIAN_POINT ( 'NONE',  ( 52.83452152375440392, -49.66311762893110426, -48.76554745825549730 ) ) ;
#6812 = ORIENTED_EDGE ( 'NONE', *, *, #27902, .T. ) ;
#6813 = CARTESIAN_POINT ( 'NONE',  ( 17.47784055284634164, 21.13935400224278283, -76.01806011802844409 ) ) ;
#6814 = CARTESIAN_POINT ( 'NONE',  ( 22.46012469463212469, -20.47783660219755220, -74.00066485091836910 ) ) ;
#6815 = CARTESIAN_POINT ( 'NONE',  ( 13.56093559663669978, 20.01022379959449893, -22.27875244362760299 ) ) ;
#6816 = CARTESIAN_POINT ( 'NONE',  ( 83.70899958829821230, 13.23037409732310010, -46.59258846095900708 ) ) ;
#6817 = CARTESIAN_POINT ( 'NONE',  ( 9.082333282492209392, -15.48413554993459940, -45.45878041868800068 ) ) ;
#6818 = CARTESIAN_POINT ( 'NONE',  ( 52.68346203708500042, 18.53457133105899857, -48.72605036086640240 ) ) ;
#6819 = CARTESIAN_POINT ( 'NONE',  ( 56.08437071186119738, -45.70248805069130071, -17.77137460264779989 ) ) ;
#6820 = EDGE_CURVE ( 'NONE', #6962, #26597, #40973, .T. ) ;
#6821 = CYLINDRICAL_SURFACE ( 'NONE', #38100, 2.000000000000170530 ) ;
#6822 = ORIENTED_EDGE ( 'NONE', *, *, #34531, .F. ) ;
#6823 = CARTESIAN_POINT ( 'NONE',  ( 23.94862035779809872, -16.33554867129409871, -37.31672440967509630 ) ) ;
#6824 = EDGE_CURVE ( 'NONE', #1526, #4493, #21401, .T. ) ;
#6825 = ORIENTED_EDGE ( 'NONE', *, *, #4071, .F. ) ;
#6826 = DIRECTION ( 'NONE',  ( -0.4640893551880381218, 0.8857883891772070362, 0.000000000000000000 ) ) ;
#6827 = CARTESIAN_POINT ( 'NONE',  ( 10.42914237359489960, 33.65646982241409546, -47.08729022436619971 ) ) ;
#6828 = CARTESIAN_POINT ( 'NONE',  ( 72.94510729672219895, 1.263823323415690147, -62.32316323322979912 ) ) ;
#6829 = AXIS2_PLACEMENT_3D ( 'NONE', #26373, #42652, #2032 ) ;
#6830 = CARTESIAN_POINT ( 'NONE',  ( 55.91595722987329964, -45.90465052577939531, -25.32543029193989881 ) ) ;
#6831 = CARTESIAN_POINT ( 'NONE',  ( 52.57435367313225782, -49.85246693219066572, -48.51308846454130475 ) ) ;
#6832 = DIRECTION ( 'NONE',  ( 0.000000000000000000, 0.000000000000000000, -1.000000000000000000 ) ) ;
#6833 = CARTESIAN_POINT ( 'NONE',  ( 22.03288545771612306, -12.23521849110922233, -62.28727064598228935 ) ) ;
#6834 = AXIS2_PLACEMENT_3D ( 'NONE', #4761, #31737, #43827 ) ;
#6835 = TOROIDAL_SURFACE ( 'NONE', #21846, 14.50000000000000000, 1.500000000000000000 ) ;
#6836 = CARTESIAN_POINT ( 'NONE',  ( 20.89950193901299613, -21.95748695813169959, -45.80256656510095326 ) ) ;
#6837 = VERTEX_POINT ( 'NONE', #14280 ) ;
#6838 = CARTESIAN_POINT ( 'NONE',  ( 64.89503925317049493, 1.371509258145880095, -70.32114135108699315 ) ) ;
#6839 = ORIENTED_EDGE ( 'NONE', *, *, #18392, .T. ) ;
#6840 = CARTESIAN_POINT ( 'NONE',  ( 10.48523087532100107, -63.11543068638779630, -45.62962604688630108 ) ) ;
#6841 = CARTESIAN_POINT ( 'NONE',  ( 9.221455577410790028, -11.63198688526945546, -46.95899850799102637 ) ) ;
#6842 = ORIENTED_EDGE ( 'NONE', *, *, #41294, .T. ) ;
#6843 = CARTESIAN_POINT ( 'NONE',  ( 16.13393739769620083, -38.61618894467930119, -59.64999999999999147 ) ) ;
#6844 = CARTESIAN_POINT ( 'NONE',  ( 57.28991729228510366, 19.34649676830889931, -53.44461810997239581 ) ) ;
#6845 = CARTESIAN_POINT ( 'NONE',  ( 53.79479188179159621, 19.37048951312020151, -76.98386108904900027 ) ) ;
#6846 = ORIENTED_EDGE ( 'NONE', *, *, #19462, .T. ) ;
#6847 = CARTESIAN_POINT ( 'NONE',  ( 8.875293496618541056, -63.51482374781645746, -46.68678634667735139 ) ) ;
#6848 = CYLINDRICAL_SURFACE ( 'NONE', #17517, 6.766999999999998572 ) ;
#6849 = CARTESIAN_POINT ( 'NONE',  ( 15.05440318628110141, 21.88381105532300097, -76.14999999999999147 ) ) ;
#6850 = CARTESIAN_POINT ( 'NONE',  ( 14.06321007543174417, -7.911101406802497849, -69.20899948135398461 ) ) ;
#6851 = CARTESIAN_POINT ( 'NONE',  ( 23.82603912714330363, -18.58507611662970049, -61.90958082047689004 ) ) ;
#6852 = DIRECTION ( 'NONE',  ( 1.882763000000000063E-17, 1.367908000000000040E-17, -1.000000000000000000 ) ) ;
#6853 = CARTESIAN_POINT ( 'NONE',  ( 46.52731067088307526, -38.20626701087121546, -57.68312601967695485 ) ) ;
#6854 = VERTEX_POINT ( 'NONE', #38385 ) ;
#6855 = VERTEX_POINT ( 'NONE', #41532 ) ;
#6856 = CARTESIAN_POINT ( 'NONE',  ( -22.84939731388132245, -15.19272276721277493, -54.74980512766139640 ) ) ;
#6857 = CARTESIAN_POINT ( 'NONE',  ( 21.31786979423969797, -20.96722050067040399, -56.48770572707099547 ) ) ;
#6858 = VECTOR ( 'NONE', #31378, 1000.000000000000114 ) ;
#6859 = CARTESIAN_POINT ( 'NONE',  ( 52.56445806708630641, -49.86260722447150329, -48.47378032971909789 ) ) ;
#6860 = CARTESIAN_POINT ( 'NONE',  ( 8.912722752349319322, -17.33563004555450249, -32.14999999999999858 ) ) ;
#6862 = EDGE_CURVE ( 'NONE', #8182, #9073, #2017, .T. ) ;
#6861 = DIRECTION ( 'NONE',  ( 0.000000000000000000, 0.000000000000000000, 1.000000000000000000 ) ) ;
#6863 = DIRECTION ( 'NONE',  ( 7.935614746461580696E-16, 6.060292087350920604E-16, -1.000000000000000000 ) ) ;
#6864 = EDGE_CURVE ( 'NONE', #50522, #8604, #28270, .T. ) ;
#6865 = DIRECTION ( 'NONE',  ( 1.000000000000000000, 0.000000000000000000, 0.000000000000000000 ) ) ;
#6866 = CARTESIAN_POINT ( 'NONE',  ( 41.23778026548699671, -45.08170077868949477, -5.742147589652049966 ) ) ;
#6867 = AXIS2_PLACEMENT_3D ( 'NONE', #39707, #46814, #19263 ) ;
#6868 = DIRECTION ( 'NONE',  ( 0.000000000000000000, 1.000000000000000000, 0.000000000000000000 ) ) ;
#6869 = CARTESIAN_POINT ( 'NONE',  ( 13.39647449081169839, -23.39365752657710473, -68.11539470288319364 ) ) ;
#6870 = CARTESIAN_POINT ( 'NONE',  ( 54.18928026078430094, -48.04840664809780293, -26.03349461057250025 ) ) ;
#6871 = CARTESIAN_POINT ( 'NONE',  ( 56.50083622498900127, -50.76116396499730143, -74.29147146558989334 ) ) ;
#6873 = CARTESIAN_POINT ( 'NONE',  ( 16.13393739769620083, -15.61618894467929941, -19.14999999999999858 ) ) ;
#6872 = CARTESIAN_POINT ( 'NONE',  ( -8.804542933903709567, 12.11215359422420157, -4.447949915414280753 ) ) ;
#6874 = CARTESIAN_POINT ( 'NONE',  ( 47.18324681005260146, -54.80726426785999905, -54.61059023070370699 ) ) ;
#6875 = CARTESIAN_POINT ( 'NONE',  ( 47.18325654339099628, 23.57487866773040253, -54.61058579560449289 ) ) ;
#6876 = ORIENTED_EDGE ( 'NONE', *, *, #14, .T. ) ;
#6877 = CARTESIAN_POINT ( 'NONE',  ( -8.116933555837720249, -44.87420182772909527, -5.094470740012030596 ) ) ;
#6878 = CARTESIAN_POINT ( 'NONE',  ( 47.80451765783929829, 23.19120698434290162, -54.80734825992600179 ) ) ;
#6879 = CARTESIAN_POINT ( 'NONE',  ( 56.17779366879769753, -45.64891426883350078, -28.15000000000000213 ) ) ;
#6880 = DIRECTION ( 'NONE',  ( 0.000000000000000000, -1.000000000000000000, 0.000000000000000000 ) ) ;
#6881 = CARTESIAN_POINT ( 'NONE',  ( 61.12568535967459837, 14.12366961404920040, -47.15003794073030008 ) ) ;
#6882 = CARTESIAN_POINT ( 'NONE',  ( 12.04669083382830053, 34.10719181568249780, -17.12210558019860329 ) ) ;
#6883 = CARTESIAN_POINT ( 'NONE',  ( 51.75950492042200324, 18.21739703323269666, -76.84761919141568853 ) ) ;
#6884 = CARTESIAN_POINT ( 'NONE',  ( 53.18776295313059421, 18.24184040730330025, -48.84930895489249991 ) ) ;
#6885 = DIRECTION ( 'NONE',  ( 0.000000000000000000, 1.000000000000000000, 0.000000000000000000 ) ) ;
#6886 = CARTESIAN_POINT ( 'NONE',  ( 13.10629489870503583, 18.33238584480843159, -34.89146800830128115 ) ) ;
#6887 = CARTESIAN_POINT ( 'NONE',  ( 55.96589641171290452, 15.46583100414529888, -26.32679269575499958 ) ) ;
#6888 = CARTESIAN_POINT ( 'NONE',  ( 50.58453602478152789, 4.710080170683036194, -76.22811488052452944 ) ) ;
#6889 = EDGE_CURVE ( 'NONE', #51433, #12167, #42629, .T. ) ;
#6890 = CARTESIAN_POINT ( 'NONE',  ( 9.746758075853771075, -63.31345910889199757, -46.29788637164419640 ) ) ;
#6891 = CARTESIAN_POINT ( 'NONE',  ( 24.04493739769620930, -15.61618894467930119, -81.23899999999999011 ) ) ;
#6892 = DIRECTION ( 'NONE',  ( 0.4042525045258802963, 0.000000000000000000, -0.9146474252872268673 ) ) ;
#6893 = CARTESIAN_POINT ( 'NONE',  ( 71.34390086684349797, 1.188582381068100213, -60.69479001402090290 ) ) ;
#6894 = CARTESIAN_POINT ( 'NONE',  ( 10.77457706359389888, 32.17075419748780263, -45.20848294960729419 ) ) ;
#6895 = CARTESIAN_POINT ( 'NONE',  ( 72.88602187343720118, 1.308647200627810259, -62.31695083504749988 ) ) ;
#6896 = DIRECTION ( 'NONE',  ( 0.3294064756440934771, -0.9441882088883220003, -3.885780586188049864E-16 ) ) ;
#6897 = CARTESIAN_POINT ( 'NONE',  ( 22.90093729192429350, -15.13018493110448759, -66.42996439909107664 ) ) ;
#6898 = VERTEX_POINT ( 'NONE', #37595 ) ;
#6899 = ORIENTED_EDGE ( 'NONE', *, *, #24996, .T. ) ;
#6900 = CARTESIAN_POINT ( 'NONE',  ( 40.50275707922880031, 13.54185611314979987, -4.148922232357650230 ) ) ;
#6901 = CARTESIAN_POINT ( 'NONE',  ( 76.55750383288518890, 0.1397330900750557992, -13.47521080995300480 ) ) ;
#6902 = ORIENTED_EDGE ( 'NONE', *, *, #28370, .T. ) ;
#6903 = CARTESIAN_POINT ( 'NONE',  ( 56.51428737249189993, -45.39462441605950005, -25.50343997284580055 ) ) ;
#6904 = DIRECTION ( 'NONE',  ( 0.000000000000000000, 0.000000000000000000, 1.000000000000000000 ) ) ;
#6905 = CIRCLE ( 'NONE', #4373, 9.000000000000007105 ) ;
#6906 = B_SPLINE_CURVE_WITH_KNOTS ( 'NONE', 3,
 ( #37916, #5439, #21394, #9874, #30292, #22163, #45265, #6467, #38175, #38428, #2531, #37397, #6208, #49468, #34482, #9621, #25577, #2269, #18243 ),
 .UNSPECIFIED., .F., .F.,
 ( 4, 3, 3, 3, 3, 3, 4 ),
 ( 1.000000950999999910E-06, 0.01506370868781899824, 0.03155346947011499620, 0.06469334631533249502, 0.07088861345938199388, 0.1184795979030530133, 0.1410854872666899851 ),
 .UNSPECIFIED. ) ;
#6907 = FACE_OUTER_BOUND ( 'NONE', #32856, .T. ) ;
#6908 = ORIENTED_EDGE ( 'NONE', *, *, #47966, .T. ) ;
#6909 = VECTOR ( 'NONE', #13015, 1000.000000000000000 ) ;
#6910 = FACE_BOUND ( 'NONE', #43764, .T. ) ;
#6911 = CARTESIAN_POINT ( 'NONE',  ( 42.79442115924850754, 6.514747503090039693, -76.34753345981675920 ) ) ;
#6912 = CARTESIAN_POINT ( 'NONE',  ( 11.73992142287220197, 32.72645697550250077, -24.71095559905290173 ) ) ;
#6913 = EDGE_LOOP ( 'NONE', ( #13468, #38932, #41012, #1916 ) ) ;
#6914 = CARTESIAN_POINT ( 'NONE',  ( 24.33017316509850048, -16.51309434721139979, -37.82702577713659764 ) ) ;
#6915 = DIRECTION ( 'NONE',  ( -1.000000000000000000, 0.000000000000000000, 0.000000000000000000 ) ) ;
#6916 = CARTESIAN_POINT ( 'NONE',  ( 16.05893884862259924, 19.85742967422829608, -20.93640534643579798 ) ) ;
#6917 = CARTESIAN_POINT ( 'NONE',  ( 22.31602583494875702, -18.45493576387408652, -50.58969767961466601 ) ) ;
#6918 = CARTESIAN_POINT ( 'NONE',  ( 60.96203672470600310, -29.75511121401200043, -15.98584738528380278 ) ) ;
#6919 = CARTESIAN_POINT ( 'NONE',  ( 16.13393739769620083, -15.61618894467929941, -6.649999999999999467 ) ) ;
#6920 = CARTESIAN_POINT ( 'NONE',  ( 47.07006461603570102, -54.26997103497729569, -75.46887108633241326 ) ) ;
#6921 = CARTESIAN_POINT ( 'NONE',  ( 49.81260523996059675, 12.27001346555440087, -6.460395669183189860 ) ) ;
#6922 = EDGE_CURVE ( 'NONE', #46486, #29806, #17712, .T. ) ;
#6923 = DIRECTION ( 'NONE',  ( 1.000000000000000000, 0.000000000000000000, 0.000000000000000000 ) ) ;
#6924 = EDGE_CURVE ( 'NONE', #10836, #31099, #23368, .T. ) ;
#6925 = PRODUCT_DEFINITION_SHAPE ( 'NONE', 'NONE',  #21256 ) ;
#6926 = DIRECTION ( 'NONE',  ( 0.000000000000000000, 0.000000000000000000, 1.000000000000000000 ) ) ;
#6927 = EDGE_CURVE ( 'NONE', #17717, #18887, #22555, .T. ) ;
#6928 = CARTESIAN_POINT ( 'NONE',  ( 10.62413350085140173, -21.20446320448329658, -78.03525497637551211 ) ) ;
#6929 = ORIENTED_EDGE ( 'NONE', *, *, #10533, .F. ) ;
#6930 = CARTESIAN_POINT ( 'NONE',  ( 54.23650158716049674, -48.37337528119039831, -26.83965679272169780 ) ) ;
#6931 = CARTESIAN_POINT ( 'NONE',  ( 9.468372918422769402, -62.32709119060739766, -13.97902442704289960 ) ) ;
#6932 = CARTESIAN_POINT ( 'NONE',  ( 75.70026563160030264, -21.87202185586589565, -11.67482764317330002 ) ) ;
#6933 = CARTESIAN_POINT ( 'NONE',  ( 75.35176292259957620, 13.18942012435235078, -13.85075860070319287 ) ) ;
#6934 = CARTESIAN_POINT ( 'NONE',  ( -1.839728563314010135, -2.929686987007059873, -54.64999999999999858 ) ) ;
#6935 = AXIS2_PLACEMENT_3D ( 'NONE', #24259, #3612, #27945 ) ;
#6936 = DIRECTION ( 'NONE',  ( 0.000000000000000000, -1.000000000000000000, 0.000000000000000000 ) ) ;
#6937 = CIRCLE ( 'NONE', #46261, 2.999999999999999112 ) ;
#6938 = CARTESIAN_POINT ( 'NONE',  ( 8.222952931006085819, -16.65185013945336223, -38.75066497196897330 ) ) ;
#6939 = EDGE_CURVE ( 'NONE', #28860, #11300, #20871, .T. ) ;
#6940 = DIRECTION ( 'NONE',  ( 0.000000000000000000, -1.000000000000000000, 0.000000000000000000 ) ) ;
#6941 = LINE ( 'NONE', #29274, #15616 ) ;
#6942 = CARTESIAN_POINT ( 'NONE',  ( 42.30536707493200055, 11.93584660880990000, -3.349718967436809525 ) ) ;
#6943 = CARTESIAN_POINT ( 'NONE',  ( 24.04493320937934442, -15.61618918076996110, -53.79232900421944663 ) ) ;
#6944 = CARTESIAN_POINT ( 'NONE',  ( 65.36732126366399598, -45.11618894467940066, -12.60113342886489995 ) ) ;
#6945 = CARTESIAN_POINT ( 'NONE',  ( 19.53299984191638927, 24.23912880602019726, -75.56421462368636810 ) ) ;
#6946 = DIRECTION ( 'NONE',  ( 0.3863301728269249447, 0.9223605572461988089, -3.330669073875469621E-16 ) ) ;
#6947 = CARTESIAN_POINT ( 'NONE',  ( 76.69488533474444125, -43.19260729310870062, -14.37252596537610394 ) ) ;
#6948 = CARTESIAN_POINT ( 'NONE',  ( 17.63527260060340041, -51.92834279550939414, -75.76244777734170555 ) ) ;
#6950 = ADVANCED_FACE ( 'NONE', ( #50696 ), #39166, .F. ) ;
#6949 = CARTESIAN_POINT ( 'NONE',  ( 43.06099782924809460, -45.11618894467940066, -6.588391211254950086 ) ) ;
#6951 = CARTESIAN_POINT ( 'NONE',  ( 10.60517752403560010, -20.61013614081009848, -67.83350675970849863 ) ) ;
#6952 = CARTESIAN_POINT ( 'NONE',  ( 63.84815580435130045, 1.437400661353670062, -61.78179097966380340 ) ) ;
#6953 = ORIENTED_EDGE ( 'NONE', *, *, #30300, .F. ) ;
#6954 = CARTESIAN_POINT ( 'NONE',  ( 44.12711257345860361, 1.883811055320659955, -54.38706558040959749 ) ) ;
#6955 = DIRECTION ( 'NONE',  ( -0.2260571801428090388, -1.168509733417976470E-14, 0.9741140340359961680 ) ) ;
#6956 = CARTESIAN_POINT ( 'NONE',  ( 73.13235683752471061, 1.096291039689160085, -68.89363957891330870 ) ) ;
#6957 = CARTESIAN_POINT ( 'NONE',  ( 9.176796790077460741, -16.74902148356379783, -81.23899999999999011 ) ) ;
#6958 = CARTESIAN_POINT ( 'NONE',  ( 41.40015264295030306, -45.44364689039419858, -6.186196351018840467 ) ) ;
#6959 = ORIENTED_EDGE ( 'NONE', *, *, #2063, .T. ) ;
#6960 = ORIENTED_EDGE ( 'NONE', *, *, #43477, .T. ) ;
#6961 = VECTOR ( 'NONE', #3181, 1000.000000000000114 ) ;
#6962 = VERTEX_POINT ( 'NONE', #15574 ) ;
#6963 = LINE ( 'NONE', #7217, #21844 ) ;
#6964 = CARTESIAN_POINT ( 'NONE',  ( 23.39056959072010144, -13.30350361608390131, -81.23899999999999011 ) ) ;
#6965 = ADVANCED_FACE ( 'NONE', ( #22641 ), #34953, .T. ) ;
#6966 = ORIENTED_EDGE ( 'NONE', *, *, #14618, .F. ) ;
#6967 = CARTESIAN_POINT ( 'NONE',  ( -5.366062602303798279, -15.61618894467929586, -11.65000000000000036 ) ) ;
#6968 = ORIENTED_EDGE ( 'NONE', *, *, #9854, .T. ) ;
#6969 = FACE_OUTER_BOUND ( 'NONE', #50521, .T. ) ;
#6970 = CARTESIAN_POINT ( 'NONE',  ( 45.22176751739600320, -33.50786583678460318, -34.76635026929679384 ) ) ;
#6971 = AXIS2_PLACEMENT_3D ( 'NONE', #38850, #6356, #34629 ) ;
#6972 = VERTEX_POINT ( 'NONE', #38658 ) ;
#6973 = CARTESIAN_POINT ( 'NONE',  ( 41.61626771661330082, 6.328436186825659782, -82.23834840541459812 ) ) ;
#6975 = CARTESIAN_POINT ( 'NONE',  ( 53.64468172317890549, -51.26703106273480159, -75.63087525034551106 ) ) ;
#6974 = AXIS2_PLACEMENT_3D ( 'NONE', #11491, #44214, #23497 ) ;
#6976 = CARTESIAN_POINT ( 'NONE',  ( 60.53471020050410090, 14.39428645268190010, -47.24686264531659674 ) ) ;
#6977 = DIRECTION ( 'NONE',  ( -1.000000000000000000, 0.000000000000000000, 0.000000000000000000 ) ) ;
#6978 = CARTESIAN_POINT ( 'NONE',  ( 40.87221823369649343, -44.53072057087500468, -4.420649961794050675 ) ) ;
#6979 = DIRECTION ( 'NONE',  ( 0.000000000000000000, 0.000000000000000000, 1.000000000000000000 ) ) ;
#6980 = CARTESIAN_POINT ( 'NONE',  ( -6.895430101768229569, 14.71875163426810040, -5.354287734213469818 ) ) ;
#6981 = EDGE_CURVE ( 'NONE', #9856, #21614, #27609, .T. ) ;
#6982 = CARTESIAN_POINT ( 'NONE',  ( 64.91115770917960504, 1.389801772588459938, -70.26683326709820676 ) ) ;
#6983 = LINE ( 'NONE', #11688, #21374 ) ;
#6984 = CARTESIAN_POINT ( 'NONE',  ( 17.77818319944547909, -51.52597369355607526, -75.36997958382859508 ) ) ;
#6985 = EDGE_CURVE ( 'NONE', #51033, #26368, #51406, .T. ) ;
#6986 = CARTESIAN_POINT ( 'NONE',  ( 22.62628819889769716, -20.02483150870289919, -53.47738634665349622 ) ) ;
#6987 = VERTEX_POINT ( 'NONE', #6943 ) ;
#6988 = CARTESIAN_POINT ( 'NONE',  ( -1.365754458141149819, 11.26366790782569893, -20.15000000000000213 ) ) ;
#6989 = VECTOR ( 'NONE', #38955, 1000.000000000000000 ) ;
#6990 = CARTESIAN_POINT ( 'NONE',  ( 57.55751162087899786, 19.35892401864479950, -53.59933301304759823 ) ) ;
#6991 = CARTESIAN_POINT ( 'NONE',  ( 71.90108049458170569, 1.446932438105679841, -69.97684691838689730 ) ) ;
#6992 = CARTESIAN_POINT ( 'NONE',  ( 44.63094208885492975, -40.00404795335505526, -63.60229216252963624 ) ) ;
#6993 = CARTESIAN_POINT ( 'NONE',  ( 15.66736729374060211, 19.66432312694319862, -20.45701610577899743 ) ) ;
#6994 =( BOUNDED_CURVE ( )  B_SPLINE_CURVE ( 3, ( #51129, #7361, #39330, #3433 ),
 .UNSPECIFIED., .F., .T. ) 
 B_SPLINE_CURVE_WITH_KNOTS ( ( 4, 4 ),
 ( 0.000000000000000000, 0.5134355670272889860 ),
 .UNSPECIFIED. ) 
 CURVE ( )  GEOMETRIC_REPRESENTATION_ITEM ( )  RATIONAL_B_SPLINE_CURVE ( ( 1.000000000000000000, 0.9781523768112215800, 0.9781523768112215800, 1.000000000000000000 ) ) 
 REPRESENTATION_ITEM ( '' )  );
#6995 = B_SPLINE_CURVE_WITH_KNOTS ( 'NONE', 3,
 ( #12590, #44551, #8651, #40620, #17300, #6018, #34285, #45856, #9688, #9942, #50306, #9441, #34029, #45337, #25390, #45592, #25648, #26168, #21204, #30355, #49278, #13627, #21975, #30098, #6278, #10207, #33776, #42178, #29587, #41917, #41652, #17802, #37987 ),
 .UNSPECIFIED., .F., .F.,
 ( 4, 2, 2, 2, 1, 1, 1, 1, 1, 1, 1, 2, 2, 2, 2, 1, 1, 1, 1, 2, 2, 4 ),
 ( 0.000000000000000000, 0.2500000000003731460, 0.3750000000005595524, 0.4375000000006527001, 0.4687500000006993850, 0.4843750000007223111, 0.4921875000007341350, 0.4960937500007400192, 0.4980468750007425172, 0.4990234375007434053, 0.4995117187507441825, 0.4997558593757441270, 0.5000000000007440715, 0.6250000000005758727, 0.6875000000004914957, 0.7187500000004496403, 0.7343750000004286571, 0.7421875000004182210, 0.7460937500004128919, 0.7480468750004098943, 0.7500000000004067857, 1.000000000000000000 ),
 .UNSPECIFIED. ) ;
#6996 = CARTESIAN_POINT ( 'NONE',  ( 0.9655226856871633734, -38.79346329613591138, -84.65000000000000568 ) ) ;
#6997 = DIRECTION ( 'NONE',  ( -0.000000000000000000, -1.000000000000000000, -0.000000000000000000 ) ) ;
#6998 = CARTESIAN_POINT ( 'NONE',  ( 48.08635818190299460, -54.25091888102380011, -54.70531615945079551 ) ) ;
#6999 = CARTESIAN_POINT ( 'NONE',  ( -15.32468133715470238, -15.61618894467930296, -84.65000000000000568 ) ) ;
#7000 = CARTESIAN_POINT ( 'NONE',  ( 22.48345733077898245, -12.66161032470672332, -36.70821858127289516 ) ) ;
#7001 = CARTESIAN_POINT ( 'NONE',  ( 24.04485091158800003, -15.61618876680915236, -45.79233931912149558 ) ) ;
#7002 = CARTESIAN_POINT ( 'NONE',  ( 47.68999173674550462, 23.28182553471719984, -55.17369749140770097 ) ) ;
#7003 = ORIENTED_EDGE ( 'NONE', *, *, #18309, .T. ) ;
#7004 = CIRCLE ( 'NONE', #32894, 2.000000000000004441 ) ;
#7005 = CARTESIAN_POINT ( 'NONE',  ( 18.68994930968700174, -9.042806080414319325, -70.46522537534779929 ) ) ;
#7006 = AXIS2_PLACEMENT_3D ( 'NONE', #46745, #35438, #3220 ) ;
#7007 = ORIENTED_EDGE ( 'NONE', *, *, #22674, .T. ) ;
#7008 = CARTESIAN_POINT ( 'NONE',  ( 71.44150897753121399, 1.096153228089730147, -70.60852099187108877 ) ) ;
#7009 = CARTESIAN_POINT ( 'NONE',  ( 22.46012054408591752, -20.47784229346886065, -57.71600103834494178 ) ) ;
#7010 = CARTESIAN_POINT ( 'NONE',  ( 0.1457840918194806823, -20.72567761198500591, -34.68167776469320529 ) ) ;
#7011 = CARTESIAN_POINT ( 'NONE',  ( 13.13393739769619906, -49.61618894467939356, -34.64999999999999858 ) ) ;
#7013 = CARTESIAN_POINT ( 'NONE',  ( 44.50508471174445191, -33.13860886180549414, -47.72927995595490813 ) ) ;
#7012 = CARTESIAN_POINT ( 'NONE',  ( 38.67452568954060155, 4.883811055320659733, -81.65000000000000568 ) ) ;
#7014 = DIRECTION ( 'NONE',  ( 1.000000000000000000, -4.005157696510369650E-32, -3.556943099846429769E-14 ) ) ;
#7015 = CARTESIAN_POINT ( 'NONE',  ( 18.20470158624356927, -7.911112766937162810, -67.37566343967748139 ) ) ;
#7016 = DIRECTION ( 'NONE',  ( 0.6339889056055360017, 0.000000000000000000, -0.7733421413379041320 ) ) ;
#7017 = ORIENTED_EDGE ( 'NONE', *, *, #47470, .T. ) ;
#7018 = CARTESIAN_POINT ( 'NONE',  ( 16.13393739769620083, -15.61618894467929941, -32.14999999999999858 ) ) ;
#7019 = ORIENTED_EDGE ( 'NONE', *, *, #21105, .T. ) ;
#7020 = ORIENTED_EDGE ( 'NONE', *, *, #24991, .T. ) ;
#7021 = CARTESIAN_POINT ( 'NONE',  ( 12.36320305068320025, -64.54682834576858852, -15.76422791927960176 ) ) ;
#7022 = DIRECTION ( 'NONE',  ( 1.000000000000000000, 0.000000000000000000, 0.000000000000000000 ) ) ;
#7023 = CARTESIAN_POINT ( 'NONE',  ( 76.42505012355316296, -22.70526211292518326, -12.90445136872428655 ) ) ;
#7024 = CARTESIAN_POINT ( 'NONE',  ( 11.26003149166710138, -65.11465353321858629, -47.09181534538819847 ) ) ;
#7025 = ORIENTED_EDGE ( 'NONE', *, *, #24143, .F. ) ;
#7026 = EDGE_CURVE ( 'NONE', #21662, #32183, #49337, .T. ) ;
#7027 = VERTEX_POINT ( 'NONE', #43102 ) ;
#7028 = CARTESIAN_POINT ( 'NONE',  ( 24.04463300525956981, -15.61618495692933273, -55.50767188603018809 ) ) ;
#7029 = CARTESIAN_POINT ( 'NONE',  ( 56.79275862933049979, 14.79020353670410159, -26.24735317389830058 ) ) ;
#7030 = EDGE_CURVE ( 'NONE', #43570, #14404, #18620, .T. ) ;
#7031 = AXIS2_PLACEMENT_3D ( 'NONE', #3872, #39769, #7288 ) ;
#7032 = DIRECTION ( 'NONE',  ( 0.000000000000000000, -1.000000000000000000, 0.000000000000000000 ) ) ;
#7033 = CARTESIAN_POINT ( 'NONE',  ( 59.64872764346009859, -1.856411653216130109, -15.80443724322539900 ) ) ;
#7034 = EDGE_CURVE ( 'NONE', #18843, #24877, #35915, .T. ) ;
#7035 = DIRECTION ( 'NONE',  ( 0.000000000000000000, 0.000000000000000000, -1.000000000000000000 ) ) ;
#7036 = VERTEX_POINT ( 'NONE', #50953 ) ;
#7037 = FACE_OUTER_BOUND ( 'NONE', #31298, .T. ) ;
#7038 = CARTESIAN_POINT ( 'NONE',  ( 18.13393739769639978, 10.38381105532070059, -54.64999999999999858 ) ) ;
#7039 = CARTESIAN_POINT ( 'NONE',  ( 20.29261090969894354, -10.20487204212595245, -52.16115171938402995 ) ) ;
#7040 = CARTESIAN_POINT ( 'NONE',  ( 55.55365133010059964, -45.11618894467940066, -14.32025150907159983 ) ) ;
#7041 = CARTESIAN_POINT ( 'NONE',  ( 21.63365994436270157, -21.21438503817850219, -40.26531874956899770 ) ) ;
#7042 = CARTESIAN_POINT ( 'NONE',  ( 13.55383807960289921, -51.02647431419499924, -21.89020893026379611 ) ) ;
#7043 = CARTESIAN_POINT ( 'NONE',  ( 57.24950193371399365, 19.38381105532069881, -74.41700251245109143 ) ) ;
#7044 = DIRECTION ( 'NONE',  ( 0.000000000000000000, 0.000000000000000000, -1.000000000000000000 ) ) ;
#7045 = CARTESIAN_POINT ( 'NONE',  ( 57.13451053105050192, 13.89565872282230075, -17.02117289981309867 ) ) ;
#7046 = CARTESIAN_POINT ( 'NONE',  ( 61.00296193527120181, -45.42954057104920196, -47.27669373200819791 ) ) ;
#7047 = AXIS2_PLACEMENT_3D ( 'NONE', #4083, #48113, #8275 ) ;
#7048 = B_SPLINE_CURVE_WITH_KNOTS ( 'NONE', 3,
 ( #50975, #46549, #23425, #31292, #34716, #26858, #14818, #11413, #27375, #15598, #19517, #14557, #47067, #26590, #11668, #6703 ),
 .UNSPECIFIED., .F., .F.,
 ( 4, 2, 2, 2, 2, 2, 2, 4 ),
 ( -4.238728269404560045, -3.496950822258759750, -2.649205168377850139, -2.119364134702280023, -1.854443617864499849, -1.430570790924039937, -0.7523742678193099387, -8.881784197001252323E-16 ),
 .UNSPECIFIED. ) ;
#7049 = CARTESIAN_POINT ( 'NONE',  ( 56.62412426209190386, -50.71562078093869985, -53.71767670194419964 ) ) ;
#7050 = CARTESIAN_POINT ( 'NONE',  ( 23.01920207597069634, -14.08789267609899909, -38.77765294989999489 ) ) ;
#7051 = CARTESIAN_POINT ( 'NONE',  ( 47.02248099559329120, -39.42604202605379982, -54.03776557770559208 ) ) ;
#7052 = EDGE_CURVE ( 'NONE', #13860, #1516, #5820, .T. ) ;
#7053 = VERTEX_POINT ( 'NONE', #47300 ) ;
#7054 = CARTESIAN_POINT ( 'NONE',  ( 47.18716110640669825, 22.75249779235520009, -75.65750133416010215 ) ) ;
#7055 = CARTESIAN_POINT ( 'NONE',  ( 65.03937945068028625, 1.384708701328909886, -60.99162623037230446 ) ) ;
#7056 = CARTESIAN_POINT ( 'NONE',  ( 23.62216879347590037, 17.52774233096729617, -35.08633291502829366 ) ) ;
#7057 = CARTESIAN_POINT ( 'NONE',  ( 17.87990108355959862, 20.00716050925151990, -74.86151687916520814 ) ) ;
#7058 = CARTESIAN_POINT ( 'NONE',  ( 35.63393739769620083, -15.61618894467929941, -14.68999999999999950 ) ) ;
#7059 = CARTESIAN_POINT ( 'NONE',  ( 60.34784566561199881, 13.88381105532070059, -11.22422230768829898 ) ) ;
#7060 = CARTESIAN_POINT ( 'NONE',  ( 68.13393739769618662, -31.81618894467930403, -80.15000000000000568 ) ) ;
#7061 = CARTESIAN_POINT ( 'NONE',  ( 82.13853704237929776, 14.20578202076580077, -47.46441090728419709 ) ) ;
#7062 = AXIS2_PLACEMENT_3D ( 'NONE', #6585, #23061, #30412 ) ;
#7063 = CARTESIAN_POINT ( 'NONE',  ( 0.1368909795571799926, 19.95311627097120066, -35.13391829916529474 ) ) ;
#7065 = DIRECTION ( 'NONE',  ( -1.000000000000000000, 0.000000000000000000, 0.000000000000000000 ) ) ;
#7064 = CARTESIAN_POINT ( 'NONE',  ( 47.13393739769619373, 7.029298498933709283, -54.64999999999999858 ) ) ;
#7066 = CARTESIAN_POINT ( 'NONE',  ( 18.31867110002825427, -23.24857340604850364, -32.20353412124205761 ) ) ;
#7067 = DIRECTION ( 'NONE',  ( 0.000000000000000000, 1.000000000000000000, 0.000000000000000000 ) ) ;
#7068 = CARTESIAN_POINT ( 'NONE',  ( 49.44022876851060033, 22.43072660820480024, -54.54742833745199704 ) ) ;
#7069 = ORIENTED_EDGE ( 'NONE', *, *, #27435, .F. ) ;
#7070 = CARTESIAN_POINT ( 'NONE',  ( 53.42698669076009566, -49.38007291881159944, -49.00234524114569723 ) ) ;
#7071 = ORIENTED_EDGE ( 'NONE', *, *, #19648, .T. ) ;
#7072 = CARTESIAN_POINT ( 'NONE',  ( 43.22292296461858285, 6.401212194726233484, -74.17814224749000118 ) ) ;
#7073 = CARTESIAN_POINT ( 'NONE',  ( 16.46289132105319908, -8.571024043077699162, -40.36203157117240181 ) ) ;
#7074 = CARTESIAN_POINT ( 'NONE',  ( 13.69515105064549942, 20.07945732920870086, -22.67923001873320032 ) ) ;
#7075 = CARTESIAN_POINT ( 'NONE',  ( 51.67587649748560352, -48.61618894467930119, -77.01363636363639387 ) ) ;
#7076 = CARTESIAN_POINT ( 'NONE',  ( 9.338672804374079206, -13.72755509891449854, -53.53911138717720064 ) ) ;
#7077 = CARTESIAN_POINT ( 'NONE',  ( 53.52649861393759778, 18.16770936907249734, -49.17036649158689698 ) ) ;
#7078 = CARTESIAN_POINT ( 'NONE',  ( 56.11585462898960230, -45.54751570299690400, -17.03826781972080084 ) ) ;
#7079 = CARTESIAN_POINT ( 'NONE',  ( 16.13393739769620083, -45.61618894467940066, -62.64999999999999858 ) ) ;
#7080 = ORIENTED_EDGE ( 'NONE', *, *, #47600, .F. ) ;
#7081 = CIRCLE ( 'NONE', #19597, 25.10000000000000142 ) ;
#7082 = CARTESIAN_POINT ( 'NONE',  ( 15.03207885390800058, -7.846204650443991291, -38.74266516882029521 ) ) ;
#7083 = ORIENTED_EDGE ( 'NONE', *, *, #42880, .T. ) ;
#7085 = CARTESIAN_POINT ( 'NONE',  ( 72.74645547301390991, 1.390806392144110060, -68.86952544730040415 ) ) ;
#7084 = AXIS2_PLACEMENT_3D ( 'NONE', #4741, #8424, #16801 ) ;
#7086 = CARTESIAN_POINT ( 'NONE',  ( 9.643247817651371179, 32.68959971546669863, -46.55912598233139477 ) ) ;
#7087 = CARTESIAN_POINT ( 'NONE',  ( 72.88423911510749065, 1.325841671674429900, -62.37472934403619718 ) ) ;
#7088 = CARTESIAN_POINT ( 'NONE',  ( 52.88442569144270067, -50.11009285736640351, -50.03528398879910100 ) ) ;
#7089 = CARTESIAN_POINT ( 'NONE',  ( 52.59026075507055964, -49.83798095265304084, -48.57069100191421995 ) ) ;
#7090 = CARTESIAN_POINT ( 'NONE',  ( 10.90011346691389171, -20.34373019107950498, -67.61334385707304762 ) ) ;
#7091 = FACE_OUTER_BOUND ( 'NONE', #10951, .T. ) ;
#7092 = ORIENTED_EDGE ( 'NONE', *, *, #27565, .T. ) ;
#7093 = CARTESIAN_POINT ( 'NONE',  ( 61.28398356453099893, 14.37233669519349988, -47.68178229854910199 ) ) ;
#7094 = VERTEX_POINT ( 'NONE', #47043 ) ;
#7095 = CARTESIAN_POINT ( 'NONE',  ( 10.14913760601130122, -63.33847347462889843, -45.99399621147029649 ) ) ;
#7096 = EDGE_CURVE ( 'NONE', #41037, #10101, #11131, .T. ) ;
#7097 = CARTESIAN_POINT ( 'NONE',  ( 70.03247032090601465, 18.72622661238169783, -73.39853292320987066 ) ) ;
#7098 = EDGE_LOOP ( 'NONE', ( #36795, #43419, #32828, #33409 ) ) ;
#7099 = CARTESIAN_POINT ( 'NONE',  ( 11.23030387052107315, -64.15300031985499629, -44.07782004882023585 ) ) ;
#7100 = CARTESIAN_POINT ( 'NONE',  ( 57.13721803582939884, 19.38601056229089892, -53.74365126442869922 ) ) ;
#7101 = TOROIDAL_SURFACE ( 'NONE', #17114, 34.55616290057869833, 2.000000000000000000 ) ;
#7102 = EDGE_CURVE ( 'NONE', #32691, #19523, #43358, .T. ) ;
#7103 = CARTESIAN_POINT ( 'NONE',  ( 53.53698247381380781, 19.31898572816820092, -77.03764896304019771 ) ) ;
#7104 = ORIENTED_EDGE ( 'NONE', *, *, #47577, .F. ) ;
#7105 = CARTESIAN_POINT ( 'NONE',  ( 71.71126032029680175, -47.11618894467930119, -46.37203261889099792 ) ) ;
#7106 = FACE_OUTER_BOUND ( 'NONE', #8494, .T. ) ;
#7107 = DIRECTION ( 'NONE',  ( 0.000000000000000000, 0.000000000000000000, 1.000000000000000000 ) ) ;
#7108 = CARTESIAN_POINT ( 'NONE',  ( 17.68664282411100075, -32.20606442350149479, -34.65032322548079691 ) ) ;
#7109 = CARTESIAN_POINT ( 'NONE',  ( 14.17907360716779941, -7.606118556947649267, -59.21613716431379260 ) ) ;
#7110 = AXIS2_PLACEMENT_3D ( 'NONE', #2915, #22030, #43014 ) ;
#7111 = DIRECTION ( 'NONE',  ( 0.000000000000000000, -1.000000000000000000, 0.000000000000000000 ) ) ;
#7112 = CARTESIAN_POINT ( 'NONE',  ( 46.71367998675990663, -38.22377110652077192, -56.75123991735566165 ) ) ;
#7113 = EDGE_LOOP ( 'NONE', ( #10495, #7242, #44003, #22338, #10690, #19663, #10706 ) ) ;
#7114 = ORIENTED_EDGE ( 'NONE', *, *, #51717, .T. ) ;
#7115 = CARTESIAN_POINT ( 'NONE',  ( 20.62402991675640251, -21.56141921569700060, -52.52675917389010607 ) ) ;
#7116 = CARTESIAN_POINT ( 'NONE',  ( 53.24445252169859799, 13.88381105524720027, -12.91583287338970010 ) ) ;
#7117 = FACE_OUTER_BOUND ( 'NONE', #16500, .T. ) ;
#7118 = EDGE_CURVE ( 'NONE', #34659, #33336, #33288, .T. ) ;
#7119 = LINE ( 'NONE', #39090, #21645 ) ;
#7120 = VECTOR ( 'NONE', #14725, 1000.000000000000000 ) ;
#7121 = ADVANCED_FACE ( 'NONE', ( #23911 ), #26701, .T. ) ;
#7122 = CARTESIAN_POINT ( 'NONE',  ( 0.08551642312347559893, 14.63024707446910000, -34.70586877331279396 ) ) ;
#7123 = CARTESIAN_POINT ( 'NONE',  ( 9.976573729570530347, 22.56200410046550076, -34.67842804303189297 ) ) ;
#7124 = CARTESIAN_POINT ( 'NONE',  ( 12.13449217322260054, 33.70756578350810173, -16.24910028838000287 ) ) ;
#7125 = CARTESIAN_POINT ( 'NONE',  ( 22.72588359820849746, -10.66351633299509949, -61.30256663141189932 ) ) ;
#7126 = CARTESIAN_POINT ( 'NONE',  ( 52.69455864859469330, -49.72372575057979560, -27.57640321585610010 ) ) ;
#7127 = CARTESIAN_POINT ( 'NONE',  ( 53.93843392091529410, -50.96933828858919924, -75.87693567902510949 ) ) ;
#7129 = CARTESIAN_POINT ( 'NONE',  ( 19.54188346692635037, -9.703250399025609596, -60.11946100766459722 ) ) ;
#7128 = CARTESIAN_POINT ( 'NONE',  ( -3.436548605939819812, 18.89937065357259982, -7.972479206788761097 ) ) ;
#7130 = DIRECTION ( 'NONE',  ( -0.5720614028176840282, -0.4156269377774530760, 0.7071067811865479058 ) ) ;
#7131 = CARTESIAN_POINT ( 'NONE',  ( 16.13393739769620083, -15.61618894467929941, -46.39999999999999858 ) ) ;
#7132 = ORIENTED_EDGE ( 'NONE', *, *, #26058, .F. ) ;
#7133 = CARTESIAN_POINT ( 'NONE',  ( -5.673894891273640440, -46.74181062945210385, -4.529014137033779974 ) ) ;
#7134 = CARTESIAN_POINT ( 'NONE',  ( 47.54393415417700197, 23.34658024450819980, -54.99317590619320129 ) ) ;
#7135 = CARTESIAN_POINT ( 'NONE',  ( 51.13393739769659874, -50.61618894467899565, 17.35000000000000142 ) ) ;
#7136 = CARTESIAN_POINT ( 'NONE',  ( 63.23627918741579634, 0.9395704634982890990, -62.18392983749130565 ) ) ;
#7137 = CARTESIAN_POINT ( 'NONE',  ( 60.85471687133040319, 14.24866023781859958, -47.26085515436560058 ) ) ;
#7138 = CARTESIAN_POINT ( 'NONE',  ( 13.54377112832909980, -8.630651498136270305, -79.61963359764780535 ) ) ;
#7139 = CARTESIAN_POINT ( 'NONE',  ( 51.51980099933500412, 18.20712782104119754, -76.63338017729078899 ) ) ;
#7140 = CARTESIAN_POINT ( 'NONE',  ( 52.81767038776369816, 18.43487472115680248, -48.48655862607250100 ) ) ;
#7141 = FACE_OUTER_BOUND ( 'NONE', #18349, .T. ) ;
#7142 = CARTESIAN_POINT ( 'NONE',  ( 52.87019085405700025, -49.63973566670129856, -48.66536726492419263 ) ) ;
#7143 = CARTESIAN_POINT ( 'NONE',  ( 54.72133342176110204, 16.56637610245050141, -26.54825754140699701 ) ) ;
#7144 = VECTOR ( 'NONE', #19665, 1000.000000000000000 ) ;
#7145 = CARTESIAN_POINT ( 'NONE',  ( 50.12648257197400170, 22.24397334070440380, -55.01261709213260076 ) ) ;
#7146 = CARTESIAN_POINT ( 'NONE',  ( 9.299128317299539148, -63.29430534918720497, -46.53057822423220102 ) ) ;
#7147 = CARTESIAN_POINT ( 'NONE',  ( 52.88388581274700329, 18.44024018630440409, -49.00306432449180249 ) ) ;
#7148 = CARTESIAN_POINT ( 'NONE',  ( 63.72329982364428957, -31.81072269598050184, -17.26606606354560114 ) ) ;
#7149 = CARTESIAN_POINT ( 'NONE',  ( 71.39250861737149023, 1.096110717717199812, -60.66079369553730061 ) ) ;
#7150 = CARTESIAN_POINT ( 'NONE',  ( 11.13393739769619906, 32.28996932333459569, -43.76018303787720498 ) ) ;
#7151 = CARTESIAN_POINT ( 'NONE',  ( 72.38882998111121481, 1.407740700961940039, -61.66563034611200322 ) ) ;
#7152 = DIRECTION ( 'NONE',  ( -1.000000000000000000, -2.362305513541788125E-32, -1.430038757655089944E-15 ) ) ;
#7153 = AXIS2_PLACEMENT_3D ( 'NONE', #1750, #17736, #11175 ) ;
#7154 = CARTESIAN_POINT ( 'NONE',  ( 9.366921553120977961, -14.97355191961400500, -65.48305900605150498 ) ) ;
#7155 = ORIENTED_EDGE ( 'NONE', *, *, #16488, .T. ) ;
#7156 = EDGE_LOOP ( 'NONE', ( #1728, #36853, #574, #43247 ) ) ;
#7157 = CARTESIAN_POINT ( 'NONE',  ( 41.72053738002269796, 12.47914145849200018, -3.400228433360679592 ) ) ;
#7158 = EDGE_CURVE ( 'NONE', #30658, #5655, #45103, .T. ) ;
#7159 = AXIS2_PLACEMENT_3D ( 'NONE', #38901, #39153, #43346 ) ;
#7160 = CARTESIAN_POINT ( 'NONE',  ( 76.49475639570208330, -3.230431607988094811, -13.20482276423291879 ) ) ;
#7161 = ORIENTED_EDGE ( 'NONE', *, *, #28309, .T. ) ;
#7162 = CARTESIAN_POINT ( 'NONE',  ( 57.13573030296199562, -45.16451340659830294, -25.51734512155490364 ) ) ;
#7163 = CARTESIAN_POINT ( 'NONE',  ( 21.28925556178230494, -21.62091513535972709, -77.78184806566041232 ) ) ;
#7164 = ORIENTED_EDGE ( 'NONE', *, *, #12526, .F. ) ;
#7165 = CARTESIAN_POINT ( 'NONE',  ( 42.82578949616635100, 6.519398624929172215, -76.19070175595297201 ) ) ;
#7166 = CARTESIAN_POINT ( 'NONE',  ( 41.34377498613339696, -44.75585903957070144, -5.356936576703770214 ) ) ;
#7167 = ORIENTED_EDGE ( 'NONE', *, *, #9190, .T. ) ;
#7168 = CARTESIAN_POINT ( 'NONE',  ( 47.18077207768379822, -45.11618894467940066, -8.347044623099190375 ) ) ;
#7169 = CARTESIAN_POINT ( 'NONE',  ( 16.13393739769620083, -38.61618894467930119, -59.64999999999999147 ) ) ;
#7170 = CARTESIAN_POINT ( 'NONE',  ( 9.133937397696382021, -15.61618894467929763, -23.74958330439410048 ) ) ;
#7171 = CARTESIAN_POINT ( 'NONE',  ( 61.08036406955709907, -29.31821407486409825, -15.93372933320830143 ) ) ;
#7172 = DIRECTION ( 'NONE',  ( 1.000000000000000000, 0.000000000000000000, 0.000000000000000000 ) ) ;
#7173 = CARTESIAN_POINT ( 'NONE',  ( 46.63190898996919742, -53.39441561763939603, -76.07596939981860373 ) ) ;
#7174 = CARTESIAN_POINT ( 'NONE',  ( 22.90093738118858013, -16.50198597715758808, -36.49448425584234457 ) ) ;
#7175 = CIRCLE ( 'NONE', #44014, 10.00000000000000711 ) ;
#7176 = EDGE_CURVE ( 'NONE', #22439, #1287, #42692, .T. ) ;
#7177 = FACE_OUTER_BOUND ( 'NONE', #4042, .T. ) ;
#7178 = CARTESIAN_POINT ( 'NONE',  ( 83.94975121583560451, -44.29606033358990658, -46.94103493214879563 ) ) ;
#7179 = CARTESIAN_POINT ( 'NONE',  ( 61.50012592447659898, 13.88381109315920092, -27.25296643813030073 ) ) ;
#7180 = CARTESIAN_POINT ( 'NONE',  ( 8.445554253283772184, -12.63784234794610128, -32.62531358638169365 ) ) ;
#7181 = B_SPLINE_SURFACE_WITH_KNOTS ( 'NONE', 3, 3, ( 
 ( #13466, #29927, #22067, #6111, #25479, #41226, #10299, #2173, #33865 ),
 ( #29421, #2422, #38076, #14480, #6365, #25221, #49876, #29673, #49625 ),
 ( #30451, #41483, #5340, #45944, #21293, #1395, #18152, #18406, #10034 ),
 ( #26000, #34382, #45426, #34118, #9530, #5597, #46214, #50129, #21552 ),
 ( #37297, #38333, #22327, #13971, #41742, #17384, #14225, #33349, #49366 ),
 ( #30197, #37548, #1653, #1913, #17645, #50394, #33611, #13719, #45682 ),
 ( #9784, #25735, #37820, #5848, #21813, #25575, #33447, #33703, #49467 ),
 ( #5692, #4640, #49209, #13558, #41581, #29520, #36605, #45524, #710 ),
 ( #17735, #21392, #29765, #21643, #24534, #33189, #45004, #13053, #37143 ),
 ( #4908, #20616, #45264, #45784, #16701, #5438, #49720, #9376, #9106 ),
 ( #13808, #8847, #9620, #44743, #24798, #37650, #1498, #20882, #29007 ),
 ( #41323, #25055, #40808, #40552, #1749, #32655, #48685, #12786, #36877 ),
 ( #28744, #32923, #976, #16977, #48952, #41072, #5184, #21137, #1240 ),
 ( #17228, #25320, #13301, #37396, #29262, #17483, #42102, #41843, #46307 ),
 ( #14837, #2268, #5946, #33954, #50738, #30799, #31059, #46567, #50997 ),
 ( #46049, #18761, #9873, #10136, #14577, #6466, #6207, #30543, #34481 ),
 ( #2008, #34734, #18507, #25828, #21904, #38173, #6725, #15098, #10916 ),
 ( #34211, #10655, #14319, #26613, #30291, #22423, #22161, #37915, #10396 ),
 ( #46828, #18242, #17990, #49972, #26878, #42889, #14064, #42627, #30024 ),
 ( #26097, #6982, #50232, #26351, #22681, #38427, #42363, #38700, #50487 ) ),
 .UNSPECIFIED., .F., .F., .F.,
 ( 4, 2, 2, 2, 2, 2, 2, 2, 2, 4 ),
 ( 4, 1, 1, 1, 1, 1, 4 ),
 ( -1.826162956740689847, -1.664693056096139934, -1.413098168491170092, -1.141351847962929877, -0.9130814783703469217, -0.7989462935740540006, -0.6163299978999839945, -0.3676482854780290244, -0.1181677997689200010, 0.000000000000000000 ),
 ( 0.000000000000000000, 0.1666666666666670182, 0.3333333333333329818, 0.5000000000000000000, 0.6666666666666670737, 0.8333333333333330373, 1.000000000000000000 ),
 .UNSPECIFIED. ) ;
#7182 = VERTEX_POINT ( 'NONE', #351 ) ;
#7183 = CARTESIAN_POINT ( 'NONE',  ( 52.83769228248530681, -49.65410697577470245, -28.03887768922920287 ) ) ;
#7184 = CARTESIAN_POINT ( 'NONE',  ( 6.339668291764630759, -58.73921203693550552, -11.09392847882710065 ) ) ;
#7185 = CARTESIAN_POINT ( 'NONE',  ( 75.18881547038029112, 0.6024962871804371289, -12.00534390646789973 ) ) ;
#7186 = CARTESIAN_POINT ( 'NONE',  ( 75.41655381601106001, 12.84207971899083489, -13.62414596433559311 ) ) ;
#7187 = CARTESIAN_POINT ( 'NONE',  ( 19.71407736822502699, -55.45560309152967449, -75.36448431255345781 ) ) ;
#7188 = FACE_OUTER_BOUND ( 'NONE', #22276, .T. ) ;
#7189 = CARTESIAN_POINT ( 'NONE',  ( 17.16953927579633898, -23.52718117654557872, -38.25066653675266792 ) ) ;
#7190 = TOROIDAL_SURFACE ( 'NONE', #5510, 17.19098300429530113, 0.5000000000822009127 ) ;
#7191 = CARTESIAN_POINT ( 'NONE',  ( 63.01386660552499563, 0.9960089569207349891, -62.53811752243721145 ) ) ;
#7192 = CARTESIAN_POINT ( 'NONE',  ( 57.43388575162559562, -50.22061705833820611, -52.72793123370430379 ) ) ;
#7193 = CARTESIAN_POINT ( 'NONE',  ( 40.68015366847210146, 13.39283706869419888, -4.085852594949460403 ) ) ;
#7194 = DIRECTION ( 'NONE',  ( -0.8732394366197193669, -0.4872913772396092469, 0.000000000000000000 ) ) ;
#7195 = CARTESIAN_POINT ( 'NONE',  ( 63.43778145654710698, 0.9561296872662310431, -61.91446069548659636 ) ) ;
#7196 = CARTESIAN_POINT ( 'NONE',  ( 57.46792114364419746, -47.23085594836910417, -47.80306618055729473 ) ) ;
#7197 = VECTOR ( 'NONE', #43292, 1000.000000000000227 ) ;
#7198 = DIRECTION ( 'NONE',  ( 0.04100182651872441575, 0.05643417272666774454, -0.9975640502598241977 ) ) ;
#7199 = CARTESIAN_POINT ( 'NONE',  ( 66.69979047892330470, -1.463808326225739975, -17.02723538977290119 ) ) ;
#7200 = CARTESIAN_POINT ( 'NONE',  ( 18.34505658028029984, -52.20693806470120535, -75.61048537065330777 ) ) ;
#7201 = CARTESIAN_POINT ( 'NONE',  ( 8.826359436922910362, -14.16498300286340140, -62.12974372312799431 ) ) ;
#7202 = CARTESIAN_POINT ( 'NONE',  ( 63.27515794601240628, 0.9525601718079100833, -62.12948614655890367 ) ) ;
#7203 = EDGE_LOOP ( 'NONE', ( #7626, #45723, #48387, #45109, #1397 ) ) ;
#7204 = CARTESIAN_POINT ( 'NONE',  ( 10.81033552764298555, -63.45699809194467633, -23.82639812994678863 ) ) ;
#7205 = CYLINDRICAL_SURFACE ( 'NONE', #39296, 0.4999999999999994449 ) ;
#7206 = CARTESIAN_POINT ( 'NONE',  ( 73.04943094402750603, 1.269319268680890067, -68.77895457036579785 ) ) ;
#7207 = PLANE ( 'NONE',  #37416 ) ;
#7208 = CIRCLE ( 'NONE', #24745, 2.999999999999998224 ) ;
#7209 = CARTESIAN_POINT ( 'NONE',  ( 9.006752130201981288, -14.38476595312559958, -81.23899999999999011 ) ) ;
#7210 = CARTESIAN_POINT ( 'NONE',  ( 40.80913783761709368, -45.21803053746209855, -5.659197024988120717 ) ) ;
#7211 = EDGE_LOOP ( 'NONE', ( #43647, #21885, #40840, #12238, #8232 ) ) ;
#7212 = CARTESIAN_POINT ( 'NONE',  ( 17.68279279595209985, 20.56214955651219967, -75.65676662446099954 ) ) ;
#7213 = CIRCLE ( 'NONE', #29808, 0.4906046190927097483 ) ;
#7214 = ORIENTED_EDGE ( 'NONE', *, *, #35453, .F. ) ;
#7215 = EDGE_CURVE ( 'NONE', #40924, #43673, #35743, .T. ) ;
#7216 = EDGE_LOOP ( 'NONE', ( #45237, #41810, #8607, #2793 ) ) ;
#7217 = CARTESIAN_POINT ( 'NONE',  ( -0.2444979013989767025, -31.15369398163246473, 4.943674098299959851 ) ) ;
#7218 = CARTESIAN_POINT ( 'NONE',  ( 23.37200753273739906, -13.22834593274319914, -81.23899999999999011 ) ) ;
#7219 = EDGE_CURVE ( 'NONE', #43577, #11677, #35089, .T. ) ;
#7220 = LINE ( 'NONE', #51248, #38556 ) ;
#7221 = EDGE_CURVE ( 'NONE', #11267, #16071, #32809, .T. ) ;
#7222 = VERTEX_POINT ( 'NONE', #16861 ) ;
#7223 = ADVANCED_FACE ( 'NONE', ( #12159 ), #8481, .T. ) ;
#7224 = CARTESIAN_POINT ( 'NONE',  ( 9.807767002083743080, -10.75451754946909944, -52.71600246173886717 ) ) ;
#7225 = ORIENTED_EDGE ( 'NONE', *, *, #48943, .T. ) ;
#7226 = DIRECTION ( 'NONE',  ( 0.000000000000000000, -1.000000000000000000, 0.000000000000000000 ) ) ;
#7227 =( GEOMETRIC_REPRESENTATION_CONTEXT ( 3 ) GLOBAL_UNCERTAINTY_ASSIGNED_CONTEXT ( ( #4394 ) ) GLOBAL_UNIT_ASSIGNED_CONTEXT ( ( #23715, #32088, #47856 ) ) REPRESENTATION_CONTEXT ( 'NONE', 'WORKASPACE' ) );
#7228 = CYLINDRICAL_SURFACE ( 'NONE', #32629, 0.4999999999999982236 ) ;
#7229 = ORIENTED_EDGE ( 'NONE', *, *, #39535, .F. ) ;
#7230 = CARTESIAN_POINT ( 'NONE',  ( 13.39998208309999939, 20.55440457967890211, -74.14999999999999147 ) ) ;
#7231 = CARTESIAN_POINT ( 'NONE',  ( 51.04849420485089695, -50.89596744187040400, -76.15025768116009885 ) ) ;
#7232 = CARTESIAN_POINT ( 'NONE',  ( 60.70121379090529956, 14.34289773273770052, -47.37813858017759827 ) ) ;
#7233 = AXIS2_PLACEMENT_3D ( 'NONE', #17868, #29902, #46450 ) ;
#7234 = VECTOR ( 'NONE', #46665, 1000.000000000000000 ) ;
#7235 = DIRECTION ( 'NONE',  ( 0.5547001962252301466, -1.445602896647336944E-16, 0.8320502943378429439 ) ) ;
#7236 = EDGE_CURVE ( 'NONE', #6837, #51855, #29326, .T. ) ;
#7237 = CARTESIAN_POINT ( 'NONE',  ( 42.29536634146689522, -43.17774985521609921, -3.241362036132330093 ) ) ;
#7238 = CARTESIAN_POINT ( 'NONE',  ( -3.853615750487999758, 16.96449338327530043, -5.240522787413070205 ) ) ;
#7239 = CARTESIAN_POINT ( 'NONE',  ( 46.91750639651494481, 22.97282010492738280, -75.61476957852809733 ) ) ;
#7240 = DIRECTION ( 'NONE',  ( 0.000000000000000000, -4.336808689941963009E-16, 1.000000000000000000 ) ) ;
#7241 = CARTESIAN_POINT ( 'NONE',  ( 8.298661659914731814, -16.05800598386570144, -54.26957565728969257 ) ) ;
#7242 = ORIENTED_EDGE ( 'NONE', *, *, #41390, .T. ) ;
#7243 = CIRCLE ( 'NONE', #44913, 2.000000000000002665 ) ;
#7244 = CYLINDRICAL_SURFACE ( 'NONE', #8757, 6.766999999999998572 ) ;
#7245 = CARTESIAN_POINT ( 'NONE',  ( 57.46598710300569479, 19.38381105532060289, -53.87378585246109708 ) ) ;
#7246 = CARTESIAN_POINT ( 'NONE',  ( 72.05097492716728880, 1.266076987106930174, -70.10514767873740993 ) ) ;
#7247 = CARTESIAN_POINT ( 'NONE',  ( 44.40914995519487007, -39.98739809836357040, -64.67686260219700500 ) ) ;
#7248 = CARTESIAN_POINT ( 'NONE',  ( 14.17150143965160147, 19.18236913456970072, -20.90975112687780069 ) ) ;
#7249 = EDGE_CURVE ( 'NONE', #12485, #22335, #11690, .T. ) ;
#7250 = CARTESIAN_POINT ( 'NONE',  ( 16.13393739769620083, -15.61618894467929941, -28.45282021618999835 ) ) ;
#7251 = CYLINDRICAL_SURFACE ( 'NONE', #37219, 11.00000000000000000 ) ;
#7252 = CARTESIAN_POINT ( 'NONE',  ( 48.49909158994660174, -54.16138566422429790, -55.13510240093949477 ) ) ;
#7253 = CARTESIAN_POINT ( 'NONE',  ( 24.04525281611314824, -15.61618915252426376, -57.50766930885080086 ) ) ;
#7254 = VECTOR ( 'NONE', #29720, 999.9999999999998863 ) ;
#7255 = DIRECTION ( 'NONE',  ( 0.000000000000000000, 0.000000000000000000, 1.000000000000000000 ) ) ;
#7256 = CARTESIAN_POINT ( 'NONE',  ( 8.222926147295824606, -14.58072384180595549, -70.83399561464088379 ) ) ;
#7257 = ORIENTED_EDGE ( 'NONE', *, *, #14417, .F. ) ;
#7258 = CARTESIAN_POINT ( 'NONE',  ( 20.74347699498930098, -9.763083867941830363, -36.77968578276969680 ) ) ;
#7259 = ORIENTED_EDGE ( 'NONE', *, *, #20618, .F. ) ;
#7260 = CARTESIAN_POINT ( 'NONE',  ( 71.37118938927949330, 1.325715844996850024, -70.41854262496009653 ) ) ;
#7261 = CARTESIAN_POINT ( 'NONE',  ( 20.99565119372854483, -21.94232563707941353, -57.79933445449422891 ) ) ;
#7262 = AXIS2_PLACEMENT_3D ( 'NONE', #40049, #47919, #40306 ) ;
#7263 = CARTESIAN_POINT ( 'NONE',  ( 0.2589946642435042579, -20.70800519868845413, -34.65038329361674130 ) ) ;
#7264 = LINE ( 'NONE', #43423, #47853 ) ;
#7265 = CYLINDRICAL_SURFACE ( 'NONE', #13940, 6.766999999999998572 ) ;
#7266 = CARTESIAN_POINT ( 'NONE',  ( -0.007164427059776000244, -10.48291004383190028, -34.77269723891829756 ) ) ;
#7267 = CARTESIAN_POINT ( 'NONE',  ( 12.14991857309165368, -8.703602074731387361, -67.12566404048868662 ) ) ;
#7268 = CARTESIAN_POINT ( 'NONE',  ( -5.866062602303799167, -15.61618894467929586, -14.65000000000000036 ) ) ;
#7269 = ORIENTED_EDGE ( 'NONE', *, *, #9567, .F. ) ;
#7270 = CARTESIAN_POINT ( 'NONE',  ( 84.44784216359251161, -43.11618894467930119, -47.47585302082339354 ) ) ;
#7271 = VERTEX_POINT ( 'NONE', #37291 ) ;
#7272 = ORIENTED_EDGE ( 'NONE', *, *, #51064, .F. ) ;
#7273 = DIRECTION ( 'NONE',  ( 0.000000000000000000, 0.000000000000000000, 1.000000000000000000 ) ) ;
#7274 = CARTESIAN_POINT ( 'NONE',  ( 56.50022374573209305, 14.94172953599193754, -26.24581867127661639 ) ) ;
#7275 = CARTESIAN_POINT ( 'NONE',  ( 8.222937397696199469, -15.61618894467929941, -32.14999999999999858 ) ) ;
#7276 = CARTESIAN_POINT ( 'NONE',  ( 10.49965938277759925, -64.70776751887689215, -46.82084276604349071 ) ) ;
#7277 = AXIS2_PLACEMENT_3D ( 'NONE', #1339, #28843, #3797 ) ;
#7278 = ORIENTED_EDGE ( 'NONE', *, *, #33166, .F. ) ;
#7279 = B_SPLINE_CURVE_WITH_KNOTS ( 'NONE', 3,
 ( #30517, #34450, #13527, #5661, #49941, #17702, #9587, #42071, #9843, #29990 ),
 .UNSPECIFIED., .F., .F.,
 ( 4, 1, 1, 1, 1, 1, 1, 4 ),
 ( 0.4999968673859223056, 0.5271528655503062710, 0.6063717966138713056, 0.6855907276774317882, 0.7648096587411550296, 0.8440285898047201751, 0.9232475208684389756, 1.000000000000000000 ),
 .UNSPECIFIED. ) ;
#7280 = ORIENTED_EDGE ( 'NONE', *, *, #44073, .T. ) ;
#7281 = EDGE_CURVE ( 'NONE', #8293, #16490, #21030, .T. ) ;
#7282 = CARTESIAN_POINT ( 'NONE',  ( 24.04489399084747703, -15.64449660401445996, -55.50881072821707818 ) ) ;
#7283 = CARTESIAN_POINT ( 'NONE',  ( 50.95182575631829991, -50.95090194773979420, -76.14999999999999147 ) ) ;
#7284 = CARTESIAN_POINT ( 'NONE',  ( 56.36079422399649985, -50.55996778040380235, -52.89779376298050551 ) ) ;
#7285 = CARTESIAN_POINT ( 'NONE',  ( 10.81595853043058675, -11.36155942741024560, -45.66747770548867891 ) ) ;
#7286 = CARTESIAN_POINT ( 'NONE',  ( 64.11742790134928782, 0.5060918581745209588, -17.20042942902649941 ) ) ;
#7287 = CARTESIAN_POINT ( 'NONE',  ( 51.94902347081840333, -49.52373935748639866, -77.02691575752830033 ) ) ;
#7288 = DIRECTION ( 'NONE',  ( 1.000000000000000000, 0.000000000000000000, 0.000000000000000000 ) ) ;
#7289 = ORIENTED_EDGE ( 'NONE', *, *, #50569, .T. ) ;
#7290 = CARTESIAN_POINT ( 'NONE',  ( 63.93393739769614825, 11.38381105532090309, -62.44999999999986784 ) ) ;
#7291 = CARTESIAN_POINT ( 'NONE',  ( 20.48068097650709873, -21.17032068915356646, -51.13580619584276832 ) ) ;
#7292 = FACE_OUTER_BOUND ( 'NONE', #30113, .T. ) ;
#7293 = CARTESIAN_POINT ( 'NONE',  ( 14.06332963686348059, -23.32130743969031172, -54.09100309838140674 ) ) ;
#7294 = CARTESIAN_POINT ( 'NONE',  ( 8.617266676947521020, -17.87149576802320183, -46.91970895891299165 ) ) ;
#7295 = CARTESIAN_POINT ( 'NONE',  ( 13.04440776331039942, -50.02432106228609854, -21.04429563615369858 ) ) ;
#7296 = ADVANCED_FACE ( 'NONE', ( #17639 ), #6104, .T. ) ;
#7297 = LINE ( 'NONE', #47144, #43524 ) ;
#7298 = CARTESIAN_POINT ( 'NONE',  ( 56.32680328304889628, 14.04817129808600029, -16.42293331861320027 ) ) ;
#7299 = CARTESIAN_POINT ( 'NONE',  ( 60.99063479934959275, -45.64856812161170296, -47.70729053994229929 ) ) ;
#7300 =( BOUNDED_CURVE ( )  B_SPLINE_CURVE ( 3, ( #48154, #4386, #20612, #19599 ),
 .UNSPECIFIED., .F., .T. ) 
 B_SPLINE_CURVE_WITH_KNOTS ( ( 4, 4 ),
 ( 1.125870930210365994, 1.195525503939052436 ),
 .UNSPECIFIED. ) 
 CURVE ( )  GEOMETRIC_REPRESENTATION_ITEM ( )  RATIONAL_B_SPLINE_CURVE ( ( 1.000000000000000000, 0.9995957275622157079, 0.9995957275622157079, 1.000000000000000000 ) ) 
 REPRESENTATION_ITEM ( '' )  );
#7301 = CARTESIAN_POINT ( 'NONE',  ( 56.55337564821359564, -50.50557100886170048, -52.91477395665069849 ) ) ;
#7302 = CARTESIAN_POINT ( 'NONE',  ( 9.942021269482310686, -12.23939551960640060, -44.00610240009889651 ) ) ;
#7303 = CARTESIAN_POINT ( 'NONE',  ( 22.72480813554982149, -13.84492922675662463, -44.36947208136891163 ) ) ;
#7304 = EDGE_LOOP ( 'NONE', ( #43256, #25738, #37367, #18652, #5348 ) ) ;
#7305 = CARTESIAN_POINT ( 'NONE',  ( 46.52565835080890366, 21.89345249355760004, -76.13734531346200640 ) ) ;
#7306 = CARTESIAN_POINT ( 'NONE',  ( 64.79014552703418417, 0.9971903505820729485, -60.67679930835159752 ) ) ;
#7307 = B_SPLINE_CURVE_WITH_KNOTS ( 'NONE', 3,
 ( #49839, #29889, #33828, #1360, #45908, #13680 ),
 .UNSPECIFIED., .F., .F.,
 ( 4, 2, 4 ),
 ( 0.01784182840660334182, 0.02050618711215480144, 0.03595209231937170069 ),
 .UNSPECIFIED. ) ;
#7308 = CARTESIAN_POINT ( 'NONE',  ( 0.1457840807894888180, 19.59951024407514097, -34.68167773519660813 ) ) ;
#7309 = CARTESIAN_POINT ( 'NONE',  ( 55.25526344926753808, -47.47676247021213669, -26.53762684301318231 ) ) ;
#7310 = CARTESIAN_POINT ( 'NONE',  ( 9.555189432054399745, -11.06668960550747727, -54.70064004558554416 ) ) ;
#7311 = CONICAL_SURFACE ( 'NONE', #48305, 19.50000000000000000, 0.2449786631268651149 ) ;
#7312 = ADVANCED_FACE ( 'NONE', ( #5074 ), #45154, .F. ) ;
#7313 = CARTESIAN_POINT ( 'NONE',  ( 47.26413010207565435, -54.05555214137573472, -75.56727778750388325 ) ) ;
#7315 = EDGE_CURVE ( 'NONE', #10362, #29849, #21684, .T. ) ;
#7314 = CARTESIAN_POINT ( 'NONE',  ( 82.74207635200149014, 14.32739582876689965, -47.63391066194130019 ) ) ;
#7316 = DIRECTION ( 'NONE',  ( 0.000000000000000000, 0.000000000000000000, -1.000000000000000000 ) ) ;
#7318 = CARTESIAN_POINT ( 'NONE',  ( 11.41017075758820809, 33.30599513501292819, -24.00668485612997216 ) ) ;
#7317 = LINE ( 'NONE', #39283, #11406 ) ;
#7319 = CARTESIAN_POINT ( 'NONE',  ( 68.13393739769620083, 0.8838110553206759423, -65.65000000000000568 ) ) ;
#7320 = CARTESIAN_POINT ( 'NONE',  ( 49.25538189185729721, 22.42010655522559759, -54.36832621985269753 ) ) ;
#7321 = ADVANCED_FACE ( 'NONE', ( #29154 ), #41792, .F. ) ;
#7322 = ORIENTED_EDGE ( 'NONE', *, *, #42556, .T. ) ;
#7323 = CARTESIAN_POINT ( 'NONE',  ( 52.59812909015290217, -49.82798299618050208, -48.49246230761499277 ) ) ;
#7324 = EDGE_LOOP ( 'NONE', ( #40284, #3652, #41899, #2712, #33735 ) ) ;
#7325 = CARTESIAN_POINT ( 'NONE',  ( 47.10325001712173076, 6.750336882473666478, -54.73793454088935562 ) ) ;
#7326 = CARTESIAN_POINT ( 'NONE',  ( -14.01196063605392439, -54.14290045843446109, 10.84999999999999964 ) ) ;
#7327 = CARTESIAN_POINT ( 'NONE',  ( 13.63913721475599949, 20.12796159149439745, -22.70105333191040131 ) ) ;
#7328 = CARTESIAN_POINT ( 'NONE',  ( 12.73487912048826232, 24.23912916116268690, -75.56421958049274679 ) ) ;
#7329 = CARTESIAN_POINT ( 'NONE',  ( 9.677450050134419612, -18.45455640281440068, -51.32098131739589775 ) ) ;
#7330 = CARTESIAN_POINT ( 'NONE',  ( 52.71454275216699870, 18.51637985033769951, -48.77935984480249942 ) ) ;
#7331 = CARTESIAN_POINT ( 'NONE',  ( 22.20691379552689426, -12.48290680228687322, -80.69525706773917761 ) ) ;
#7332 = FACE_OUTER_BOUND ( 'NONE', #47437, .T. ) ;
#7333 = ORIENTED_EDGE ( 'NONE', *, *, #9370, .T. ) ;
#7334 = CARTESIAN_POINT ( 'NONE',  ( 23.37872820719320188, -17.35397704167489863, -81.14228717839650074 ) ) ;
#7335 = ORIENTED_EDGE ( 'NONE', *, *, #46144, .F. ) ;
#7336 = CARTESIAN_POINT ( 'NONE',  ( 11.37397765035290043, -65.29604510817189578, -17.68262795671300225 ) ) ;
#7337 = CYLINDRICAL_SURFACE ( 'NONE', #25325, 0.4999999999999982236 ) ;
#7338 = CARTESIAN_POINT ( 'NONE',  ( 72.91105647262868672, 1.325839985408290067, -62.43087585298830078 ) ) ;
#7339 = EDGE_CURVE ( 'NONE', #41355, #33328, #1624, .T. ) ;
#7340 = CARTESIAN_POINT ( 'NONE',  ( 24.04493741668374440, -16.65174122825144920, -39.83400417788456593 ) ) ;
#7341 = CARTESIAN_POINT ( 'NONE',  ( 53.59003930803689997, -49.40628012469949937, -49.22510501142529904 ) ) ;
#7342 = DIRECTION ( 'NONE',  ( 0.3294064756441054120, -0.9441882088883177815, 9.436895709313929201E-16 ) ) ;
#7343 = VERTEX_POINT ( 'NONE', #33076 ) ;
#7344 = EDGE_CURVE ( 'NONE', #26468, #49915, #30891, .T. ) ;
#7345 = CARTESIAN_POINT ( 'NONE',  ( 44.09915591415798275, -33.11626185954118284, -54.64999999999999858 ) ) ;
#7346 = CARTESIAN_POINT ( 'NONE',  ( 9.726666662871039648, -63.11543068638779630, -46.30264950036470140 ) ) ;
#7347 = CARTESIAN_POINT ( 'NONE',  ( 68.13393739769630031, 16.88381105531719939, -74.20000000000000284 ) ) ;
#7348 = ORIENTED_EDGE ( 'NONE', *, *, #20746, .F. ) ;
#7349 = CARTESIAN_POINT ( 'NONE',  ( 23.62216879347609932, -48.76012022032579551, -35.08633291502829366 ) ) ;
#7350 = CARTESIAN_POINT ( 'NONE',  ( 10.09028208944064353, -10.43082494342464450, -76.73325434315464122 ) ) ;
#7351 = DIRECTION ( 'NONE',  ( 1.000000000000000000, 0.000000000000000000, 0.000000000000000000 ) ) ;
#7352 = ORIENTED_EDGE ( 'NONE', *, *, #21820, .T. ) ;
#7353 = CARTESIAN_POINT ( 'NONE',  ( 46.25525774125583922, -33.99486860111965569, -54.56299356781535437 ) ) ;
#7354 = CARTESIAN_POINT ( 'NONE',  ( 52.32303876295807754, 20.18503163261358679, -75.90202713928304945 ) ) ;
#7355 = PLANE ( 'NONE',  #9265 ) ;
#7356 = VECTOR ( 'NONE', #51251, 1000.000000000000000 ) ;
#7357 = DIRECTION ( 'NONE',  ( 0.000000000000000000, 0.000000000000000000, 1.000000000000000000 ) ) ;
#7358 = CARTESIAN_POINT ( 'NONE',  ( 22.16775957127159913, -9.996962126548099903, -65.55365164940339184 ) ) ;
#7359 = CARTESIAN_POINT ( 'NONE',  ( 52.75108815572690446, -49.73378124990440341, -48.86094483346149531 ) ) ;
#7360 = DIRECTION ( 'NONE',  ( 0.000000000000000000, -1.000000000000000000, 0.000000000000000000 ) ) ;
#7361 = CARTESIAN_POINT ( 'NONE',  ( 61.28610861176740343, -45.23040055550220018, -46.54508491471730025 ) ) ;
#7362 = AXIS2_PLACEMENT_3D ( 'NONE', #23404, #3261, #16079 ) ;
#7363 = ORIENTED_EDGE ( 'NONE', *, *, #13127, .T. ) ;
#7364 = ORIENTED_EDGE ( 'NONE', *, *, #48986, .F. ) ;
#7365 = SPHERICAL_SURFACE ( 'NONE', #12507, 2.000000000000000000 ) ;
#7366 = CARTESIAN_POINT ( 'NONE',  ( 20.14552668288030191, -9.338144248108390499, -57.91364648621609490 ) ) ;
#7367 = CARTESIAN_POINT ( 'NONE',  ( 53.59007319633400357, -49.40623578145169859, -49.22505640094960455 ) ) ;
#7368 = CARTESIAN_POINT ( 'NONE',  ( 50.31596467094429670, -49.96707859667039742, -76.14999999999999147 ) ) ;
#7369 = CARTESIAN_POINT ( 'NONE',  ( 10.11873436104249890, -20.36210433234809969, -32.14999999999999858 ) ) ;
#7370 = CARTESIAN_POINT ( 'NONE',  ( 46.38946308792309736, 21.75434083481459879, -76.14871748201410639 ) ) ;
#7371 = DIRECTION ( 'NONE',  ( 0.000000000000000000, 0.000000000000000000, -1.000000000000000000 ) ) ;
#7372 = B_SPLINE_CURVE_WITH_KNOTS ( 'NONE', 3,
 ( #6611, #38591, #45934, #46203, #10023, #42000, #22055, #39106, #26507, #26766, #35150, #26251, #2938, #30440, #18142, #34107, #38322, #2411, #14214, #18393, #34371, #50384, #43549, #47233, #23336, #3715 ),
 .UNSPECIFIED., .F., .F.,
 ( 4, 2, 2, 2, 2, 2, 2, 2, 2, 2, 2, 2, 4 ),
 ( 0.5000000130881896432, 0.5625000114521658823, 0.6250000098161422324, 0.6875000081801185825, 0.7500000065440948216, 0.7812500057260829411, 0.8125000049080710607, 0.8437500040900592913, 0.8750000032720474108, 0.9062500024540355303, 0.9375000016360237609, 0.9687500008180118805, 1.000000000000000000 ),
 .UNSPECIFIED. ) ;
#7373 = CARTESIAN_POINT ( 'NONE',  ( 12.17975455548389974, 33.45308329381320078, -15.92303081429079903 ) ) ;
#7374 = CARTESIAN_POINT ( 'NONE',  ( 19.86463262639870209, -22.96905463225390065, -69.85821118628290094 ) ) ;
#7375 = CARTESIAN_POINT ( 'NONE',  ( 21.17364772268240003, -21.52724977567429931, -32.14999999999999858 ) ) ;
#7376 = ADVANCED_FACE ( 'NONE', ( #17377 ), #29416, .T. ) ;
#7377 = CARTESIAN_POINT ( 'NONE',  ( 57.01978172671810086, -50.62831244894230309, -74.38112120481839895 ) ) ;
#7379 = CARTESIAN_POINT ( 'NONE',  ( 31.38963856960426568, -35.88105874546273100, -84.64183929351709423 ) ) ;
#7378 = CARTESIAN_POINT ( 'NONE',  ( -9.451250797512591006, 12.57291231543609911, -6.018481141893100350 ) ) ;
#7380 = CARTESIAN_POINT ( 'NONE',  ( 1.027904703268279984, -42.68661147989060112, -20.15000000000000213 ) ) ;
#7381 = CARTESIAN_POINT ( 'NONE',  ( 22.37318698975080267, 22.37488585622680048, -34.64999999999999858 ) ) ;
#7382 = CARTESIAN_POINT ( 'NONE',  ( -6.866062602303790285, -15.61618894467929941, 4.943674098299959851 ) ) ;
#7383 = ADVANCED_FACE ( 'NONE', ( #30192 ), #24456, .T. ) ;
#7384 = EDGE_LOOP ( 'NONE', ( #175, #37628, #45756, #11939, #182, #24992 ) ) ;
#7385 = CARTESIAN_POINT ( 'NONE',  ( 15.82102960914879830, -7.675182713834671766, -80.99522283173863002 ) ) ;
#7386 = CARTESIAN_POINT ( 'NONE',  ( 47.60612636963649891, 23.31708596581999871, -55.05355304419519769 ) ) ;
#7387 = PRESENTATION_LAYER_ASSIGNMENT (  '', '', ( #39190 ) ) ;
#7388 = CARTESIAN_POINT ( 'NONE',  ( 59.11255455559349770, -45.23257961995879839, -26.22557274275510153 ) ) ;
#7389 = CARTESIAN_POINT ( 'NONE',  ( 36.93393739769619799, -15.61618894467929941, -11.54999999999999893 ) ) ;
#7390 = CARTESIAN_POINT ( 'NONE',  ( 60.94773661516500596, 14.19689157201089991, -47.19004457261220153 ) ) ;
#7391 = CARTESIAN_POINT ( 'NONE',  ( 21.28336590497879754, -10.23194527880280091, -75.97556276872150249 ) ) ;
#7392 = CARTESIAN_POINT ( 'NONE',  ( 51.55656746335520779, 18.27266258789200037, -76.63870291393729417 ) ) ;
#7393 = CARTESIAN_POINT ( 'NONE',  ( 53.10940561484209610, 18.28271463908539829, -48.84491345906369730 ) ) ;
#7394 = CARTESIAN_POINT ( 'NONE',  ( 8.222948648952634443, -16.65181879039660018, -70.75066497221537531 ) ) ;
#7395 = CARTESIAN_POINT ( 'NONE',  ( 52.94585587482559674, -49.60009264233129755, -48.75076953771959865 ) ) ;
#7396 = B_SPLINE_CURVE_WITH_KNOTS ( 'NONE', 3,
 ( #1859, #17838, #30394, #49822, #22270, #46417, #13914, #29870, #10504, #45891, #9977, #41956, #38280, #10244, #34324, #50339, #22530, #16418 ),
 .UNSPECIFIED., .F., .F.,
 ( 4, 2, 2, 2, 2, 2, 2, 2, 4 ),
 ( 0.000000000000000000, 0.06249998230893073076, 0.1249999646178614615, 0.1874999469267921992, 0.2499999292357229230, 0.3124999115446535636, 0.3749998938535841764, 0.4374998761625147892, 0.4999998584714454020 ),
 .UNSPECIFIED. ) ;
#7397 = CARTESIAN_POINT ( 'NONE',  ( 51.49137293625199874, 21.54576438608010136, -53.98331227670009724 ) ) ;
#7398 = CARTESIAN_POINT ( 'NONE',  ( 15.09829607975676957, -23.52717697970637190, -62.04932902358816449 ) ) ;
#7399 = CARTESIAN_POINT ( 'NONE',  ( -22.60067283610179700, -11.07416626356550005, -54.64998264227110525 ) ) ;
#7400 = DIRECTION ( 'NONE',  ( 0.000000000000000000, 1.000000000000000000, 0.000000000000000000 ) ) ;
#7401 = CARTESIAN_POINT ( 'NONE',  ( 59.22067766047359783, -28.67256876376159980, -15.68016428579549881 ) ) ;
#7402 = CARTESIAN_POINT ( 'NONE',  ( 71.28940315555229290, 0.9947083095259759977, -60.55634004142090276 ) ) ;
#7403 = DIRECTION ( 'NONE',  ( 0.000000000000000000, 0.000000000000000000, 1.000000000000000000 ) ) ;
#7404 = CARTESIAN_POINT ( 'NONE',  ( 72.32632772932539922, 1.200157260841289819, -61.39419087681179832 ) ) ;
#7405 = CARTESIAN_POINT ( 'NONE',  ( 51.58134242171076522, -34.14973535910032609, -76.88488821125437767 ) ) ;
#7406 = ADVANCED_FACE ( 'NONE', ( #15451 ), #32556, .F. ) ;
#7407 = CARTESIAN_POINT ( 'NONE',  ( 11.03453497164934838, -11.13167925635793942, -65.68238587149497221 ) ) ;
#7408 = ORIENTED_EDGE ( 'NONE', *, *, #12361, .T. ) ;
#7409 = ORIENTED_EDGE ( 'NONE', *, *, #22875, .T. ) ;
#7410 = CARTESIAN_POINT ( 'NONE',  ( 9.366458663215507130, -15.75911442933090889, -37.84046178158559570 ) ) ;
#7411 = EDGE_CURVE ( 'NONE', #24770, #40057, #3304, .T. ) ;
#7412 = DIRECTION ( 'NONE',  ( 0.000000000000000000, -1.000000000000000000, 0.000000000000000000 ) ) ;
#7413 = EDGE_LOOP ( 'NONE', ( #11139, #49693 ) ) ;
#7414 = CARTESIAN_POINT ( 'NONE',  ( 57.33727144475490434, -45.20148317274580307, -25.72981098958030088 ) ) ;
#7415 = CARTESIAN_POINT ( 'NONE',  ( 0.8044204053651899944, -8.725579796100580765, -34.68801049095939959 ) ) ;
#7416 = CARTESIAN_POINT ( 'NONE',  ( 0.03808610503982447909, -4.264599916538029944, -34.73334895013598356 ) ) ;
#7417 = VERTEX_POINT ( 'NONE', #35870 ) ;
#7418 = DIRECTION ( 'NONE',  ( 0.000000000000000000, -1.000000000000000000, 0.000000000000000000 ) ) ;
#7419 = CARTESIAN_POINT ( 'NONE',  ( 42.69833145473944569, 6.500458167497354722, -76.82796414980892052 ) ) ;
#7420 = CARTESIAN_POINT ( 'NONE',  ( 12.54247866899070019, 34.25618301002470645, -23.07435593645569938 ) ) ;
#7421 = EDGE_LOOP ( 'NONE', ( #12381, #37190, #18931, #798, #37275 ) ) ;
#7422 = CARTESIAN_POINT ( 'NONE',  ( 18.64322687137160273, -7.762133735154519876, -33.39076563757389948 ) ) ;
#7423 = DIRECTION ( 'NONE',  ( -6.580805000000000321E-18, -4.248364000000000300E-18, 1.000000000000000000 ) ) ;
#7424 = CARTESIAN_POINT ( 'NONE',  ( 21.98228690486360648, -21.02318771973998324, -50.02964728310828235 ) ) ;
#7425 = CARTESIAN_POINT ( 'NONE',  ( 64.68287081661640059, -30.48142292270370035, -16.53828615335140029 ) ) ;
#7426 = CARTESIAN_POINT ( 'NONE',  ( 22.04685551236088870, -12.20820984684314681, -64.28615539813523583 ) ) ;
#7427 = CARTESIAN_POINT ( 'NONE',  ( 46.35275103504449845, -52.90993241930539881, -76.14999999999999147 ) ) ;
#7428 = CARTESIAN_POINT ( 'NONE',  ( 23.84448207147010024, -14.15528223125809859, -71.95289117501670262 ) ) ;
#7429 = CARTESIAN_POINT ( 'NONE',  ( -1.143840380081599717, -17.22304274993012285, -35.76111111111112706 ) ) ;
#7430 = VECTOR ( 'NONE', #27644, 1000.000000000000000 ) ;
#7431 = CARTESIAN_POINT ( 'NONE',  ( 41.48254013806749896, 13.91499593496540044, -5.927804853516350114 ) ) ;
#7432 = AXIS2_PLACEMENT_3D ( 'NONE', #32758, #36707, #12890 ) ;
#7433 = AXIS2_PLACEMENT_3D ( 'NONE', #16862, #4802, #41738 ) ;
#7434 = CARTESIAN_POINT ( 'NONE',  ( 87.04559528857579664, 18.79802461769378397, -61.26127762739950811 ) ) ;
#7435 = CARTESIAN_POINT ( 'NONE',  ( 84.24534987432259925, -43.83635652924289872, -47.12743895163409746 ) ) ;
#7436 = DIRECTION ( 'NONE',  ( 0.000000000000000000, 0.000000000000000000, -1.000000000000000000 ) ) ;
#7437 = CARTESIAN_POINT ( 'NONE',  ( 21.98967281619519909, -9.811619623081579533, -33.25906503489069621 ) ) ;
#7438 = ORIENTED_EDGE ( 'NONE', *, *, #27312, .T. ) ;
#7439 = DIRECTION ( 'NONE',  ( 0.3294064756441278941, 0.9441882088883097879, 0.000000000000000000 ) ) ;
#7440 = ADVANCED_FACE ( 'NONE', ( #11525 ), #779, .T. ) ;
#7441 = CARTESIAN_POINT ( 'NONE',  ( 9.945332009489360914, -62.12608445570190696, -13.67195039459510042 ) ) ;
#7442 = CARTESIAN_POINT ( 'NONE',  ( 75.68634210793200623, -12.48868729177629966, -11.61082697430510002 ) ) ;
#7443 = CARTESIAN_POINT ( 'NONE',  ( 18.06932202639800167, 24.33696219936669891, -76.14999999999999147 ) ) ;
#7444 = DIRECTION ( 'NONE',  ( 0.6415444970810866288, 0.4854844151940982400, 0.5939070136550167467 ) ) ;
#7445 = CARTESIAN_POINT ( 'NONE',  ( 48.93887227096879400, -45.11618894467940066, -44.18916148508130703 ) ) ;
#7446 = CARTESIAN_POINT ( 'NONE',  ( 23.04647088892617646, -19.60030115133175599, -37.95900078287649393 ) ) ;
#7447 = CARTESIAN_POINT ( 'NONE',  ( 15.24823161472325772, -22.38320011598096926, -48.99448779884927774 ) ) ;
#7448 = CARTESIAN_POINT ( 'NONE',  ( 63.00666467042349694, 0.9212109678634080590, -62.53374032209040223 ) ) ;
#7449 = CARTESIAN_POINT ( 'NONE',  ( 57.35498654301330390, -50.32030778642509716, -52.86924993879389945 ) ) ;
#7450 = CARTESIAN_POINT ( 'NONE',  ( 42.15277068879080247, 12.54031964892660156, -4.489091469251048849 ) ) ;
#7451 = CARTESIAN_POINT ( 'NONE',  ( 22.90112932213407149, -15.61618880384378905, -64.45281843961751633 ) ) ;
#7452 = CARTESIAN_POINT ( 'NONE',  ( 63.30304092011339634, 0.9208623934744530892, -62.09132346512820533 ) ) ;
#7453 = CARTESIAN_POINT ( 'NONE',  ( 55.49599478882970516, -48.26400341526499460, -48.16694294531140486 ) ) ;
#7454 = CYLINDRICAL_SURFACE ( 'NONE', #21435, 2.999999999999999112 ) ;
#7455 = CARTESIAN_POINT ( 'NONE',  ( 104.6856170952509757, -28.80002732851738045, -102.2016796975550079 ) ) ;
#7456 = CARTESIAN_POINT ( 'NONE',  ( 17.69922415165360263, -51.74824662968959643, -75.61048537065330777 ) ) ;
#7457 = CARTESIAN_POINT ( 'NONE',  ( 63.44426004651669615, -45.11618894467940066, -11.74199176319659976 ) ) ;
#7458 = CARTESIAN_POINT ( 'NONE',  ( 9.344596190075201037, -18.68401232695549652, -65.93225241418160465 ) ) ;
#7459 = CARTESIAN_POINT ( 'NONE',  ( 15.54400253304468116, 19.58458200056557530, -20.39351677730839185 ) ) ;
#7460 = DIRECTION ( 'NONE',  ( 1.000000000000000000, 0.000000000000000000, 0.000000000000000000 ) ) ;
#7461 = ORIENTED_EDGE ( 'NONE', *, *, #3081, .T. ) ;
#7462 = CARTESIAN_POINT ( 'NONE',  ( 45.31003520305578292, 14.31855968887177255, -8.676032565373851924 ) ) ;
#7463 = CARTESIAN_POINT ( 'NONE',  ( 21.43037387198247856, -19.89010587847297984, -34.66902735005525216 ) ) ;
#7464 = CARTESIAN_POINT ( 'NONE',  ( 73.14800808192789816, 0.9948723650351710690, -68.93161800279381168 ) ) ;
#7465 = AXIS2_PLACEMENT_3D ( 'NONE', #11944, #35523, #15613 ) ;
#7466 = CARTESIAN_POINT ( 'NONE',  ( 45.73288634929132002, 8.845650597630955403, -58.25629762057298677 ) ) ;
#7467 = VECTOR ( 'NONE', #21244, 1000.000000000000000 ) ;
#7468 = CARTESIAN_POINT ( 'NONE',  ( 11.84380770541370076, -9.249706252957370367, -81.23899999999999011 ) ) ;
#7469 = ORIENTED_EDGE ( 'NONE', *, *, #40241, .F. ) ;
#7470 = EDGE_CURVE ( 'NONE', #8281, #23002, #7591, .T. ) ;
#7471 = CARTESIAN_POINT ( 'NONE',  ( 17.21347160910339724, 21.88381105532300097, -76.14999999999999147 ) ) ;
#7472 = EDGE_LOOP ( 'NONE', ( #13797, #2302, #36712, #33579 ) ) ;
#7473 = CONICAL_SURFACE ( 'NONE', #42635, 0.7349999999999987654, 0.06981317007977388966 ) ;
#7474 = EDGE_CURVE ( 'NONE', #51185, #12580, #4673, .T. ) ;
#7475 = ORIENTED_EDGE ( 'NONE', *, *, #49913, .T. ) ;
#7476 = FACE_OUTER_BOUND ( 'NONE', #48592, .T. ) ;
#7477 = CARTESIAN_POINT ( 'NONE',  ( 23.01036527161310019, -12.13836321956489783, -81.23899999999999011 ) ) ;
#7478 = CARTESIAN_POINT ( 'NONE',  ( 61.73062563639849998, 13.90432078297569873, -46.66292371669469929 ) ) ;
#7479 = VERTEX_POINT ( 'NONE', #20646 ) ;
#7480 = CARTESIAN_POINT ( 'NONE',  ( 23.04646052128485323, -11.63205733350218551, -53.34100437166649300 ) ) ;
#7481 = ORIENTED_EDGE ( 'NONE', *, *, #46636, .F. ) ;
#7482 = CARTESIAN_POINT ( 'NONE',  ( 41.13393739769620083, -15.61618894467929941, 4.450000000000000178 ) ) ;
#7483 = CARTESIAN_POINT ( 'NONE',  ( 56.16732778801245018, 19.38381105532069881, -76.24890161727635984 ) ) ;
#7484 = ORIENTED_EDGE ( 'NONE', *, *, #14510, .T. ) ;
#7485 = CARTESIAN_POINT ( 'NONE',  ( 72.80030139158668590, 1.384887413063060180, -62.68544474927200127 ) ) ;
#7486 = CARTESIAN_POINT ( 'NONE',  ( 53.09964378157899745, -51.41544001692909660, -75.69941956541140371 ) ) ;
#7487 = CARTESIAN_POINT ( 'NONE',  ( 60.91162229252049798, 14.31804145399359918, -47.50905935143390479 ) ) ;
#7488 = CARTESIAN_POINT ( 'NONE',  ( 22.88339355091036964, -15.11907872941729991, -40.42942904639821222 ) ) ;
#7489 = CARTESIAN_POINT ( 'NONE',  ( 42.62644315484929791, -42.85940974227979439, -3.197525305375130245 ) ) ;
#7490 = CARTESIAN_POINT ( 'NONE',  ( -6.454950692847609695, 15.20115021654400067, -5.551883511487449852 ) ) ;
#7491 = CIRCLE ( 'NONE', #33435, 0.4999999999096970127 ) ;
#7492 = CIRCLE ( 'NONE', #14192, 38.00000000000000000 ) ;
#7493 = CARTESIAN_POINT ( 'NONE',  ( -0.1295185695942999982, 0.6472670226113349523, -59.64999999999999147 ) ) ;
#7494 = LINE ( 'NONE', #18762, #41478 ) ;
#7495 = CIRCLE ( 'NONE', #30933, 34.47562460986249988 ) ;
#7496 = AXIS2_PLACEMENT_3D ( 'NONE', #24518, #13037, #693 ) ;
#7497 = CARTESIAN_POINT ( 'NONE',  ( 15.08639525488320032, -7.838695541132539191, -54.74488924367149423 ) ) ;
#7498 = ORIENTED_EDGE ( 'NONE', *, *, #22640, .T. ) ;
#7499 = DIRECTION ( 'NONE',  ( 0.000000000000000000, 0.000000000000000000, -1.000000000000000000 ) ) ;
#7500 = ADVANCED_FACE ( 'NONE', ( #44772 ), #2478, .F. ) ;
#7501 = CARTESIAN_POINT ( 'NONE',  ( 44.20345041334109482, 14.84825193712300084, -8.431702830100249457 ) ) ;
#7502 = CARTESIAN_POINT ( 'NONE',  ( 71.78321337075939823, 1.149538111076449987, -70.36367628376740413 ) ) ;
#7503 = CARTESIAN_POINT ( 'NONE',  ( 45.27541171706066336, -40.04939379810706157, -60.47585066460795389 ) ) ;
#7504 = EDGE_CURVE ( 'NONE', #47622, #19762, #802, .T. ) ;
#7505 = CARTESIAN_POINT ( 'NONE',  ( 14.79307399754019947, 19.45299727194570139, -20.88395191203290224 ) ) ;
#7506 = ADVANCED_FACE ( 'NONE', ( #29791 ), #25601, .T. ) ;
#7507 = PRESENTATION_STYLE_ASSIGNMENT (( #3578 ) ) ;
#7508 = CARTESIAN_POINT ( 'NONE',  ( 12.76110939629680097, 18.75367528263859995, -21.08964675879520101 ) ) ;
#7509 = EDGE_CURVE ( 'NONE', #39070, #6528, #16625, .T. ) ;
#7510 = DIRECTION ( 'NONE',  ( -0.06889765579810419593, -0.01091231665325485128, -0.9975640502598241977 ) ) ;
#7511 = CARTESIAN_POINT ( 'NONE',  ( 48.78510665982869909, -53.94511784475069760, -54.68190458609500126 ) ) ;
#7512 = CARTESIAN_POINT ( 'NONE',  ( -33.14629235451243972, -25.37746373560590740, -57.60079496986296732 ) ) ;
#7513 = CARTESIAN_POINT ( 'NONE',  ( 51.13393739769620083, 19.38381105532069881, 16.85000000000000142 ) ) ;
#7514 = CARTESIAN_POINT ( 'NONE',  ( 17.16955493387669307, -23.52717894132403842, -37.96600343497949126 ) ) ;
#7515 = CARTESIAN_POINT ( 'NONE',  ( 47.81335647231740182, 23.16511464034180179, -54.71582838609170096 ) ) ;
#7516 = VERTEX_POINT ( 'NONE', #13331 ) ;
#7517 = CARTESIAN_POINT ( 'NONE',  ( 8.698584540071550464, -16.08759346412580271, -38.04718867978759533 ) ) ;
#7518 = DIRECTION ( 'NONE',  ( 0.000000000000000000, 0.000000000000000000, -1.000000000000000000 ) ) ;
#7519 = VERTEX_POINT ( 'NONE', #21164 ) ;
#7520 = CARTESIAN_POINT ( 'NONE',  ( 71.56253747416570832, 1.100585178972000033, -70.52983742103249654 ) ) ;
#7521 = CARTESIAN_POINT ( 'NONE',  ( 60.27360767123050067, -45.79670854958099824, -47.49318409392839868 ) ) ;
#7522 = CARTESIAN_POINT ( 'NONE',  ( 59.41577471975829638, -46.21032088470760613, -47.36236646002819839 ) ) ;
#7523 = CARTESIAN_POINT ( 'NONE',  ( 83.45566975104344465, 13.44200870639070722, -46.48562894763595921 ) ) ;
#7525 = DIRECTION ( 'NONE',  ( 0.000000000000000000, 0.000000000000000000, -1.000000000000000000 ) ) ;
#7524 = CARTESIAN_POINT ( 'NONE',  ( 84.25371145582080601, 12.95080643885139970, -47.43624648648039965 ) ) ;
#7526 = CARTESIAN_POINT ( 'NONE',  ( 59.52869175205803032, 14.25746298374641441, -26.73578769780420572 ) ) ;
#7527 = CARTESIAN_POINT ( 'NONE',  ( 16.13393739769620083, -15.61618894467929941, -28.45282021618999835 ) ) ;
#7528 = VERTEX_POINT ( 'NONE', #17760 ) ;
#7529 = CARTESIAN_POINT ( 'NONE',  ( 0.08375394646315241498, 19.63944928676770019, -34.70982966457259522 ) ) ;
#7530 = ORIENTED_EDGE ( 'NONE', *, *, #2016, .F. ) ;
#7531 = EDGE_CURVE ( 'NONE', #31864, #50665, #23400, .T. ) ;
#7532 = ORIENTED_EDGE ( 'NONE', *, *, #24931, .F. ) ;
#7533 = CARTESIAN_POINT ( 'NONE',  ( 9.921778078347148977, -18.94533778500921173, -59.69054780769135249 ) ) ;
#7534 = CIRCLE ( 'NONE', #27599, 4.649999999999999467 ) ;
#7535 = CARTESIAN_POINT ( 'NONE',  ( 16.13393739769620083, -15.61618894467929941, -44.64999999999999858 ) ) ;
#7536 = CIRCLE ( 'NONE', #40180, 0.5000000000000004441 ) ;
#7537 = CARTESIAN_POINT ( 'NONE',  ( 76.47144082675787047, -26.50245961684229101, -13.10435250752327718 ) ) ;
#7538 = CARTESIAN_POINT ( 'NONE',  ( 11.29861653319979986, -65.19153529705319272, -47.24805190295079882 ) ) ;
#7539 = ORIENTED_EDGE ( 'NONE', *, *, #28960, .T. ) ;
#7540 = VECTOR ( 'NONE', #30516, 1000.000000000000000 ) ;
#7541 = ORIENTED_EDGE ( 'NONE', *, *, #29086, .F. ) ;
#7542 = CARTESIAN_POINT ( 'NONE',  ( 22.46008086064721354, -20.47789713743962281, -55.71595987601556743 ) ) ;
#7543 = CARTESIAN_POINT ( 'NONE',  ( -20.42916145723442867, -2.043494675895988877, -52.78588572598070527 ) ) ;
#7544 = CARTESIAN_POINT ( 'NONE',  ( 56.38980056118450079, -50.68245470039340006, -53.17791771570339421 ) ) ;
#7545 = CARTESIAN_POINT ( 'NONE',  ( 22.90091625179776358, -15.59788028122024350, -46.45196706549376842 ) ) ;
#7546 = CARTESIAN_POINT ( 'NONE',  ( 65.26361326256220252, 0.1311058356091460153, -16.98102554325449987 ) ) ;
#7547 = CARTESIAN_POINT ( 'NONE',  ( 51.70989473440189954, -48.92491810616539993, -77.02394377353789423 ) ) ;
#7548 = DIRECTION ( 'NONE',  ( 0.2201775510703259942, -0.9741807197500960136, 0.04993767387313000072 ) ) ;
#7549 = ORIENTED_EDGE ( 'NONE', *, *, #19285, .T. ) ;
#7550 = CARTESIAN_POINT ( 'NONE',  ( 63.13746035244330557, 0.8910129994591539093, -68.97194292341539779 ) ) ;
#7551 = CARTESIAN_POINT ( 'NONE',  ( 12.14992424677891947, -22.52877902415496081, -48.45899884107838318 ) ) ;
#7552 = CARTESIAN_POINT ( 'NONE',  ( 22.72481315194836782, -13.84495412362821831, -52.36948451444106212 ) ) ;
#7553 = CARTESIAN_POINT ( 'NONE',  ( 16.13393739769620083, -15.61618894467929941, -20.15000000000000213 ) ) ;
#7554 = EDGE_CURVE ( 'NONE', #26020, #50974, #8876, .T. ) ;
#7555 = CARTESIAN_POINT ( 'NONE',  ( 23.05439743991649948, -19.31672679688609762, -58.16879716994689886 ) ) ;
#7556 = CARTESIAN_POINT ( 'NONE',  ( 57.18064182625810332, 19.38381105532069881, -74.68520933546099627 ) ) ;
#7557 = DIRECTION ( 'NONE',  ( 0.8732394366197157032, 0.4872913772396159082, 0.000000000000000000 ) ) ;
#7558 = CARTESIAN_POINT ( 'NONE',  ( 56.73667420260279926, 14.03196537716829972, -17.93020592428829829 ) ) ;
#7559 = CARTESIAN_POINT ( 'NONE',  ( 60.98488730395339985, -45.38821883831149506, -46.95029822698879940 ) ) ;
#7560 = CARTESIAN_POINT ( 'NONE',  ( 14.36274735259626567, -22.20707703622060336, -39.03615485351005532 ) ) ;
#7561 = CARTESIAN_POINT ( 'NONE',  ( 13.41159479355990136, -22.12244823248479975, -57.47332068091419188 ) ) ;
#7562 = DIRECTION ( 'NONE',  ( 0.000000000000000000, 0.000000000000000000, -1.000000000000000000 ) ) ;
#7563 = ORIENTED_EDGE ( 'NONE', *, *, #34363, .T. ) ;
#7564 = CARTESIAN_POINT ( 'NONE',  ( 46.35275103504439898, 21.67755452994670406, -76.14999999999999147 ) ) ;
#7565 = CARTESIAN_POINT ( 'NONE',  ( 65.11747358718548639, 1.386342629514219826, -61.00047607903670155 ) ) ;
#7566 = AXIS2_PLACEMENT_3D ( 'NONE', #34725, #35516, #31559 ) ;
#7567 = CARTESIAN_POINT ( 'NONE',  ( 41.89773878495709880, -45.76711833347420111, -6.740064978679530583 ) ) ;
#7568 = ADVANCED_FACE ( 'NONE', ( #36905 ), #32952, .F. ) ;
#7569 = CARTESIAN_POINT ( 'NONE',  ( 17.92370450339628007, 19.88381105532280202, -74.33587756533624713 ) ) ;
#7570 = ADVANCED_FACE ( 'NONE', ( #45812 ), #20362, .F. ) ;
#7571 = DIRECTION ( 'NONE',  ( -0.3863301728269232238, -0.9223605572461994750, 0.000000000000000000 ) ) ;
#7572 = CIRCLE ( 'NONE', #51075, 5.499999999999998224 ) ;
#7573 = AXIS2_PLACEMENT_3D ( 'NONE', #39642, #35709, #8187 ) ;
#7575 = AXIS2_PLACEMENT_3D ( 'NONE', #21057, #36787, #37057 ) ;
#7574 = CARTESIAN_POINT ( 'NONE',  ( 47.13794097070190503, -53.89583813975270488, -75.74423906255060501 ) ) ;
#7576 = ADVANCED_FACE ( 'NONE', ( #33219 ), #25350, .T. ) ;
#7577 = CARTESIAN_POINT ( 'NONE',  ( 11.43201365337999853, 34.12765256329690544, -18.10223070852750027 ) ) ;
#7578 = CARTESIAN_POINT ( 'NONE',  ( 73.01385068780759013, 0.9098571636355720083, -69.14090909090960224 ) ) ;
#7580 = CARTESIAN_POINT ( 'NONE',  ( 8.428882786094106905, -17.68703364650084353, -58.70899815131578237 ) ) ;
#7579 = DIRECTION ( 'NONE',  ( 1.000000000000000000, 0.000000000000000000, 0.000000000000000000 ) ) ;
#7581 = CARTESIAN_POINT ( 'NONE',  ( -11.21082239979770101, -42.00354444696370138, -6.430205136515479758 ) ) ;
#7582 = CARTESIAN_POINT ( 'NONE',  ( 49.01754034824669759, 22.51163454169229894, -54.40023370205440045 ) ) ;
#7583 = VERTEX_POINT ( 'NONE', #1523 ) ;
#7584 = CARTESIAN_POINT ( 'NONE',  ( 53.36579634005869366, -49.42372989600390554, -49.05761866421319439 ) ) ;
#7585 = ORIENTED_EDGE ( 'NONE', *, *, #44852, .T. ) ;
#7586 = CARTESIAN_POINT ( 'NONE',  ( 47.11598513326693904, 6.751028634652659122, -54.67405396673499496 ) ) ;
#7587 = CARTESIAN_POINT ( 'NONE',  ( 9.367202679915338948, -15.61634672871210050, -75.45282021618999124 ) ) ;
#7588 = CARTESIAN_POINT ( 'NONE',  ( 53.63393739769619373, 31.88381105532059934, 11.84999999999999964 ) ) ;
#7589 = CARTESIAN_POINT ( 'NONE',  ( 51.73306225781979606, -49.00921943299249506, -77.03096025453059781 ) ) ;
#7590 = CARTESIAN_POINT ( 'NONE',  ( 10.56036407591849979, -19.93797551083379815, -59.24287442375789681 ) ) ;
#7591 = LINE ( 'NONE', #31916, #14195 ) ;
#7592 = CARTESIAN_POINT ( 'NONE',  ( 55.35937001036280236, -45.20692410961479624, -14.95305198190059848 ) ) ;
#7593 = CARTESIAN_POINT ( 'NONE',  ( 52.57331737020290063, 18.62080981822910175, -27.97395075092120109 ) ) ;
#7594 = ORIENTED_EDGE ( 'NONE', *, *, #38044, .F. ) ;
#7595 = CARTESIAN_POINT ( 'NONE',  ( 10.70276100678979958, -21.28091057897379912, -46.03080682667329881 ) ) ;
#7596 = EDGE_CURVE ( 'NONE', #30791, #44451, #26207, .T. ) ;
#7597 = B_SPLINE_CURVE_WITH_KNOTS ( 'NONE', 3,
 ( #38649, #35211, #26830, #47037, #6669, #22887, #6414, #51213, #22634, #42838, #39158, #22372, #38378, #50688, #34686, #18711, #14784, #27090, #27345, #34426, #30754, #47292, #2737, #43350, #3252, #6933, #38905, #15306, #15040, #2995, #18965, #7186, #3516, #11121, #19483, #31010, #43094, #35475, #48558, #36486, #43605, #19983, #40176, #24156, #24677, #28360, #36745 ),
 .UNSPECIFIED., .F., .F.,
 ( 4, 2, 2, 2, 1, 1, 2, 2, 2, 2, 1, 1, 1, 2, 2, 2, 2, 1, 1, 1, 2, 2, 2, 2, 1, 2, 2, 4 ),
 ( 0.000000000000000000, 0.1250000000000352496, 0.1875000000000550116, 0.2187500000000639211, 0.2343750000000658085, 0.2421875000000672240, 0.2460937500000678901, 0.2500000000000685563, 0.3750000000000802136, 0.4375000000000867084, 0.4687500000000899836, 0.4843750000000934808, 0.4921875000000958678, 0.4960937500000944245, 0.5000000000000929257, 0.6250000000000990319, 0.6875000000001015854, 0.7187500000001020295, 0.7343750000001014744, 0.7421875000001018075, 0.7460937500001014744, 0.7500000000001011413, 0.8125000000000764944, 0.8437500000000640599, 0.8593750000000591749, 0.8671875000000557332, 0.8750000000000521805, 1.000000000000000000 ),
 .UNSPECIFIED. ) ;
#7598 = ORIENTED_EDGE ( 'NONE', *, *, #48823, .F. ) ;
#7599 = CARTESIAN_POINT ( 'NONE',  ( 11.46543046584420011, -65.12255705699759289, -16.91315247372250141 ) ) ;
#7600 = CARTESIAN_POINT ( 'NONE',  ( 9.603216745788369479, 33.01762841516160307, -46.77201822708810397 ) ) ;
#7601 = CARTESIAN_POINT ( 'NONE',  ( 72.79231116732400153, 1.384708701328909886, -62.55544205298410532 ) ) ;
#7602 = CARTESIAN_POINT ( 'NONE',  ( 68.13393739769620083, -15.61618894467929941, -65.65000000000000568 ) ) ;
#7603 = CARTESIAN_POINT ( 'NONE',  ( 10.76627208480596387, -64.36776573450144667, -23.46779268753286019 ) ) ;
#7604 = LINE ( 'NONE', #2897, #28424 ) ;
#7605 = ORIENTED_EDGE ( 'NONE', *, *, #49696, .F. ) ;
#7606 = CARTESIAN_POINT ( 'NONE',  ( 8.222916120934886663, -14.58079724080996264, -74.54932982785270212 ) ) ;
#7607 = CARTESIAN_POINT ( 'NONE',  ( 11.13393739769619906, -63.13952684277840177, -43.74348518090240390 ) ) ;
#7608 = CARTESIAN_POINT ( 'NONE',  ( 68.13393739769630031, 16.88381105531719939, -74.20000000000000284 ) ) ;
#7609 = VERTEX_POINT ( 'NONE', #22964 ) ;
#7610 = CARTESIAN_POINT ( 'NONE',  ( 23.62400244246340009, -48.75656286698960429, -35.12503119152809461 ) ) ;
#7611 = CARTESIAN_POINT ( 'NONE',  ( 17.01696881212998136, -7.733254499902739276, -77.04325171109016424 ) ) ;
#7612 = CARTESIAN_POINT ( 'NONE',  ( 11.37537782909544504, -65.24381549433910266, -22.78468322869543172 ) ) ;
#7613 = LINE ( 'NONE', #15473, #2839 ) ;
#7614 =( BOUNDED_CURVE ( )  B_SPLINE_CURVE ( 3, ( #3519, #4028, #7712, #16073 ),
 .UNSPECIFIED., .F., .T. ) 
 B_SPLINE_CURVE_WITH_KNOTS ( ( 4, 4 ),
 ( 5.087659803240767609, 5.157314376969199365 ),
 .UNSPECIFIED. ) 
 CURVE ( )  GEOMETRIC_REPRESENTATION_ITEM ( )  RATIONAL_B_SPLINE_CURVE ( ( 1.000000000000000000, 0.9995957275622187055, 0.9995957275622187055, 1.000000000000000000 ) ) 
 REPRESENTATION_ITEM ( '' )  );
#7615 = EDGE_LOOP ( 'NONE', ( #32559, #16430, #15455, #428 ) ) ;
#7616 = FILL_AREA_STYLE ('',( #11548 ) ) ;
#7617 = LINE ( 'NONE', #23563, #47673 ) ;
#7618 = CARTESIAN_POINT ( 'NONE',  ( 9.493364934882555062, -17.11955126427607965, -33.38210457755312177 ) ) ;
#7619 = LINE ( 'NONE', #20670, #5251 ) ;
#7620 = EDGE_CURVE ( 'NONE', #20658, #31407, #2823, .T. ) ;
#7621 = TOROIDAL_SURFACE ( 'NONE', #31856, 6.949999999999999289, 2.999999999999960032 ) ;
#7622 = CARTESIAN_POINT ( 'NONE',  ( 21.43117737877189910, -21.93457233315599808, -78.07024275745530417 ) ) ;
#7623 = EDGE_CURVE ( 'NONE', #22194, #42604, #25105, .T. ) ;
#7624 = FACE_OUTER_BOUND ( 'NONE', #29461, .T. ) ;
#7625 = DIRECTION ( 'NONE',  ( 0.000000000000000000, 0.000000000000000000, -1.000000000000000000 ) ) ;
#7626 = ORIENTED_EDGE ( 'NONE', *, *, #49750, .F. ) ;
#7627 = ORIENTED_EDGE ( 'NONE', *, *, #33913, .T. ) ;
#7628 = CARTESIAN_POINT ( 'NONE',  ( 13.14039184046809972, -22.43860631698549923, -58.86427365897949926 ) ) ;
#7629 = CARTESIAN_POINT ( 'NONE',  ( 13.00414154252451659, -49.37472093637801862, -34.70142521051216988 ) ) ;
#7630 = CARTESIAN_POINT ( 'NONE',  ( 11.76305550340469885, -22.11297765233079815, -32.14999999999999858 ) ) ;
#7631 = CARTESIAN_POINT ( 'NONE',  ( 47.08376783210989913, 23.19752807116610072, -75.29485540125669729 ) ) ;
#7632 = DIRECTION ( 'NONE',  ( -1.000000000000000000, 1.127159607568241538E-32, -7.935614746461580696E-16 ) ) ;
#7633 = CARTESIAN_POINT ( 'NONE',  ( 10.03166977892496625, 22.68747772516197259, -34.73809820100316870 ) ) ;
#7634 = ADVANCED_FACE ( 'NONE', ( #22190 ), #21931, .T. ) ;
#7635 = CARTESIAN_POINT ( 'NONE',  ( 11.62560706826469925, 33.71532168021870035, -16.46999247996680182 ) ) ;
#7636 = CARTESIAN_POINT ( 'NONE',  ( 23.94181861929380162, -12.96671512174780005, -75.40353636073618304 ) ) ;
#7637 = EDGE_CURVE ( 'NONE', #5655, #36176, #50262, .T. ) ;
#7638 = CARTESIAN_POINT ( 'NONE',  ( 22.14137220198069755, -20.37380969475220027, -32.14999999999999858 ) ) ;
#7639 = CARTESIAN_POINT ( 'NONE',  ( 55.44147505427400091, -50.69485088026120678, -75.76380498141109854 ) ) ;
#7641 = CARTESIAN_POINT ( 'NONE',  ( 74.93037295002240228, 11.88381105532070059, -15.31098073120859837 ) ) ;
#7640 = CARTESIAN_POINT ( 'NONE',  ( -11.32741028376500125, 10.64927095071240082, -6.431200827838360112 ) ) ;
#7642 = CARTESIAN_POINT ( 'NONE',  ( 63.11986671346460298, 0.9948723650351710690, -68.93161800279381168 ) ) ;
#7643 = CARTESIAN_POINT ( 'NONE',  ( 61.33698243797909555, 13.98069162214219929, -46.67936773079180313 ) ) ;
#7644 = CARTESIAN_POINT ( 'NONE',  ( 20.38275687770202538, 4.296863009278949264, -59.64999999999999147 ) ) ;
#7645 = FACE_OUTER_BOUND ( 'NONE', #725, .T. ) ;
#7646 = VERTEX_POINT ( 'NONE', #18534 ) ;
#7647 = CIRCLE ( 'NONE', #26027, 2.999999999999960920 ) ;
#7648 = CARTESIAN_POINT ( 'NONE',  ( 52.86806099848610074, -49.64085155770939650, -48.68114582883949737 ) ) ;
#7649 = CARTESIAN_POINT ( 'NONE',  ( 47.59379709645970280, 23.30360333313180021, -54.77931482373369931 ) ) ;
#7650 = DIRECTION ( 'NONE',  ( 0.5000000000000003331, 0.8660254037844383745, 0.000000000000000000 ) ) ;
#7651 = FACE_OUTER_BOUND ( 'NONE', #3588, .T. ) ;
#7652 = CARTESIAN_POINT ( 'NONE',  ( 61.60324134049525924, -45.27018021557786653, -47.14317994272850143 ) ) ;
#7653 = AXIS2_PLACEMENT_3D ( 'NONE', #37433, #34520, #38467 ) ;
#7654 = CARTESIAN_POINT ( 'NONE',  ( 23.45398833085310031, -14.22926856443589827, -72.17305407766770031 ) ) ;
#7655 = CARTESIAN_POINT ( 'NONE',  ( 50.83757470097779674, 17.49618323911590068, -76.31330844465840357 ) ) ;
#7656 = CARTESIAN_POINT ( 'NONE',  ( 53.05831033682530062, 18.31656324100610078, -48.91556381798330477 ) ) ;
#7657 = CARTESIAN_POINT ( 'NONE',  ( 0.3209249304026170480, -15.61618894467929941, -35.14999999999999858 ) ) ;
#7658 = CARTESIAN_POINT ( 'NONE',  ( 52.93498292564289187, -49.60578928504740048, -48.74287988808979577 ) ) ;
#7659 = ORIENTED_EDGE ( 'NONE', *, *, #45538, .F. ) ;
#7660 = LINE ( 'NONE', #40644, #21265 ) ;
#7661 = CARTESIAN_POINT ( 'NONE',  ( 47.56676769225379786, -54.56411824221549978, -54.92148441692940253 ) ) ;
#7662 = DIRECTION ( 'NONE',  ( 0.6888026391158329487, -0.7071067811865494601, 0.1598465650148944150 ) ) ;
#7663 = CYLINDRICAL_SURFACE ( 'NONE', #32737, 2.000000000000001776 ) ;
#7664 = CARTESIAN_POINT ( 'NONE',  ( 59.60922403236150302, -29.31984253203929569, -15.79452132106010076 ) ) ;
#7665 = CARTESIAN_POINT ( 'NONE',  ( 71.29497000743199919, 0.8840451408750739093, -60.55014093144429665 ) ) ;
#7666 = CARTESIAN_POINT ( 'NONE',  ( 16.13393739769620083, -1.759782484128323166, -35.01561944896766221 ) ) ;
#7667 = CARTESIAN_POINT ( 'NONE',  ( 72.27703085588929355, 1.458412159422780130, -61.64333151374460584 ) ) ;
#7668 = CARTESIAN_POINT ( 'NONE',  ( 56.46551566992090443, -50.77616483350429633, -53.85225086718720178 ) ) ;
#7669 = DIRECTION ( 'NONE',  ( -0.000000000000000000, -1.000000000000000000, -0.000000000000000000 ) ) ;
#7670 = ORIENTED_EDGE ( 'NONE', *, *, #19714, .T. ) ;
#7671 = ORIENTED_EDGE ( 'NONE', *, *, #41923, .T. ) ;
#7672 = CARTESIAN_POINT ( 'NONE',  ( 68.13393739769618662, -30.66618894467940137, -31.09383709942130380 ) ) ;
#7673 = CARTESIAN_POINT ( 'NONE',  ( -0.007164427059776000244, -45.70803162167019451, -34.77269723891829756 ) ) ;
#7674 = ORIENTED_EDGE ( 'NONE', *, *, #20221, .T. ) ;
#7675 = CYLINDRICAL_SURFACE ( 'NONE', #46156, 1.999999999999996225 ) ;
#7676 = CARTESIAN_POINT ( 'NONE',  ( 21.70064287550836113, -21.23721361656830453, -77.75920763157944293 ) ) ;
#7677 = DIRECTION ( 'NONE',  ( 0.000000000000000000, 0.000000000000000000, -1.000000000000000000 ) ) ;
#7678 = ORIENTED_EDGE ( 'NONE', *, *, #19768, .F. ) ;
#7679 = CARTESIAN_POINT ( 'NONE',  ( 10.98599679800559770, 33.59687660070252946, -23.20934807910649766 ) ) ;
#7680 = CARTESIAN_POINT ( 'NONE',  ( 43.34489039530834020, 6.595245306295674403, -73.59517026744862278 ) ) ;
#7681 = CARTESIAN_POINT ( 'NONE',  ( 12.71511855601199947, 34.23582645008529823, -23.64159478333349895 ) ) ;
#7682 = EDGE_CURVE ( 'NONE', #33030, #34403, #50502, .T. ) ;
#7683 = CARTESIAN_POINT ( 'NONE',  ( 13.37138816098100058, -23.38478223887699770, -36.40108501799149820 ) ) ;
#7684 = ADVANCED_FACE ( 'NONE', ( #31086, #47114 ), #18017, .T. ) ;
#7685 = CARTESIAN_POINT ( 'NONE',  ( 16.13393739769620083, -15.61618894467929941, -28.45282021618999835 ) ) ;
#7686 = CARTESIAN_POINT ( 'NONE',  ( 10.66246720353709954, 33.63422984119760173, -18.01843150758180201 ) ) ;
#7687 =( NAMED_UNIT ( * ) SI_UNIT ( $, .STERADIAN. ) SOLID_ANGLE_UNIT ( ) );
#7688 = EDGE_CURVE ( 'NONE', #49694, #9565, #47412, .T. ) ;
#7689 = CARTESIAN_POINT ( 'NONE',  ( 59.28323976345399871, -28.29587047411439826, -15.67173192143519955 ) ) ;
#7690 = CIRCLE ( 'NONE', #36957, 9.000000000000007105 ) ;
#7691 = CARTESIAN_POINT ( 'NONE',  ( 16.13393739769639623, 7.383811055320659733, -59.64999999999999147 ) ) ;
#7692 = CARTESIAN_POINT ( 'NONE',  ( 46.42028843557609719, -53.00875148048739760, -76.14999999999999147 ) ) ;
#7693 = CARTESIAN_POINT ( 'NONE',  ( 23.60773268908170053, -13.22262851426480168, -75.91383772819759201 ) ) ;
#7694 = AXIS2_PLACEMENT_3D ( 'NONE', #20021, #28402, #48085 ) ;
#7695 = CARTESIAN_POINT ( 'NONE',  ( 55.12912832402329144, 14.86073885494939972, -16.25649608933859724 ) ) ;
#7696 = AXIS2_PLACEMENT_3D ( 'NONE', #25214, #17376, #21285 ) ;
#7697 = CARTESIAN_POINT ( 'NONE',  ( 41.40014251418400448, 14.21126602188850008, -6.186187947539579568 ) ) ;
#7698 = CARTESIAN_POINT ( 'NONE',  ( 15.05440318628110141, 21.88381105532300097, -76.14999999999999147 ) ) ;
#7699 = CARTESIAN_POINT ( 'NONE',  ( 83.73251846585449698, -44.53015045067650135, -46.86010343433790126 ) ) ;
#7700 = CARTESIAN_POINT ( 'NONE',  ( 16.13393739769620083, -15.61618894467929941, -54.64999999999999858 ) ) ;
#7701 = CARTESIAN_POINT ( 'NONE',  ( 22.01250374557920253, -21.39764018139420187, -39.75501738210738978 ) ) ;
#7702 = EDGE_CURVE ( 'NONE', #18529, #50796, #34592, .T. ) ;
#7703 = VERTEX_POINT ( 'NONE', #10685 ) ;
#7704 = CARTESIAN_POINT ( 'NONE',  ( 16.13393739769620083, -15.61618894467929941, 9.349999999999999645 ) ) ;
#7705 = CARTESIAN_POINT ( 'NONE',  ( 15.41374403315040098, -50.77302816826519916, -20.47798662115089741 ) ) ;
#7706 = CARTESIAN_POINT ( 'NONE',  ( 50.26043905619395247, -36.48157363899628791, -76.16290606360576021 ) ) ;
#7707 = CARTESIAN_POINT ( 'NONE',  ( 9.367479537931210132, -15.61613030728229923, -79.45282021618999124 ) ) ;
#7708 = APPLICATION_CONTEXT ( 'automotive_design' ) ;
#7709 = CARTESIAN_POINT ( 'NONE',  ( 68.13393739845098196, -29.66618894551239904, -65.65000000119469803 ) ) ;
#7710 = ORIENTED_EDGE ( 'NONE', *, *, #14710, .T. ) ;
#7711 = CARTESIAN_POINT ( 'NONE',  ( -11.32734370190460105, -41.88171845330919751, -6.430192534648670133 ) ) ;
#7712 = CARTESIAN_POINT ( 'NONE',  ( -0.01592648613897638260, -4.171047364367892030, -34.78031642072625829 ) ) ;
#7713 = CARTESIAN_POINT ( 'NONE',  ( 18.15116866486563652, 18.38379944632345797, -83.15271738017148095 ) ) ;
#7714 = CARTESIAN_POINT ( 'NONE',  ( 63.45006824032990522, 1.383161449028140089, -62.62844710992279573 ) ) ;
#7715 = CARTESIAN_POINT ( 'NONE',  ( 57.55751162055879888, -50.51057731619299318, -53.27961218324600168 ) ) ;
#7716 = CARTESIAN_POINT ( 'NONE',  ( 42.31976157503279978, 12.63773038262479886, -4.715714940419609924 ) ) ;
#7717 = CARTESIAN_POINT ( 'NONE',  ( 61.47028729602050845, -45.40949600205838976, -47.41717745499089887 ) ) ;
#7718 = CARTESIAN_POINT ( 'NONE',  ( 63.38217364139809007, 0.9405967369938049716, -61.98545004926840107 ) ) ;
#7719 = CARTESIAN_POINT ( 'NONE',  ( 56.53085617112640193, -47.72181054224110142, -48.00558725693349515 ) ) ;
#7720 = CARTESIAN_POINT ( 'NONE',  ( 24.04489396232973064, -15.58787332083394617, -75.79118696779985953 ) ) ;
#7721 = CARTESIAN_POINT ( 'NONE',  ( 15.24810277342973031, -22.38318460617302819, -62.99448372488342329 ) ) ;
#7722 = CARTESIAN_POINT ( 'NONE',  ( 18.26290488187510164, -51.89834789502650381, -75.53980707817230211 ) ) ;
#7723 = CIRCLE ( 'NONE', #15279, 20.00000000000000000 ) ;
#7724 = CARTESIAN_POINT ( 'NONE',  ( 9.020183826706210439, -17.83005535202389780, -61.97130586100059446 ) ) ;
#7725 = CARTESIAN_POINT ( 'NONE',  ( 46.98749101202549383, 7.998570365497442936, -34.79644638567071269 ) ) ;
#7726 = CARTESIAN_POINT ( 'NONE',  ( 50.89343982362250074, -52.15145316057449776, -52.52829244528589925 ) ) ;
#7727 = ORIENTED_EDGE ( 'NONE', *, *, #14061, .T. ) ;
#7728 = CARTESIAN_POINT ( 'NONE',  ( 71.33393739769650210, 1.396834109478129804, -70.23662692463440749 ) ) ;
#7729 = TOROIDAL_SURFACE ( 'NONE', #12729, 23.49999999909039872, 0.4999999999562930175 ) ;
#7730 = CARTESIAN_POINT ( 'NONE',  ( 9.973190895944735956, -18.47182041587143431, -35.31469777396277010 ) ) ;
#7731 = CARTESIAN_POINT ( 'NONE',  ( 72.81285642849219641, 1.383357884654609959, -68.68594134708139620 ) ) ;
#7732 = DIRECTION ( 'NONE',  ( 0.3805321250008311118, 0.000000000000000000, -0.9247677015566405645 ) ) ;
#7733 = CARTESIAN_POINT ( 'NONE',  ( 9.374784576662598568, -12.69651527581430095, -81.23899999999999011 ) ) ;
#7734 = EDGE_LOOP ( 'NONE', ( #17522, #34315, #14388, #44515, #6089 ) ) ;
#7735 = CARTESIAN_POINT ( 'NONE',  ( 17.43015572509100153, 21.57872223484060115, -76.12922349804929922 ) ) ;
#7736 = ORIENTED_EDGE ( 'NONE', *, *, #31576, .T. ) ;
#7737 = EDGE_LOOP ( 'NONE', ( #9125, #31180, #17663, #49723, #46222 ) ) ;
#7738 = CARTESIAN_POINT ( 'NONE',  ( 57.18178511478169668, -45.84706250231700153, -26.25564504989590020 ) ) ;
#7739 = CARTESIAN_POINT ( 'NONE',  ( 23.51964986281049974, -16.15416379988030116, -81.23899999999999011 ) ) ;
#7740 = CARTESIAN_POINT ( 'NONE',  ( -11.54263325867530199, -34.48402086119780563, -44.80353970119273299 ) ) ;
#7741 = ORIENTED_EDGE ( 'NONE', *, *, #47852, .T. ) ;
#7742 = CARTESIAN_POINT ( 'NONE',  ( 20.25644374842187645, -10.19188613274733157, -80.15984542592896389 ) ) ;
#7743 = EDGE_LOOP ( 'NONE', ( #48118, #24371, #21226, #33620, #45693, #35147 ) ) ;
#7744 = CARTESIAN_POINT ( 'NONE',  ( 9.221449101009920213, -11.63199795648596258, -62.95899854462519585 ) ) ;
#7745 = EDGE_CURVE ( 'NONE', #38464, #13785, #10163, .T. ) ;
#7746 = CARTESIAN_POINT ( 'NONE',  ( 45.15010597285510130, -33.29644663991430065, -35.08262351468650309 ) ) ;
#7747 = VERTEX_POINT ( 'NONE', #46339 ) ;
#7748 = ORIENTED_EDGE ( 'NONE', *, *, #47447, .F. ) ;
#7749 = LINE ( 'NONE', #19784, #42599 ) ;
#7750 = DIRECTION ( 'NONE',  ( 0.8660254037844387076, 0.4999999999999998890, 2.775557561562889194E-17 ) ) ;
#7751 = CARTESIAN_POINT ( 'NONE',  ( 60.82616199806800239, 14.39437461288099840, -47.60746935378129763 ) ) ;
#7752 = CARTESIAN_POINT ( 'NONE',  ( 16.13393739769620083, -3.616188944679339823, -22.14999999999999858 ) ) ;
#7753 = CARTESIAN_POINT ( 'NONE',  ( 84.44784216359251161, -43.11618894467930119, -47.47585302082339354 ) ) ;
#7754 = CARTESIAN_POINT ( 'NONE',  ( -7.968642834068480951, 13.86896153487260008, -5.614579153141090018 ) ) ;
#7755 = CIRCLE ( 'NONE', #20292, 0.4999999999999982236 ) ;
#7756 = CARTESIAN_POINT ( 'NONE',  ( 47.01289945827778638, 23.18945904231436117, -75.36289877398526471 ) ) ;
#7757 = CARTESIAN_POINT ( 'NONE',  ( 9.934167556912912644, -18.97671188063486980, -43.68906509112390779 ) ) ;
#7758 = CARTESIAN_POINT ( 'NONE',  ( 11.14170694428959862, -9.561076783599030904, -64.56803669556019543 ) ) ;
#7759 = EDGE_CURVE ( 'NONE', #9610, #42606, #26123, .T. ) ;
#7760 = ORIENTED_EDGE ( 'NONE', *, *, #41352, .T. ) ;
#7761 = CARTESIAN_POINT ( 'NONE',  ( 56.52536539877740296, -50.75180572374080157, -53.84278118897309895 ) ) ;
#7762 = CARTESIAN_POINT ( 'NONE',  ( 11.63245656708829756, -51.88627667935560339, -69.46507341766636046 ) ) ;
#7763 = ADVANCED_FACE ( 'NONE', ( #30574 ), #40470, .F. ) ;
#7764 = CARTESIAN_POINT ( 'NONE',  ( 71.92220195954379847, 1.332297898505690137, -70.13430431592830416 ) ) ;
#7765 = CARTESIAN_POINT ( 'NONE',  ( 42.62445565279771387, -39.82941498042225703, -73.31524913290161294 ) ) ;
#7766 = CYLINDRICAL_SURFACE ( 'NONE', #43975, 2.000000000000003553 ) ;
#7767 = FACE_OUTER_BOUND ( 'NONE', #14921, .T. ) ;
#7768 = CARTESIAN_POINT ( 'NONE',  ( 61.14297911010989850, 14.08836397059769574, -46.99578574395629715 ) ) ;
#7769 = CARTESIAN_POINT ( 'NONE',  ( 48.87989277424459544, -54.00735095224600002, -55.25437946346490037 ) ) ;
#7770 = CARTESIAN_POINT ( 'NONE',  ( 72.38393739769620083, 4.883811055320659733, -61.44999999999999574 ) ) ;
#7771 = DIRECTION ( 'NONE',  ( 0.000000000000000000, 0.000000000000000000, -1.000000000000000000 ) ) ;
#7772 = CARTESIAN_POINT ( 'NONE',  ( 47.81203533955039831, 23.17981727675569914, -54.77279602202729336 ) ) ;
#7773 = VERTEX_POINT ( 'NONE', #38200 ) ;
#7774 = CARTESIAN_POINT ( 'NONE',  ( 11.68549127948460153, -10.14317847777680015, -80.12993496510929958 ) ) ;
#7775 = CARTESIAN_POINT ( 'NONE',  ( 11.97525711002020898, -21.02750221141963394, -77.16116563337958212 ) ) ;
#7776 = ORIENTED_EDGE ( 'NONE', *, *, #29136, .F. ) ;
#7777 = CARTESIAN_POINT ( 'NONE',  ( 17.51664573667515157, 21.64019614504773870, -76.12465453343314437 ) ) ;
#7778 = CARTESIAN_POINT ( 'NONE',  ( 60.96180853276540290, -45.45167203910889242, -47.29837554833880375 ) ) ;
#7779 = CARTESIAN_POINT ( 'NONE',  ( 13.39998208310050032, -51.78678246903520233, -23.15000000000000213 ) ) ;
#7780 = CARTESIAN_POINT ( 'NONE',  ( 83.53665348990875827, 13.38079070459579967, -46.51478504176231610 ) ) ;
#7782 = CARTESIAN_POINT ( 'NONE',  ( 16.13393739769620083, -45.61618894467940066, -35.14999999999999858 ) ) ;
#7781 = CARTESIAN_POINT ( 'NONE',  ( 41.83358903174870846, 8.514088802998820427, -77.13456888834446090 ) ) ;
#7783 = CARTESIAN_POINT ( 'NONE',  ( 30.96406434931616403, 4.463581150976708933, -84.62099912964093562 ) ) ;
#7784 = CARTESIAN_POINT ( 'NONE',  ( 75.13393739769618662, 4.883811055320659733, -84.38499399519520239 ) ) ;
#7785 = EDGE_LOOP ( 'NONE', ( #5142, #17185, #4346, #38645, #13985 ) ) ;
#7786 = CARTESIAN_POINT ( 'NONE',  ( 0.1155610841158959956, 19.94237700917059897, -35.14999985728680088 ) ) ;
#7787 = EDGE_LOOP ( 'NONE', ( #45604, #28330 ) ) ;
#7788 = ORIENTED_EDGE ( 'NONE', *, *, #47296, .T. ) ;
#7789 = CARTESIAN_POINT ( 'NONE',  ( -1.224559824875987468, -24.96582652780387690, -84.65000000000000568 ) ) ;
#7790 = CARTESIAN_POINT ( 'NONE',  ( 29.13393466042959901, -4.484470077231426544, -35.10904485683914800 ) ) ;
#7791 = AXIS2_PLACEMENT_3D ( 'NONE', #9773, #33601, #40696 ) ;
#7792 = CARTESIAN_POINT ( 'NONE',  ( 22.90117443638819239, -15.61618876209028528, -62.84717844892357164 ) ) ;
#7793 = CARTESIAN_POINT ( 'NONE',  ( 10.75428388279330072, -64.86834293686459318, -46.90868476786780406 ) ) ;
#7794 = AXIS2_PLACEMENT_3D ( 'NONE', #28805, #12847, #19473 ) ;
#7795 = ORIENTED_EDGE ( 'NONE', *, *, #16365, .T. ) ;
#7796 = CARTESIAN_POINT ( 'NONE',  ( 20.11801379417378755, -22.52874512401025342, -55.84094417680480404 ) ) ;
#7797 = CARTESIAN_POINT ( 'NONE',  ( 12.20479792536879948, -10.10644435241950134, -32.14999999999999858 ) ) ;
#7798 = CARTESIAN_POINT ( 'NONE',  ( 56.35668519540149646, -50.69685899399890161, -53.18239453017169893 ) ) ;
#7799 = EDGE_CURVE ( 'NONE', #14157, #20336, #50750, .T. ) ;
#7800 = CARTESIAN_POINT ( 'NONE',  ( 22.90093709110179887, -15.61375976151432532, -46.45271396509134831 ) ) ;
#7801 = CARTESIAN_POINT ( 'NONE',  ( 59.71002301575170179, -1.985703112241369972, -15.78375127595690230 ) ) ;
#7802 = CARTESIAN_POINT ( 'NONE',  ( 51.67727694508769787, -49.68733520360949996, -76.65630996370649086 ) ) ;
#7803 = CARTESIAN_POINT ( 'NONE',  ( 57.64403164091130094, -49.99897929508820482, -52.47668038226420606 ) ) ;
#7804 = ORIENTED_EDGE ( 'NONE', *, *, #46751, .F. ) ;
#7805 = CARTESIAN_POINT ( 'NONE',  ( 46.63393739769619373, -39.11086919362080039, -34.64999999999999858 ) ) ;
#7806 = CARTESIAN_POINT ( 'NONE',  ( 82.81464131963001307, -43.11618894467930119, -49.28546657628889704 ) ) ;
#7807 = DIRECTION ( 'NONE',  ( 0.000000000000000000, 0.000000000000000000, 1.000000000000000000 ) ) ;
#7808 = DIRECTION ( 'NONE',  ( 1.000000000000000000, 0.000000000000000000, 0.000000000000000000 ) ) ;
#7809 = CARTESIAN_POINT ( 'NONE',  ( 18.57444516463139905, -8.157591929750100945, -49.61315261507609620 ) ) ;
#7810 = CARTESIAN_POINT ( 'NONE',  ( 12.28937801554179821, -50.00765209207849438, -21.14656546066629872 ) ) ;
#7811 = AXIS2_PLACEMENT_3D ( 'NONE', #44546, #8648, #40614 ) ;
#7812 = CARTESIAN_POINT ( 'NONE',  ( 55.48172515062150012, 19.38381105532069881, -76.40185937632740831 ) ) ;
#7813 = CARTESIAN_POINT ( 'NONE',  ( 71.33393739769628894, 10.88381105532070059, -61.94999999999999574 ) ) ;
#7814 = CARTESIAN_POINT ( 'NONE',  ( 57.48325051288529863, 13.88381105532070059, -17.42702951318920057 ) ) ;
#7815 = CARTESIAN_POINT ( 'NONE',  ( 61.12227989346150281, -45.45881623026480156, -47.44113852007230037 ) ) ;
#7816 = LINE ( 'NONE', #12010, #15380 ) ;
#7817 = CARTESIAN_POINT ( 'NONE',  ( 14.34415610061919821, -8.794221333858748935, -58.26550999155039534 ) ) ;
#7818 = CARTESIAN_POINT ( 'NONE',  ( -0.03447620312152738231, -22.81072779144790275, -34.79644660940672907 ) ) ;
#7819 = ORIENTED_EDGE ( 'NONE', *, *, #14254, .T. ) ;
#7820 = CARTESIAN_POINT ( 'NONE',  ( 13.42425491221250056, -51.80633386256230466, -74.54427505470819426 ) ) ;
#7821 = AXIS2_PLACEMENT_3D ( 'NONE', #16088, #44906, #878 ) ;
#7822 = CARTESIAN_POINT ( 'NONE',  ( 47.24973492052809831, -54.75565816223589621, -54.63348945589360284 ) ) ;
#7823 = ADVANCED_FACE ( 'NONE', ( #18269 ), #48821, .F. ) ;
#7824 = CARTESIAN_POINT ( 'NONE',  ( 11.71414166050488248, 34.09778695713147556, -47.42034454217008488 ) ) ;
#7825 = CIRCLE ( 'NONE', #12883, 29.70020322226740106 ) ;
#7826 = DIRECTION ( 'NONE',  ( 0.000000000000000000, 0.000000000000000000, 1.000000000000000000 ) ) ;
#7827 = CARTESIAN_POINT ( 'NONE',  ( 15.67961772667648290, -50.86266697332435172, -20.20261269004708993 ) ) ;
#7828 = AXIS2_PLACEMENT_3D ( 'NONE', #16817, #35703, #43824 ) ;
#7829 = DIRECTION ( 'NONE',  ( 0.5818181818182710519, 0.000000000000000000, -0.8133188816852104930 ) ) ;
#7830 = CARTESIAN_POINT ( 'NONE',  ( 9.366916744691108576, -14.73054192615060032, -75.49448329847818684 ) ) ;
#7831 = CARTESIAN_POINT ( 'NONE',  ( -6.866062602303809825, -22.61618894467929763, -59.64999999999999147 ) ) ;
#7832 = DIRECTION ( 'NONE',  ( 0.000000000000000000, 0.000000000000000000, -1.000000000000000000 ) ) ;
#7833 = DIRECTION ( 'NONE',  ( -0.2260571801428149508, -1.665334536937734318E-16, 0.9741140340359947247 ) ) ;
#7834 = FACE_OUTER_BOUND ( 'NONE', #2183, .T. ) ;
#7835 = CARTESIAN_POINT ( 'NONE',  ( 49.16018969832690289, 22.62491742194789879, -54.90022772030559395 ) ) ;
#7836 = EDGE_LOOP ( 'NONE', ( #34578, #14099, #19479, #7659 ) ) ;
#7837 = CARTESIAN_POINT ( 'NONE',  ( 52.96080973490879984, -49.61775551211789548, -48.98458849178360452 ) ) ;
#7838 = EDGE_LOOP ( 'NONE', ( #440, #14884, #5152, #24851, #5415 ) ) ;
#7839 = CARTESIAN_POINT ( 'NONE',  ( 42.60159069889220262, 7.610747875504726423, -77.64264605067509706 ) ) ;
#7840 = CARTESIAN_POINT ( 'NONE',  ( 4.133937397696209715, -22.54439217495480108, -47.64999999999999858 ) ) ;
#7841 = CARTESIAN_POINT ( 'NONE',  ( 14.29774505810699914, 19.88381105514569924, -22.54670832509589928 ) ) ;
#7842 = DIRECTION ( 'NONE',  ( 0.000000000000000000, 0.000000000000000000, -1.000000000000000000 ) ) ;
#7843 = CARTESIAN_POINT ( 'NONE',  ( 22.07441835734369917, -11.81444662507229992, -52.27160849015929500 ) ) ;
#7844 = CARTESIAN_POINT ( 'NONE',  ( 53.36465014982429977, 18.25085194934079880, -49.20420490330940311 ) ) ;
#7845 = CARTESIAN_POINT ( 'NONE',  ( 55.59033526946949877, -45.44877594268120191, -15.86859551517999911 ) ) ;
#7846 = CARTESIAN_POINT ( 'NONE',  ( 53.37088539291629985, 17.75190881940810073, -26.62991259020409984 ) ) ;
#7847 = CIRCLE ( 'NONE', #40459, 1.999999999999998224 ) ;
#7848 = ORIENTED_EDGE ( 'NONE', *, *, #28958, .T. ) ;
#7849 = CARTESIAN_POINT ( 'NONE',  ( 13.17756150054800024, -8.346622950897849336, -46.66455827518229427 ) ) ;
#7850 = ORIENTED_EDGE ( 'NONE', *, *, #48497, .F. ) ;
#7851 = CARTESIAN_POINT ( 'NONE',  ( 11.64437505592259825, -65.39202089365400639, -17.80448344477410316 ) ) ;
#7852 = CARTESIAN_POINT ( 'NONE',  ( 11.80354816905300019, 33.97835162598539682, -46.90015655923220095 ) ) ;
#7853 = CARTESIAN_POINT ( 'NONE',  ( 72.92486918121919359, 1.326324093417220240, -62.46048956832549948 ) ) ;
#7854 = CARTESIAN_POINT ( 'NONE',  ( 11.63393739769619906, -41.61618894467930119, -34.64999999999999858 ) ) ;
#7855 = CARTESIAN_POINT ( 'NONE',  ( 11.34809686822852726, -65.22440864330458510, -22.81359155188068044 ) ) ;
#7856 = DIRECTION ( 'NONE',  ( 0.000000000000000000, 1.000000000000000000, 0.000000000000000000 ) ) ;
#7857 = ORIENTED_EDGE ( 'NONE', *, *, #13740, .T. ) ;
#7858 = CARTESIAN_POINT ( 'NONE',  ( 64.65764093855688088, 1.007912009470870229, -70.53231455471869538 ) ) ;
#7859 = CARTESIAN_POINT ( 'NONE',  ( 11.10551638025419940, -63.28312641050290210, -44.25178297920150072 ) ) ;
#7860 = EDGE_CURVE ( 'NONE', #26641, #33083, #26909, .T. ) ;
#7861 = CARTESIAN_POINT ( 'NONE',  ( 70.83745409581385388, 17.98087126524510637, -71.50000000000081002 ) ) ;
#7862 = EDGE_LOOP ( 'NONE', ( #48210, #37435 ) ) ;
#7863 = CARTESIAN_POINT ( 'NONE',  ( 8.382179679036624975, -17.45534441210563159, -44.71833966285539219 ) ) ;
#7864 = CARTESIAN_POINT ( 'NONE',  ( 19.37692227700529202, -8.371908506326338539, -77.14162090755425538 ) ) ;
#7865 = CARTESIAN_POINT ( 'NONE',  ( 12.13393739769649926, 24.18330853958550364, -23.15000000000000213 ) ) ;
#7866 = CARTESIAN_POINT ( 'NONE',  ( 9.081253177307520019, -11.91239544520527005, -48.66177660431670660 ) ) ;
#7867 = AXIS2_PLACEMENT_3D ( 'NONE', #32545, #15825, #4285 ) ;
#7868 = VERTEX_POINT ( 'NONE', #4811 ) ;
#7869 = EDGE_CURVE ( 'NONE', #49041, #42488, #37223, .T. ) ;
#7870 = CARTESIAN_POINT ( 'NONE',  ( 11.27225553591746809, -21.94235124599162390, -36.21600094350794308 ) ) ;
#7871 = DIRECTION ( 'NONE',  ( 0.000000000000000000, 9.718338800990680596E-16, -1.000000000000000000 ) ) ;
#7872 = CARTESIAN_POINT ( 'NONE',  ( 0.3209249304026220440, -50.71887597443840434, -34.64999999999999858 ) ) ;
#7873 = CARTESIAN_POINT ( 'NONE',  ( 56.37610586342359653, 14.84999283348500043, -45.22263387109850186 ) ) ;
#7874 = ADVANCED_FACE ( 'NONE', ( #24178 ), #20262, .T. ) ;
#7875 = CARTESIAN_POINT ( 'NONE',  ( 19.73760564896319991, -23.03213764937959951, -70.14834965109328380 ) ) ;
#7876 = CARTESIAN_POINT ( 'NONE',  ( 22.72644110385109428, -13.50767635585680715, -38.74801692456930624 ) ) ;
#7877 = CARTESIAN_POINT ( 'NONE',  ( 46.06102281558538891, -38.15968466400891401, -60.01451776560848117 ) ) ;
#7878 = APPLICATION_PROTOCOL_DEFINITION ( 'draft international standard', 'automotive_design', 1998, #22066 ) ;
#7879 = ORIENTED_EDGE ( 'NONE', *, *, #45381, .F. ) ;
#7880 = CARTESIAN_POINT ( 'NONE',  ( 18.54562800134210221, -22.66533373234200255, -66.62772890321430452 ) ) ;
#7881 = DIRECTION ( 'NONE',  ( 0.000000000000000000, 0.000000000000000000, 1.000000000000000000 ) ) ;
#7882 = CARTESIAN_POINT ( 'NONE',  ( 10.42052905183000000, -20.77277191077440222, -32.14999999999999858 ) ) ;
#7883 = AXIS2_PLACEMENT_3D ( 'NONE', #31826, #36281, #39467 ) ;
#7884 = CARTESIAN_POINT ( 'NONE',  ( 47.30620419303679824, 23.48429292510279609, -74.17369128426381053 ) ) ;
#7885 = ADVANCED_FACE ( 'NONE', ( #16344 ), #14516, .T. ) ;
#7886 = DIRECTION ( 'NONE',  ( 0.6911981449639433839, -0.7226652920947592706, -1.665334536937735550E-16 ) ) ;
#7887 = CARTESIAN_POINT ( 'NONE',  ( 11.96713421144920098, 33.63456231549939446, -16.19173486065400169 ) ) ;
#7888 = CARTESIAN_POINT ( 'NONE',  ( 8.703895965235538768, -12.04166729543830172, -70.65040049691889124 ) ) ;
#7889 = CARTESIAN_POINT ( 'NONE',  ( 22.52859995526739922, -19.73945381444989877, -32.14999999999999858 ) ) ;
#7890 = CARTESIAN_POINT ( 'NONE',  ( 56.90565798765720729, -50.64481172289290356, -74.14903650335379837 ) ) ;
#7891 = CARTESIAN_POINT ( 'NONE',  ( 10.83485780772508988, -55.26361012050001165, -45.05995334480344638 ) ) ;
#7892 = AXIS2_PLACEMENT_3D ( 'NONE', #51467, #11382, #46256 ) ;
#7893 = CARTESIAN_POINT ( 'NONE',  ( 63.41515590138089919, 1.383136297697689976, -68.56705292396610218 ) ) ;
#7894 = CARTESIAN_POINT ( 'NONE',  ( 61.56738629693729337, 13.90151360212160014, -46.47169905912059562 ) ) ;
#7895 = DIRECTION ( 'NONE',  ( 0.5835456732599411112, 0.8120803206700689669, 0.000000000000000000 ) ) ;
#7896 = ORIENTED_EDGE ( 'NONE', *, *, #43818, .T. ) ;
#7897 = CARTESIAN_POINT ( 'NONE',  ( 52.84731369148340008, -49.65172165314799457, -48.60966827451729699 ) ) ;
#7898 = EDGE_CURVE ( 'NONE', #31235, #42670, #9512, .T. ) ;
#7899 = CARTESIAN_POINT ( 'NONE',  ( 58.54882648235869880, -45.58368087071139740, -26.43241409811030351 ) ) ;
#7900 = CARTESIAN_POINT ( 'NONE',  ( 18.20455076684766027, -23.32130774566027753, -72.20902145591645649 ) ) ;
#7901 = CARTESIAN_POINT ( 'NONE',  ( 61.16408118782140946, 14.10070246553319961, -47.10588363253890520 ) ) ;
#7902 = CARTESIAN_POINT ( 'NONE',  ( 23.45321186227019794, -17.00720120824169612, -76.29243849297590430 ) ) ;
#7903 = CARTESIAN_POINT ( 'NONE',  ( 51.67727282663010158, 18.45495170809379815, -76.65630935983880079 ) ) ;
#7904 = CARTESIAN_POINT ( 'NONE',  ( 52.72459105117300737, 18.49182676863240005, -48.48894656618049481 ) ) ;
#7905 = CARTESIAN_POINT ( 'NONE',  ( 0.1457841021255935343, -4.451138319363987073, -34.68167779225149161 ) ) ;
#7906 = CARTESIAN_POINT ( 'NONE',  ( -0.3963262347861145618, -45.30092459685357653, -35.11109881085425144 ) ) ;
#7907 = ORIENTED_EDGE ( 'NONE', *, *, #17615, .T. ) ;
#7908 = DIRECTION ( 'NONE',  ( 0.000000000000000000, 0.000000000000000000, 1.000000000000000000 ) ) ;
#7909 = CARTESIAN_POINT ( 'NONE',  ( 47.58993135570310073, -54.55740034306059982, -55.07469421153570721 ) ) ;
#7910 = DIRECTION ( 'NONE',  ( -1.000000000000000000, 0.000000000000000000, 0.000000000000000000 ) ) ;
#7911 =( BOUNDED_CURVE ( )  B_SPLINE_CURVE ( 3, ( #4546, #45164, #41489, #9278 ),
 .UNSPECIFIED., .F., .T. ) 
 B_SPLINE_CURVE_WITH_KNOTS ( ( 4, 4 ),
 ( 0.7853981633974360665, 1.570796326794899000 ),
 .UNSPECIFIED. ) 
 CURVE ( )  GEOMETRIC_REPRESENTATION_ITEM ( )  RATIONAL_B_SPLINE_CURVE ( ( 1.000000000000000000, 0.9492530216741892346, 0.9492530216741892346, 1.000000000000000000 ) ) 
 REPRESENTATION_ITEM ( '' )  );
#7912 = CARTESIAN_POINT ( 'NONE',  ( -15.86606260230380094, -15.61618894467929941, -21.15000000000000213 ) ) ;
#7913 = CARTESIAN_POINT ( 'NONE',  ( 58.98156044741060100, -28.10868613328409893, -15.65041641687770024 ) ) ;
#7914 = CARTESIAN_POINT ( 'NONE',  ( 71.19138260135351004, 1.383767307422969939, -60.97855929785719553 ) ) ;
#7915 = CARTESIAN_POINT ( 'NONE',  ( 68.13393739769620083, 6.883811055320649963, -71.50000000000000000 ) ) ;
#7916 = CARTESIAN_POINT ( 'NONE',  ( 72.19159089122339878, 1.443555314919450216, -61.52390474483700444 ) ) ;
#7917 = DIRECTION ( 'NONE',  ( 8.462868000000000073E-18, -1.066343000000000058E-17, 1.000000000000000000 ) ) ;
#7918 = DIRECTION ( 'NONE',  ( 0.000000000000000000, 0.000000000000000000, -1.000000000000000000 ) ) ;
#7919 = ORIENTED_EDGE ( 'NONE', *, *, #30689, .F. ) ;
#7920 = ORIENTED_EDGE ( 'NONE', *, *, #30685, .T. ) ;
#7921 = CIRCLE ( 'NONE', #36327, 23.00000000000000000 ) ;
#7922 = CARTESIAN_POINT ( 'NONE',  ( 23.04645333911465599, -11.63204389240351588, -55.62566189992365651 ) ) ;
#7923 = CARTESIAN_POINT ( 'NONE',  ( 50.02500898439532762, -29.89093149159158713, -15.97526755063678117 ) ) ;
#7924 = ORIENTED_EDGE ( 'NONE', *, *, #10767, .T. ) ;
#7925 = CARTESIAN_POINT ( 'NONE',  ( 8.428802417734461372, -13.54563645402293659, -58.59099060088449562 ) ) ;
#7926 = CARTESIAN_POINT ( 'NONE',  ( 15.10086521727856379, -23.46371762042167575, -78.04932787247608417 ) ) ;
#7927 = DIRECTION ( 'NONE',  ( 1.000000000000000000, 0.000000000000000000, 0.000000000000000000 ) ) ;
#7929 = ORIENTED_EDGE ( 'NONE', *, *, #35357, .F. ) ;
#7928 = B_SPLINE_CURVE_WITH_KNOTS ( 'NONE', 3,
 ( #46514, #17425, #13507, #26559, #41525, #18454, #26300, #29714 ),
 .UNSPECIFIED., .F., .F.,
 ( 4, 2, 2, 4 ),
 ( 0.000000000000000000, 0.006927380359722845604, 0.5031982232999553384, 1.000000000000000000 ),
 .UNSPECIFIED. ) ;
#7930 = CARTESIAN_POINT ( 'NONE',  ( 20.71851373775454519, -20.65600983156726045, -80.71802773679567622 ) ) ;
#7931 = CARTESIAN_POINT ( 'NONE',  ( 44.38457061139609294, 6.734955052058427150, -68.39683385616302758 ) ) ;
#7932 = CARTESIAN_POINT ( 'NONE',  ( 23.92337672836263351, -17.04563464948125073, -65.56543222284031458 ) ) ;
#7933 = EDGE_CURVE ( 'NONE', #9877, #5342, #43808, .T. ) ;
#7934 = CARTESIAN_POINT ( 'NONE',  ( 12.66766167757590011, -8.135035779020970637, -41.15422088180859816 ) ) ;
#7935 = CARTESIAN_POINT ( 'NONE',  ( 20.99562311489945898, -21.94234805090159313, -67.79933317097351164 ) ) ;
#7936 = STYLED_ITEM ( 'NONE', ( #42372 ), #9246 ) ;
#7937 = CARTESIAN_POINT ( 'NONE',  ( 19.72404980843187516, -22.74131306260592567, -50.14348317235646135 ) ) ;
#7938 = CARTESIAN_POINT ( 'NONE',  ( 0.000000000000000000, 0.000000000000000000, 0.000000000000000000 ) ) ;
#7939 = CARTESIAN_POINT ( 'NONE',  ( 62.45731387899189713, -29.68130429890049982, -16.13463557047360197 ) ) ;
#7940 = CARTESIAN_POINT ( 'NONE',  ( 8.428880519735075794, -17.68702540576067506, -42.70899812693631503 ) ) ;
#7941 = CARTESIAN_POINT ( 'NONE',  ( 10.02178489954199847, -19.87626377456960114, -33.03890213223969141 ) ) ;
#7942 = CARTESIAN_POINT ( 'NONE',  ( 40.73312621558000046, 14.05717019330969819, -5.671158935740639784 ) ) ;
#7943 = DIRECTION ( 'NONE',  ( -0.6911981449639438280, -0.7226652920947587155, -3.885780586188047891E-16 ) ) ;
#7944 = CARTESIAN_POINT ( 'NONE',  ( 83.93595989616819963, -44.26186973806559877, -46.83273212233100224 ) ) ;
#7945 = CARTESIAN_POINT ( 'NONE',  ( 63.80708344237820739, 1.446931645112450093, -69.41713212316639670 ) ) ;
#7946 = CARTESIAN_POINT ( 'NONE',  ( 19.01438204251930131, -7.890533027083360018, -39.12126593359850091 ) ) ;
#7947 = ORIENTED_EDGE ( 'NONE', *, *, #40761, .T. ) ;
#7948 = CARTESIAN_POINT ( 'NONE',  ( 56.00515889221910015, -46.65902915747689406, -26.31855334364909993 ) ) ;
#7949 = CARTESIAN_POINT ( 'NONE',  ( 15.67956920600099835, -50.86263546383059975, -20.20255632743579710 ) ) ;
#7950 = CARTESIAN_POINT ( 'NONE',  ( 76.63910079429579980, 12.04342629570849965, -14.20152708415839982 ) ) ;
#7951 = B_SPLINE_CURVE_WITH_KNOTS ( 'NONE', 3,
 ( #24134, #8452, #32510, #4505, #11615, #20475, #27580, #36466, #28085, #78, #12127, #24659, #44090, #12377 ),
 .UNSPECIFIED., .F., .F.,
 ( 4, 2, 2, 2, 2, 2, 4 ),
 ( -0.2176222735790200036, -0.2170920924270339780, -0.1934197942039800056, -0.1709809187548010090, -0.1448153107580100185, -0.1239068615272080065, -0.1078515919262239969 ),
 .UNSPECIFIED. ) ;
#7952 = DIRECTION ( 'NONE',  ( 1.000000000000000000, 0.000000000000000000, 0.000000000000000000 ) ) ;
#7953 = CARTESIAN_POINT ( 'NONE',  ( 12.53567563011250030, -49.97757164388899298, -21.12174283345060388 ) ) ;
#7954 = ORIENTED_EDGE ( 'NONE', *, *, #28555, .F. ) ;
#7955 = CARTESIAN_POINT ( 'NONE',  ( -6.906523692131460557, -46.00570557808070049, -5.490002812737249549 ) ) ;
#7956 = CARTESIAN_POINT ( 'NONE',  ( 8.222412332301150428, -15.61630761206940043, -38.79233150823699816 ) ) ;
#7957 = ADVANCED_FACE ( 'NONE', ( #28904 ), #40451, .T. ) ;
#7958 = CARTESIAN_POINT ( 'NONE',  ( 16.13393739769620083, -15.61618894467929941, 7.944363289481099599 ) ) ;
#7959 = CARTESIAN_POINT ( 'NONE',  ( 63.19978792402569923, 1.187415670095769871, -62.40340069948359769 ) ) ;
#7960 = CARTESIAN_POINT ( 'NONE',  ( 57.37407586127599757, -50.61618894467930119, -53.92464312453480346 ) ) ;
#7961 = CARTESIAN_POINT ( 'NONE',  ( 41.98453335044129631, 12.86081823404789937, -4.765379570853959912 ) ) ;
#7962 = CARTESIAN_POINT ( 'NONE',  ( 10.22109577499819366, -19.02429973287621578, -65.28615391924572009 ) ) ;
#7963 = CARTESIAN_POINT ( 'NONE',  ( 63.94990637464879768, 1.033013263524900083, -61.34874638836249972 ) ) ;
#7964 = CARTESIAN_POINT ( 'NONE',  ( 8.222937397696199469, -15.61618894467929941, -32.14999999999999858 ) ) ;
#7965 = LINE ( 'NONE', #36247, #51571 ) ;
#7966 = ADVANCED_FACE ( 'NONE', ( #8748 ), #46370, .T. ) ;
#7967 = CARTESIAN_POINT ( 'NONE',  ( 66.65424812453399284, -1.319067908241720044, -16.99686718764349891 ) ) ;
#7968 = CARTESIAN_POINT ( 'NONE',  ( 17.30873035729209874, -52.95108609461500748, -76.14999999999999147 ) ) ;
#7969 = EDGE_CURVE ( 'NONE', #32053, #51550, #26980, .T. ) ;
#7970 = CARTESIAN_POINT ( 'NONE',  ( 20.43992966667520150, -9.536293804314230016, -62.76349517163679081 ) ) ;
#7971 = CARTESIAN_POINT ( 'NONE',  ( 47.13393739769619373, 8.048130187719140238, -35.08812023096459853 ) ) ;
#7972 = CARTESIAN_POINT ( 'NONE',  ( 63.29963954055089914, 0.9577391936096369962, -62.09594281269529858 ) ) ;
#7973 = VERTEX_POINT ( 'NONE', #27164 ) ;
#7974 = CARTESIAN_POINT ( 'NONE',  ( 22.13834065091210235, -54.14192202099170004, -35.04035092416999220 ) ) ;
#7975 = CARTESIAN_POINT ( 'NONE',  ( 22.48775426134280409, -18.03232780092622889, -34.56855001936997240 ) ) ;
#7976 = CARTESIAN_POINT ( 'NONE',  ( 9.438650519103310543, -12.51186047500710075, -81.23899999999999011 ) ) ;
#7977 = VERTEX_POINT ( 'NONE', #39235 ) ;
#7978 = CARTESIAN_POINT ( 'NONE',  ( 17.47783027489900221, 21.13934752900200209, -76.01805773991210913 ) ) ;
#7979 = VERTEX_POINT ( 'NONE', #32300 ) ;
#7980 = B_SPLINE_CURVE_WITH_KNOTS ( 'NONE', 3,
 ( #4860, #16647, #16132, #8541, #48633, #8794, #12734, #36295, #44690, #32091, #44433, #48111, #20304, #24484, #12210, #27919 ),
 .UNSPECIFIED., .F., .F.,
 ( 4, 2, 2, 2, 2, 2, 2, 4 ),
 ( 0.000000000000000000, 0.1775000002334429783, 0.3375000001880322786, 0.4375000001596504040, 0.5000000001419118156, 0.6250000001064347499, 0.8250000000496718888, 1.000000000000000000 ),
 .UNSPECIFIED. ) ;
#7981 = EDGE_LOOP ( 'NONE', ( #8489, #37777, #51281, #13973, #31288 ) ) ;
#7982 = CYLINDRICAL_SURFACE ( 'NONE', #16016, 6.766999999999998572 ) ;
#7983 = CARTESIAN_POINT ( 'NONE',  ( 21.80530958182080070, -10.16180299264429898, -81.23899999999999011 ) ) ;
#7984 = CARTESIAN_POINT ( 'NONE',  ( 9.807863175385746146, -10.75439414787492609, -73.00066484403033940 ) ) ;
#7985 = VERTEX_POINT ( 'NONE', #44131 ) ;
#7986 = EDGE_CURVE ( 'NONE', #46545, #677, #8228, .T. ) ;
#7987 = CARTESIAN_POINT ( 'NONE',  ( 10.96668629868492317, -20.41640511211885212, -35.60889570735550080 ) ) ;
#7988 = ORIENTED_EDGE ( 'NONE', *, *, #34222, .F. ) ;
#7989 = DIRECTION ( 'NONE',  ( -1.000000000000000000, -5.367253113454777116E-16, 0.000000000000000000 ) ) ;
#7990 = AXIS2_PLACEMENT_3D ( 'NONE', #10131, #6200, #14572 ) ;
#7991 = CARTESIAN_POINT ( 'NONE',  ( 15.53930990683061353, -38.18416678424433286, 4.943674098299959851 ) ) ;
#7992 = ORIENTED_EDGE ( 'NONE', *, *, #12770, .F. ) ;
#7993 = VERTEX_POINT ( 'NONE', #4289 ) ;
#7994 = CARTESIAN_POINT ( 'NONE',  ( 44.67095740009779803, 1.932267065267109896, -44.63214371738488495 ) ) ;
#7995 = CARTESIAN_POINT ( 'NONE',  ( 50.95179065782230055, -50.95087911780539969, -76.14999999969799660 ) ) ;
#7996 = CARTESIAN_POINT ( 'NONE',  ( 61.02187414602389737, 14.32404985249469931, -47.57273269190739740 ) ) ;
#7997 = CARTESIAN_POINT ( 'NONE',  ( 10.37507727206246244, -11.93657929354967528, -39.63413252511316642 ) ) ;
#7998 = DIRECTION ( 'NONE',  ( 0.000000000000000000, 0.000000000000000000, -1.000000000000000000 ) ) ;
#7999 = CARTESIAN_POINT ( 'NONE',  ( -10.45107869171170023, 11.54332210424730043, -5.993506745208079245 ) ) ;
#8001 = VECTOR ( 'NONE', #8358, 1000.000000000000114 ) ;
#8000 = CARTESIAN_POINT ( 'NONE',  ( 0.9261640637186691061, -22.54594764139109841, -34.65800258959599489 ) ) ;
#8002 = CARTESIAN_POINT ( 'NONE',  ( 58.55928041488670033, 14.25308721433460057, -26.37445203316179843 ) ) ;
#8003 = CARTESIAN_POINT ( 'NONE',  ( 23.95544421880619979, -14.97526833297029825, -67.26148035172319339 ) ) ;
#8004 = VERTEX_POINT ( 'NONE', #36252 ) ;
#8005 = FACE_OUTER_BOUND ( 'NONE', #21110, .T. ) ;
#8006 = CARTESIAN_POINT ( 'NONE',  ( 42.86745194688189997, 14.71797365073330077, -7.481799581053440562 ) ) ;
#8007 = CARTESIAN_POINT ( 'NONE',  ( 53.68563787866792580, -51.14635906356087958, -75.73808238357163702 ) ) ;
#8008 = UNCERTAINTY_MEASURE_WITH_UNIT (LENGTH_MEASURE( 1.000000000000000082E-05 ), #10591, 'distance_accuracy_value', 'NONE');
#8009 = CARTESIAN_POINT ( 'NONE',  ( 72.65443274204099566, 1.179532368575559875, -69.54928105623400825 ) ) ;
#8010 = CARTESIAN_POINT ( 'NONE',  ( 43.33491147696511092, -39.89712550726049756, -69.87957685626012960 ) ) ;
#8011 = CARTESIAN_POINT ( 'NONE',  ( 16.13393739769620083, -15.61618894467929941, -81.23899999999999011 ) ) ;
#8012 = CIRCLE ( 'NONE', #37317, 2.000000000000001332 ) ;
#8013 = CARTESIAN_POINT ( 'NONE',  ( 46.46257346985409953, 21.93137764140289647, -76.13734532152261636 ) ) ;
#8014 = CARTESIAN_POINT ( 'NONE',  ( 48.72323709853730378, -54.03203391146720236, -54.90603619288649639 ) ) ;
#8015 = AXIS2_PLACEMENT_3D ( 'NONE', #34431, #14528, #15309 ) ;
#8016 = DIRECTION ( 'NONE',  ( 1.000000000000000000, 0.000000000000000000, 0.000000000000000000 ) ) ;
#8017 = ADVANCED_FACE ( 'NONE', ( #612, #363 ), #24436, .T. ) ;
#8018 = CARTESIAN_POINT ( 'NONE',  ( 16.15069188244332210, 19.81939201856824795, -15.66900176635303232 ) ) ;
#8019 = CARTESIAN_POINT ( 'NONE',  ( 66.28197446254964120, -33.07501703851021091, -19.91060653315744489 ) ) ;
#8020 = CARTESIAN_POINT ( 'NONE',  ( 75.13393739769618662, -43.11618894467930119, -84.38499399519520239 ) ) ;
#8021 = EDGE_CURVE ( 'NONE', #21139, #17894, #27632, .T. ) ;
#8022 = EDGE_LOOP ( 'NONE', ( #27028, #49122, #2074, #50350 ) ) ;
#8023 = CARTESIAN_POINT ( 'NONE',  ( 16.34294028551579814, -22.66593182482080238, -79.33774565447309612 ) ) ;
#8024 = LINE ( 'NONE', #12471, #25733 ) ;
#8025 = ORIENTED_EDGE ( 'NONE', *, *, #30989, .T. ) ;
#8026 = CYLINDRICAL_SURFACE ( 'NONE', #21689, 2.000000000000040856 ) ;
#8027 = CARTESIAN_POINT ( 'NONE',  ( 60.95366616844789576, -45.42739688593400160, -47.19077871656730139 ) ) ;
#8028 = CARTESIAN_POINT ( 'NONE',  ( 56.51601257069349771, -47.72958752039729546, -47.92267345016619373 ) ) ;
#8029 = CARTESIAN_POINT ( 'NONE',  ( 47.40322300430459990, 23.42336669154519768, -54.88279555090589668 ) ) ;
#8031 = CARTESIAN_POINT ( 'NONE',  ( 20.99565638127380041, -9.290056386383136910, -35.50066289986691004 ) ) ;
#8030 = CARTESIAN_POINT ( 'NONE',  ( 42.48761169368059853, 8.583421331073370908, -73.97586456252511766 ) ) ;
#8032 = LINE ( 'NONE', #23983, #25954 ) ;
#8033 = DIRECTION ( 'NONE',  ( 1.000000000000000000, 0.000000000000000000, 0.000000000000000000 ) ) ;
#8034 = VERTEX_POINT ( 'NONE', #18155 ) ;
#8035 = CARTESIAN_POINT ( 'NONE',  ( 48.82567944625920120, -28.11618896394480061, -15.64999999241030082 ) ) ;
#8036 = ORIENTED_EDGE ( 'NONE', *, *, #15517, .T. ) ;
#8037 = B_SPLINE_CURVE_WITH_KNOTS ( 'NONE', 3,
 ( #5254, #1314, #9694, #29592, #8656 ),
 .UNSPECIFIED., .F., .F.,
 ( 4, 1, 4 ),
 ( 0.000000000000000000, 0.5000000000000000000, 1.000000000000000000 ),
 .UNSPECIFIED. ) ;
#8038 = ORIENTED_EDGE ( 'NONE', *, *, #9938, .T. ) ;
#8039 = CARTESIAN_POINT ( 'NONE',  ( 12.24635195013770073, -21.50085024014760293, -59.53301288856830098 ) ) ;
#8040 = CARTESIAN_POINT ( 'NONE',  ( 12.14984766995591059, -8.703642186092894306, -79.12566561758120542 ) ) ;
#8041 = CARTESIAN_POINT ( 'NONE',  ( 76.39902651674920264, -19.28652455383290132, -12.79235177570935456 ) ) ;
#8042 = CARTESIAN_POINT ( 'NONE',  ( 52.50031725165329988, -52.44384906523560375, -54.11907245731389793 ) ) ;
#8043 = CIRCLE ( 'NONE', #10566, 11.00000000000000000 ) ;
#8044 = ORIENTED_EDGE ( 'NONE', *, *, #31202, .T. ) ;
#8045 = ORIENTED_EDGE ( 'NONE', *, *, #31199, .F. ) ;
#8046 = EDGE_CURVE ( 'NONE', #36938, #12364, #30683, .T. ) ;
#8047 = DIRECTION ( 'NONE',  ( 0.000000000000000000, 0.000000000000000000, -1.000000000000000000 ) ) ;
#8048 = B_SPLINE_CURVE_WITH_KNOTS ( 'NONE', 3,
 ( #1229, #46501, #26291, #6655, #4899, #50158, #21129, #44995, #36868, #33178, #9095, #22358, #37130, #42563, #9363, #25312, #34672, #41314, #6399, #17218, #5174, #14255, #29249, #49200, #17473, #14512, #30223, #40796, #10330, #22615, #46243, #5425, #42300, #50673, #10593, #967, #20867, #38362, #21382, #2455, #18435, #18695, #45258, #38630, #16966, #26547, #13292 ),
 .UNSPECIFIED., .F., .F.,
 ( 4, 2, 2, 2, 2, 2, 2, 1, 1, 1, 2, 2, 2, 2, 2, 2, 2, 1, 1, 1, 1, 2, 2, 2, 2, 2, 4 ),
 ( 0.5000059655526006841, 0.5312555927055534477, 0.5625052198585062113, 0.5937548470114590859, 0.6093796605879354678, 0.6171920673761737142, 0.6210982707702927819, 0.6230513724673523157, 0.6240279233158819716, 0.6245161987401469661, 0.6247603364522794633, 0.6250044741644119606, 0.6562541013173609494, 0.6875037284703100493, 0.7187533556232591492, 0.7343781691997335326, 0.7421905759879710018, 0.7460967793820898475, 0.7480498810791493813, 0.7490264319276790372, 0.7495147073519436987, 0.7497588450640761959, 0.7500029827762088042, 0.8125022370821566309, 0.8750014913881043466, 0.9375007456940522843, 1.000000000000000000 ),
 .UNSPECIFIED. ) ;
#8049 = AXIS2_PLACEMENT_3D ( 'NONE', #47733, #35146, #39607 ) ;
#8050 = CARTESIAN_POINT ( 'NONE',  ( -22.40773940430613109, -9.428819728254625332, -54.48440151228250983 ) ) ;
#8051 = CARTESIAN_POINT ( 'NONE',  ( 56.48750829591079992, -50.75384514585400098, -53.61740582762440255 ) ) ;
#8052 = CARTESIAN_POINT ( 'NONE',  ( 52.67900408153330005, -49.77440099653090044, -48.75317613627849767 ) ) ;
#8053 = CARTESIAN_POINT ( 'NONE',  ( 22.86958133952598615, -14.94427170521152881, -46.42118020533612111 ) ) ;
#8054 = EDGE_CURVE ( 'NONE', #12711, #1664, #43846, .T. ) ;
#8055 = CARTESIAN_POINT ( 'NONE',  ( 59.03458116493130348, -2.378454724218949767, -15.69068937066560032 ) ) ;
#8056 = PRODUCT_DEFINITION_SHAPE ( 'NONE', 'NONE',  #51875 ) ;
#8057 =( BOUNDED_CURVE ( )  B_SPLINE_CURVE ( 2, ( #3030, #14823, #27127 ),
 .UNSPECIFIED., .F., .T. ) 
 B_SPLINE_CURVE_WITH_KNOTS ( ( 3, 3 ),
 ( 1.923142637343010053, 4.853851569643779840 ),
 .UNSPECIFIED. ) 
 CURVE ( )  GEOMETRIC_REPRESENTATION_ITEM ( )  RATIONAL_B_SPLINE_CURVE ( ( 1.003436844930060134, 1.004455541115540029, 1.000597593688330011 ) ) 
 REPRESENTATION_ITEM ( '' )  );
#8058 = EDGE_LOOP ( 'NONE', ( #2509, #6908, #36852, #35547 ) ) ;
#8059 = DIRECTION ( 'NONE',  ( 0.000000000000000000, 0.000000000000000000, -1.000000000000000000 ) ) ;
#8060 = CARTESIAN_POINT ( 'NONE',  ( 53.27342897376659892, -50.46946016740059804, -77.09451958621460221 ) ) ;
#8061 = CARTESIAN_POINT ( 'NONE',  ( 64.68608103367601814, 0.9036513197889380899, -70.56049771322830111 ) ) ;
#8062 = FACE_OUTER_BOUND ( 'NONE', #51432, .T. ) ;
#8063 = CIRCLE ( 'NONE', #13892, 5.461610137242769447 ) ;
#8064 = CARTESIAN_POINT ( 'NONE',  ( 8.486932887716839957, -17.37972789121199924, -52.94034771974808962 ) ) ;
#8065 = CIRCLE ( 'NONE', #41534, 15.24604989415149703 ) ;
#8066 = CARTESIAN_POINT ( 'NONE',  ( 13.68260753953069830, -50.61260876938109732, -21.30691141874990180 ) ) ;
#8067 = DIRECTION ( 'NONE',  ( 1.224646799147353207E-16, 1.000000000000000000, -0.000000000000000000 ) ) ;
#8068 = DIRECTION ( 'NONE',  ( -1.000000000000000000, 0.000000000000000000, 0.000000000000000000 ) ) ;
#8069 = CARTESIAN_POINT ( 'NONE',  ( 56.78179639309170312, 13.88381105532070059, -15.59568127148789962 ) ) ;
#8070 = CARTESIAN_POINT ( 'NONE',  ( 60.75158972514669387, -45.53853088870819477, -47.32592394361339672 ) ) ;
#8071 = LINE ( 'NONE', #24016, #37981 ) ;
#8072 = CARTESIAN_POINT ( 'NONE',  ( 13.83887629744999970, -22.28516590674690079, -51.45268192007920049 ) ) ;
#8073 = CARTESIAN_POINT ( 'NONE',  ( 18.20470410219303403, -7.911113479266316695, -41.37566450579876687 ) ) ;
#8074 = ORIENTED_EDGE ( 'NONE', *, *, #26592, .T. ) ;
#8075 = CARTESIAN_POINT ( 'NONE',  ( 47.06135413716880578, 22.56673458592310055, -75.82639806884090206 ) ) ;
#8076 = AXIS2_PLACEMENT_3D ( 'NONE', #26833, #15046, #19488 ) ;
#8077 = CARTESIAN_POINT ( 'NONE',  ( 47.34394088935550116, -54.69230464071289788, -54.81224997073749705 ) ) ;
#8078 = CARTESIAN_POINT ( 'NONE',  ( -4.666062602303798990, -15.61618894467930119, -12.65000000000000036 ) ) ;
#8079 = CARTESIAN_POINT ( 'NONE',  ( 5.741632552282960766, -9.616188944679340267, -22.14999999999999858 ) ) ;
#8080 = CARTESIAN_POINT ( 'NONE',  ( 16.13393739769620083, -15.61618894467929941, -28.45282021618999835 ) ) ;
#8081 = CARTESIAN_POINT ( 'NONE',  ( 60.91226570742461632, -45.44496133806553217, -47.18149654191857678 ) ) ;
#8082 = AXIS2_PLACEMENT_3D ( 'NONE', #14393, #15943, #42963 ) ;
#8083 = CARTESIAN_POINT ( 'NONE',  ( 47.26511662130825897, -54.05680164242729546, -75.56574662652583640 ) ) ;
#8084 = CARTESIAN_POINT ( 'NONE',  ( 10.72320681404810117, 33.67578529855150293, -17.84617904793899967 ) ) ;
#8085 = DIRECTION ( 'NONE',  ( -0.8133188816852104930, 0.000000000000000000, -0.5818181818182710519 ) ) ;
#8087 = CARTESIAN_POINT ( 'NONE',  ( 9.221436020990983806, -19.60035757305728410, -52.62566441095005842 ) ) ;
#8086 = CARTESIAN_POINT ( 'NONE',  ( 16.13393739769620083, -15.61618894467929941, 1.600000000000000089 ) ) ;
#8088 = ADVANCED_FACE ( 'NONE', ( #5343 ), #29164, .T. ) ;
#8089 = CYLINDRICAL_SURFACE ( 'NONE', #49365, 2.576499999999998902 ) ;
#8090 = CYLINDRICAL_SURFACE ( 'NONE', #19601, 2.000000000000001776 ) ;
#8091 = CARTESIAN_POINT ( 'NONE',  ( 49.30929069640199458, 22.32182524534569978, -54.21028152426279689 ) ) ;
#8092 = ORIENTED_EDGE ( 'NONE', *, *, #37210, .F. ) ;
#8093 = CARTESIAN_POINT ( 'NONE',  ( 52.90147003455390262, -49.64573303326979214, -48.94440827424179474 ) ) ;
#8094 = ORIENTED_EDGE ( 'NONE', *, *, #1565, .F. ) ;
#8095 = CARTESIAN_POINT ( 'NONE',  ( 41.63907510861591987, 6.190619291336893149, -82.10713965745907217 ) ) ;
#8096 = AXIS2_PLACEMENT_3D ( 'NONE', #22893, #14531, #46264 ) ;
#8097 = DIRECTION ( 'NONE',  ( -1.000000000000000000, 0.000000000000000000, 0.000000000000000000 ) ) ;
#8098 = DIRECTION ( 'NONE',  ( 0.000000000000000000, 0.000000000000000000, -1.000000000000000000 ) ) ;
#8100 = CARTESIAN_POINT ( 'NONE',  ( 52.95630170018949912, 18.21339351390729888, -27.21371790733410023 ) ) ;
#8099 = CARTESIAN_POINT ( 'NONE',  ( 83.86651039750330483, 13.16223578792310001, -46.90523421348220268 ) ) ;
#8101 = CARTESIAN_POINT ( 'NONE',  ( 23.18661920690770017, -15.56888149661560128, -58.45068511312169335 ) ) ;
#8102 = CARTESIAN_POINT ( 'NONE',  ( 52.84346299185870066, 18.45884386080550144, -48.96941050064629763 ) ) ;
#8103 = CARTESIAN_POINT ( 'NONE',  ( 56.87281233921919466, -45.18115549338420323, -17.04514278619280176 ) ) ;
#8104 = CARTESIAN_POINT ( 'NONE',  ( 54.52192486798780635, 16.42131495964800436, -25.85211914981980286 ) ) ;
#8105 = ORIENTED_EDGE ( 'NONE', *, *, #4960, .F. ) ;
#8106 = CARTESIAN_POINT ( 'NONE',  ( 22.36052287337500033, -20.39283855473529883, -43.49580103263740227 ) ) ;
#8107 = ORIENTED_EDGE ( 'NONE', *, *, #36141, .F. ) ;
#8108 = CARTESIAN_POINT ( 'NONE',  ( 10.91696776951759951, -65.00855143979499928, -17.52451585372379839 ) ) ;
#8109 = CARTESIAN_POINT ( 'NONE',  ( 11.15097258569349847, 33.37846234896409925, -45.98097165681439691 ) ) ;
#8110 = CARTESIAN_POINT ( 'NONE',  ( 34.13393739769620083, -15.61618894467929941, -20.58999999999999986 ) ) ;
#8111 = CARTESIAN_POINT ( 'NONE',  ( 53.08619397177870525, -49.46320494400659840, -48.78329442807490324 ) ) ;
#8112 = CARTESIAN_POINT ( 'NONE',  ( 11.42100611455456871, -65.27489793864438639, -22.73641203297022884 ) ) ;
#8113 = DIRECTION ( 'NONE',  ( 0.05023550054956202326, 0.000000000000000000, -0.9987374001630934250 ) ) ;
#8114 = ORIENTED_EDGE ( 'NONE', *, *, #49145, .F. ) ;
#8115 = CARTESIAN_POINT ( 'NONE',  ( 9.221344252930924412, -11.63217719309666975, -74.67431699540968282 ) ) ;
#8116 = CARTESIAN_POINT ( 'NONE',  ( 11.13393739769619906, -63.28004284733241036, -43.74619111847169961 ) ) ;
#8117 = CARTESIAN_POINT ( 'NONE',  ( 68.13393739769814772, 19.38381105532029736, -71.50000000000200373 ) ) ;
#8118 = ORIENTED_EDGE ( 'NONE', *, *, #32660, .F. ) ;
#8119 = EDGE_CURVE ( 'NONE', #35503, #34565, #41487, .T. ) ;
#8120 = DIRECTION ( 'NONE',  ( 0.000000000000000000, 0.000000000000000000, -1.000000000000000000 ) ) ;
#8121 = CARTESIAN_POINT ( 'NONE',  ( 56.50450790981899729, 19.50659178549170036, -53.50133212754479928 ) ) ;
#8122 = DIRECTION ( 'NONE',  ( 1.000000000000000000, 0.000000000000000000, 0.000000000000000000 ) ) ;
#8123 = CARTESIAN_POINT ( 'NONE',  ( 23.45932441199935425, -12.52460061254321388, -49.38066021020333807 ) ) ;
#8124 = ORIENTED_EDGE ( 'NONE', *, *, #25888, .F. ) ;
#8125 = CARTESIAN_POINT ( 'NONE',  ( 15.09834424264556318, -23.52718342601810519, -62.33399675319203936 ) ) ;
#8126 = CARTESIAN_POINT ( 'NONE',  ( 10.13393739769589885, 22.91950879131600161, -35.09469305598949518 ) ) ;
#8128 = CARTESIAN_POINT ( 'NONE',  ( 56.95883376355960337, -50.25507440355580258, -52.69722347720740174 ) ) ;
#8127 = AXIS2_PLACEMENT_3D ( 'NONE', #28885, #24937, #29408 ) ;
#8129 = CARTESIAN_POINT ( 'NONE',  ( 2.434269054290299827, -25.76645817901039948, -34.90839531524130024 ) ) ;
#8130 = CARTESIAN_POINT ( 'NONE',  ( 10.24496007140159826, -21.38703515708219882, -78.54555634383700635 ) ) ;
#8131 = DIRECTION ( 'NONE',  ( -0.000000000000000000, 1.000000000000000000, 0.000000000000000000 ) ) ;
#8132 = CARTESIAN_POINT ( 'NONE',  ( 16.13393739769620083, -15.61618894467929941, -54.64999999999999858 ) ) ;
#8133 = ORIENTED_EDGE ( 'NONE', *, *, #6143, .F. ) ;
#8134 = CARTESIAN_POINT ( 'NONE',  ( 8.969861584858589865, -13.57102109018409841, -69.32117255937750144 ) ) ;
#8135 = AXIS2_PLACEMENT_3D ( 'NONE', #42653, #47112, #30571 ) ;
#8136 = CARTESIAN_POINT ( 'NONE',  ( 68.13393739771808555, -29.66618894456289723, -82.15000000031059812 ) ) ;
#8137 = CARTESIAN_POINT ( 'NONE',  ( 10.44026233180520080, -20.79788605865429929, -32.14999999999999858 ) ) ;
#8138 = CARTESIAN_POINT ( 'NONE',  ( 46.53489442956319522, 22.05800845228959872, -76.11277936651509890 ) ) ;
#8139 = FACE_OUTER_BOUND ( 'NONE', #32501, .T. ) ;
#8141 = B_SPLINE_CURVE_WITH_KNOTS ( 'NONE', 3,
 ( #48577, #20507, #36757, #33077, #32810, #44122, #28895, #25216, #44897, #28632, #9004, #1391, #28373, #1129, #12408, #44380, #44633, #24947, #40958, #48836 ),
 .UNSPECIFIED., .F., .F.,
 ( 4, 2, 2, 2, 2, 2, 2, 2, 2, 4 ),
 ( 0.000000000000000000, 0.08842663233499932496, 0.2261948956690018608, 0.3750000000000019984, 0.5000000000000005551, 0.5625000000000008882, 0.6625000000000003109, 0.7983826544665608704, 0.9363829142900766955, 1.000000000000000000 ),
 .UNSPECIFIED. ) ;
#8140 = PRODUCT_RELATED_PRODUCT_CATEGORY ( 'part', '', ( #22363 ) ) ;
#8142 = FACE_OUTER_BOUND ( 'NONE', #16654, .T. ) ;
#8143 = CARTESIAN_POINT ( 'NONE',  ( 12.10858429747900011, 33.61313455612010159, -16.12611387918660100 ) ) ;
#8144 = CARTESIAN_POINT ( 'NONE',  ( 15.36781655846439953, -23.82568220362479749, -76.03728780924519981 ) ) ;
#8145 = CARTESIAN_POINT ( 'NONE',  ( 54.27570680556749494, -50.62601669679319372, -76.71275195964710747 ) ) ;
#8147 = FACE_OUTER_BOUND ( 'NONE', #29085, .T. ) ;
#8146 = CARTESIAN_POINT ( 'NONE',  ( 71.33393739769628894, 10.88381105532070059, -69.84999999999999432 ) ) ;
#8148 = EDGE_CURVE ( 'NONE', #19682, #19506, #39698, .T. ) ;
#8149 = CARTESIAN_POINT ( 'NONE',  ( 63.06393505168800573, 0.8850831926798630178, -68.85873448833339694 ) ) ;
#8150 = CARTESIAN_POINT ( 'NONE',  ( 61.27465791697959929, 14.01526204812190102, -46.81188391966050233 ) ) ;
#8151 = CARTESIAN_POINT ( 'NONE',  ( 72.38393739883420608, 4.883811055320659733, -61.44999999999999574 ) ) ;
#8152 = ADVANCED_FACE ( 'NONE', ( #1398 ), #21816, .T. ) ;
#8153 = ORIENTED_EDGE ( 'NONE', *, *, #38277, .F. ) ;
#8154 = CARTESIAN_POINT ( 'NONE',  ( 53.01963658129270129, -49.56143686301879825, -48.79855610848599667 ) ) ;
#8155 = ADVANCED_FACE ( 'NONE', ( #9276 ), #6368, .T. ) ;
#8156 = CARTESIAN_POINT ( 'NONE',  ( 57.62794015340739406, -45.42613097097460439, -26.09739812807309889 ) ) ;
#8157 = CARTESIAN_POINT ( 'NONE',  ( 20.24725285149263598, -22.43897999005509547, -66.11977884462595512 ) ) ;
#8158 = CARTESIAN_POINT ( 'NONE',  ( 57.07496343321250265, 14.26128913866610048, -26.05062655201860267 ) ) ;
#8159 = CARTESIAN_POINT ( 'NONE',  ( 16.71323853210260069, -8.188463586211829792, -73.75743269894009302 ) ) ;
#8160 = EDGE_CURVE ( 'NONE', #51641, #18232, #25224, .T. ) ;
#8161 = CARTESIAN_POINT ( 'NONE',  ( 50.55764111442330488, 18.57534966417999911, -76.16355215269059897 ) ) ;
#8162 = CARTESIAN_POINT ( 'NONE',  ( 53.04305184480200097, 18.31989923538939991, -48.87083722090200411 ) ) ;
#8163 = CARTESIAN_POINT ( 'NONE',  ( 71.04878173523039209, 1.375383258925270136, -70.44587820682191648 ) ) ;
#8164 = FACE_OUTER_BOUND ( 'NONE', #41040, .T. ) ;
#8165 = EDGE_LOOP ( 'NONE', ( #2581, #21411, #43327, #36202 ) ) ;
#8166 = CARTESIAN_POINT ( 'NONE',  ( 9.205734167420720482, -3.616188944679329609, -24.14999999999999858 ) ) ;
#8167 = CARTESIAN_POINT ( 'NONE',  ( 47.69978268171949765, -54.49413833317590417, -54.91276148295600734 ) ) ;
#8168 = CARTESIAN_POINT ( 'NONE',  ( -9.468778083922810396, 12.47338336450459906, -5.557361636894910362 ) ) ;
#8169 = CARTESIAN_POINT ( 'NONE',  ( 36.93393739717168245, -15.61618894541809688, -10.44999999999999929 ) ) ;
#8170 = CARTESIAN_POINT ( 'NONE',  ( 65.26406672541840237, -31.36357188815229335, -16.98112372788800073 ) ) ;
#8171 = CARTESIAN_POINT ( 'NONE',  ( 71.44620697304119972, 0.9254905997697669973, -60.64710470602509673 ) ) ;
#8172 = CARTESIAN_POINT ( 'NONE',  ( 2.543036500622910090, -25.25580902796040306, -34.65032322548090349 ) ) ;
#8173 = CARTESIAN_POINT ( 'NONE',  ( 72.09652352821250076, 1.406831506490820116, -61.37777621199789735 ) ) ;
#8174 = AXIS2_PLACEMENT_3D ( 'NONE', #49697, #49953, #21621 ) ;
#8175 = DIRECTION ( 'NONE',  ( 1.590235242698480059E-09, 2.885242803146169796E-09, 1.000000000000000000 ) ) ;
#8176 = CARTESIAN_POINT ( 'NONE',  ( 65.17314292416639887, 1.382830464309369844, -70.35440931850220636 ) ) ;
#8177 = ORIENTED_EDGE ( 'NONE', *, *, #15915, .T. ) ;
#8178 = EDGE_LOOP ( 'NONE', ( #9330, #134, #20217, #30529 ) ) ;
#8179 = CARTESIAN_POINT ( 'NONE',  ( 8.428814366912718015, -13.54559301151024719, -54.87566131310629203 ) ) ;
#8180 = CIRCLE ( 'NONE', #39157, 1.000000000000000888 ) ;
#8181 = CARTESIAN_POINT ( 'NONE',  ( 20.29260965567053887, -21.02750684390549907, -58.74448668235789484 ) ) ;
#8182 = VERTEX_POINT ( 'NONE', #13469 ) ;
#8183 = ADVANCED_FACE ( 'NONE', ( #29424 ), #16733, .T. ) ;
#8184 = CARTESIAN_POINT ( 'NONE',  ( 56.18863030598410546, -45.60033839361480545, -25.30081866445960159 ) ) ;
#8185 = CARTESIAN_POINT ( 'NONE',  ( 0.3209249304026170480, -15.61618894467929941, -35.14999999999999858 ) ) ;
#8186 = ORIENTED_EDGE ( 'NONE', *, *, #42182, .F. ) ;
#8187 = DIRECTION ( 'NONE',  ( 0.000000000000000000, -1.000000000000000000, 0.000000000000000000 ) ) ;
#8188 = CARTESIAN_POINT ( 'NONE',  ( 42.51832970315865623, 6.473372013560068083, -77.72799465092199966 ) ) ;
#8189 = CARTESIAN_POINT ( 'NONE',  ( 24.03992025865239768, -15.92081808833121670, -65.51992199243797188 ) ) ;
#8190 = CARTESIAN_POINT ( 'NONE',  ( 15.11686583926219996, -7.433995748417090432, -39.25296653628179655 ) ) ;
#8191 = CARTESIAN_POINT ( 'NONE',  ( 16.13393739769620083, -15.61618894467929941, -18.35000000000000142 ) ) ;
#8192 = CARTESIAN_POINT ( 'NONE',  ( 22.53432111889044975, -20.33647081035346105, -49.99467920166775059 ) ) ;
#8193 = ORIENTED_EDGE ( 'NONE', *, *, #26950, .F. ) ;
#8194 = B_SPLINE_CURVE_WITH_KNOTS ( 'NONE', 3,
 ( #4716, #4202, #28552, #40878, #48231, #4982 ),
 .UNSPECIFIED., .F., .F.,
 ( 4, 2, 4 ),
 ( 0.1924323111301881328, 0.5962161555650941080, 1.000000000000000000 ),
 .UNSPECIFIED. ) ;
#8195 = CARTESIAN_POINT ( 'NONE',  ( 11.82388200435210024, -65.03973971535801013, -23.85088417817880213 ) ) ;
#8196 = CARTESIAN_POINT ( 'NONE',  ( 21.24986970212820125, -10.48466363836469917, -31.98264971805809509 ) ) ;
#8197 = ADVANCED_FACE ( 'NONE', ( #21233, #46154 ), #10241, .T. ) ;
#8198 = CARTESIAN_POINT ( 'NONE',  ( 45.22532672935899711, 14.34554167113489953, -8.601054614529550335 ) ) ;
#8199 = CARTESIAN_POINT ( 'NONE',  ( 14.49215175659190002, 20.43782862716600235, -75.53341961486970035 ) ) ;
#8200 = CARTESIAN_POINT ( 'NONE',  ( 17.84154075489263391, -23.41191558886454871, -60.22387759140665509 ) ) ;
#8201 = CARTESIAN_POINT ( 'NONE',  ( 83.91322170983950457, -44.47913769101550230, -47.13452068490819613 ) ) ;
#8202 = TOROIDAL_SURFACE ( 'NONE', #48379, 17.39999999955150045, 3.400000000022779911 ) ;
#8203 = DIRECTION ( 'NONE',  ( 0.000000000000000000, 0.000000000000000000, -1.000000000000000000 ) ) ;
#8204 = CARTESIAN_POINT ( 'NONE',  ( 16.49341532545370015, -23.85351231628670376, -47.99378621272389722 ) ) ;
#8205 = VERTEX_POINT ( 'NONE', #1341 ) ;
#8206 = CARTESIAN_POINT ( 'NONE',  ( 52.75143703161269571, -49.69438780581380399, -27.88778421337200442 ) ) ;
#8207 = CARTESIAN_POINT ( 'NONE',  ( 15.65801254756290106, -50.85536889816550143, -20.25518593351960206 ) ) ;
#8208 = CARTESIAN_POINT ( 'NONE',  ( 50.91918776801460922, -35.36424194159308598, -76.35849960748986121 ) ) ;
#8209 = CARTESIAN_POINT ( 'NONE',  ( 8.222962928588657405, -16.65192332958894994, -64.75066493400071010 ) ) ;
#8210 = CARTESIAN_POINT ( 'NONE',  ( 22.81411325381436228, -16.71917589191833287, -56.50489658860690412 ) ) ;
#8211 = LINE ( 'NONE', #17115, #9771 ) ;
#8212 = EDGE_CURVE ( 'NONE', #51131, #51304, #17331, .T. ) ;
#8213 = ORIENTED_EDGE ( 'NONE', *, *, #38049, .T. ) ;
#8214 = DIRECTION ( 'NONE',  ( -1.000000000000000000, 0.000000000000000000, 0.000000000000000000 ) ) ;
#8215 = CARTESIAN_POINT ( 'NONE',  ( 47.31231821074380406, 23.47848045659210214, -54.67852925653989615 ) ) ;
#8216 = CARTESIAN_POINT ( 'NONE',  ( 10.72267551889550141, -19.77493392430376318, -49.24448729921695644 ) ) ;
#8217 = CARTESIAN_POINT ( 'NONE',  ( 63.45501836690030473, 1.383357884654609959, -62.61405865291869333 ) ) ;
#8218 = CARTESIAN_POINT ( 'NONE',  ( 57.47389180249940921, -50.59199526962510163, -53.60388562653090361 ) ) ;
#8219 = CARTESIAN_POINT ( 'NONE',  ( 42.47447998727660234, 12.94812977345070060, -5.039225366711079346 ) ) ;
#8220 = EDGE_CURVE ( 'NONE', #13785, #36880, #37008, .T. ) ;
#8221 = DIRECTION ( 'NONE',  ( 0.000000000000000000, 0.000000000000000000, -1.000000000000000000 ) ) ;
#8222 = CARTESIAN_POINT ( 'NONE',  ( 24.04493429539773430, -15.60809896981181844, -75.79200058820715924 ) ) ;
#8223 = CARTESIAN_POINT ( 'NONE',  ( 30.68460988201149320, -15.41618894468070344, -28.20067248431509199 ) ) ;
#8224 = CARTESIAN_POINT ( 'NONE',  ( 17.80205609966759894, -52.64324949044360125, -76.02664804518839503 ) ) ;
#8225 = CARTESIAN_POINT ( 'NONE',  ( 23.32430482491550094, 18.10127401595489971, -34.64999999999999858 ) ) ;
#8226 = CARTESIAN_POINT ( 'NONE',  ( 50.15655331733719891, -52.83076837965879946, -53.34591643228289826 ) ) ;
#8227 = ORIENTED_EDGE ( 'NONE', *, *, #28727, .T. ) ;
#8228 = LINE ( 'NONE', #51290, #30432 ) ;
#8229 = CARTESIAN_POINT ( 'NONE',  ( 22.13393739769619728, -54.15188668067469990, -35.14999999999999858 ) ) ;
#8230 = FACE_OUTER_BOUND ( 'NONE', #46324, .T. ) ;
#8231 = CARTESIAN_POINT ( 'NONE',  ( 10.95696251514589825, -10.06216002319020042, -81.23899999999999011 ) ) ;
#8232 = ORIENTED_EDGE ( 'NONE', *, *, #15458, .T. ) ;
#8233 = CARTESIAN_POINT ( 'NONE',  ( 18.12471141111990036, 20.82672717200830093, -75.71427953954510315 ) ) ;
#8234 = ORIENTED_EDGE ( 'NONE', *, *, #13307, .T. ) ;
#8235 = VERTEX_POINT ( 'NONE', #27235 ) ;
#8236 = ADVANCED_FACE ( 'NONE', ( #35365 ), #32135, .T. ) ;
#8237 = CARTESIAN_POINT ( 'NONE',  ( 56.94969803572780620, -45.93464612349889364, -26.24572192374850133 ) ) ;
#8238 = CARTESIAN_POINT ( 'NONE',  ( 21.26232505384869853, -20.42786076864270228, -81.23899999999999011 ) ) ;
#8239 = CARTESIAN_POINT ( 'NONE',  ( 61.60836755608340098, 14.03242982913499937, -47.13168653318339807 ) ) ;
#8240 = AXIS2_PLACEMENT_3D ( 'NONE', #32975, #20666, #41373 ) ;
#8241 = CARTESIAN_POINT ( 'NONE',  ( 66.63393739769620083, -43.11618894467930119, -73.25000000000000000 ) ) ;
#8242 = CARTESIAN_POINT ( 'NONE',  ( 8.815605938724019097, -63.28267558148569094, -46.67186391142220003 ) ) ;
#8243 = VERTEX_POINT ( 'NONE', #50589 ) ;
#8244 = DIRECTION ( 'NONE',  ( 1.000000000000000000, 0.000000000000000000, 0.000000000000000000 ) ) ;
#8245 = CARTESIAN_POINT ( 'NONE',  ( -11.39236625349550103, 2.585530954890270294, -54.64999999999999858 ) ) ;
#8246 = ORIENTED_EDGE ( 'NONE', *, *, #28302, .F. ) ;
#8247 = ORIENTED_EDGE ( 'NONE', *, *, #45330, .T. ) ;
#8248 = CARTESIAN_POINT ( 'NONE',  ( 72.73458218292580568, 1.393731187554809958, -62.48946499964799983 ) ) ;
#8249 = CARTESIAN_POINT ( 'NONE',  ( 11.63826681151173226, -65.39198021151038631, -17.83149674230410398 ) ) ;
#8250 = CARTESIAN_POINT ( 'NONE',  ( 60.94487250823569724, 14.43811055919129949, -47.71586022308749619 ) ) ;
#8251 = EDGE_CURVE ( 'NONE', #24679, #19168, #22782, .T. ) ;
#8252 = EDGE_CURVE ( 'NONE', #48088, #5276, #43075, .T. ) ;
#8253 = CARTESIAN_POINT ( 'NONE',  ( 46.19336502865940020, 14.89804580897780006, -9.780208910710129544 ) ) ;
#8254 = CARTESIAN_POINT ( 'NONE',  ( 40.36721523011259904, -44.88645108045319887, -4.296538310234230273 ) ) ;
#8255 = CARTESIAN_POINT ( 'NONE',  ( -6.415768085208600091, 15.00222229924320061, -4.992725166975239937 ) ) ;
#8256 = DIRECTION ( 'NONE',  ( -0.7071067811865510144, -0.7071067811865440200, 0.000000000000000000 ) ) ;
#8257 = CARTESIAN_POINT ( 'NONE',  ( 60.21275759892589718, 14.07912474133270031, -26.88233855053889698 ) ) ;
#8258 = CARTESIAN_POINT ( 'NONE',  ( 21.78406605850910083, -10.16983288769560012, -65.04335028194189761 ) ) ;
#8259 = ORIENTED_EDGE ( 'NONE', *, *, #15289, .T. ) ;
#8260 = CARTESIAN_POINT ( 'NONE',  ( 16.13393739769620083, -15.61618894467929941, -643.2998782751060389 ) ) ;
#8261 = CARTESIAN_POINT ( 'NONE',  ( 9.375144655580747610, -14.42380164995869762, -75.90328100709491821 ) ) ;
#8262 = CARTESIAN_POINT ( 'NONE',  ( 53.83033730549027496, -50.85522578410522243, -76.11623740298810503 ) ) ;
#8263 = CARTESIAN_POINT ( 'NONE',  ( 72.19051388041059170, 1.409766894666529824, -69.84163571632670653 ) ) ;
#8264 = CARTESIAN_POINT ( 'NONE',  ( 42.84502392579520347, -39.85101499308053263, -72.24970805093310844 ) ) ;
#8265 = ADVANCED_FACE ( 'NONE', ( #27495 ), #17102, .F. ) ;
#8266 = AXIS2_PLACEMENT_3D ( 'NONE', #16370, #32070, #1163 ) ;
#8267 = CARTESIAN_POINT ( 'NONE',  ( 12.06284766121009966, -63.44323389162830296, -46.39999999999999858 ) ) ;
#8268 = CIRCLE ( 'NONE', #38429, 38.50000000000001421 ) ;
#8269 = EDGE_CURVE ( 'NONE', #44411, #14960, #5388, .T. ) ;
#8270 = CARTESIAN_POINT ( 'NONE',  ( 46.81801046767949970, 22.71153819036710075, -75.82551469934900013 ) ) ;
#8271 = CARTESIAN_POINT ( 'NONE',  ( 48.70825858349740400, -54.07088363299979505, -55.10877340735739693 ) ) ;
#8272 = CARTESIAN_POINT ( 'NONE',  ( 51.68175210104495676, -32.44720899933275149, -18.13119989886391537 ) ) ;
#8273 = CIRCLE ( 'NONE', #15842, 3.000000000000004885 ) ;
#8274 = CARTESIAN_POINT ( 'NONE',  ( 57.50723796702470025, -47.11618894467930119, -17.93019253464870033 ) ) ;
#8275 = DIRECTION ( 'NONE',  ( -1.000000000000000000, 5.464378949326942347E-15, 0.000000000000000000 ) ) ;
#8276 = CARTESIAN_POINT ( 'NONE',  ( 18.20466641262020957, -23.32127506069581102, -54.20900001018016923 ) ) ;
#8277 = EDGE_LOOP ( 'NONE', ( #19873, #43462, #26010, #36347, #44255 ) ) ;
#8278 = CARTESIAN_POINT ( 'NONE',  ( 19.57145990817480197, -9.006337712462819667, -34.71999357511560191 ) ) ;
#8279 = B_SPLINE_CURVE_WITH_KNOTS ( 'NONE', 3,
 ( #47113, #51545, #34765, #26636, #50773, #15643, #10943, #3332, #23732, #3850 ),
 .UNSPECIFIED., .F., .F.,
 ( 4, 1, 1, 1, 1, 1, 1, 4 ),
 ( 0.000000000000000000, 0.05072724174294171440, 0.1299461728065594013, 0.2091651038701793641, 0.2883840349337947750, 0.3676029659974147656, 0.4468218970610324248, 0.4999964962326966522 ),
 .UNSPECIFIED. ) ;
#8280 = CARTESIAN_POINT ( 'NONE',  ( 10.72255522605177447, -19.77477957111918627, -77.24449668687897486 ) ) ;
#8281 = VERTEX_POINT ( 'NONE', #26458 ) ;
#8282 = CARTESIAN_POINT ( 'NONE',  ( 71.50269221454749413, 1.097545367735389910, -70.56928864606310015 ) ) ;
#8283 = CARTESIAN_POINT ( 'NONE',  ( 61.01538930092709734, -45.46451225926809769, -47.38536193545689912 ) ) ;
#8284 = CARTESIAN_POINT ( 'NONE',  ( 12.20262858312635146, -8.709503763698991818, -81.12752589049252094 ) ) ;
#8285 = CARTESIAN_POINT ( 'NONE',  ( 16.13393739769620083, -15.61618894467929941, -22.14999999999999858 ) ) ;
#8287 = CARTESIAN_POINT ( 'NONE',  ( 22.46009329050373537, -20.47787971217975667, -78.00066235776243673 ) ) ;
#8286 = CARTESIAN_POINT ( 'NONE',  ( 41.14166300954741473, 8.434767834753492011, -80.47192884955046566 ) ) ;
#8288 = CARTESIAN_POINT ( 'NONE',  ( 29.69570898453723728, 4.415807149541521426, -84.61328641085442825 ) ) ;
#8289 = CARTESIAN_POINT ( 'NONE',  ( 12.14981476090708945, -22.52871708785758997, -52.17433418267898304 ) ) ;
#8290 = VERTEX_POINT ( 'NONE', #42473 ) ;
#8291 = CARTESIAN_POINT ( 'NONE',  ( 84.44303304399450383, -43.32157562320250577, -47.45512980871949793 ) ) ;
#8292 = ORIENTED_EDGE ( 'NONE', *, *, #29071, .F. ) ;
#8293 = VERTEX_POINT ( 'NONE', #10502 ) ;
#8294 = ORIENTED_EDGE ( 'NONE', *, *, #48028, .T. ) ;
#8295 = DIRECTION ( 'NONE',  ( -1.000000000000000000, 0.000000000000000000, 0.000000000000000000 ) ) ;
#8296 = CARTESIAN_POINT ( 'NONE',  ( 54.17308945005400034, -50.61618894467930119, -77.01198594373980200 ) ) ;
#8297 = CARTESIAN_POINT ( 'NONE',  ( 76.41350034479297904, -9.865538814804375889, -12.85467835030281414 ) ) ;
#8298 = CARTESIAN_POINT ( 'NONE',  ( 53.65725511832430072, -51.85618790261810318, -53.56195944851729962 ) ) ;
#8299 = VERTEX_POINT ( 'NONE', #34846 ) ;
#8300 = ORIENTED_EDGE ( 'NONE', *, *, #43962, .T. ) ;
#8301 = CARTESIAN_POINT ( 'NONE',  ( 48.51124500827120301, 22.78135976125399864, -54.58137771766570268 ) ) ;
#8302 = CARTESIAN_POINT ( 'NONE',  ( 57.32036346896229873, -45.12488344740960144, -25.31853672637360120 ) ) ;
#8303 = CARTESIAN_POINT ( 'NONE',  ( 56.40269203625919658, -50.74743185910909915, -53.40076008979360012 ) ) ;
#8304 = LINE ( 'NONE', #12498, #978 ) ;
#8305 = CARTESIAN_POINT ( 'NONE',  ( 24.04476370363584792, -15.55956450748785080, -59.79004764092346846 ) ) ;
#8306 = DIRECTION ( 'NONE',  ( 0.000000000000000000, 0.000000000000000000, -1.000000000000000000 ) ) ;
#8307 = ORIENTED_EDGE ( 'NONE', *, *, #28773, .F. ) ;
#8308 = CARTESIAN_POINT ( 'NONE',  ( 51.13393739769620083, 19.38381105532069881, 10.84999999999999964 ) ) ;
#8309 = CARTESIAN_POINT ( 'NONE',  ( 53.03699916977929973, -50.36565223154730120, -77.13749947632319959 ) ) ;
#8310 = CARTESIAN_POINT ( 'NONE',  ( 60.34379259250669492, 14.63564649040839960, -47.72732609510669732 ) ) ;
#8311 = VECTOR ( 'NONE', #25256, 1000.000000000000227 ) ;
#8312 = LINE ( 'NONE', #196, #46298 ) ;
#8313 = AXIS2_PLACEMENT_3D ( 'NONE', #29194, #26749, #13501 ) ;
#8314 = AXIS2_PLACEMENT_3D ( 'NONE', #51221, #7194, #15051 ) ;
#8315 = CARTESIAN_POINT ( 'NONE',  ( 8.292221284752539390, -15.92316776411449908, -55.00003992740219871 ) ) ;
#8316 = EDGE_CURVE ( 'NONE', #49564, #19884, #10096, .T. ) ;
#8317 = CARTESIAN_POINT ( 'NONE',  ( 12.49509346338360061, -50.35846906381240018, -21.18371118359339889 ) ) ;
#8318 = CARTESIAN_POINT ( 'NONE',  ( 59.49262858449159808, -48.61618894467930119, -53.92796738110899923 ) ) ;
#8319 = CARTESIAN_POINT ( 'NONE',  ( -22.62717218277616738, -11.30032500101179238, -54.65011942300672132 ) ) ;
#8320 = LINE ( 'NONE', #972, #29325 ) ;
#8321 = EDGE_CURVE ( 'NONE', #15443, #371, #49760, .T. ) ;
#8322 = CARTESIAN_POINT ( 'NONE',  ( 70.83745409581581498, -49.21324915460289162, -70.54648330188271643 ) ) ;
#8323 = CARTESIAN_POINT ( 'NONE',  ( 61.10200083216010114, -45.74837858088729803, -47.83148726571160125 ) ) ;
#8324 = CARTESIAN_POINT ( 'NONE',  ( 12.72600710236050503, -21.52913500508059386, -39.11948792604604108 ) ) ;
#8325 = CARTESIAN_POINT ( 'NONE',  ( 18.64395816326110022, -9.025107475687740077, -54.46300130049669264 ) ) ;
#8326 = CARTESIAN_POINT ( 'NONE',  ( 12.14992226638847939, -8.703599986432690727, -41.12566464970087310 ) ) ;
#8327 = ORIENTED_EDGE ( 'NONE', *, *, #48033, .F. ) ;
#8328 = CARTESIAN_POINT ( 'NONE',  ( 14.25534935311820028, -51.38128844478910651, -75.14498753492070193 ) ) ;
#8329 = CARTESIAN_POINT ( 'NONE',  ( 47.35085381701830443, -54.68778914017550363, -54.79599060749220030 ) ) ;
#8330 = FACE_OUTER_BOUND ( 'NONE', #49702, .T. ) ;
#8331 = CARTESIAN_POINT ( 'NONE',  ( 12.72592927279295516, -9.703286911501191270, -37.78615459271271249 ) ) ;
#8332 = CARTESIAN_POINT ( 'NONE',  ( 11.18221182729259944, -20.63843675327109750, -77.59492917107350252 ) ) ;
#8333 = B_SPLINE_CURVE_WITH_KNOTS ( 'NONE', 3,
 ( #2576, #48139, #47888, #39510, #12496, #8302, #51810, #43950, #24257, #23233, #15917, #184, #40278, #12240, #3352, #28203, #19326, #44204, #19836, #27696, #43694, #4368, #43188, #31871, #11737 ),
 .UNSPECIFIED., .F., .F.,
 ( 4, 3, 3, 3, 3, 3, 3, 3, 4 ),
 ( -0.9179866157961039663, -0.8390154556610909253, -0.8167403651645870344, -0.7424182710533929752, -0.7016502394034429546, -0.6210824869669100412, -0.5865601136422979867, -0.5066596203617099725, -0.4589335890893689873 ),
 .UNSPECIFIED. ) ;
#8334 = CARTESIAN_POINT ( 'NONE',  ( 60.91744553903900083, -45.44454046914316336, -47.19084313326123237 ) ) ;
#8335 = CARTESIAN_POINT ( 'NONE',  ( 46.81978912889830013, -53.49478526707780190, -76.01748491306379663 ) ) ;
#8336 = ADVANCED_FACE ( 'NONE', ( #47442 ), #11537, .F. ) ;
#8337 = CARTESIAN_POINT ( 'NONE',  ( 10.62398834547849980, 33.60001816844019373, -18.14938726548519909 ) ) ;
#8339 = CARTESIAN_POINT ( 'NONE',  ( -7.450541063502280181, -45.60837410880110099, -5.667773980459688943 ) ) ;
#8338 = CARTESIAN_POINT ( 'NONE',  ( 61.04001029137710077, 14.12696047140060074, -46.86320535112459851 ) ) ;
#8340 = CARTESIAN_POINT ( 'NONE',  ( 1.775259308235590083, -55.58082413018939860, -10.96133985404039990 ) ) ;
#8341 = CARTESIAN_POINT ( 'NONE',  ( 43.91474985151640453, 12.31375205243809923, -5.093415854581109237 ) ) ;
#8342 = CARTESIAN_POINT ( 'NONE',  ( 48.47704942716229937, 22.94511149931419780, -55.22628212196720199 ) ) ;
#8343 = ORIENTED_EDGE ( 'NONE', *, *, #4835, .T. ) ;
#8344 = CIRCLE ( 'NONE', #27601, 2.000000000000001776 ) ;
#8345 = CARTESIAN_POINT ( 'NONE',  ( 53.25070616645550103, -49.48958487454920174, -49.09190788158600327 ) ) ;
#8346 = ORIENTED_EDGE ( 'NONE', *, *, #27688, .T. ) ;
#8347 = AXIS2_PLACEMENT_3D ( 'NONE', #30231, #18700, #46247 ) ;
#8348 = DIRECTION ( 'NONE',  ( 0.6888026391158329487, 0.7071067811865494601, 0.1598465650148944150 ) ) ;
#8349 = DIRECTION ( 'NONE',  ( -0.5109955813515499878, 0.8595833385072046973, 0.000000000000000000 ) ) ;
#8350 = FACE_OUTER_BOUND ( 'NONE', #31605, .T. ) ;
#8352 = CARTESIAN_POINT ( 'NONE',  ( 53.83139499286720309, 17.29048075286380026, -26.60275948463279860 ) ) ;
#8351 = CARTESIAN_POINT ( 'NONE',  ( 83.67009235204480433, 13.30315351291969961, -46.70940576878270178 ) ) ;
#8353 = AXIS2_PLACEMENT_3D ( 'NONE', #44058, #28313, #796 ) ;
#8354 = CARTESIAN_POINT ( 'NONE',  ( 9.109991519162420559, -14.97842488795170013, -67.48164325437429056 ) ) ;
#8355 = VECTOR ( 'NONE', #16731, 1000.000000000000114 ) ;
#8356 = CARTESIAN_POINT ( 'NONE',  ( 52.70698220066480388, 18.52838197885590077, -48.81385519956149466 ) ) ;
#8357 = CARTESIAN_POINT ( 'NONE',  ( 55.78374828174529654, -45.43414358645100037, -16.08112280697800145 ) ) ;
#8358 = DIRECTION ( 'NONE',  ( 0.3294064756440929220, 0.9441882088883218893, 0.000000000000000000 ) ) ;
#8359 = ORIENTED_EDGE ( 'NONE', *, *, #43436, .F. ) ;
#8360 = VECTOR ( 'NONE', #18728, 1000.000000000000000 ) ;
#8361 = CARTESIAN_POINT ( 'NONE',  ( 9.232756519280840735, -19.35255759171839784, -44.12955248114639772 ) ) ;
#8362 = ORIENTED_EDGE ( 'NONE', *, *, #42131, .T. ) ;
#8363 = CARTESIAN_POINT ( 'NONE',  ( 11.65337902053890140, -65.21696613297268641, -16.97470852089599802 ) ) ;
#8364 = CARTESIAN_POINT ( 'NONE',  ( 12.56561337444859916, 34.23963782672920075, -47.52000344619509775 ) ) ;
#8365 = CARTESIAN_POINT ( 'NONE',  ( 17.92370450342619748, 19.88381105532299742, -15.67980087199299888 ) ) ;
#8366 =( BOUNDED_CURVE ( )  B_SPLINE_CURVE ( 3, ( #19924, #35917, #12085, #20432 ),
 .UNSPECIFIED., .F., .T. ) 
 B_SPLINE_CURVE_WITH_KNOTS ( ( 4, 4 ),
 ( 2.702343591312255100, 2.767378142270199959 ),
 .UNSPECIFIED. ) 
 CURVE ( )  GEOMETRIC_REPRESENTATION_ITEM ( )  RATIONAL_B_SPLINE_CURVE ( ( 1.000000000000000000, 0.9996475733206606762, 0.9996475733206606762, 1.000000000000000000 ) ) 
 REPRESENTATION_ITEM ( '' )  );
#8367 = CARTESIAN_POINT ( 'NONE',  ( 53.24273501492499605, -49.42207489150700184, -48.94011550641359776 ) ) ;
#8368 = CARTESIAN_POINT ( 'NONE',  ( 10.64863409883700029, -63.44323389162830296, -23.66469670114080159 ) ) ;
#8369 = CARTESIAN_POINT ( 'NONE',  ( 18.20470691751352632, -23.32126361575343054, -63.92433611861847709 ) ) ;
#8370 = ORIENTED_EDGE ( 'NONE', *, *, #29964, .T. ) ;
#8371 = CARTESIAN_POINT ( 'NONE',  ( 13.32898876123410403, 19.91878638302433657, -21.92090654609880218 ) ) ;
#8372 = CARTESIAN_POINT ( 'NONE',  ( 10.97902946416030012, -63.29183189191540748, -44.74276748639299939 ) ) ;
#8373 = FACE_OUTER_BOUND ( 'NONE', #17015, .T. ) ;
#8374 = ORIENTED_EDGE ( 'NONE', *, *, #5622, .T. ) ;
#8375 = CARTESIAN_POINT ( 'NONE',  ( 71.63754647491310834, 1.424120032877639996, -70.11997829442159968 ) ) ;
#8376 = DIRECTION ( 'NONE',  ( 0.5516667872527449834, 0.8340645993220396903, 2.775557561562889194E-17 ) ) ;
#8377 = FACE_OUTER_BOUND ( 'NONE', #35207, .T. ) ;
#8378 = ORIENTED_EDGE ( 'NONE', *, *, #32687, .T. ) ;
#8379 = CARTESIAN_POINT ( 'NONE',  ( 11.27221019095833654, -21.94231694163175916, -62.50066393684475230 ) ) ;
#8380 = DIRECTION ( 'NONE',  ( 0.000000000000000000, 0.000000000000000000, 1.000000000000000000 ) ) ;
#8381 = CARTESIAN_POINT ( 'NONE',  ( 57.36123081458359962, -50.13537923174280309, -52.61896056486340001 ) ) ;
#8382 = CARTESIAN_POINT ( 'NONE',  ( 49.38980915263670113, 22.26227279580249885, -54.14433698582279675 ) ) ;
#8383 = CARTESIAN_POINT ( 'NONE',  ( 8.086907174455379987, -17.41285937694659935, -68.72240889194819147 ) ) ;
#8384 = EDGE_CURVE ( 'NONE', #9438, #4297, #3884, .T. ) ;
#8385 = CARTESIAN_POINT ( 'NONE',  ( 10.10517893431049963, -55.15925497894330931, -21.14999999999999858 ) ) ;
#8386 = DIRECTION ( 'NONE',  ( 1.000000000000000000, 0.000000000000000000, 0.000000000000000000 ) ) ;
#8387 = CONTEXT_DEPENDENT_SHAPE_REPRESENTATION ( #23739, #37855 ) ;
#8388 = ORIENTED_EDGE ( 'NONE', *, *, #51070, .F. ) ;
#8389 = VECTOR ( 'NONE', #28470, 1000.000000000000000 ) ;
#8390 = AXIS2_PLACEMENT_3D ( 'NONE', #4127, #449, #24795 ) ;
#8391 = CARTESIAN_POINT ( 'NONE',  ( 18.50026580205109639, -8.551687285829688179, -65.83553959257810106 ) ) ;
#8392 = CIRCLE ( 'NONE', #14231, 0.4999999999999865663 ) ;
#8393 = CARTESIAN_POINT ( 'NONE',  ( 11.73137203405248385, 10.53025766472752522, -34.79644660940672907 ) ) ;
#8394 = VECTOR ( 'NONE', #49632, 1000.000000000000000 ) ;
#8395 = PLANE ( 'NONE',  #47954 ) ;
#8396 = CARTESIAN_POINT ( 'NONE',  ( 47.24370953076470414, 23.52822497215869646, -74.17376148375639389 ) ) ;
#8397 = FACE_OUTER_BOUND ( 'NONE', #16278, .T. ) ;
#8398 = EDGE_CURVE ( 'NONE', #51191, #17738, #34491, .T. ) ;
#8399 = DIRECTION ( 'NONE',  ( 0.000000000000000000, 0.000000000000000000, 1.000000000000000000 ) ) ;
#8400 = CARTESIAN_POINT ( 'NONE',  ( 12.28024544113380045, 33.39054034926959957, -15.84304030212500081 ) ) ;
#8401 = CARTESIAN_POINT ( 'NONE',  ( 15.62259167844689856, -7.386896978515079759, -76.98791498200849048 ) ) ;
#8402 = ADVANCED_FACE ( 'NONE', ( #19543 ), #48981, .T. ) ;
#8403 = CARTESIAN_POINT ( 'NONE',  ( 56.17731397218030054, -50.61618894601519969, -75.94110601102539704 ) ) ;
#8405 = CARTESIAN_POINT ( 'NONE',  ( 42.40177580631258536, -39.88217762379048281, -74.07840177966397732 ) ) ;
#8404 = DIRECTION ( 'NONE',  ( -0.7071067811865475727, 0.000000000000000000, -0.7071067811865475727 ) ) ;
#8406 = B_SPLINE_CURVE_WITH_KNOTS ( 'NONE', 3,
 ( #14212, #11322, #43037, #6354 ),
 .UNSPECIFIED., .F., .F.,
 ( 4, 4 ),
 ( 0.4931821396943200098, 20.02578215755499969 ),
 .UNSPECIFIED. ) ;
#8408 = ADVANCED_FACE ( 'NONE', ( #49156 ), #13253, .T. ) ;
#8407 = CARTESIAN_POINT ( 'NONE',  ( 63.06902243323368396, 0.9940695285616559795, -68.85188839627709001 ) ) ;
#8409 = CARTESIAN_POINT ( 'NONE',  ( 61.39588016577010166, 13.94803720521050039, -46.37201980406299384 ) ) ;
#8410 = CARTESIAN_POINT ( 'NONE',  ( -0.3068767133167060179, -63.31736862303570490, -50.59628790670890197 ) ) ;
#8411 = AXIS2_PLACEMENT_3D ( 'NONE', #4132, #25056, #8849 ) ;
#8412 = VERTEX_POINT ( 'NONE', #9321 ) ;
#8413 = CARTESIAN_POINT ( 'NONE',  ( 52.84340795157500281, -49.65376797971740075, -48.59551871909959431 ) ) ;
#8414 = CARTESIAN_POINT ( 'NONE',  ( 61.34256095932860120, -45.15002362613940079, -27.50959865473700106 ) ) ;
#8415 = CARTESIAN_POINT ( 'NONE',  ( 12.14970019625365438, -22.52865228160853306, -72.45901836890904235 ) ) ;
#8416 = CARTESIAN_POINT ( 'NONE',  ( 57.10264026197389597, 14.43158848240689984, -26.17393976174119885 ) ) ;
#8417 = CARTESIAN_POINT ( 'NONE',  ( 12.65851744802729861, -22.20616599455440010, -80.88713649466581046 ) ) ;
#8418 = CARTESIAN_POINT ( 'NONE',  ( 50.30621290460380379, 17.52022015291559853, -76.16272939178270462 ) ) ;
#8419 = CARTESIAN_POINT ( 'NONE',  ( 52.76045202141140322, 18.46818829728630007, -48.50240600070850405 ) ) ;
#8420 = CARTESIAN_POINT ( 'NONE',  ( 71.21626143364200345, 1.196343736543249880, -70.67573229508370503 ) ) ;
#8421 = CARTESIAN_POINT ( 'NONE',  ( 42.62644315484929791, -42.85940974227979439, -3.197525305375130245 ) ) ;
#8422 = CARTESIAN_POINT ( 'NONE',  ( 53.78771641980449658, -51.63629534268280707, -53.21849989078970111 ) ) ;
#8423 = ORIENTED_EDGE ( 'NONE', *, *, #19489, .F. ) ;
#8424 = DIRECTION ( 'NONE',  ( 0.000000000000000000, 1.000000000000000000, 0.000000000000000000 ) ) ;
#8425 = VECTOR ( 'NONE', #16106, 1000.000000000000000 ) ;
#8426 = CARTESIAN_POINT ( 'NONE',  ( 47.73397142286539463, -54.47958293233019589, -54.93080396559629719 ) ) ;
#8427 = CARTESIAN_POINT ( 'NONE',  ( -8.011283399303589903, 13.73034950232750084, -5.061381375665199300 ) ) ;
#8428 = AXIS2_PLACEMENT_3D ( 'NONE', #34950, #10612, #6940 ) ;
#8429 = CARTESIAN_POINT ( 'NONE',  ( 42.93197233849420513, 11.32569894967160096, -3.187564294433600232 ) ) ;
#8430 = CARTESIAN_POINT ( 'NONE',  ( 56.91683567916710018, 19.43129369009569984, -53.20179923793649834 ) ) ;
#8431 = CARTESIAN_POINT ( 'NONE',  ( 71.28621524259639841, 1.327322800621349996, -60.84198109300940160 ) ) ;
#8432 = CARTESIAN_POINT ( 'NONE',  ( 41.13393739769620083, -15.61618894467929941, 4.450000000000000178 ) ) ;
#8433 = CARTESIAN_POINT ( 'NONE',  ( 71.67377888102110717, 1.031491003830389941, -60.81565309434889599 ) ) ;
#8434 = TOROIDAL_SURFACE ( 'NONE', #37717, 38.50000000000000000, 0.5000000000000000000 ) ;
#8435 = VECTOR ( 'NONE', #22218, 1000.000000000000000 ) ;
#8436 = CARTESIAN_POINT ( 'NONE',  ( 24.04464518807997919, -15.61618401921712618, -71.50767245506341396 ) ) ;
#8437 = CARTESIAN_POINT ( 'NONE',  ( 64.97290478796050195, 0.8840451408750739093, -70.74985906855570761 ) ) ;
#8438 = ORIENTED_EDGE ( 'NONE', *, *, #13849, .T. ) ;
#8439 = ORIENTED_EDGE ( 'NONE', *, *, #38931, .F. ) ;
#8440 = CARTESIAN_POINT ( 'NONE',  ( 71.83406239765299972, 11.38381103969570063, -62.44999999999849649 ) ) ;
#8441 = CYLINDRICAL_SURFACE ( 'NONE', #27717, 5.000000000000000000 ) ;
#8442 = ORIENTED_EDGE ( 'NONE', *, *, #26884, .T. ) ;
#8443 = DIRECTION ( 'NONE',  ( 0.6933752452815367118, 0.7071067811865475727, -0.1386750490563054827 ) ) ;
#8444 = CARTESIAN_POINT ( 'NONE',  ( 22.13393739769589885, 22.91950879131610108, -54.64999999999999858 ) ) ;
#8445 = CARTESIAN_POINT ( 'NONE',  ( 17.26073403098808257, -8.923770253816476483, -50.00599002542245586 ) ) ;
#8446 = ORIENTED_EDGE ( 'NONE', *, *, #28555, .T. ) ;
#8447 = DIRECTION ( 'NONE',  ( -1.000000000000000000, 1.330268894940021809E-33, -1.060511545910580040E-15 ) ) ;
#8448 = CARTESIAN_POINT ( 'NONE',  ( 42.32923956695206869, 6.443803624954492548, -78.67348905400854164 ) ) ;
#8449 = CARTESIAN_POINT ( 'NONE',  ( 24.04501723819814529, -15.61618889329698412, -35.50767088183642528 ) ) ;
#8450 = CARTESIAN_POINT ( 'NONE',  ( 15.87474718106880012, -23.85727749459430314, -38.30233936351829982 ) ) ;
#8451 = ADVANCED_FACE ( 'NONE', ( #25265 ), #41366, .T. ) ;
#8452 = CARTESIAN_POINT ( 'NONE',  ( 45.34361468062490275, 2.694758396794109778, -34.64999999999999858 ) ) ;
#8453 = DIRECTION ( 'NONE',  ( 0.000000000000000000, 0.000000000000000000, 1.000000000000000000 ) ) ;
#8454 = ORIENTED_EDGE ( 'NONE', *, *, #9783, .F. ) ;
#8455 = CARTESIAN_POINT ( 'NONE',  ( 11.75056615120120185, -63.52426806926749236, -24.76662875350499959 ) ) ;
#8456 = CARTESIAN_POINT ( 'NONE',  ( 15.89973463379899776, -23.06278836122699971, -38.74266516882029521 ) ) ;
#8457 = CARTESIAN_POINT ( 'NONE',  ( 41.71810510585039822, 14.49570306633170169, -6.599646603091770203 ) ) ;
#8458 = CARTESIAN_POINT ( 'NONE',  ( 14.41909000996080081, 21.14718688187949880, -75.96082109999758814 ) ) ;
#8459 = CARTESIAN_POINT ( 'NONE',  ( 51.73306225501220013, 17.77684153297740011, -77.03096025368019184 ) ) ;
#8460 = CARTESIAN_POINT ( 'NONE',  ( 47.13393739769619373, 4.883811055320659733, -35.14999999999999858 ) ) ;
#8461 = EDGE_CURVE ( 'NONE', #33975, #31547, #3708, .T. ) ;
#8462 = CARTESIAN_POINT ( 'NONE',  ( -18.86606260230390220, 19.38381105532060289, 17.35000000000000142 ) ) ;
#8463 = AXIS2_PLACEMENT_3D ( 'NONE', #29052, #9151, #17275 ) ;
#8464 = CARTESIAN_POINT ( 'NONE',  ( 21.64425948049070314, -9.482750165915568630, -43.24065034890669068 ) ) ;
#8465 = ORIENTED_EDGE ( 'NONE', *, *, #42246, .T. ) ;
#8466 = CARTESIAN_POINT ( 'NONE',  ( 53.86231929347299996, -48.56206393835490331, -26.75416873081589841 ) ) ;
#8467 = CARTESIAN_POINT ( 'NONE',  ( 15.94236692260130006, -50.98710977590300075, -20.14988694616399911 ) ) ;
#8468 = CARTESIAN_POINT ( 'NONE',  ( 76.84075427690970628, 10.73731228644500035, -14.69578844725669953 ) ) ;
#8469 = CARTESIAN_POINT ( 'NONE',  ( -21.36606260230379917, 21.88381105532059934, 17.35000000000000142 ) ) ;
#8471 = ADVANCED_FACE ( 'NONE', ( #18457 ), #42576, .F. ) ;
#8470 = CARTESIAN_POINT ( 'NONE',  ( 13.10370563145657030, -9.247495623643706253, -56.20581778389941974 ) ) ;
#8472 = DIRECTION ( 'NONE',  ( 0.1686178020941689892, 0.6660492713794449182, -0.7265992051412129005 ) ) ;
#8473 = VERTEX_POINT ( 'NONE', #7443 ) ;
#8474 = CARTESIAN_POINT ( 'NONE',  ( -4.044075683915660413, -48.07007205289909990, -5.230652478517891169 ) ) ;
#8475 = CARTESIAN_POINT ( 'NONE',  ( 47.36954728576590412, 23.43543924705889836, -54.64415512175509804 ) ) ;
#8476 = CARTESIAN_POINT ( 'NONE',  ( 68.13393739769618662, -0.5161889446793590519, -65.65000000000000568 ) ) ;
#8477 = CARTESIAN_POINT ( 'NONE',  ( 63.06339012708429692, 0.9214125008369580261, -62.44212918470660156 ) ) ;
#8478 = CARTESIAN_POINT ( 'NONE',  ( 26.13393739769619728, -2.337132753317950229, -62.14999999999999858 ) ) ;
#8479 = CARTESIAN_POINT ( 'NONE',  ( 43.02291017071019752, 12.66373381907540008, -5.004961222460109660 ) ) ;
#8480 = LINE ( 'NONE', #9267, #27760 ) ;
#8481 = CYLINDRICAL_SURFACE ( 'NONE', #10842, 0.4999999999999984457 ) ;
#8482 = DIRECTION ( 'NONE',  ( 0.4042525045258790750, 0.000000000000000000, -0.9146474252872273114 ) ) ;
#8483 = CARTESIAN_POINT ( 'NONE',  ( 59.50642288013500547, -46.25939025630010093, -47.77182982531389399 ) ) ;
#8484 = CARTESIAN_POINT ( 'NONE',  ( 24.04492188529094321, -15.60000870450956789, -75.79167514006502415 ) ) ;
#8485 = CARTESIAN_POINT ( 'NONE',  ( -21.36606260230379917, -62.82329572586585442, 17.05710678118654400 ) ) ;
#8486 = CARTESIAN_POINT ( 'NONE',  ( 56.45472350107259984, 19.54838399657660020, -53.73843559234909861 ) ) ;
#8487 = DIRECTION ( 'NONE',  ( 0.000000000000000000, 0.000000000000000000, -1.000000000000000000 ) ) ;
#8488 = CARTESIAN_POINT ( 'NONE',  ( 50.44542158113339525, 13.88381105532070059, -10.59990841363550018 ) ) ;
#8489 = ORIENTED_EDGE ( 'NONE', *, *, #41754, .F. ) ;
#8490 = CARTESIAN_POINT ( 'NONE',  ( -0.05431535188140382969, -10.47559300615912115, -34.81369804311114535 ) ) ;
#8491 = CARTESIAN_POINT ( 'NONE',  ( 9.736267853041370657, 31.97384013447830142, -46.29821234986540190 ) ) ;
#8492 = CARTESIAN_POINT ( 'NONE',  ( 41.60144942313346661, 13.58288154834297501, -5.503716546408811361 ) ) ;
#8493 = CARTESIAN_POINT ( 'NONE',  ( 14.10774154971239902, -8.019855601378861110, -81.23899999999999011 ) ) ;
#8494 = EDGE_LOOP ( 'NONE', ( #33155, #23740, #13917, #49735 ) ) ;
#8495 = CARTESIAN_POINT ( 'NONE',  ( 18.36003180639029964, 20.26946707534090208, -75.09610479291009710 ) ) ;
#8496 = EDGE_LOOP ( 'NONE', ( #11929, #32550, #1454, #18876, #31481, #12426 ) ) ;
#8497 = ORIENTED_EDGE ( 'NONE', *, *, #4957, .T. ) ;
#8498 = ORIENTED_EDGE ( 'NONE', *, *, #33825, .T. ) ;
#8499 = FACE_OUTER_BOUND ( 'NONE', #21799, .T. ) ;
#8500 = CARTESIAN_POINT ( 'NONE',  ( 22.75585767527259762, -18.49336363850369835, -81.23899999999999011 ) ) ;
#8501 = AXIS2_PLACEMENT_3D ( 'NONE', #4413, #35349, #8349 ) ;
#8502 = CARTESIAN_POINT ( 'NONE',  ( 0.4253373362159595383, -8.849698965567686315, -35.06583844469757594 ) ) ;
#8503 = ORIENTED_EDGE ( 'NONE', *, *, #51861, .T. ) ;
#8504 = CIRCLE ( 'NONE', #50370, 0.5000000000000004441 ) ;
#8505 = CARTESIAN_POINT ( 'NONE',  ( 14.34417029198830029, 19.88381105532299742, -74.14999999999999147 ) ) ;
#8506 = CIRCLE ( 'NONE', #37796, 5.999999999999998224 ) ;
#8507 = FACE_OUTER_BOUND ( 'NONE', #32319, .T. ) ;
#8508 = ORIENTED_EDGE ( 'NONE', *, *, #39766, .F. ) ;
#8509 = CARTESIAN_POINT ( 'NONE',  ( -28.43713041416927467, 28.95487886718607129, 11.84999999999999964 ) ) ;
#8510 = EDGE_CURVE ( 'NONE', #21889, #32046, #15566, .T. ) ;
#8511 = CARTESIAN_POINT ( 'NONE',  ( 51.81838375203209779, 2.459119445085170330, -77.22003095415269058 ) ) ;
#8512 = ORIENTED_EDGE ( 'NONE', *, *, #20425, .T. ) ;
#8513 = EDGE_CURVE ( 'NONE', #33500, #15767, #45566, .T. ) ;
#8514 = ORIENTED_EDGE ( 'NONE', *, *, #29327, .T. ) ;
#8515 = EDGE_CURVE ( 'NONE', #12957, #13595, #28788, .T. ) ;
#8516 = FACE_OUTER_BOUND ( 'NONE', #39444, .T. ) ;
#8517 = DIRECTION ( 'NONE',  ( 0.000000000000000000, 0.000000000000000000, -1.000000000000000000 ) ) ;
#8518 = CARTESIAN_POINT ( 'NONE',  ( 60.77958717670829714, 14.50249311732349966, -47.75277892092170617 ) ) ;
#8519 = ADVANCED_FACE ( 'NONE', ( #46518 ), #19225, .T. ) ;
#8520 = CARTESIAN_POINT ( 'NONE',  ( 45.70140901369219932, 14.68666752987680013, -9.304972802417179167 ) ) ;
#8521 = CARTESIAN_POINT ( 'NONE',  ( 20.11808723905773988, -22.52870104806199691, -68.12566323940706070 ) ) ;
#8522 = CARTESIAN_POINT ( 'NONE',  ( -7.088889386270000870, 14.46722970464960056, -4.961773261597420159 ) ) ;
#8523 = DIRECTION ( 'NONE',  ( 0.000000000000000000, 0.000000000000000000, 1.000000000000000000 ) ) ;
#8524 = CARTESIAN_POINT ( 'NONE',  ( 54.47259832750690123, 15.01994964729280113, -15.76422791930239953 ) ) ;
#8525 = CARTESIAN_POINT ( 'NONE',  ( 20.55998394979739885, -22.09668739015519989, -57.59677076196169310 ) ) ;
#8526 = VERTEX_POINT ( 'NONE', #10861 ) ;
#8527 = DIRECTION ( 'NONE',  ( -1.000000000000000000, 0.000000000000000000, 0.000000000000000000 ) ) ;
#8528 = B_SPLINE_CURVE_WITH_KNOTS ( 'NONE', 3,
 ( #39222, #35279, #7512, #43160, #47354, #11450, #27408, #35010, #2806, #42381 ),
 .UNSPECIFIED., .F., .F.,
 ( 4, 2, 2, 2, 4 ),
 ( 0.4999999999999911737, 0.5970844297732782469, 0.7236511483078821305, 0.8661472597497344994, 1.000000000000000000 ),
 .UNSPECIFIED. ) ;
#8529 = CARTESIAN_POINT ( 'NONE',  ( 40.84819594366380358, 14.17549957042029973, -5.828853726967939686 ) ) ;
#8530 = CARTESIAN_POINT ( 'NONE',  ( 12.21949317767530019, 34.07078414252080023, -46.32488671064290031 ) ) ;
#8531 = UNCERTAINTY_MEASURE_WITH_UNIT (LENGTH_MEASURE( 1.000000000000000082E-05 ), #23837, 'distance_accuracy_value', 'NONE');
#8533 = EDGE_CURVE ( 'NONE', #10891, #3359, #7597, .T. ) ;
#8532 = CARTESIAN_POINT ( 'NONE',  ( 72.25629666767210324, 1.056850087111250058, -70.01040857010899288 ) ) ;
#8534 = B_SPLINE_CURVE_WITH_KNOTS ( 'NONE', 3,
 ( #33809, #13912, #45889, #50071, #14166, #25938, #10243, #22010, #36816, #37865, #17685, #34428, #10608, #1962, #21722, #29841 ),
 .UNSPECIFIED., .F., .F.,
 ( 4, 2, 2, 2, 2, 2, 2, 4 ),
 ( -8.599659000000000768E-15, 0.07216186899280199740, 0.1546325764131579739, 0.2061767685508799908, 0.2319488646197410409, 0.2731842183299189597, 0.3391607842662029970, 0.4123535371017689743 ),
 .UNSPECIFIED. ) ;
#8535 = CARTESIAN_POINT ( 'NONE',  ( 42.93611710919282842, -39.85996260035505401, -71.80852276252326760 ) ) ;
#8536 = CIRCLE ( 'NONE', #21051, 22.00000000000000000 ) ;
#8537 = TOROIDAL_SURFACE ( 'NONE', #11922, 18.00000000000000000, 2.000000000000000000 ) ;
#8538 = CARTESIAN_POINT ( 'NONE',  ( 11.68991505667689879, -64.90566085822540288, -16.36861125146140239 ) ) ;
#8539 = CARTESIAN_POINT ( 'NONE',  ( 46.38760183179699936, 21.75546072051859881, -76.14872548137130082 ) ) ;
#8540 = CARTESIAN_POINT ( 'NONE',  ( 49.05314114107740409, -53.88090997908469859, -54.81529494278139936 ) ) ;
#8541 = CARTESIAN_POINT ( 'NONE',  ( -4.967261132674519963, 16.44508974743529706, -5.583919853821729617 ) ) ;
#8542 = CARTESIAN_POINT ( 'NONE',  ( 17.07732798564219578, -23.50820749086367911, -33.96988921057287314 ) ) ;
#8543 = CARTESIAN_POINT ( 'NONE',  ( 18.13393739769630031, 1.380694156556650176, -35.10658870009205401 ) ) ;
#8544 = CARTESIAN_POINT ( 'NONE',  ( 11.51802410812858923, -20.94872152101151030, -71.57429041023839034 ) ) ;
#8545 = VERTEX_POINT ( 'NONE', #16069 ) ;
#8546 = CARTESIAN_POINT ( 'NONE',  ( 22.79714714506240369, -12.28327277397440120, -46.91970895891289928 ) ) ;
#8547 = CARTESIAN_POINT ( 'NONE',  ( 22.72480921377356822, -17.38744322059056913, -76.53615365903577583 ) ) ;
#8548 = ORIENTED_EDGE ( 'NONE', *, *, #48493, .T. ) ;
#8549 = DIRECTION ( 'NONE',  ( 0.000000000000000000, 0.000000000000000000, -1.000000000000000000 ) ) ;
#8550 = CARTESIAN_POINT ( 'NONE',  ( 60.52205090682910082, -45.66102862280700236, -47.41488707632970545 ) ) ;
#8551 = CARTESIAN_POINT ( 'NONE',  ( 68.13393739769620083, -48.61618894467930119, -65.65000000000000568 ) ) ;
#8552 = CARTESIAN_POINT ( 'NONE',  ( 64.89113374320363903, -43.41649467415835772, -10.41665185867834964 ) ) ;
#8554 = CARTESIAN_POINT ( 'NONE',  ( 44.97636411188102556, -33.23110557053604452, -38.73002865210571599 ) ) ;
#8553 = CARTESIAN_POINT ( 'NONE',  ( 42.84219048620263948, 8.618426686109231127, -72.26305710318311526 ) ) ;
#8555 = EDGE_CURVE ( 'NONE', #50303, #39386, #31520, .T. ) ;
#8556 = CARTESIAN_POINT ( 'NONE',  ( 29.52393724633215299, 4.446165992738185579, -84.61793436501787369 ) ) ;
#8557 = DIRECTION ( 'NONE',  ( -0.7071067811865476838, -0.7071067811865473507, 0.000000000000000000 ) ) ;
#8558 = VERTEX_POINT ( 'NONE', #4271 ) ;
#8559 = CARTESIAN_POINT ( 'NONE',  ( 83.49396592876078671, -45.25227995425159833, -47.52773119087509457 ) ) ;
#8560 = ORIENTED_EDGE ( 'NONE', *, *, #3242, .T. ) ;
#8561 = ORIENTED_EDGE ( 'NONE', *, *, #6654, .F. ) ;
#8562 = ORIENTED_EDGE ( 'NONE', *, *, #11092, .F. ) ;
#8563 = CARTESIAN_POINT ( 'NONE',  ( 61.54545584751650011, -45.33073283442580248, -47.27437412891610080 ) ) ;
#8564 = CARTESIAN_POINT ( 'NONE',  ( 52.97776617209801486, -50.30125835459202932, -77.23905649395202033 ) ) ;
#8565 = CARTESIAN_POINT ( 'NONE',  ( 76.39547088046599299, -13.14241137819745653, -12.77698718076613815 ) ) ;
#8566 = CARTESIAN_POINT ( 'NONE',  ( 52.30020358789180079, -52.26933069182599212, -53.48872967491809760 ) ) ;
#8567 = ORIENTED_EDGE ( 'NONE', *, *, #33836, .F. ) ;
#8568 = VERTEX_POINT ( 'NONE', #32279 ) ;
#8569 = CARTESIAN_POINT ( 'NONE',  ( 47.82941845642289991, 23.15673897679920046, -54.71834399002119653 ) ) ;
#8570 = FACE_OUTER_BOUND ( 'NONE', #41552, .T. ) ;
#8571 = CARTESIAN_POINT ( 'NONE',  ( 16.10427296349248394, -8.563410825654969472, -66.34584096005498566 ) ) ;
#8572 = CARTESIAN_POINT ( 'NONE',  ( 8.788636732660460638, -63.13527780971870129, -46.67124789091300130 ) ) ;
#8573 = CARTESIAN_POINT ( 'NONE',  ( 63.14276237176480322, 0.4687350093257069972, -17.15814307286319718 ) ) ;
#8574 = DIRECTION ( 'NONE',  ( -0.3863301728269271096, 0.9223605572461979207, 0.000000000000000000 ) ) ;
#8575 = ADVANCED_FACE ( 'NONE', ( #20241 ), #35506, .T. ) ;
#8576 = CIRCLE ( 'NONE', #190, 1.999999999999998224 ) ;
#8577 = VERTEX_POINT ( 'NONE', #340 ) ;
#8578 = CARTESIAN_POINT ( 'NONE',  ( -1.549418844231527537, 19.36423916373297160, -6.286238266776149608 ) ) ;
#8580 = CARTESIAN_POINT ( 'NONE',  ( 54.17317666706389900, -50.61618894916709621, -77.01210126949929702 ) ) ;
#8579 = CIRCLE ( 'NONE', #2741, 2.000000000000001332 ) ;
#8581 = CARTESIAN_POINT ( 'NONE',  ( 19.53857308744663257, -9.751301291141226457, -34.12023054736771854 ) ) ;
#8582 = LINE ( 'NONE', #31881, #221 ) ;
#8583 = EDGE_CURVE ( 'NONE', #31649, #7985, #2014, .T. ) ;
#8584 = CARTESIAN_POINT ( 'NONE',  ( 15.22032918994340100, -7.821827672945169674, -55.47535351378380142 ) ) ;
#8585 = CARTESIAN_POINT ( 'NONE',  ( -21.36606260230379917, 31.88381105532059934, 11.84999999999999964 ) ) ;
#8586 = CARTESIAN_POINT ( 'NONE',  ( 41.32046296083159831, -44.52894084121439988, -4.975097116197259695 ) ) ;
#8587 = CARTESIAN_POINT ( 'NONE',  ( 21.79705635832086585, -42.73068571072664668, -84.65000000000000568 ) ) ;
#8588 = CARTESIAN_POINT ( 'NONE',  ( 57.04834586696819798, 13.88381105532070059, -16.05449549621770089 ) ) ;
#8589 = CARTESIAN_POINT ( 'NONE',  ( 61.29293631677610676, -45.55587099302650955, -47.63113523840529950 ) ) ;
#8590 = CARTESIAN_POINT ( 'NONE',  ( 9.757136478812640235, -12.60305615381579969, -53.98768771411499756 ) ) ;
#8591 = CARTESIAN_POINT ( 'NONE',  ( 22.46012617239150799, -10.75454331186309531, -41.58399771921369847 ) ) ;
#8592 = ORIENTED_EDGE ( 'NONE', *, *, #29623, .F. ) ;
#8593 = CARTESIAN_POINT ( 'NONE',  ( 14.38326576340259955, -51.65751396603660339, -75.51495726157199329 ) ) ;
#8594 = CARTESIAN_POINT ( 'NONE',  ( 47.34625512861649810, -54.69081487665980035, -54.80683018298890374 ) ) ;
#8595 = CARTESIAN_POINT ( 'NONE',  ( 10.53031889351280981, 33.70290473897190964, -47.11352251473290664 ) ) ;
#8596 = FACE_OUTER_BOUND ( 'NONE', #29494, .T. ) ;
#8597 = CARTESIAN_POINT ( 'NONE',  ( 60.89412992731197249, -45.44744514121628498, -47.14788752398113303 ) ) ;
#8598 = CARTESIAN_POINT ( 'NONE',  ( 57.40776171064106137, 14.07025572946862368, -25.91845855463345671 ) ) ;
#8599 = FACE_OUTER_BOUND ( 'NONE', #2584, .T. ) ;
#8601 = CARTESIAN_POINT ( 'NONE',  ( 8.223585368203801593, -15.61624251583899969, -52.79233150823699816 ) ) ;
#8600 = DIRECTION ( 'NONE',  ( 0.000000000000000000, 0.000000000000000000, 1.000000000000000000 ) ) ;
#8602 = CARTESIAN_POINT ( 'NONE',  ( 14.98839500567465599, -52.93031137934188024, -76.14999999999994884 ) ) ;
#8603 = CARTESIAN_POINT ( 'NONE',  ( 48.45558241519640319, 22.90200554677129929, -54.87093290419399949 ) ) ;
#8604 = VERTEX_POINT ( 'NONE', #7707 ) ;
#8605 = CARTESIAN_POINT ( 'NONE',  ( 16.10427296349259763, -8.563410825682879590, -66.34584096003949583 ) ) ;
#8606 = TOROIDAL_SURFACE ( 'NONE', #51302, 14.50000000000000000, 1.500000000000000000 ) ;
#8607 = ORIENTED_EDGE ( 'NONE', *, *, #2540, .F. ) ;
#8608 = DIRECTION ( 'NONE',  ( -1.000000000000000000, 0.000000000000000000, 0.000000000000000000 ) ) ;
#8609 = CARTESIAN_POINT ( 'NONE',  ( 64.97340239734420209, 1.393731187554809958, -61.04935521477050031 ) ) ;
#8610 = DIRECTION ( 'NONE',  ( 0.000000000000000000, 0.000000000000000000, -1.000000000000000000 ) ) ;
#8612 = CARTESIAN_POINT ( 'NONE',  ( 55.08137342987989626, 16.01549851114500100, -26.24734268074100285 ) ) ;
#8611 = CARTESIAN_POINT ( 'NONE',  ( 82.65203287802668797, 13.84520072205750019, -46.57208626984800048 ) ) ;
#8613 = EDGE_CURVE ( 'NONE', #50973, #11348, #21952, .T. ) ;
#8614 = CARTESIAN_POINT ( 'NONE',  ( 13.67824910300939933, -22.22770569168709898, -69.06602187564659801 ) ) ;
#8615 = CARTESIAN_POINT ( 'NONE',  ( 52.57435089425080577, 18.62009177781090230, -48.51307714252150305 ) ) ;
#8616 = CARTESIAN_POINT ( 'NONE',  ( 54.83244778698070121, -45.50794643880949764, -15.28355693140960092 ) ) ;
#8617 = DIRECTION ( 'NONE',  ( 0.000000000000000000, -1.000000000000000000, 0.000000000000000000 ) ) ;
#8618 = EDGE_CURVE ( 'NONE', #4597, #13604, #4790, .T. ) ;
#8619 = EDGE_LOOP ( 'NONE', ( #15428, #28658, #9968, #10737 ) ) ;
#8620 = VERTEX_POINT ( 'NONE', #20758 ) ;
#8621 = EDGE_CURVE ( 'NONE', #25343, #38938, #10752, .T. ) ;
#8622 = CARTESIAN_POINT ( 'NONE',  ( 11.80495200724810090, -64.96876320708929597, -16.40176568415489911 ) ) ;
#8623 = CARTESIAN_POINT ( 'NONE',  ( 11.11335566852529944, 33.52968406517779698, -46.40488835177220039 ) ) ;
#8624 = CARTESIAN_POINT ( 'NONE',  ( 51.17461318815491467, 0.4193470954621815738, -17.11446460828111427 ) ) ;
#8625 = CARTESIAN_POINT ( 'NONE',  ( 16.13393739769620083, -15.61618894467929941, -6.649999999999999467 ) ) ;
#8626 = CARTESIAN_POINT ( 'NONE',  ( 23.83903869154858413, -17.68685940192425221, -63.59100333396448690 ) ) ;
#8627 = ORIENTED_EDGE ( 'NONE', *, *, #3260, .T. ) ;
#8628 = FACE_OUTER_BOUND ( 'NONE', #39131, .T. ) ;
#8629 = CARTESIAN_POINT ( 'NONE',  ( 11.13393739769619906, -63.35298109097990960, -43.74913429451299862 ) ) ;
#8630 = CARTESIAN_POINT ( 'NONE',  ( 53.58906601315669604, 18.17498435715450000, -49.22641449468370212 ) ) ;
#8631 = CARTESIAN_POINT ( 'NONE',  ( 47.64143405402000297, 23.30250925608569901, -55.14905519569659731 ) ) ;
#8632 = CARTESIAN_POINT ( 'NONE',  ( 50.40317164625179913, -49.92886143348300720, -76.14999999999999147 ) ) ;
#8633 = CARTESIAN_POINT ( 'NONE',  ( 23.83903513718275846, -17.68687693612751488, -43.59100491536354838 ) ) ;
#8634 = ORIENTED_EDGE ( 'NONE', *, *, #40471, .T. ) ;
#8635 = CARTESIAN_POINT ( 'NONE',  ( 10.06369629474122185, 22.76024865223496363, -34.79644414665609986 ) ) ;
#8636 = CARTESIAN_POINT ( 'NONE',  ( 57.03107162669589769, -50.22865659835970575, -52.68131389647400198 ) ) ;
#8637 = CARTESIAN_POINT ( 'NONE',  ( 52.56662653895409676, 22.94659662340869843, -56.87452811520210361 ) ) ;
#8638 = EDGE_CURVE ( 'NONE', #39256, #49799, #41370, .T. ) ;
#8639 = CARTESIAN_POINT ( 'NONE',  ( 16.77044965268740029, -23.83674684576979885, -74.26773406640140252 ) ) ;
#8640 = CARTESIAN_POINT ( 'NONE',  ( 14.12233147869610050, -51.14020415306820411, -22.75736351947179870 ) ) ;
#8641 = CARTESIAN_POINT ( 'NONE',  ( 53.72798125810859915, 20.02004718435770059, -75.61331206641780511 ) ) ;
#8642 = CARTESIAN_POINT ( 'NONE',  ( 46.48018481170299765, -53.11273823506989800, -76.13961530627510399 ) ) ;
#8643 = EDGE_LOOP ( 'NONE', ( #31163, #34681, #44524, #9317 ) ) ;
#8644 = CARTESIAN_POINT ( 'NONE',  ( 22.90106509282977854, -15.61618896609811458, -36.45282238757207693 ) ) ;
#8645 = CIRCLE ( 'NONE', #2777, 6.999999999999999112 ) ;
#8646 = CARTESIAN_POINT ( 'NONE',  ( 21.58606382555289827, -10.53868845528379872, -65.99397745470530197 ) ) ;
#8647 = DIRECTION ( 'NONE',  ( -1.000000000000000000, 0.000000000000000000, 0.000000000000000000 ) ) ;
#8648 = DIRECTION ( 'NONE',  ( -0.9339609686412669864, 0.000000000000000000, -0.3573750257847720380 ) ) ;
#8649 = CARTESIAN_POINT ( 'NONE',  ( 47.43599257781200151, 23.40374490022220044, -74.17365615959539582 ) ) ;
#8650 = CARTESIAN_POINT ( 'NONE',  ( 19.71324513114140231, -54.20984286782871919, -17.35305593079180042 ) ) ;
#8651 = CARTESIAN_POINT ( 'NONE',  ( 75.07156378438740774, -22.19556467665293553, -11.41441923602980602 ) ) ;
#8652 = CARTESIAN_POINT ( 'NONE',  ( 41.31714037750759871, -44.78197124420869812, -5.389672071857970259 ) ) ;
#8653 = CARTESIAN_POINT ( 'NONE',  ( 28.63499203762230394, -4.678279065789539892, -34.64999999999999858 ) ) ;
#8654 = CARTESIAN_POINT ( 'NONE',  ( 13.13393739769619906, -49.61618894467939356, -83.01107220193038927 ) ) ;
#8655 = AXIS2_PLACEMENT_3D ( 'NONE', #7493, #24207, #8256 ) ;
#8656 = CARTESIAN_POINT ( 'NONE',  ( 60.23130391296999875, -45.78304229081430066, -47.24246919202539630 ) ) ;
#8658 = LINE ( 'NONE', #48759, #2983 ) ;
#8657 = DIRECTION ( 'NONE',  ( 0.8660254037844380415, -0.5000000000000012212, -2.498001805406606160E-16 ) ) ;
#8659 = CARTESIAN_POINT ( 'NONE',  ( 63.34531745652139989, 1.374300485541529948, -68.58542282960749503 ) ) ;
#8660 = CARTESIAN_POINT ( 'NONE',  ( 61.45294174464890347, 13.92837788602000160, -46.37201849592059943 ) ) ;
#8661 = CARTESIAN_POINT ( 'NONE',  ( 72.60719124696490212, 0.9098571636355720083, -68.84999999999999432 ) ) ;
#8662 = DIRECTION ( 'NONE',  ( 0.000000000000000000, 1.000000000000000000, 0.000000000000000000 ) ) ;
#8663 = VERTEX_POINT ( 'NONE', #37803 ) ;
#8664 =( BOUNDED_CURVE ( )  B_SPLINE_CURVE ( 2, ( #25117, #33761, #29573, #36935, #40604 ),
 .UNSPECIFIED., .F., .T. ) 
 B_SPLINE_CURVE_WITH_KNOTS ( ( 3, 2, 3 ),
 ( -0.003205554297748039981, 0.8238407534185530068, 1.650887061134849843 ),
 .UNSPECIFIED. ) 
 CURVE ( )  GEOMETRIC_REPRESENTATION_ITEM ( )  RATIONAL_B_SPLINE_CURVE ( ( 1.000000000000000000, 0.9157107718030679244, 1.000000000000000000, 0.9157107718030469412, 1.000000000000000000 ) ) 
 REPRESENTATION_ITEM ( '' )  );
#8665 = CARTESIAN_POINT ( 'NONE',  ( 52.86217718811949595, -49.64393425081360789, -48.67083959267399962 ) ) ;
#8666 = CARTESIAN_POINT ( 'NONE',  ( 60.50740924954109801, -45.14437743309510154, -26.64919274788590187 ) ) ;
#8667 = DIRECTION ( 'NONE',  ( 0.000000000000000000, -1.000000000000000000, 0.000000000000000000 ) ) ;
#8668 = CARTESIAN_POINT ( 'NONE',  ( 56.62419727214309262, 14.29741701462000059, -25.88689047256800180 ) ) ;
#8669 = CARTESIAN_POINT ( 'NONE',  ( 20.06281976506910070, -10.10654536788180025, -32.14999999999999858 ) ) ;
#8670 = CARTESIAN_POINT ( 'NONE',  ( 50.21099649534220077, 18.14781963348989891, -76.14999999999999147 ) ) ;
#8671 = CARTESIAN_POINT ( 'NONE',  ( 53.22412257189229479, 18.23394763870219748, -48.94726806477149950 ) ) ;
#8672 = CARTESIAN_POINT ( 'NONE',  ( 71.29455428839979447, 0.9209334348186318797, -70.75011546227260339 ) ) ;
#8673 = CARTESIAN_POINT ( 'NONE',  ( 11.13393739769619906, -55.30245861064819479, -24.15000000000000213 ) ) ;
#8674 = CARTESIAN_POINT ( 'NONE',  ( 66.97218591609239979, -45.11618894467940066, -13.04694144512030007 ) ) ;
#8675 = EDGE_CURVE ( 'NONE', #10139, #39738, #45080, .T. ) ;
#8676 = ORIENTED_EDGE ( 'NONE', *, *, #4784, .T. ) ;
#8677 = DIRECTION ( 'NONE',  ( 0.5516667872527207805, -0.8340645993220556775, 0.000000000000000000 ) ) ;
#8678 = EDGE_CURVE ( 'NONE', #11745, #27748, #41994, .T. ) ;
#8680 = CARTESIAN_POINT ( 'NONE',  ( 73.01149271009099095, 1.265664290790580182, -68.85308916926389600 ) ) ;
#8679 = AXIS2_PLACEMENT_3D ( 'NONE', #29541, #9893, #21664 ) ;
#8681 = CARTESIAN_POINT ( 'NONE',  ( 47.64143405402000297, -54.53488714544450033, -55.14905519569939685 ) ) ;
#8682 = CARTESIAN_POINT ( 'NONE',  ( 11.89321892217540011, -65.43602743108330344, -18.17421237901570308 ) ) ;
#8683 = CARTESIAN_POINT ( 'NONE',  ( 73.10258273731270151, 1.278021359705829862, -62.63015105704819518 ) ) ;
#8684 = CARTESIAN_POINT ( 'NONE',  ( 41.06001733956060207, 13.06695014755839956, -3.719605790254209676 ) ) ;
#8685 = CARTESIAN_POINT ( 'NONE',  ( 57.18156601109950543, 18.52541442572180230, -52.05824807082350247 ) ) ;
#8686 = CARTESIAN_POINT ( 'NONE',  ( 71.54045699608269615, 0.8986939045430379913, -60.71074964625670134 ) ) ;
#8687 = CARTESIAN_POINT ( 'NONE',  ( 62.63393739769619373, -39.36618894467940066, 16.35000000000000142 ) ) ;
#8688 = AXIS2_PLACEMENT_3D ( 'NONE', #48416, #454, #36344 ) ;
#8689 = CARTESIAN_POINT ( 'NONE',  ( 71.95061440476429482, 1.334524132314490075, -61.18591595078659395 ) ) ;
#8690 = CIRCLE ( 'NONE', #35466, 34.47562460986249278 ) ;
#8691 = FACE_OUTER_BOUND ( 'NONE', #39688, .T. ) ;
#8692 = CARTESIAN_POINT ( 'NONE',  ( 65.07262241358380095, 1.198183261254780030, -70.68687062374729635 ) ) ;
#8693 = VERTEX_POINT ( 'NONE', #9513 ) ;
#8694 = EDGE_LOOP ( 'NONE', ( #23165, #14632, #16735, #39242, #37454 ) ) ;
#8695 = CARTESIAN_POINT ( 'NONE',  ( 20.99559283022811584, -9.290005664590468726, -55.50065785785324124 ) ) ;
#8696 = CARTESIAN_POINT ( 'NONE',  ( 16.13232929059349985, -51.04699384658444217, -15.66849738685780657 ) ) ;
#8697 = ORIENTED_EDGE ( 'NONE', *, *, #3799, .F. ) ;
#8698 = CARTESIAN_POINT ( 'NONE',  ( 16.13393739769620083, -15.61618894467929941, -11.23251175440650051 ) ) ;
#8699 = DIRECTION ( 'NONE',  ( 0.000000000000000000, -1.000000000000000000, 0.000000000000000000 ) ) ;
#8700 = CARTESIAN_POINT ( 'NONE',  ( 54.11862986506081796, 20.00205326672937645, -75.47294485644663098 ) ) ;
#8701 = CARTESIAN_POINT ( 'NONE',  ( 51.62918027504110086, 19.74959736141559929, -76.14997290609490221 ) ) ;
#8702 = EDGE_LOOP ( 'NONE', ( #5676, #3248, #30510, #48460, #4663 ) ) ;
#8703 = DIRECTION ( 'NONE',  ( 0.2956364143885911178, -0.8200397212266696823, 0.4900346580579206246 ) ) ;
#8704 = CARTESIAN_POINT ( 'NONE',  ( 41.81045037156589217, 6.360722813067012815, -81.26737402878971750 ) ) ;
#8705 = CARTESIAN_POINT ( 'NONE',  ( 61.28085239525059791, 14.36939662108470017, -47.67834120296360112 ) ) ;
#8706 = EDGE_CURVE ( 'NONE', #31690, #32099, #7081, .T. ) ;
#8707 = CARTESIAN_POINT ( 'NONE',  ( 17.88447765263330069, -23.67338007259600019, -46.22423246988029888 ) ) ;
#8708 = CARTESIAN_POINT ( 'NONE',  ( 18.20463661421896617, -23.32128348042572341, -67.92433352170111505 ) ) ;
#8709 = CARTESIAN_POINT ( 'NONE',  ( 41.63696876380908662, -37.56364127202510872, -82.13484301340810134 ) ) ;
#8710 = EDGE_CURVE ( 'NONE', #18800, #20534, #31289, .T. ) ;
#8711 = B_SPLINE_CURVE_WITH_KNOTS ( 'NONE', 3,
 ( #35161, #38603, #2693, #18666, #43050, #34640, #15519, #46733, #31472, #34904, #26778, #22840 ),
 .UNSPECIFIED., .F., .F.,
 ( 4, 2, 2, 2, 2, 4 ),
 ( 0.000000000000000000, 0.1250000000000000000, 0.2500000000000000000, 0.5000000000000000000, 0.7500000000000000000, 1.000000000000000000 ),
 .UNSPECIFIED. ) ;
#8712 = ORIENTED_EDGE ( 'NONE', *, *, #26234, .T. ) ;
#8713 = CARTESIAN_POINT ( 'NONE',  ( 23.83903802589029297, -17.68686261538724125, -41.87566431392930610 ) ) ;
#8714 = CARTESIAN_POINT ( 'NONE',  ( 14.99016206921919903, -22.97815008590309915, -34.78171861563929923 ) ) ;
#8715 = CARTESIAN_POINT ( 'NONE',  ( 24.04493703497947621, -14.58063303858524939, -33.46599845918103000 ) ) ;
#8716 = AXIS2_PLACEMENT_3D ( 'NONE', #49092, #40948, #32798 ) ;
#8717 = CARTESIAN_POINT ( 'NONE',  ( 13.83803551327370229, 20.84559406376729740, -75.48537863783369062 ) ) ;
#8718 = CARTESIAN_POINT ( 'NONE',  ( 24.04493739318474610, -15.62253491305603426, -59.79258081469907182 ) ) ;
#8719 = CARTESIAN_POINT ( 'NONE',  ( 83.10006388208900319, -44.89976216378850182, -46.45756164887509954 ) ) ;
#8720 = CARTESIAN_POINT ( 'NONE',  ( 64.93393739769619799, 1.396834109478129804, -70.23662692463440749 ) ) ;
#8721 = CARTESIAN_POINT ( 'NONE',  ( 23.49678657892749811, -19.32714200870689680, -41.65627172763429797 ) ) ;
#8722 = ORIENTED_EDGE ( 'NONE', *, *, #291, .F. ) ;
#8723 = CARTESIAN_POINT ( 'NONE',  ( 53.52135793756909976, -48.91598921442630399, -26.96728785596230082 ) ) ;
#8724 = CARTESIAN_POINT ( 'NONE',  ( 14.79734571143089994, -51.11619430643680317, -22.20703854455320325 ) ) ;
#8725 = CARTESIAN_POINT ( 'NONE',  ( 76.59936668305130070, 10.83832045962729929, -14.02863287010100102 ) ) ;
#8726 = CARTESIAN_POINT ( 'NONE',  ( 57.24929578234380045, 19.38381105828390361, -53.91492796160409284 ) ) ;
#8727 = DIRECTION ( 'NONE',  ( 0.000000000000000000, 0.000000000000000000, -1.000000000000000000 ) ) ;
#8728 = FACE_OUTER_BOUND ( 'NONE', #22182, .T. ) ;
#8729 = ORIENTED_EDGE ( 'NONE', *, *, #15618, .T. ) ;
#8730 = CARTESIAN_POINT ( 'NONE',  ( -11.32734370190460105, -41.88171845330919751, -6.430192534648670133 ) ) ;
#8731 = CARTESIAN_POINT ( 'NONE',  ( 47.35435173871399428, 23.44893959130619976, -54.68374326288559928 ) ) ;
#8732 = CARTESIAN_POINT ( 'NONE',  ( 29.13393739769619728, 4.555383930574479656, -84.63196841427449613 ) ) ;
#8733 = CARTESIAN_POINT ( 'NONE',  ( 63.41515590138089919, 1.383136297697689976, -62.73294707603399445 ) ) ;
#8734 = DIRECTION ( 'NONE',  ( -0.6522074047277892639, -0.2731766849828938248, 0.7071067811865464625 ) ) ;
#8735 = CARTESIAN_POINT ( 'NONE',  ( 41.40756461421400303, 13.53921217941219979, -5.393981499654319833 ) ) ;
#8736 = FACE_OUTER_BOUND ( 'NONE', #37629, .T. ) ;
#8737 = DIRECTION ( 'NONE',  ( 0.3535533905932736198, -0.6123724356957950254, 0.7071067811865472397 ) ) ;
#8738 = CARTESIAN_POINT ( 'NONE',  ( -3.839728563314090071, -24.83858928721370063, -54.64999999999999858 ) ) ;
#8739 = CARTESIAN_POINT ( 'NONE',  ( 59.91112534698100234, -46.04755292983879400, -47.70997890928379803 ) ) ;
#8740 = CARTESIAN_POINT ( 'NONE',  ( -0.2544260390843469111, -20.43873413140054041, -34.98772936183320326 ) ) ;
#8741 = CIRCLE ( 'NONE', #26301, 21.50000000000000000 ) ;
#8742 = EDGE_CURVE ( 'NONE', #37946, #41163, #48901, .T. ) ;
#8743 = CARTESIAN_POINT ( 'NONE',  ( 64.93408011569830762, 1.389468113695450091, -61.03004030278179926 ) ) ;
#8744 = CARTESIAN_POINT ( 'NONE',  ( 17.86672151352269822, -52.48721817738829287, -75.97756937697440094 ) ) ;
#8745 = CYLINDRICAL_SURFACE ( 'NONE', #14536, 1.999999999999999778 ) ;
#8746 = CARTESIAN_POINT ( 'NONE',  ( 22.89998043194958655, -16.40826371516535431, -60.88444288611811572 ) ) ;
#8747 = ORIENTED_EDGE ( 'NONE', *, *, #47880, .T. ) ;
#8748 = FACE_OUTER_BOUND ( 'NONE', #35864, .T. ) ;
#8749 = CARTESIAN_POINT ( 'NONE',  ( 8.975705354591740459, 32.03333151996960027, -46.63325874977040542 ) ) ;
#8750 = FACE_OUTER_BOUND ( 'NONE', #19333, .T. ) ;
#8751 = CARTESIAN_POINT ( 'NONE',  ( 67.98302783225990709, -31.38011479710340623, -18.18687859448679944 ) ) ;
#8752 = ORIENTED_EDGE ( 'NONE', *, *, #39577, .F. ) ;
#8754 = B_SPLINE_CURVE_WITH_KNOTS ( 'NONE', 3,
 ( #42858, #14288, #6171, #26061, #38137, #10626, #2237, #26580, #10363, #6693, #21872, #38670, #37883, #18213, #26324, #42333, #6432, #42596 ),
 .UNSPECIFIED., .F., .F.,
 ( 4, 2, 2, 2, 2, 2, 2, 2, 4 ),
 ( 0.4999987983750606158, 0.5624989485781780596, 0.6249990987812954479, 0.6874992489844128363, 0.7499993991875302246, 0.8124995493906477240, 0.8749996995937651123, 0.9374998497968825006, 1.000000000000000000 ),
 .UNSPECIFIED. ) ;
#8753 = CARTESIAN_POINT ( 'NONE',  ( 18.54732536477180105, 20.81202934652590031, -75.33782839756391070 ) ) ;
#8755 = ORIENTED_EDGE ( 'NONE', *, *, #41887, .F. ) ;
#8756 = EDGE_LOOP ( 'NONE', ( #29173, #16800, #19117, #28911 ) ) ;
#8757 = AXIS2_PLACEMENT_3D ( 'NONE', #39722, #51771, #15102 ) ;
#8758 = ORIENTED_EDGE ( 'NONE', *, *, #42309, .F. ) ;
#8759 = CARTESIAN_POINT ( 'NONE',  ( 10.80918145290640098, -64.05807750357701025, -45.60126697491269709 ) ) ;
#8760 = PLANE ( 'NONE',  #49477 ) ;
#8761 = CARTESIAN_POINT ( 'NONE',  ( 21.15506732860339767, -20.52346999403679817, -81.23899999999999011 ) ) ;
#8762 = CARTESIAN_POINT ( 'NONE',  ( 61.49527322741659674, 13.95390136402409986, -46.82383681851589330 ) ) ;
#8763 = EDGE_LOOP ( 'NONE', ( #11606, #46092, #45528, #44777, #5202 ) ) ;
#8764 = CARTESIAN_POINT ( 'NONE',  ( 75.24686161380772376, 2.959163858433984551, -12.27461306487479042 ) ) ;
#8765 = DIRECTION ( 'NONE',  ( 0.000000000000000000, 0.000000000000000000, -1.000000000000000000 ) ) ;
#8766 = ORIENTED_EDGE ( 'NONE', *, *, #11824, .T. ) ;
#8767 = CARTESIAN_POINT ( 'NONE',  ( 50.59865144046819552, -46.19777500518519986, -12.88937842738419981 ) ) ;
#8768 = CARTESIAN_POINT ( 'NONE',  ( 14.90064330294591954, -52.99263552515018461, -76.14999999999999147 ) ) ;
#8769 = EDGE_CURVE ( 'NONE', #19, #34516, #17366, .T. ) ;
#8770 = CARTESIAN_POINT ( 'NONE',  ( 10.47385409520754784, -55.21366976880749888, -45.62050209441289894 ) ) ;
#8771 = ORIENTED_EDGE ( 'NONE', *, *, #11966, .T. ) ;
#8772 = ORIENTED_EDGE ( 'NONE', *, *, #5628, .T. ) ;
#8773 = CARTESIAN_POINT ( 'NONE',  ( 55.98803936394586600, 15.85709954156585333, 10.84999999999999964 ) ) ;
#8774 = DIRECTION ( 'NONE',  ( 1.000000000000000000, 0.000000000000000000, 0.000000000000000000 ) ) ;
#8775 = CARTESIAN_POINT ( 'NONE',  ( 60.74502025776879321, 14.51238070346370002, -47.75426036517409756 ) ) ;
#8776 = FACE_OUTER_BOUND ( 'NONE', #31817, .T. ) ;
#8777 = AXIS2_PLACEMENT_3D ( 'NONE', #11555, #3948, #23567 ) ;
#8778 = DIRECTION ( 'NONE',  ( 0.000000000000000000, 0.000000000000000000, 1.000000000000000000 ) ) ;
#8779 = CARTESIAN_POINT ( 'NONE',  ( -5.332450679183510012, 15.75303166516230036, -4.673630178135430135 ) ) ;
#8780 = CARTESIAN_POINT ( 'NONE',  ( 21.12773481075143422, -20.59660524975024387, -55.09675274900580177 ) ) ;
#8781 = CARTESIAN_POINT ( 'NONE',  ( 61.28115109886760337, 13.99884544370929973, -28.05810216926879974 ) ) ;
#8782 = CARTESIAN_POINT ( 'NONE',  ( 23.97508750825819845, -15.93730127209270009, -63.30053379854238926 ) ) ;
#8783 = B_SPLINE_SURFACE_WITH_KNOTS ( 'NONE', 3, 3, ( 
 ( #15576, #24168, #31532, #11910, #7453, #31270, #15053, #39426, #39678, #35486, #23913, #16080, #43104, #50955, #23405, #19995 ),
 ( #108, #3526, #32039, #48061, #12161, #44123, #7719, #23664, #19238, #7196, #40192, #3784, #31020, #15317, #19753, #47045 ),
 ( #3262, #35745, #15822, #35220, #51223, #47302, #11392, #27354, #36245, #32292, #17379, #16863, #37033, #13463, #32542, #13207 ),
 ( #21288, #44898, #48578, #28633, #33078, #32811, #25474, #41222, #12940, #37294, #12679, #354, #9527, #8483, #8739, #16337 ),
 ( #29418, #44634, #24689, #45422, #48314, #12410, #41479, #24429, #1392, #9270, #40704, #28374, #25217, #4803, #5337, #36758 ),
 ( #36500, #28896, #5594, #33346, #604, #48837, #29157, #44381, #40443, #20770, #870, #9005, #45156, #24948, #40959, #5076 ),
 ( #49106, #4534, #49362, #20508, #16589, #21032, #1130, #17125, #5844, #25996, #21810, #6107, #10295, #21548, #6363, #2690 ),
 ( #22063, #42264, #30708, #37817, #30448, #41739, #1910, #38073, #22323, #38329, #26259, #2419, #14738, #18662, #49622, #25731 ) ),
 .UNSPECIFIED., .F., .F., .F.,
 ( 4, 1, 3, 4 ),
 ( 4, 2, 2, 2, 2, 2, 2, 4 ),
 ( 0.000000000000000000, 0.5000000000000000000, 1.000000000000000000, 1.010000000000000009 ),
 ( 0.000000000000000000, 1.372899869568840137, 2.941928291933239681, 3.922571055910980320, 4.412892437899860631, 5.197406649082060071, 6.452629386973570469, 7.845142111821970410 ),
 .UNSPECIFIED. ) ;
#8784 = EDGE_LOOP ( 'NONE', ( #29057, #24703, #39082, #894 ) ) ;
#8785 = CARTESIAN_POINT ( 'NONE',  ( 59.77423841227909662, 14.93359823389899788, -47.80915357183090464 ) ) ;
#8786 = AXIS2_PLACEMENT_3D ( 'NONE', #46976, #51148, #15246 ) ;
#8787 = CARTESIAN_POINT ( 'NONE',  ( 15.87259861546077389, -15.80606268419046678, -24.90346750000000142 ) ) ;
#8788 = CARTESIAN_POINT ( 'NONE',  ( -28.43713041416927823, -60.18725675654476959, 16.35000000000000142 ) ) ;
#8789 = CARTESIAN_POINT ( 'NONE',  ( 72.52593196779452001, 1.270920007605160107, -69.64171779669759133 ) ) ;
#8790 = CARTESIAN_POINT ( 'NONE',  ( 43.55496689572915159, -39.91667278102725192, -68.81525705887698052 ) ) ;
#8791 = CARTESIAN_POINT ( 'NONE',  ( 11.22384634879449905, -65.01277928531338546, -16.94931743789749845 ) ) ;
#8792 = CARTESIAN_POINT ( 'NONE',  ( -0.03447620312153643757, -27.09132598751343579, -34.79644660940672907 ) ) ;
#8793 = CARTESIAN_POINT ( 'NONE',  ( 49.66352655669079752, -53.65682907869459939, -54.86856413023180323 ) ) ;
#8794 = CARTESIAN_POINT ( 'NONE',  ( -6.178851728588689696, 15.46435443030710033, -5.588668033364348808 ) ) ;
#8795 = EDGE_CURVE ( 'NONE', #10642, #15006, #33834, .T. ) ;
#8796 = CARTESIAN_POINT ( 'NONE',  ( 14.26078212116266108, -23.32907417233825598, -34.08344229577145512 ) ) ;
#8797 = DIRECTION ( 'NONE',  ( 0.000000000000000000, -1.000000000000000000, 0.000000000000000000 ) ) ;
#8798 = CARTESIAN_POINT ( 'NONE',  ( 14.62412072909329552, -22.50552946476252458, -71.41585254811130312 ) ) ;
#8799 = ORIENTED_EDGE ( 'NONE', *, *, #41882, .F. ) ;
#8800 = ADVANCED_FACE ( 'NONE', ( #16849 ), #50583, .F. ) ;
#8801 = CARTESIAN_POINT ( 'NONE',  ( 8.741056682034429315, -14.69314557498439910, -40.10688088744169733 ) ) ;
#8802 = ADVANCED_FACE ( 'NONE', ( #28884 ), #49862, .T. ) ;
#8803 = CARTESIAN_POINT ( 'NONE',  ( 64.18351159802539030, 1.441354674475120001, -61.42706364365079708 ) ) ;
#8804 = VERTEX_POINT ( 'NONE', #33596 ) ;
#8805 = CARTESIAN_POINT ( 'NONE',  ( 21.98073010695431151, -11.67187985524638805, -34.65826853459201118 ) ) ;
#8806 = CARTESIAN_POINT ( 'NONE',  ( 61.18220403599099910, -45.50035139021139940, -47.53341915241229998 ) ) ;
#8807 = CARTESIAN_POINT ( 'NONE',  ( 57.24507233897389824, 19.38381439978470056, -53.91419826472959898 ) ) ;
#8808 = CARTESIAN_POINT ( 'NONE',  ( 13.61804212000129866, 18.93546666416320079, -20.94890277169909965 ) ) ;
#8810 = PLANE ( 'NONE',  #34875 ) ;
#8809 = CARTESIAN_POINT ( 'NONE',  ( 40.97558342559717914, 8.414888246701108798, -81.27204827182337965 ) ) ;
#8811 = EDGE_CURVE ( 'NONE', #27118, #35815, #45742, .T. ) ;
#8812 = CARTESIAN_POINT ( 'NONE',  ( -30.36606260230379917, 21.88381105532059934, 11.84999999999999964 ) ) ;
#8813 = CARTESIAN_POINT ( 'NONE',  ( 24.04504587474531263, -15.61618895646369687, -51.50767080737492165 ) ) ;
#8814 = ORIENTED_EDGE ( 'NONE', *, *, #46767, .T. ) ;
#8815 = CARTESIAN_POINT ( 'NONE',  ( 83.82017571155999747, -44.67807987934809688, -47.23783155238629661 ) ) ;
#8816 = CIRCLE ( 'NONE', #48162, 17.19098300562509962 ) ;
#8817 = ORIENTED_EDGE ( 'NONE', *, *, #27750, .F. ) ;
#8818 = ORIENTED_EDGE ( 'NONE', *, *, #47790, .F. ) ;
#8819 = ORIENTED_EDGE ( 'NONE', *, *, #13620, .T. ) ;
#8820 = CARTESIAN_POINT ( 'NONE',  ( 61.60870436204309897, -45.23813693204910180, -47.07717016886380179 ) ) ;
#8821 = DIRECTION ( 'NONE',  ( 0.06672502100504951184, 0.04847856544221944286, 0.9965929962951476373 ) ) ;
#8822 = CARTESIAN_POINT ( 'NONE',  ( 76.40019456172100831, -19.50358666587276346, -12.79738190608483883 ) ) ;
#8823 = CARTESIAN_POINT ( 'NONE',  ( 54.77086636619779370, -51.21734551792319223, -53.06498560372880746 ) ) ;
#8824 = EDGE_CURVE ( 'NONE', #9855, #20898, #49610, .T. ) ;
#8825 = EDGE_LOOP ( 'NONE', ( #14284, #42572, #14942, #24444, #4212, #20668, #37315, #43274, #13344, #43244 ) ) ;
#8826 = EDGE_LOOP ( 'NONE', ( #42454, #51208, #21685, #19193, #8889, #39635, #27809 ) ) ;
#8827 = CARTESIAN_POINT ( 'NONE',  ( -0.007164427059776000244, 14.47565373231149977, -34.77269723891829756 ) ) ;
#8828 = CARTESIAN_POINT ( 'NONE',  ( -16.19549477698355844, 6.204146130383243474, -49.15060503604010478 ) ) ;
#8829 = DIRECTION ( 'NONE',  ( -0.2846079131720410937, -0.9586440088791334801, 0.000000000000000000 ) ) ;
#8830 = DIRECTION ( 'NONE',  ( -1.000000000000000000, 0.000000000000000000, 0.000000000000000000 ) ) ;
#8831 = DIRECTION ( 'NONE',  ( -1.000000000000000000, 0.000000000000000000, 0.000000000000000000 ) ) ;
#8832 = EDGE_CURVE ( 'NONE', #41771, #33944, #9303, .T. ) ;
#8833 = CARTESIAN_POINT ( 'NONE',  ( 18.63393739769599833, 14.38381105532070059, -35.14999999999999858 ) ) ;
#8834 = ORIENTED_EDGE ( 'NONE', *, *, #22027, .T. ) ;
#8835 = CARTESIAN_POINT ( 'NONE',  ( 7.542479837843401924, 28.49039248266597824, -11.77476003560691176 ) ) ;
#8836 = DIRECTION ( 'NONE',  ( 0.6888026391158329487, -0.7071067811865494601, 0.1598465650148944150 ) ) ;
#8837 = CARTESIAN_POINT ( 'NONE',  ( 19.12892251208798911, -9.528728375619987645, -34.09841683067057971 ) ) ;
#8838 = CARTESIAN_POINT ( 'NONE',  ( 60.56956494586819417, 14.37343996889240039, -47.17558661336109793 ) ) ;
#8839 = CARTESIAN_POINT ( 'NONE',  ( 8.587688456862030861, -13.46192003979740015, -69.10100965672640427 ) ) ;
#8840 = CARTESIAN_POINT ( 'NONE',  ( 19.13393739769600188, 18.38381105532069881, -35.14999999999999858 ) ) ;
#8841 = DIRECTION ( 'NONE',  ( 0.000000000000000000, -1.000000000000000000, 0.000000000000000000 ) ) ;
#8842 = CARTESIAN_POINT ( 'NONE',  ( 42.31976156911279929, -43.87010827594590268, -4.715714940980549663 ) ) ;
#8843 = CARTESIAN_POINT ( 'NONE',  ( 66.63393739769620083, 11.88381105532070059, -71.50000000000000000 ) ) ;
#8844 = CARTESIAN_POINT ( 'NONE',  ( 68.13393739769745139, -49.21324915460109395, -75.95351669811962836 ) ) ;
#8845 = CARTESIAN_POINT ( 'NONE',  ( 68.38971107296249841, -1.116188944679350037, -18.15384911730639672 ) ) ;
#8846 = EDGE_CURVE ( 'NONE', #21618, #28130, #17945, .T. ) ;
#8847 = CARTESIAN_POINT ( 'NONE',  ( 64.11159536369549983, 1.443019942996689897, -69.80885301619480288 ) ) ;
#8848 = CIRCLE ( 'NONE', #44830, 1.500000000000001332 ) ;
#8849 = DIRECTION ( 'NONE',  ( 0.000000000000000000, 0.000000000000000000, -1.000000000000000000 ) ) ;
#8850 = CARTESIAN_POINT ( 'NONE',  ( 67.20513489140449792, 1.550091694609170068, -19.24943083180730241 ) ) ;
#8851 = ORIENTED_EDGE ( 'NONE', *, *, #11966, .F. ) ;
#8852 = AXIS2_PLACEMENT_3D ( 'NONE', #20627, #465, #32406 ) ;
#8853 = CARTESIAN_POINT ( 'NONE',  ( 13.83004271473379987, -51.93606027628250388, -75.41551559479479749 ) ) ;
#8854 = CARTESIAN_POINT ( 'NONE',  ( 47.32093757237190346, -54.70280804132740116, -54.63841117994249430 ) ) ;
#8855 = CARTESIAN_POINT ( 'NONE',  ( 9.367501421782780113, -15.61622054991689978, -37.45282021618999835 ) ) ;
#8856 = DIRECTION ( 'NONE',  ( -1.000000000000000000, 0.000000000000000000, 0.000000000000000000 ) ) ;
#8857 = FACE_OUTER_BOUND ( 'NONE', #35496, .T. ) ;
#8858 = CARTESIAN_POINT ( 'NONE',  ( 22.96203127631590135, -18.80250976734449964, -32.14999999999999858 ) ) ;
#8859 = CARTESIAN_POINT ( 'NONE',  ( 55.13250725764758187, -46.09227360768333170, -16.25833532637385304 ) ) ;
#8860 = VECTOR ( 'NONE', #31060, 1000.000000000000000 ) ;
#8861 = CARTESIAN_POINT ( 'NONE',  ( 47.78697217749750337, -54.43650991200640021, -54.82585106944300435 ) ) ;
#8863 = CARTESIAN_POINT ( 'NONE',  ( -7.625187662226220020, -45.45404276017920608, -5.684751090845729493 ) ) ;
#8862 = CARTESIAN_POINT ( 'NONE',  ( 47.46022127273401026, 23.07192594333263358, -75.17786410066094049 ) ) ;
#8864 = CARTESIAN_POINT ( 'NONE',  ( 56.28151124241350800, 19.36078090757409953, -52.90566144362949785 ) ) ;
#8865 = CARTESIAN_POINT ( 'NONE',  ( 48.54525988008339255, 22.76209179570290075, -54.56845936111729856 ) ) ;
#8866 = ORIENTED_EDGE ( 'NONE', *, *, #34767, .F. ) ;
#8867 = CARTESIAN_POINT ( 'NONE',  ( 21.40734412481930349, -20.29953610934510166, -65.07833806302160440 ) ) ;
#8868 = ORIENTED_EDGE ( 'NONE', *, *, #51660, .F. ) ;
#8869 = AXIS2_PLACEMENT_3D ( 'NONE', #4675, #37425, #45035 ) ;
#8870 = CARTESIAN_POINT ( 'NONE',  ( 2.558369240368460140, -6.046280207075140467, -34.64999999999999858 ) ) ;
#8871 = CARTESIAN_POINT ( 'NONE',  ( 22.90105422030644533, -15.61618894250064571, -66.84718200393152188 ) ) ;
#8872 = DIRECTION ( 'NONE',  ( 0.6566103562584382214, -0.5836782507651213647, 0.4776845608117712971 ) ) ;
#8874 = CARTESIAN_POINT ( 'NONE',  ( 52.62011612078570266, 18.57322221019510167, -27.98591982627220176 ) ) ;
#8873 = CARTESIAN_POINT ( 'NONE',  ( 83.71674455129429759, 13.26039317643239990, -46.72760658838089398 ) ) ;
#8875 = CARTESIAN_POINT ( 'NONE',  ( 11.74162816692980016, -10.09802092277660002, -65.73882677097459748 ) ) ;
#8877 = EDGE_CURVE ( 'NONE', #51503, #46428, #15419, .T. ) ;
#8876 = LINE ( 'NONE', #41100, #8355 ) ;
#8878 = CARTESIAN_POINT ( 'NONE',  ( 56.83984272715319719, -45.11618894467940066, -15.86913725221539906 ) ) ;
#8879 = CARTESIAN_POINT ( 'NONE',  ( 63.93393739769619089, 10.88381105532070059, -68.84999999999999432 ) ) ;
#8880 = AXIS2_PLACEMENT_3D ( 'NONE', #49863, #17876, #29911 ) ;
#8881 = ORIENTED_EDGE ( 'NONE', *, *, #4594, .F. ) ;
#8882 = ORIENTED_EDGE ( 'NONE', *, *, #32512, .T. ) ;
#8883 = CARTESIAN_POINT ( 'NONE',  ( 12.01222358505219923, -65.01572836191429872, -16.39655052253609924 ) ) ;
#8884 = CARTESIAN_POINT ( 'NONE',  ( 12.30426158441329854, 34.20084824820960279, -47.48507929029160124 ) ) ;
#8885 = CARTESIAN_POINT ( 'NONE',  ( 61.04001029137710077, -45.35933836075930259, -46.86320535112459851 ) ) ;
#8886 = DIRECTION ( 'NONE',  ( 1.000000000000000000, 0.000000000000000000, 0.000000000000000000 ) ) ;
#8887 = CARTESIAN_POINT ( 'NONE',  ( 9.807872506304869731, -20.47799571592583234, -64.29933550135423559 ) ) ;
#8888 = VECTOR ( 'NONE', #29275, 1000.000000000000114 ) ;
#8889 = ORIENTED_EDGE ( 'NONE', *, *, #42779, .F. ) ;
#8890 = CARTESIAN_POINT ( 'NONE',  ( 12.54923789920940180, 19.17756050559142267, -21.20205464577261267 ) ) ;
#8891 = VECTOR ( 'NONE', #11393, 1000.000000000000000 ) ;
#8892 = DIRECTION ( 'NONE',  ( 1.000000000000000000, 0.000000000000000000, 0.000000000000000000 ) ) ;
#8893 = CARTESIAN_POINT ( 'NONE',  ( 24.04475233726670780, -15.61618925176752271, -59.50766149565701113 ) ) ;
#8894 = CARTESIAN_POINT ( 'NONE',  ( 57.50723796702470025, 13.88381105532070059, -17.93019253464870033 ) ) ;
#8895 = EDGE_CURVE ( 'NONE', #24585, #17738, #22093, .T. ) ;
#8896 = CARTESIAN_POINT ( 'NONE',  ( 50.36549737501839985, -50.07561419642740219, -76.14999999999999147 ) ) ;
#8897 = CARTESIAN_POINT ( 'NONE',  ( 24.04493737916699914, -16.65173673504433793, -43.54933322766937920 ) ) ;
#8898 = VERTEX_POINT ( 'NONE', #26761 ) ;
#8899 = CARTESIAN_POINT ( 'NONE',  ( 54.18928026078430094, -48.04840664809780293, -26.03349461057250025 ) ) ;
#8900 = DIRECTION ( 'NONE',  ( 1.000000000000000000, 2.460964292799963328E-14, 0.000000000000000000 ) ) ;
#8901 = ORIENTED_EDGE ( 'NONE', *, *, #48319, .T. ) ;
#8902 = CYLINDRICAL_SURFACE ( 'NONE', #14303, 2.999999999999999112 ) ;
#8903 = CARTESIAN_POINT ( 'NONE',  ( 51.61135292554669718, -46.21249342017139838, -13.62812988203759801 ) ) ;
#8904 = CARTESIAN_POINT ( 'NONE',  ( 23.95747192159750227, -15.00051440004449965, -35.98749647213350045 ) ) ;
#8905 = CARTESIAN_POINT ( 'NONE',  ( 14.34417029580689906, -51.11618894467930119, -22.49240189290920000 ) ) ;
#8906 = PRESENTATION_LAYER_ASSIGNMENT (  '', '', ( #33969 ) ) ;
#8907 = CARTESIAN_POINT ( 'NONE',  ( 16.13393739769620083, -15.61618894467929941, -13.15000000000000036 ) ) ;
#8908 = CARTESIAN_POINT ( 'NONE',  ( 47.43257551170959374, -54.63067240927929902, -74.36142533359220863 ) ) ;
#8909 = VERTEX_POINT ( 'NONE', #43291 ) ;
#8910 = FACE_OUTER_BOUND ( 'NONE', #25008, .T. ) ;
#8911 = CARTESIAN_POINT ( 'NONE',  ( 15.74786552489070068, -8.175917288739990241, -61.71615517726989708 ) ) ;
#8912 = AXIS2_PLACEMENT_3D ( 'NONE', #20073, #36066, #14868 ) ;
#8913 = EDGE_CURVE ( 'NONE', #34714, #3421, #30695, .T. ) ;
#8914 = FACE_OUTER_BOUND ( 'NONE', #41561, .T. ) ;
#8915 = CARTESIAN_POINT ( 'NONE',  ( 30.13393739769619728, 7.383811055320659733, -72.14999999999999147 ) ) ;
#8916 = AXIS2_PLACEMENT_3D ( 'NONE', #27615, #11650, #39172 ) ;
#8917 = EDGE_CURVE ( 'NONE', #18483, #2702, #11060, .T. ) ;
#8918 = CARTESIAN_POINT ( 'NONE',  ( 47.09511218098770513, 22.86011577770599956, -75.60848552117779775 ) ) ;
#8919 = CARTESIAN_POINT ( 'NONE',  ( 19.84371743758253714, -54.58381977003536178, -17.84615285344403546 ) ) ;
#8920 = EDGE_CURVE ( 'NONE', #23175, #48985, #28506, .T. ) ;
#8921 = CARTESIAN_POINT ( 'NONE',  ( 55.91595717589669334, 14.67227259378219983, -17.93019253464870033 ) ) ;
#8922 = CARTESIAN_POINT ( 'NONE',  ( 28.63710131890649890, -4.677486598597970335, -34.65001001049759566 ) ) ;
#8923 = CONICAL_SURFACE ( 'NONE', #33995, 3.567506086244480734, 0.04995839572194331335 ) ;
#8924 = CARTESIAN_POINT ( 'NONE',  ( 9.351992365096680970, -20.30531804342160029, -80.31511008668059048 ) ) ;
#8925 = VECTOR ( 'NONE', #49178, 1000.000000000000000 ) ;
#8926 = CARTESIAN_POINT ( 'NONE',  ( 63.78749078828948882, 1.530257664727401767, -62.44999999999999574 ) ) ;
#8928 = CARTESIAN_POINT ( 'NONE',  ( 42.87338644773151941, -39.93353782726089918, -71.78159119793272680 ) ) ;
#8927 = SURFACE_STYLE_FILL_AREA ( #44044 ) ;
#8929 = CARTESIAN_POINT ( 'NONE',  ( 63.15271035305199376, 0.9966178393190270324, -68.98171082814549493 ) ) ;
#8930 = CARTESIAN_POINT ( 'NONE',  ( 8.222937397696199469, -15.61618894467929941, -32.14999999999999858 ) ) ;
#8931 = CARTESIAN_POINT ( 'NONE',  ( 13.10176660314340147, -65.52395148895190857, -47.73582792185870005 ) ) ;
#8932 = VERTEX_POINT ( 'NONE', #30433 ) ;
#8933 = EDGE_CURVE ( 'NONE', #39703, #8293, #24127, .T. ) ;
#8934 = CARTESIAN_POINT ( 'NONE',  ( 52.76444823262289674, -49.70074108386170053, -48.64234372005410023 ) ) ;
#8935 = CARTESIAN_POINT ( 'NONE',  ( 57.94110753308110162, -45.18729252235269911, -25.80829669411419758 ) ) ;
#8936 = CARTESIAN_POINT ( 'NONE',  ( 8.222961546152424361, -16.65191320241268258, -74.75066484206243445 ) ) ;
#8937 = CARTESIAN_POINT ( 'NONE',  ( 13.21390947859770115, 19.65074986685339908, -21.61005117736269909 ) ) ;
#8938 = CARTESIAN_POINT ( 'NONE',  ( 56.21969265526590220, 14.80816776983419913, -26.07003510870140062 ) ) ;
#8939 = CARTESIAN_POINT ( 'NONE',  ( 13.97436713976919975, -8.902113059071330881, -37.85376303658059527 ) ) ;
#8940 = CARTESIAN_POINT ( 'NONE',  ( 51.07962909496099968, 18.40003410206369949, -76.32455169463339928 ) ) ;
#8942 = EDGE_CURVE ( 'NONE', #28918, #44905, #34100, .T. ) ;
#8941 = CARTESIAN_POINT ( 'NONE',  ( 52.73800103340319367, 18.49116459405509971, -48.71589999865829412 ) ) ;
#8943 = CARTESIAN_POINT ( 'NONE',  ( 71.25020460053529803, 1.328674444234379859, -70.47425850519080370 ) ) ;
#8944 = CARTESIAN_POINT ( 'NONE',  ( 8.133937397696209715, -59.33545798990849818, -21.14999999999999858 ) ) ;
#8945 = CARTESIAN_POINT ( 'NONE',  ( 72.29879703195499019, -43.70058892286719754, -12.53766171548880060 ) ) ;
#8946 = EDGE_LOOP ( 'NONE', ( #8074, #19882, #31167, #41628, #26130, #26923, #11996 ) ) ;
#8947 = CARTESIAN_POINT ( 'NONE',  ( 23.18909320594459800, -13.22213989345240037, -74.96321055543420186 ) ) ;
#8948 = CARTESIAN_POINT ( 'NONE',  ( 72.96606887121211571, 1.263738073398970041, -68.93858679394679712 ) ) ;
#8949 = CARTESIAN_POINT ( 'NONE',  ( 47.42745323055219586, -54.62870758109379921, -54.65928341309859917 ) ) ;
#8950 = DIRECTION ( 'NONE',  ( -1.000000000000000000, 0.000000000000000000, 0.000000000000000000 ) ) ;
#8951 = CYLINDRICAL_SURFACE ( 'NONE', #5637, 7.910999999999997812 ) ;
#8952 = CARTESIAN_POINT ( 'NONE',  ( 57.29122018273359629, 19.04244741251779871, -52.77760329876059586 ) ) ;
#8953 = CARTESIAN_POINT ( 'NONE',  ( 71.29339335573889969, 1.327097482837290121, -60.84525133028229504 ) ) ;
#8954 = CARTESIAN_POINT ( 'NONE',  ( 24.04473007462266310, -15.61618926727986789, -75.50766188105974663 ) ) ;
#8955 = CARTESIAN_POINT ( 'NONE',  ( 71.75685251123249486, 1.434949534324269971, -61.23975123050709612 ) ) ;
#8956 = CARTESIAN_POINT ( 'NONE',  ( 20.11801501725389940, -22.52874440175187942, -71.84094734006453109 ) ) ;
#8957 = CARTESIAN_POINT ( 'NONE',  ( 64.86758340617990370, 0.9945465939392450494, -70.67393287070269992 ) ) ;
#8958 = EDGE_LOOP ( 'NONE', ( #22452, #21303, #16880, #23682, #21954 ) ) ;
#8959 = ORIENTED_EDGE ( 'NONE', *, *, #10497, .F. ) ;
#8960 = CARTESIAN_POINT ( 'NONE',  ( 8.800117217589539464, -63.19572640051600132, -46.67015592357310538 ) ) ;
#8961 = CARTESIAN_POINT ( 'NONE',  ( 48.82567944625920120, -28.11618896394480061, -15.64999999241030082 ) ) ;
#8962 = ORIENTED_EDGE ( 'NONE', *, *, #28302, .T. ) ;
#8963 = CARTESIAN_POINT ( 'NONE',  ( 11.14351463905549977, -63.74727278248460038, -43.82532547204769457 ) ) ;
#8964 = CARTESIAN_POINT ( 'NONE',  ( 20.29256136589905424, -10.20483249692997241, -70.16115577048812213 ) ) ;
#8965 = DIRECTION ( 'NONE',  ( -0.3502816565540492477, 0.000000000000000000, 0.9366444154970182678 ) ) ;
#8966 = CARTESIAN_POINT ( 'NONE',  ( 53.10072982268869879, 19.49376234953830078, -76.45474630841620467 ) ) ;
#8967 = ORIENTED_EDGE ( 'NONE', *, *, #16744, .F. ) ;
#8968 = LINE ( 'NONE', #567, #6754 ) ;
#8969 = CARTESIAN_POINT ( 'NONE',  ( 41.61626771661330082, 6.328436186825659782, -82.23834840541459812 ) ) ;
#8970 = AXIS2_PLACEMENT_3D ( 'NONE', #34764, #27162, #11201 ) ;
#8971 = CARTESIAN_POINT ( 'NONE',  ( 16.13393739769620083, -15.61618894467929941, -7.225658350974740074 ) ) ;
#8972 = CARTESIAN_POINT ( 'NONE',  ( 11.38066761511700165, -8.879042187338029635, -55.09675274900569519 ) ) ;
#8973 = DIRECTION ( 'NONE',  ( 1.000000000000000000, 0.000000000000000000, 0.000000000000000000 ) ) ;
#8974 = CARTESIAN_POINT ( 'NONE',  ( 24.04460491192063998, -15.61619351124008404, -49.79233069347445451 ) ) ;
#8975 = ORIENTED_EDGE ( 'NONE', *, *, #35399, .F. ) ;
#8976 = CARTESIAN_POINT ( 'NONE',  ( 20.11811545784118138, -22.52868417623059472, -42.12566445783141234 ) ) ;
#8977 = CARTESIAN_POINT ( 'NONE',  ( 23.38515334021269965, -17.32690840498830198, -34.30640502925760416 ) ) ;
#8978 = CARTESIAN_POINT ( 'NONE',  ( 43.88918661166069768, 14.83350785940550054, -8.216749244412550723 ) ) ;
#8979 = EDGE_CURVE ( 'NONE', #10190, #14553, #19166, .T. ) ;
#8980 = CARTESIAN_POINT ( 'NONE',  ( 14.41339629623599983, 20.77357945327109690, -75.79069550273320033 ) ) ;
#8981 = EDGE_CURVE ( 'NONE', #2493, #19930, #33003, .T. ) ;
#8982 = DIRECTION ( 'NONE',  ( 1.000000000000000000, 2.460964292799963328E-14, 0.000000000000000000 ) ) ;
#8983 =( BOUNDED_CURVE ( )  B_SPLINE_CURVE ( 3, ( #28742, #3627, #23767, #48414 ),
 .UNSPECIFIED., .F., .T. ) 
 B_SPLINE_CURVE_WITH_KNOTS ( ( 4, 4 ),
 ( 0.5134355670272889860, 0.7048181067645971076 ),
 .UNSPECIFIED. ) 
 CURVE ( )  GEOMETRIC_REPRESENTATION_ITEM ( )  RATIONAL_B_SPLINE_CURVE ( ( 1.000000000000000000, 0.9969500553388705999, 0.9969500553388705999, 1.000000000000000000 ) ) 
 REPRESENTATION_ITEM ( '' )  );
#8984 = CARTESIAN_POINT ( 'NONE',  ( 83.84453551654038961, -44.32823745891949585, -46.66649649553739465 ) ) ;
#8985 = CARTESIAN_POINT ( 'NONE',  ( 24.34665199147069714, -14.88540873820230104, -51.47941917952310575 ) ) ;
#8986 = EDGE_LOOP ( 'NONE', ( #32532, #24712, #19269, #37119 ) ) ;
#8987 = CARTESIAN_POINT ( 'NONE',  ( 53.59970586858850083, -48.90735548451660009, -27.06398614015060033 ) ) ;
#8988 = DIRECTION ( 'NONE',  ( 0.000000000000000000, 0.000000000000000000, -1.000000000000000000 ) ) ;
#8989 = CARTESIAN_POINT ( 'NONE',  ( 11.52621308753668927, -22.10078695511856850, -40.20443266154408235 ) ) ;
#8990 = DIRECTION ( 'NONE',  ( 0.000000000000000000, 0.000000000000000000, -1.000000000000000000 ) ) ;
#8991 = CARTESIAN_POINT ( 'NONE',  ( 74.93037295002240228, -43.11618894467930119, -15.31098073120859837 ) ) ;
#8992 = DIRECTION ( 'NONE',  ( 0.000000000000000000, 1.000000000000000000, 0.000000000000000000 ) ) ;
#8993 = VERTEX_POINT ( 'NONE', #26501 ) ;
#8994 = CARTESIAN_POINT ( 'NONE',  ( -3.355680836222830088, -48.40293006637049444, -5.033607157952709521 ) ) ;
#8995 = CARTESIAN_POINT ( 'NONE',  ( 47.44871638918419876, 23.38584436733959748, -54.69912089980569903 ) ) ;
#8996 = AXIS2_PLACEMENT_3D ( 'NONE', #277, #16260, #44296 ) ;
#8997 = FACE_OUTER_BOUND ( 'NONE', #29641, .T. ) ;
#8998 = CARTESIAN_POINT ( 'NONE',  ( 63.43898171031399613, 1.369976237678180109, -62.46883854029779570 ) ) ;
#8999 = LINE ( 'NONE', #8478, #45731 ) ;
#9000 = CARTESIAN_POINT ( 'NONE',  ( 11.36506040363580006, 34.06329960752539421, -17.70888297486289886 ) ) ;
#9001 = CYLINDRICAL_SURFACE ( 'NONE', #16891, 6.766999999999998572 ) ;
#9003 = ADVANCED_FACE ( 'NONE', ( #6606 ), #26244, .T. ) ;
#9002 = CARTESIAN_POINT ( 'NONE',  ( 8.222946520301590567, -14.58057468306158100, -60.83399804565716806 ) ) ;
#9004 = CARTESIAN_POINT ( 'NONE',  ( 72.13898961932780196, 1.457833794292699992, -61.50804513633939763 ) ) ;
#9005 = CARTESIAN_POINT ( 'NONE',  ( 58.40527474631630156, -46.88335097056240386, -48.04018388860429667 ) ) ;
#9006 = CARTESIAN_POINT ( 'NONE',  ( 52.95539585931859961, 18.32046256209179802, -27.75247797855960030 ) ) ;
#9007 = CARTESIAN_POINT ( 'NONE',  ( 17.52353788780599686, -52.44145270522049884, -76.03823174343609992 ) ) ;
#9008 = ADVANCED_FACE ( 'NONE', ( #47227 ), #42310, .T. ) ;
#9009 = CARTESIAN_POINT ( 'NONE',  ( 10.72256262586727793, -19.77478906618366494, -61.24449922350422071 ) ) ;
#9010 = CARTESIAN_POINT ( 'NONE',  ( 9.367407790820902136, -15.61608574124520032, -61.84717978381009829 ) ) ;
#9011 = ORIENTED_EDGE ( 'NONE', *, *, #36468, .T. ) ;
#9012 = DIRECTION ( 'NONE',  ( 0.000000000000000000, 0.000000000000000000, -1.000000000000000000 ) ) ;
#9013 = CARTESIAN_POINT ( 'NONE',  ( 8.957196496706650635, 31.92430757304470035, -46.63362000866580104 ) ) ;
#9014 = CARTESIAN_POINT ( 'NONE',  ( 57.77564497937559906, 0.4193449612534105309, -17.11446609406728570 ) ) ;
#9015 = ORIENTED_EDGE ( 'NONE', *, *, #19161, .T. ) ;
#9016 = CARTESIAN_POINT ( 'NONE',  ( 18.34433777603829796, 20.57110240350969832, -75.40982873507010709 ) ) ;
#9017 = EDGE_LOOP ( 'NONE', ( #43634, #32873, #3013, #29969 ) ) ;
#9018 = ORIENTED_EDGE ( 'NONE', *, *, #8846, .T. ) ;
#9019 = ORIENTED_EDGE ( 'NONE', *, *, #34752, .F. ) ;
#9020 = CARTESIAN_POINT ( 'NONE',  ( 12.82504919487779915, -65.50308766827649265, -47.62518768686640414 ) ) ;
#9021 = CARTESIAN_POINT ( 'NONE',  ( 57.03244692032389906, -45.51060902889650350, -26.04968356573699850 ) ) ;
#9022 = CARTESIAN_POINT ( 'NONE',  ( 21.04481148849130179, -20.61575451790190172, -81.23899999999999011 ) ) ;
#9023 = CARTESIAN_POINT ( 'NONE',  ( 61.71737073286530517, 13.89658578540509914, -46.60406873706940445 ) ) ;
#9024 = CARTESIAN_POINT ( 'NONE',  ( 64.20123866503199395, 1.456055805561079941, -61.44407688768469455 ) ) ;
#9025 = ORIENTED_EDGE ( 'NONE', *, *, #10474, .F. ) ;
#9026 = ORIENTED_EDGE ( 'NONE', *, *, #50867, .F. ) ;
#9027 = CARTESIAN_POINT ( 'NONE',  ( 11.93810440114173055, 34.20707662183112774, -17.87564879217053004 ) ) ;
#9028 = VERTEX_POINT ( 'NONE', #19808 ) ;
#9029 = CARTESIAN_POINT ( 'NONE',  ( 46.20925947970359715, -46.13067797581490481, -9.791027853733639930 ) ) ;
#9030 = CARTESIAN_POINT ( 'NONE',  ( 17.35880188677425551, -23.50009711225479236, -34.24345447869366410 ) ) ;
#9031 = DIRECTION ( 'NONE',  ( 0.000000000000000000, 0.000000000000000000, 1.000000000000000000 ) ) ;
#9032 = VERTEX_POINT ( 'NONE', #47099 ) ;
#9033 = EDGE_LOOP ( 'NONE', ( #21957, #17215, #29376, #29010 ) ) ;
#9034 = CARTESIAN_POINT ( 'NONE',  ( 72.76396860142250489, 1.388715606738730068, -62.57493595107060713 ) ) ;
#9035 = CARTESIAN_POINT ( 'NONE',  ( 46.58330506947539362, -53.42389239804139578, -76.07703971530399656 ) ) ;
#9036 = DIRECTION ( 'NONE',  ( 0.000000000000000000, 1.000000000000000000, 0.000000000000000000 ) ) ;
#9037 = CARTESIAN_POINT ( 'NONE',  ( 50.71554509951779721, 14.96710075306869925, -12.97454429901910089 ) ) ;
#9038 = EDGE_CURVE ( 'NONE', #21587, #11026, #47602, .T. ) ;
#9039 = VECTOR ( 'NONE', #5336, 1000.000000000000000 ) ;
#9040 = DIRECTION ( 'NONE',  ( 0.000000000000000000, -0.7071067811865466846, -0.7071067811865483499 ) ) ;
#9041 = CARTESIAN_POINT ( 'NONE',  ( -8.004967211730480869, 13.73555245088170018, -5.098737574129920347 ) ) ;
#9042 = LINE ( 'NONE', #21072, #40488 ) ;
#9043 = DIRECTION ( 'NONE',  ( -1.000000000000000000, 0.000000000000000000, 0.000000000000000000 ) ) ;
#9044 = CARTESIAN_POINT ( 'NONE',  ( 9.820310712754441340, -10.95519481612969948, -72.48992980192208790 ) ) ;
#9045 = ORIENTED_EDGE ( 'NONE', *, *, #20137, .F. ) ;
#9046 = CARTESIAN_POINT ( 'NONE',  ( 58.58074692517319448, 15.55817703255979900, -48.00570932831679727 ) ) ;
#9047 = CARTESIAN_POINT ( 'NONE',  ( -8.770054618657720624, -44.34737232867720280, -5.608366899511570303 ) ) ;
#9048 = CARTESIAN_POINT ( 'NONE',  ( 11.13393739769619906, 32.28996932331859426, -43.76018303691880362 ) ) ;
#9049 = CARTESIAN_POINT ( 'NONE',  ( 72.99206043124139853, 1.132579237369250036, -69.08822821206570097 ) ) ;
#9050 = CARTESIAN_POINT ( 'NONE',  ( 11.97330428934050062, -64.78167623425329680, -16.08313759591939984 ) ) ;
#9051 = CARTESIAN_POINT ( 'NONE',  ( 71.90718900442459471, 0.9644290104346029402, -70.31590730770628284 ) ) ;
#9053 = EDGE_CURVE ( 'NONE', #235, #1350, #1234, .T. ) ;
#9052 = CARTESIAN_POINT ( 'NONE',  ( 46.36969429687169963, 21.71676565170959705, -76.14999999999999147 ) ) ;
#9054 = CARTESIAN_POINT ( 'NONE',  ( 49.43871793799859660, -53.66383539453889284, -54.54809130707169373 ) ) ;
#9055 = CARTESIAN_POINT ( 'NONE',  ( 41.40756764072759921, -44.77159127043780273, -5.393983506378570603 ) ) ;
#9056 = CARTESIAN_POINT ( 'NONE',  ( 8.222496981792570381, -15.61604333543320067, -34.50766849176299900 ) ) ;
#9057 = CARTESIAN_POINT ( 'NONE',  ( 14.63288374505870060, -32.15889263939740772, -34.64999999999999858 ) ) ;
#9058 = ADVANCED_FACE ( 'NONE', ( #35277 ), #7251, .F. ) ;
#9059 = LINE ( 'NONE', #28436, #17259 ) ;
#9060 = VERTEX_POINT ( 'NONE', #23200 ) ;
#9061 = CARTESIAN_POINT ( 'NONE',  ( 21.09612888652980089, -21.17346795211530264, -45.33533033764049947 ) ) ;
#9062 = CARTESIAN_POINT ( 'NONE',  ( 64.31051442921079797, 1.400155911913310014, -61.27037346668680584 ) ) ;
#9063 = VERTEX_POINT ( 'NONE', #19033 ) ;
#9064 = CARTESIAN_POINT ( 'NONE',  ( 83.71507600481126588, -44.45672478866849531, -46.59591550923387615 ) ) ;
#9065 = CARTESIAN_POINT ( 'NONE',  ( 60.34379256561119576, -45.86802437250690190, -47.72732608210890248 ) ) ;
#9066 = LINE ( 'NONE', #20317, #36273 ) ;
#9067 = AXIS2_PLACEMENT_3D ( 'NONE', #3874, #12248, #24007 ) ;
#9068 = CARTESIAN_POINT ( 'NONE',  ( 61.70641836169023264, 13.92968577895933535, -46.86525494990149099 ) ) ;
#9070 = CARTESIAN_POINT ( 'NONE',  ( -0.02503409344754733978, -8.417620798886582989, -34.78823607925543371 ) ) ;
#9069 = CARTESIAN_POINT ( 'NONE',  ( 44.97106839982397730, 8.796052713493059727, -61.95337525835541470 ) ) ;
#9071 = CARTESIAN_POINT ( 'NONE',  ( 22.90103297551744177, -15.28543113694585642, -60.83163026540892560 ) ) ;
#9072 = CARTESIAN_POINT ( 'NONE',  ( 17.16949042073051857, -23.52718815158684151, -51.96600023950148284 ) ) ;
#9073 = VERTEX_POINT ( 'NONE', #6739 ) ;
#9074 = CARTESIAN_POINT ( 'NONE',  ( 84.22529662124048855, -44.14854820750499442, -47.36165834067109870 ) ) ;
#9075 = ORIENTED_EDGE ( 'NONE', *, *, #14122, .T. ) ;
#9076 = ORIENTED_EDGE ( 'NONE', *, *, #6630, .T. ) ;
#9077 = ORIENTED_EDGE ( 'NONE', *, *, #11428, .F. ) ;
#9078 = CARTESIAN_POINT ( 'NONE',  ( 61.52539987384010089, -45.35174871025959931, -47.31480267961979536 ) ) ;
#9079 = CARTESIAN_POINT ( 'NONE',  ( 52.62660330590350100, -49.81109310332840323, -48.67237100752149814 ) ) ;
#9080 = CARTESIAN_POINT ( 'NONE',  ( 52.66500433930978176, -50.10310259146618961, -77.26040935214849981 ) ) ;
#9081 = CARTESIAN_POINT ( 'NONE',  ( 76.39890521214071839, -19.26305209071983526, -12.79182930615482050 ) ) ;
#9082 = CARTESIAN_POINT ( 'NONE',  ( 56.55536805559270164, -50.73789114322060101, -53.84226117436379866 ) ) ;
#9083 = ORIENTED_EDGE ( 'NONE', *, *, #4655, .T. ) ;
#9084 = VERTEX_POINT ( 'NONE', #39730 ) ;
#9085 = CARTESIAN_POINT ( 'NONE',  ( 11.64494012201000039, 34.15031286627577600, -22.50329527685726561 ) ) ;
#9086 = CARTESIAN_POINT ( 'NONE',  ( 56.55337564908950299, 19.27319311912070177, -52.91477395641850734 ) ) ;
#9087 = CARTESIAN_POINT ( 'NONE',  ( -13.33284876601550728, 9.986826335083126338, -46.69325378129649096 ) ) ;
#9088 = CARTESIAN_POINT ( 'NONE',  ( 14.02678725144039973, -50.30560580096022960, -20.88317649143804644 ) ) ;
#9089 = CARTESIAN_POINT ( 'NONE',  ( 8.799470649396189614, -63.19223985362448559, -46.67016919464409597 ) ) ;
#9090 = CARTESIAN_POINT ( 'NONE',  ( 51.84382619997980157, -49.26715712592199736, -77.06468978676770121 ) ) ;
#9091 = ORIENTED_EDGE ( 'NONE', *, *, #27469, .T. ) ;
#9092 = B_SPLINE_CURVE_WITH_KNOTS ( 'NONE', 3,
 ( #23244, #2850, #22219, #26938, #22991, #27191, #50290, #3108, #19075, #43200, #7293, #51822, #16434, #23759, #11749, #24524, #36598, #47641 ),
 .UNSPECIFIED., .F., .F.,
 ( 4, 2, 2, 2, 2, 2, 2, 2, 4 ),
 ( 0.5000015279420912950, 0.5625013369493297999, 0.6250011459565683047, 0.6875009549638069206, 0.7500007639710454255, 0.8125005729782841524, 0.8750003819855227682, 0.9375001909927613841, 1.000000000000000000 ),
 .UNSPECIFIED. ) ;
#9093 = DIRECTION ( 'NONE',  ( -1.000000000000000000, 0.000000000000000000, 0.000000000000000000 ) ) ;
#9094 = CARTESIAN_POINT ( 'NONE',  ( 23.24148394091340109, -47.84168788784550230, -54.64999999999999858 ) ) ;
#9095 = CARTESIAN_POINT ( 'NONE',  ( 21.48239107889450494, -19.76700007457129615, -46.66288234737064755 ) ) ;
#9096 = CARTESIAN_POINT ( 'NONE',  ( 13.39998208309999939, 20.55440457967890211, -76.14999999999999147 ) ) ;
#9097 = CARTESIAN_POINT ( 'NONE',  ( 23.96840403421039767, -16.07212766087679867, -64.03099806865479593 ) ) ;
#9098 = CYLINDRICAL_SURFACE ( 'NONE', #4572, 3.500000000000003109 ) ;
#9099 = EDGE_CURVE ( 'NONE', #23745, #19697, #27406, .T. ) ;
#9100 = CARTESIAN_POINT ( 'NONE',  ( 42.52205267802430200, -43.49267883201609664, -4.456987777804809703 ) ) ;
#9101 = CARTESIAN_POINT ( 'NONE',  ( 22.90065299155850198, -15.61618013372109637, -50.45281880338879432 ) ) ;
#9102 = FACE_OUTER_BOUND ( 'NONE', #35507, .T. ) ;
#9104 = EDGE_CURVE ( 'NONE', #34463, #47835, #41599, .T. ) ;
#9103 = CARTESIAN_POINT ( 'NONE',  ( 16.13393739769620083, -15.61618894467929941, -14.68999999999999950 ) ) ;
#9105 = ADVANCED_FACE ( 'NONE', ( #10669 ), #39723, .T. ) ;
#9106 = CARTESIAN_POINT ( 'NONE',  ( 63.92076813643380007, 1.033004454759739899, -69.92211063522330505 ) ) ;
#9107 = FACE_OUTER_BOUND ( 'NONE', #5101, .T. ) ;
#9108 = CARTESIAN_POINT ( 'NONE',  ( 67.25971769855989635, -0.6780106752988179775, -17.44087497863319669 ) ) ;
#9109 = ORIENTED_EDGE ( 'NONE', *, *, #23738, .T. ) ;
#9110 = CARTESIAN_POINT ( 'NONE',  ( 13.79823471886849973, -51.65733818268109445, -75.17186369577468952 ) ) ;
#9111 = CARTESIAN_POINT ( 'NONE',  ( 47.21517444068279445, -54.78196946262829670, -54.62462293534060365 ) ) ;
#9112 = CARTESIAN_POINT ( 'NONE',  ( 23.14289354968460088, -48.86424211905639936, -35.14566343974149731 ) ) ;
#9113 = DIRECTION ( 'NONE',  ( 0.000000000000000000, 0.000000000000000000, -1.000000000000000000 ) ) ;
#9114 = CYLINDRICAL_SURFACE ( 'NONE', #7262, 7.910999999999997812 ) ;
#9115 = CARTESIAN_POINT ( 'NONE',  ( 23.03048158991310146, -18.61450947644279807, -32.14999999999999858 ) ) ;
#9116 = LINE ( 'NONE', #12530, #11371 ) ;
#9117 = CARTESIAN_POINT ( 'NONE',  ( 10.81643727141089961, 33.72113552640900025, -17.63284883033089656 ) ) ;
#9119 = CARTESIAN_POINT ( 'NONE',  ( 11.27235097447594470, -21.94242344813731904, -74.21600161823359088 ) ) ;
#9118 = CARTESIAN_POINT ( 'NONE',  ( 13.97461707263510178, 19.95444906609850122, -22.92155396671540046 ) ) ;
#9120 = CARTESIAN_POINT ( 'NONE',  ( 56.42218940953110007, 19.53148004655350078, -53.51231675409619726 ) ) ;
#9121 = EDGE_CURVE ( 'NONE', #50203, #32053, #43417, .T. ) ;
#9122 = CARTESIAN_POINT ( 'NONE',  ( 48.46328056021759778, 22.91827103051950232, -54.95887287608610450 ) ) ;
#9123 = ORIENTED_EDGE ( 'NONE', *, *, #20614, .F. ) ;
#9124 = CARTESIAN_POINT ( 'NONE',  ( 11.64736116879679884, -10.17438842309400115, -64.12771089025820004 ) ) ;
#9125 = ORIENTED_EDGE ( 'NONE', *, *, #36824, .F. ) ;
#9126 = AXIS2_PLACEMENT_3D ( 'NONE', #15733, #11038, #43015 ) ;
#9127 = CARTESIAN_POINT ( 'NONE',  ( 2.558062577109650348, -6.044886501696560721, -34.64999999999999858 ) ) ;
#9128 = DIRECTION ( 'NONE',  ( 1.000000000000000000, 0.000000000000000000, -1.224646799147353207E-16 ) ) ;
#9129 = CARTESIAN_POINT ( 'NONE',  ( 20.29260782020964271, -21.02750830818477823, -42.74448647513240473 ) ) ;
#9131 = CARTESIAN_POINT ( 'NONE',  ( 53.25483989353620018, 17.95639845396440393, -27.17232069770570035 ) ) ;
#9130 = CARTESIAN_POINT ( 'NONE',  ( 84.37646258656080533, 12.22652691366610078, -47.26568110888489826 ) ) ;
#9132 = CARTESIAN_POINT ( 'NONE',  ( 22.69723333660660103, -13.03438625761980063, -70.33352477266448943 ) ) ;
#9133 = CARTESIAN_POINT ( 'NONE',  ( 12.36320305029179956, 33.31445045633500257, -15.76422791923680045 ) ) ;
#9134 = CARTESIAN_POINT ( 'NONE',  ( 72.78816252330430814, 1.385888765344509999, -68.65207957385619864 ) ) ;
#9135 = CARTESIAN_POINT ( 'NONE',  ( 16.15069456443260520, -51.05177125324679110, -17.90311212357429937 ) ) ;
#9136 = ORIENTED_EDGE ( 'NONE', *, *, #14940, .F. ) ;
#9137 = ORIENTED_EDGE ( 'NONE', *, *, #44527, .T. ) ;
#9138 = CARTESIAN_POINT ( 'NONE',  ( 11.41271396217149992, -64.98654470182599141, -16.69425700586020156 ) ) ;
#9139 = CARTESIAN_POINT ( 'NONE',  ( 11.31321705866109895, 33.19720110168429272, -44.95199481682620046 ) ) ;
#9140 = CARTESIAN_POINT ( 'NONE',  ( 61.25724218321475689, -45.31063123919039981, -47.12446599951652360 ) ) ;
#9141 = VECTOR ( 'NONE', #4765, 1000.000000000000000 ) ;
#9142 = CARTESIAN_POINT ( 'NONE',  ( 50.13069710666830048, -52.30340857919710373, -51.78329334912879744 ) ) ;
#9143 = CARTESIAN_POINT ( 'NONE',  ( 51.58134972076286573, 2.917345700074899462, -76.88489686019924818 ) ) ;
#9144 = CIRCLE ( 'NONE', #51821, 32.00000000000000000 ) ;
#9145 = AXIS2_PLACEMENT_3D ( 'NONE', #36890, #5196, #25332 ) ;
#9146 = AXIS2_PLACEMENT_3D ( 'NONE', #2122, #45897, #17844 ) ;
#9147 = ORIENTED_EDGE ( 'NONE', *, *, #23519, .F. ) ;
#9148 = CARTESIAN_POINT ( 'NONE',  ( 18.20455937407651703, -7.911072576141705781, -75.09096826776161038 ) ) ;
#9149 = CARTESIAN_POINT ( 'NONE',  ( 57.16896213477740218, 14.61892080237120162, -26.25490629759670114 ) ) ;
#9150 = AXIS2_PLACEMENT_3D ( 'NONE', #42790, #6885, #11074 ) ;
#9151 = DIRECTION ( 'NONE',  ( 0.000000000000000000, 0.000000000000000000, 1.000000000000000000 ) ) ;
#9152 = DIRECTION ( 'NONE',  ( 0.000000000000000000, -1.000000000000000000, 0.000000000000000000 ) ) ;
#9153 = CARTESIAN_POINT ( 'NONE',  ( 50.95182855010879308, -50.95090509061829209, -76.14999999999999147 ) ) ;
#9154 = DIRECTION ( 'NONE',  ( 0.000000000000000000, 0.000000000000000000, 1.000000000000000000 ) ) ;
#9155 = EDGE_LOOP ( 'NONE', ( #4134, #35873, #17709, #5024 ) ) ;
#9156 = CARTESIAN_POINT ( 'NONE',  ( 18.11511214869360131, -32.59175772023380091, -35.01387690002269437 ) ) ;
#9157 = ORIENTED_EDGE ( 'NONE', *, *, #6040, .F. ) ;
#9158 = CARTESIAN_POINT ( 'NONE',  ( 12.68691374172937003, -55.46739277041032068, -75.51638835765626823 ) ) ;
#9159 = CARTESIAN_POINT ( 'NONE',  ( 16.13393739769620083, -15.61618894467929941, -11.05000000000000071 ) ) ;
#9160 = CARTESIAN_POINT ( 'NONE',  ( 18.77779167496959900, -23.00515247567150112, -34.40311785086109353 ) ) ;
#9161 = CARTESIAN_POINT ( 'NONE',  ( 9.367549511386263461, -16.57320966654785011, -65.80214969305676220 ) ) ;
#9162 = CARTESIAN_POINT ( 'NONE',  ( 56.13201255944740353, 19.60900434519550117, -74.69880780947919163 ) ) ;
#9163 = EDGE_CURVE ( 'NONE', #16231, #8281, #48781, .T. ) ;
#9164 = CARTESIAN_POINT ( 'NONE',  ( 46.91625109622430045, -53.80736403542660184, -75.86076060431129520 ) ) ;
#9165 = ORIENTED_EDGE ( 'NONE', *, *, #30558, .F. ) ;
#9166 = CARTESIAN_POINT ( 'NONE',  ( 55.11318621343720281, 14.43546311050189956, -15.75535627857289889 ) ) ;
#9167 = ADVANCED_FACE ( 'NONE', ( #44952 ), #13837, .T. ) ;
#9168 = CARTESIAN_POINT ( 'NONE',  ( 16.91867857995320179, -8.607141901655454674, -46.38267033200752110 ) ) ;
#9169 = CARTESIAN_POINT ( 'NONE',  ( 52.56799448115409490, -49.85882480688869833, -48.49336018736870102 ) ) ;
#9170 = CARTESIAN_POINT ( 'NONE',  ( 10.41813705297420078, -19.74831615951159947, -31.64794915417429166 ) ) ;
#9171 = CARTESIAN_POINT ( 'NONE',  ( 12.29386161020425838, 34.10498507263372403, -23.62058203229901210 ) ) ;
#9172 = EDGE_CURVE ( 'NONE', #48087, #42029, #17142, .T. ) ;
#9173 = ORIENTED_EDGE ( 'NONE', *, *, #11027, .F. ) ;
#9174 = CARTESIAN_POINT ( 'NONE',  ( 47.40872200122030478, 23.22827899685340114, -74.94663380581118872 ) ) ;
#9175 = CARTESIAN_POINT ( 'NONE',  ( 16.13393739769599833, 14.38381105532070059, -34.64999999999999858 ) ) ;
#9176 = AXIS2_PLACEMENT_3D ( 'NONE', #32092, #24223, #16134 ) ;
#9177 = CARTESIAN_POINT ( 'NONE',  ( 60.23130391297029718, 14.55066440145539985, -47.24246919202519734 ) ) ;
#9178 = AXIS2_PLACEMENT_3D ( 'NONE', #1544, #1801, #50020 ) ;
#9179 = CARTESIAN_POINT ( 'NONE',  ( 12.28455908802819962, 33.49872389401299699, -15.95890976725140220 ) ) ;
#9180 = VECTOR ( 'NONE', #25900, 999.9999999999998863 ) ;
#9181 = CIRCLE ( 'NONE', #25871, 33.97624844042369574 ) ;
#9183 = TOROIDAL_SURFACE ( 'NONE', #37594, 17.39999999999999858, 3.799999999999999822 ) ;
#9182 = CARTESIAN_POINT ( 'NONE',  ( 14.67232007451260323, -49.61617055433323742, -83.19301782014780144 ) ) ;
#9184 = DIRECTION ( 'NONE',  ( 6.073366656256538404E-31, 1.365304166073849981E-11, -1.000000000000000000 ) ) ;
#9185 = CARTESIAN_POINT ( 'NONE',  ( 72.86589732295999511, 1.383811055320669947, -68.52599601131950635 ) ) ;
#9186 = B_SPLINE_CURVE_WITH_KNOTS ( 'NONE', 3,
 ( #39794, #214, #24814, #23782, #4923, #47666, #15951, #24549 ),
 .UNSPECIFIED., .F., .F.,
 ( 4, 2, 2, 4 ),
 ( -0.1350635247378738635, -0.1243669311571979907, -0.1075965482621700081, -0.1052074838067399987 ),
 .UNSPECIFIED. ) ;
#9188 = CARTESIAN_POINT ( 'NONE',  ( 29.57851616124868599, -35.65923776031012693, -84.61510634421995292 ) ) ;
#9187 = CARTESIAN_POINT ( 'NONE',  ( 66.63393739769620083, 6.883811055320649963, -71.50000000000000000 ) ) ;
#9189 = CARTESIAN_POINT ( 'NONE',  ( 61.20155191191109623, 14.04232429033380036, -46.66714648058599835 ) ) ;
#9190 = EDGE_CURVE ( 'NONE', #36469, #20584, #46445, .T. ) ;
#9191 = CARTESIAN_POINT ( 'NONE',  ( 6.188526101445139815, -63.88644423068799938, -47.34841622259269656 ) ) ;
#9192 = ORIENTED_EDGE ( 'NONE', *, *, #29710, .F. ) ;
#9193 = CARTESIAN_POINT ( 'NONE',  ( 52.90392158692600333, -49.62416384515039880, -48.79551526944879924 ) ) ;
#9194 = CARTESIAN_POINT ( 'NONE',  ( 57.72833049119049775, -45.13003903922449211, -25.57691600686959887 ) ) ;
#9195 = CARTESIAN_POINT ( 'NONE',  ( 11.27236349546028293, -21.94243292154778402, -74.50066484501441266 ) ) ;
#9196 = CARTESIAN_POINT ( 'NONE',  ( 57.40895152886420050, 14.37846127530180063, -26.19991503117499931 ) ) ;
#9197 = CARTESIAN_POINT ( 'NONE',  ( 9.124464442534721442, -16.39711836812870160, -33.41750289701789711 ) ) ;
#9198 = CARTESIAN_POINT ( 'NONE',  ( 50.57758487413249782, 18.62004947392870235, -76.16361833584198848 ) ) ;
#9199 = CARTESIAN_POINT ( 'NONE',  ( 52.81564606049040123, 18.44441551310690031, -48.78617137558140371 ) ) ;
#9200 = CARTESIAN_POINT ( 'NONE',  ( 71.19525238180870019, 1.198183261254780030, -70.68687062374729635 ) ) ;
#9201 = DIRECTION ( 'NONE',  ( 0.000000000000000000, 0.000000000000000000, -1.000000000000000000 ) ) ;
#9202 = DIRECTION ( 'NONE',  ( -1.000000000000000000, 0.000000000000000000, 0.000000000000000000 ) ) ;
#9203 = VERTEX_POINT ( 'NONE', #23514 ) ;
#9204 = CARTESIAN_POINT ( 'NONE',  ( 11.25790860626830003, -21.24921988401450079, -71.79445331288948751 ) ) ;
#9205 = ORIENTED_EDGE ( 'NONE', *, *, #39841, .T. ) ;
#9206 = CARTESIAN_POINT ( 'NONE',  ( 72.99348972288790094, 1.187296498006439993, -69.02170307486190381 ) ) ;
#9207 = CARTESIAN_POINT ( 'NONE',  ( 47.39224450036900294, -54.66215068426350143, -54.83956910525469652 ) ) ;
#9208 = CARTESIAN_POINT ( 'NONE',  ( 19.09037207632416511, -8.257022906990993505, -49.41399161769187032 ) ) ;
#9209 = CARTESIAN_POINT ( 'NONE',  ( 72.92255733887110125, 1.374300485541529948, -62.71457717039259450 ) ) ;
#9210 = CARTESIAN_POINT ( 'NONE',  ( 60.71152220950099831, -30.57213475406030057, -16.28960219260079967 ) ) ;
#9211 = CARTESIAN_POINT ( 'NONE',  ( 53.18486760013709613, 18.24248981343010101, -48.80133335483819934 ) ) ;
#9212 = CARTESIAN_POINT ( 'NONE',  ( 2.458146360389370511, -25.65221394861527671, -34.79644291222910368 ) ) ;
#9213 = CARTESIAN_POINT ( 'NONE',  ( 71.81682835125050701, 1.153605328057990098, -60.96078815522670169 ) ) ;
#9214 = EDGE_CURVE ( 'NONE', #9489, #45513, #35848, .T. ) ;
#9215 = CARTESIAN_POINT ( 'NONE',  ( 78.22251691734010137, 1.883811055320649963, -20.65000000000000213 ) ) ;
#9216 = CARTESIAN_POINT ( 'NONE',  ( 65.23737843152780158, 1.383411777981069957, -70.37541122638330648 ) ) ;
#9217 = ORIENTED_EDGE ( 'NONE', *, *, #25699, .F. ) ;
#9218 = EDGE_CURVE ( 'NONE', #18453, #51359, #1609, .T. ) ;
#9219 = ORIENTED_EDGE ( 'NONE', *, *, #4580, .F. ) ;
#9220 = CARTESIAN_POINT ( 'NONE',  ( 9.287874463674199887, -63.21240253717019897, -46.53018408198249745 ) ) ;
#9221 = DIRECTION ( 'NONE',  ( 1.000000000000000000, 0.000000000000000000, 0.000000000000000000 ) ) ;
#9222 = ORIENTED_EDGE ( 'NONE', *, *, #35321, .T. ) ;
#9223 = CYLINDRICAL_SURFACE ( 'NONE', #25002, 2.999999999999994227 ) ;
#9224 = DIRECTION ( 'NONE',  ( 0.000000000000000000, 0.000000000000000000, -1.000000000000000000 ) ) ;
#9225 = CARTESIAN_POINT ( 'NONE',  ( 26.13393739769619728, -28.89524513604070322, -62.14999999999999858 ) ) ;
#9226 = CIRCLE ( 'NONE', #33467, 0.4934525379923264121 ) ;
#9227 = CARTESIAN_POINT ( 'NONE',  ( 52.51047226760390174, 19.75004459190430239, -76.15156771798700674 ) ) ;
#9228 = AXIS2_PLACEMENT_3D ( 'NONE', #3883, #11753, #15159 ) ;
#9229 = VERTEX_POINT ( 'NONE', #11761 ) ;
#9230 = LINE ( 'NONE', #32772, #5069 ) ;
#9231 = VECTOR ( 'NONE', #18732, 1000.000000000000000 ) ;
#9232 = CARTESIAN_POINT ( 'NONE',  ( 74.23393739769618094, -15.41618894467939782, -65.65000000000000568 ) ) ;
#9233 = CARTESIAN_POINT ( 'NONE',  ( 15.09830364956688697, -7.705199274396241194, -43.25070712488398783 ) ) ;
#9234 = AXIS2_PLACEMENT_3D ( 'NONE', #40277, #15916, #31870 ) ;
#9235 = B_SPLINE_SURFACE_WITH_KNOTS ( 'NONE', 3, 3, ( 
 ( #9680, #25640, #14125, #45065, #49528, #21197 ),
 ( #25383, #30090, #45848, #33253, #36940, #13118 ),
 ( #49269, #41909, #1814, #46116, #4973, #25124 ),
 ( #40871, #41133, #45586, #37456, #9434, #21707 ),
 ( #29069, #13364, #5244, #1555, #13619, #1041 ),
 ( #37716, #10201, #18056, #2077, #29582, #21457 ),
 ( #9934, #20943, #17035, #37203, #1302, #41642 ),
 ( #33515, #17292, #25896, #37980, #6009, #29328 ),
 ( #41384, #32987, #5751, #5501, #17795, #17543 ),
 ( #33768, #49779, #13872, #29828, #46375, #10717 ),
 ( #10980, #14897, #26945, #19343, #23251, #2329 ),
 ( #6271, #31376, #35327, #31122, #6525, #26673 ),
 ( #34546, #22487, #51326, #47403, #14385, #42695 ),
 ( #38237, #7301, #42951, #46892, #7049, #15424 ),
 ( #34804, #38493, #22228, #6790, #26160, #47147 ),
 ( #18304, #50297, #43210, #50550, #27197, #39020 ) ),
 .UNSPECIFIED., .F., .F., .F.,
 ( 4, 2, 2, 2, 2, 2, 2, 4 ),
 ( 4, 1, 1, 4 ),
 ( -1.480557284018800157, -1.467872963798670050, -1.112024972574749970, -0.8896199780598010864, -0.7784174808023259784, -0.6004934851903659387, -0.3158150922112299974, 0.000000000000000000 ),
 ( 0.000000000000000000, 0.3333333333333329818, 0.6666666666666670737, 1.000000000000000000 ),
 .UNSPECIFIED. ) ;
#9236 = CARTESIAN_POINT ( 'NONE',  ( 11.92188350998449842, -22.70430026596570272, -54.46300130049679211 ) ) ;
#9237 = DIRECTION ( 'NONE',  ( 0.000000000000000000, 0.000000000000000000, -1.000000000000000000 ) ) ;
#9238 = CARTESIAN_POINT ( 'NONE',  ( 53.70553476669380188, 20.08271752784780162, -75.56421356237311215 ) ) ;
#9239 = ORIENTED_EDGE ( 'NONE', *, *, #188, .T. ) ;
#9240 = ADVANCED_FACE ( 'NONE', ( #51068 ), #22193, .T. ) ;
#9241 = CARTESIAN_POINT ( 'NONE',  ( 60.34379258661509482, -45.86802437805019395, -47.72732609191810127 ) ) ;
#9242 = CARTESIAN_POINT ( 'NONE',  ( 14.31700556835209959, -8.390854867097690573, -43.65423889476479502 ) ) ;
#9243 = CARTESIAN_POINT ( 'NONE',  ( 52.60295254337719939, -49.82768164818060086, -48.60889610034470110 ) ) ;
#9244 = CARTESIAN_POINT ( 'NONE',  ( 20.11802547147715359, -8.703639956352418494, -33.17433219651738341 ) ) ;
#9245 = EDGE_CURVE ( 'NONE', #9812, #43378, #35533, .T. ) ;
#9246 = MANIFOLD_SOLID_BREP ( 'Stock-MAS-691-1', #36027 ) ;
#9247 = CARTESIAN_POINT ( 'NONE',  ( 14.91464035002509902, 21.52412519331699770, -76.12563501418100032 ) ) ;
#9248 = CARTESIAN_POINT ( 'NONE',  ( 44.13393739769620083, 1.883811055320659955, -54.35294145922169662 ) ) ;
#9249 = CARTESIAN_POINT ( 'NONE',  ( 33.38393739769599478, 10.53025766472752522, -34.79644660940672907 ) ) ;
#9250 = CARTESIAN_POINT ( 'NONE',  ( 16.04164975777740310, -7.371541972219340266, -51.00410559314138936 ) ) ;
#9251 = ORIENTED_EDGE ( 'NONE', *, *, #8160, .F. ) ;
#9252 = CARTESIAN_POINT ( 'NONE',  ( 52.83716997623850631, -49.57025241744720745, -27.30068420219360092 ) ) ;
#9253 = CARTESIAN_POINT ( 'NONE',  ( 53.97741451551910075, -51.26237320098420014, -75.50474183165199804 ) ) ;
#9254 = DIRECTION ( 'NONE',  ( 0.000000000000000000, 0.000000000000000000, 1.000000000000000000 ) ) ;
#9255 = CARTESIAN_POINT ( 'NONE',  ( 10.22095591748514032, -19.02406068606311607, -57.28612154450400595 ) ) ;
#9256 = CARTESIAN_POINT ( 'NONE',  ( 15.26098176771331261, -14.98194955443502252, -9.392532499999980189 ) ) ;
#9257 = EDGE_LOOP ( 'NONE', ( #32253, #35267, #44982, #2043 ) ) ;
#9258 = AXIS2_PLACEMENT_3D ( 'NONE', #47001, #50910, #11086 ) ;
#9259 = CARTESIAN_POINT ( 'NONE',  ( -3.304781330980080423, -48.28933272873660343, -4.547377290988400489 ) ) ;
#9260 = AXIS2_PLACEMENT_3D ( 'NONE', #41686, #42214, #18095 ) ;
#9261 = CARTESIAN_POINT ( 'NONE',  ( 47.34367498752779824, 23.45770001724940101, -54.71075737435550224 ) ) ;
#9262 = CARTESIAN_POINT ( 'NONE',  ( 56.61928470354429521, -45.32411298099489727, -25.29356197036729981 ) ) ;
#9263 = CARTESIAN_POINT ( 'NONE',  ( 63.35681832276381442, 1.325839985408290067, -62.43087585298830078 ) ) ;
#9264 = DIRECTION ( 'NONE',  ( 1.000000000000000000, 0.000000000000000000, 0.000000000000000000 ) ) ;
#9265 = AXIS2_PLACEMENT_3D ( 'NONE', #23564, #19655, #39078 ) ;
#9266 = CARTESIAN_POINT ( 'NONE',  ( 43.60412366959330654, 12.47234831688600210, -5.064848484392650008 ) ) ;
#9267 = CARTESIAN_POINT ( 'NONE',  ( 11.96660005458869946, 10.88381105532060111, -34.64999999999999858 ) ) ;
#9268 = CARTESIAN_POINT ( 'NONE',  ( 53.02240706027900075, 18.32760744209570092, -48.78672998508179859 ) ) ;
#9269 = DIRECTION ( 'NONE',  ( 0.000000000000000000, 0.000000000000000000, -1.000000000000000000 ) ) ;
#9270 = CARTESIAN_POINT ( 'NONE',  ( 57.59002137063620097, -47.30929821719110606, -48.19818069499370239 ) ) ;
#9271 = CARTESIAN_POINT ( 'NONE',  ( 10.86891355504775802, -19.90191905193766786, -67.23537444561883092 ) ) ;
#9272 = CARTESIAN_POINT ( 'NONE',  ( 56.27101956176600339, 19.34483571430840243, -52.87263781881699032 ) ) ;
#9273 = DIRECTION ( 'NONE',  ( 0.000000000000000000, 0.000000000000000000, 1.000000000000000000 ) ) ;
#9274 = CARTESIAN_POINT ( 'NONE',  ( 23.83903448771030753, -17.68688015324557838, -75.59100382533542017 ) ) ;
#9275 = VERTEX_POINT ( 'NONE', #47344 ) ;
#9276 = FACE_OUTER_BOUND ( 'NONE', #41761, .T. ) ;
#9277 = CARTESIAN_POINT ( 'NONE',  ( 9.287340138010449664, 31.97629639357099762, -46.53025760029479585 ) ) ;
#9278 = CARTESIAN_POINT ( 'NONE',  ( 28.63393739769619728, -22.83306730954970121, -34.64999999999999858 ) ) ;
#9279 = EDGE_CURVE ( 'NONE', #39608, #18727, #6211, .T. ) ;
#9280 = FACE_OUTER_BOUND ( 'NONE', #49974, .T. ) ;
#9281 = ORIENTED_EDGE ( 'NONE', *, *, #43243, .T. ) ;
#9282 = CARTESIAN_POINT ( 'NONE',  ( 18.36813433944570306, 20.77108261440790216, -75.51240970683930698 ) ) ;
#9283 = ORIENTED_EDGE ( 'NONE', *, *, #34824, .F. ) ;
#9284 = EDGE_CURVE ( 'NONE', #24387, #38190, #42239, .T. ) ;
#9285 = EDGE_LOOP ( 'NONE', ( #1143, #21624, #17456, #48372, #11063, #22089, #9025, #42191, #27998, #3396, #29930, #38102, #10186 ) ) ;
#9286 = DIRECTION ( 'NONE',  ( -0.6209860917175333839, 0.7838215829468996310, 0.000000000000000000 ) ) ;
#9287 = VERTEX_POINT ( 'NONE', #35788 ) ;
#9288 = CARTESIAN_POINT ( 'NONE',  ( 10.66720212314140070, -63.45534415236151204, -45.40081149022140039 ) ) ;
#9289 = CARTESIAN_POINT ( 'NONE',  ( 57.13718842672530229, -45.48243698324539253, -26.05465429760539919 ) ) ;
#9290 = CARTESIAN_POINT ( 'NONE',  ( 23.24856440404530034, -17.32290095377710060, -81.23899999999999011 ) ) ;
#9291 = ADVANCED_FACE ( 'NONE', ( #35268 ), #7244, .T. ) ;
#9292 = CARTESIAN_POINT ( 'NONE',  ( 24.04493737300782996, -14.58064631294842783, -63.46600340254940420 ) ) ;
#9293 = CARTESIAN_POINT ( 'NONE',  ( 61.53499251318310570, 13.92503479677660039, -46.68296636261909782 ) ) ;
#9294 = CARTESIAN_POINT ( 'NONE',  ( 11.83723722998052175, -15.61618894467929941, -22.14999999999999858 ) ) ;
#9295 = ORIENTED_EDGE ( 'NONE', *, *, #12683, .F. ) ;
#9296 = CARTESIAN_POINT ( 'NONE',  ( 13.61938558678000000, 20.19483563406610216, -23.15000000000000213 ) ) ;
#9297 = EDGE_LOOP ( 'NONE', ( #45236, #3793, #42542, #39459 ) ) ;
#9298 = CARTESIAN_POINT ( 'NONE',  ( 46.44332427445870337, -45.55948807132040201, -9.443144690562260024 ) ) ;
#9299 = CARTESIAN_POINT ( 'NONE',  ( 24.04493739752251003, -15.61707898208110024, -33.79236563404541016 ) ) ;
#9300 = CARTESIAN_POINT ( 'NONE',  ( 0.1457840918194806823, -20.72567761198500591, -34.68167776469320529 ) ) ;
#9301 = AXIS2_PLACEMENT_3D ( 'NONE', #12131, #44092, #24136 ) ;
#9302 = AXIS2_PLACEMENT_3D ( 'NONE', #19433, #47487, #3970 ) ;
#9304 = ORIENTED_EDGE ( 'NONE', *, *, #48224, .F. ) ;
#9303 =( BOUNDED_CURVE ( )  B_SPLINE_CURVE ( 3, ( #38583, #2677, #11317, #18650 ),
 .UNSPECIFIED., .F., .T. ) 
 B_SPLINE_CURVE_WITH_KNOTS ( ( 4, 4 ),
 ( 1.570796326794898556, 2.356194490192396351 ),
 .UNSPECIFIED. ) 
 CURVE ( )  GEOMETRIC_REPRESENTATION_ITEM ( )  RATIONAL_B_SPLINE_CURVE ( ( 1.000000000000000000, 0.9492530216741847937, 0.9492530216741847937, 1.000000000000000000 ) ) 
 REPRESENTATION_ITEM ( '' )  );
#9305 = CARTESIAN_POINT ( 'NONE',  ( 72.75396425272869294, 1.390208944942419755, -62.54542373973200142 ) ) ;
#9306 = CARTESIAN_POINT ( 'NONE',  ( 47.12094126571430763, -54.61101435440190244, -75.00840848463889188 ) ) ;
#9307 = TOROIDAL_SURFACE ( 'NONE', #40962, 24.89999999999999858, 4.000000000000059508 ) ;
#9308 = DIRECTION ( 'NONE',  ( 0.8204012560548784583, -0.5717882292104110586, 0.000000000000000000 ) ) ;
#9309 = AXIS2_PLACEMENT_3D ( 'NONE', #16477, #40585, #24838 ) ;
#9310 = EDGE_CURVE ( 'NONE', #26977, #20243, #35389, .T. ) ;
#9311 = CARTESIAN_POINT ( 'NONE',  ( 49.09894036100649828, 14.73025699061659921, -11.67146733142279835 ) ) ;
#9312 = CARTESIAN_POINT ( 'NONE',  ( 17.16951678489040845, -23.52718438587707794, -68.25066353981270595 ) ) ;
#9313 = CYLINDRICAL_SURFACE ( 'NONE', #39915, 1.999999999999995559 ) ;
#9314 = CARTESIAN_POINT ( 'NONE',  ( 10.61751707702059910, 33.59325229219749787, -22.25048313876769868 ) ) ;
#9315 = CARTESIAN_POINT ( 'NONE',  ( 61.52376219282579939, 13.89663229014939994, -27.65962565353160230 ) ) ;
#9316 = CARTESIAN_POINT ( 'NONE',  ( 11.54452688086499990, -9.250337918211469557, -70.58867545639529339 ) ) ;
#9317 = ORIENTED_EDGE ( 'NONE', *, *, #1942, .T. ) ;
#9318 = CARTESIAN_POINT ( 'NONE',  ( 59.03492131492150463, 15.32045715074029957, -47.92638814198690511 ) ) ;
#9319 = CARTESIAN_POINT ( 'NONE',  ( -11.19057721206939959, -41.98697526176020034, -5.946211766447980551 ) ) ;
#9320 = CARTESIAN_POINT ( 'NONE',  ( 76.84281711086150324, -42.03110714784109803, -14.70467750791790174 ) ) ;
#9321 = CARTESIAN_POINT ( 'NONE',  ( 16.13393739769620083, -3.616188944679339823, -22.14999999999999858 ) ) ;
#9322 = CARTESIAN_POINT ( 'NONE',  ( 11.57186432615189986, -64.94495217133389531, -16.50172565924879819 ) ) ;
#9323 = CARTESIAN_POINT ( 'NONE',  ( 57.24929578595760660, -50.61618894467930119, -74.14999999999999147 ) ) ;
#9324 = CARTESIAN_POINT ( 'NONE',  ( 14.36265603518875977, -22.20705339233771269, -79.03615224225634961 ) ) ;
#9325 = CARTESIAN_POINT ( 'NONE',  ( 49.11893593088550602, -53.90327866102659726, -55.14224250079890055 ) ) ;
#9326 = CARTESIAN_POINT ( 'NONE',  ( 51.30165636469427426, -31.84994407807069905, -17.32271793605100285 ) ) ;
#9327 = CARTESIAN_POINT ( 'NONE',  ( 10.31119352376266818, -20.99649262406198247, -34.27025585054010293 ) ) ;
#9328 = CARTESIAN_POINT ( 'NONE',  ( 18.84361988317459691, -51.80633386256119621, -74.54427505469620030 ) ) ;
#9329 = CARTESIAN_POINT ( 'NONE',  ( 68.13393739769618662, -1.166188944679350081, -65.65000000000000568 ) ) ;
#9330 = ORIENTED_EDGE ( 'NONE', *, *, #29862, .T. ) ;
#9331 = AXIS2_PLACEMENT_3D ( 'NONE', #21992, #38002, #2100 ) ;
#9332 = CARTESIAN_POINT ( 'NONE',  ( 21.46166242705329807, -10.40830642393209793, -48.82096330443989984 ) ) ;
#9333 = CARTESIAN_POINT ( 'NONE',  ( 64.03462240194079413, 1.348268854479560019, -61.41792271134369940 ) ) ;
#9334 = ORIENTED_EDGE ( 'NONE', *, *, #6288, .T. ) ;
#9335 = CARTESIAN_POINT ( 'NONE',  ( 83.92831069520973131, -44.23173704228813108, -46.72265495406260527 ) ) ;
#9336 = CARTESIAN_POINT ( 'NONE',  ( 60.33694438359599843, -45.85988071783310716, -47.70890968787160347 ) ) ;
#9337 = CARTESIAN_POINT ( 'NONE',  ( 57.02861369189989915, 19.39567887795939782, -53.87746547145160037 ) ) ;
#9338 = CARTESIAN_POINT ( 'NONE',  ( 50.67689124139599244, 19.37866773268720166, -76.14999999999999147 ) ) ;
#9340 = CARTESIAN_POINT ( 'NONE',  ( 9.366543050370410128, -15.61630854221780140, -53.84717978381009829 ) ) ;
#9339 = CARTESIAN_POINT ( 'NONE',  ( 43.82411958768233262, 8.707906524021627348, -67.51045570699398013 ) ) ;
#9341 = AXIS2_PLACEMENT_3D ( 'NONE', #4435, #4691, #20402 ) ;
#9342 = CARTESIAN_POINT ( 'NONE',  ( 9.371116658539381916, -14.45533316995461171, -59.90179829052765825 ) ) ;
#9343 = CARTESIAN_POINT ( 'NONE',  ( 23.83903542067694659, -17.68687553889520458, -51.59099914178197110 ) ) ;
#9344 = VERTEX_POINT ( 'NONE', #23709 ) ;
#9345 = EDGE_LOOP ( 'NONE', ( #24704, #49448, #31982, #5658, #10371 ) ) ;
#9346 = ADVANCED_FACE ( 'NONE', ( #8005 ), #11693, .T. ) ;
#9347 = ORIENTED_EDGE ( 'NONE', *, *, #17154, .T. ) ;
#9348 = ORIENTED_EDGE ( 'NONE', *, *, #21371, .T. ) ;
#9349 = CARTESIAN_POINT ( 'NONE',  ( 61.62977292002289431, -45.12285047192839471, -46.49409185169140102 ) ) ;
#9350 = CARTESIAN_POINT ( 'NONE',  ( 53.29384558423090112, 19.31433099946569953, -38.31189016485890875 ) ) ;
#9351 = CARTESIAN_POINT ( 'NONE',  ( 53.78771641980449658, -51.63629534268280707, -53.21849989078959453 ) ) ;
#9352 = ORIENTED_EDGE ( 'NONE', *, *, #17160, .T. ) ;
#9353 = ORIENTED_EDGE ( 'NONE', *, *, #25510, .F. ) ;
#9354 = FACE_OUTER_BOUND ( 'NONE', #29229, .T. ) ;
#9355 = ORIENTED_EDGE ( 'NONE', *, *, #6028, .T. ) ;
#9356 = FACE_OUTER_BOUND ( 'NONE', #6664, .T. ) ;
#9357 = FACE_OUTER_BOUND ( 'NONE', #50941, .T. ) ;
#9358 = CARTESIAN_POINT ( 'NONE',  ( 54.62261979470819995, -51.56116820793610600, -54.09401641884280565 ) ) ;
#9359 = FACE_OUTER_BOUND ( 'NONE', #45226, .T. ) ;
#9360 = ORIENTED_EDGE ( 'NONE', *, *, #16617, .T. ) ;
#9361 = CARTESIAN_POINT ( 'NONE',  ( 20.44965901189399204, -33.35837913196784399, -75.56421356237308373 ) ) ;
#9362 = CARTESIAN_POINT ( 'NONE',  ( 52.53869631642899662, -50.56896709113740229, -76.53474691443801703 ) ) ;
#9363 = CARTESIAN_POINT ( 'NONE',  ( 21.05259680842176806, -20.26422748320269918, -46.69380980240473633 ) ) ;
#9364 = CARTESIAN_POINT ( 'NONE',  ( 14.15276264669880035, -32.59175772023380091, -35.01387690002269437 ) ) ;
#9365 = CARTESIAN_POINT ( 'NONE',  ( 23.96531136779289994, -15.10989917382340053, -67.99194462183569954 ) ) ;
#9366 = ADVANCED_FACE ( 'NONE', ( #39980 ), #28819, .T. ) ;
#9367 = B_SPLINE_CURVE_WITH_KNOTS ( 'NONE', 3,
 ( #16826, #17091, #29124, #317, #12373, #16554, #28336, #20472, #32506, #48535, #12640, #28597, #32773, #48800, #12907, #28862, #5300, #42226, #41699, #9991, #38293, #25955, #29885, #45904, #18358, #13425, #17853, #2132 ),
 .UNSPECIFIED., .F., .F.,
 ( 4, 2, 2, 2, 2, 2, 2, 2, 2, 2, 1, 1, 1, 1, 2, 4 ),
 ( 0.000000000000000000, 0.06250047518423985926, 0.1250009503684797185, 0.1875014255527195917, 0.2500019007369594370, 0.3125023759211992824, 0.3750028511054391833, 0.4375033262896790287, 0.4687535638817990069, 0.4843786826778589960, 0.4921912420758889350, 0.4960975217749039046, 0.4980506616244113061, 0.4990272315491650623, 0.4995155165115419127, 0.5000038014739186520 ),
 .UNSPECIFIED. ) ;
#9368 = CARTESIAN_POINT ( 'NONE',  ( 8.653191590475879380, 17.54226184052370030, -35.01184033120630090 ) ) ;
#9369 = CARTESIAN_POINT ( 'NONE',  ( 45.55533282443069965, 13.99868975454399944, -8.104371290795420180 ) ) ;
#9370 = EDGE_CURVE ( 'NONE', #35625, #12521, #24660, .T. ) ;
#9371 = CARTESIAN_POINT ( 'NONE',  ( 43.02291016728809581, -43.89611171023040015, -5.004961222441979274 ) ) ;
#9372 = DIRECTION ( 'NONE',  ( 0.000000000000000000, 0.000000000000000000, -1.000000000000000000 ) ) ;
#9373 = CARTESIAN_POINT ( 'NONE',  ( 68.38971107296249841, -1.116188944679350037, -18.15384911730639672 ) ) ;
#9374 = CIRCLE ( 'NONE', #50368, 0.5000000000336679573 ) ;
#9375 = AXIS2_PLACEMENT_3D ( 'NONE', #26780, #42795, #51170 ) ;
#9376 = CARTESIAN_POINT ( 'NONE',  ( 63.92116633856140595, 1.061268877959919976, -69.92250879741870051 ) ) ;
#9377 = DIRECTION ( 'NONE',  ( 1.000000000000000000, 2.460964292799963328E-14, 0.000000000000000000 ) ) ;
#9378 = AXIS2_PLACEMENT_3D ( 'NONE', #29415, #45419, #28893 ) ;
#9379 = CARTESIAN_POINT ( 'NONE',  ( 66.62841617083020651, 1.722393603085859981, -19.40721067926959975 ) ) ;
#9380 = ORIENTED_EDGE ( 'NONE', *, *, #2851, .F. ) ;
#9381 = CARTESIAN_POINT ( 'NONE',  ( 14.03647079426650102, -51.35642126254130346, -74.98719232987430416 ) ) ;
#9382 = CARTESIAN_POINT ( 'NONE',  ( 57.34629640291740316, 19.08899856727470379, -52.87029358442639904 ) ) ;
#9383 = CARTESIAN_POINT ( 'NONE',  ( 88.13393739769618662, -29.16618894467940137, -65.65000000000000568 ) ) ;
#9384 = CARTESIAN_POINT ( 'NONE',  ( 17.65356943138449708, -22.50337107214560106, -77.27805344681910071 ) ) ;
#9385 = CARTESIAN_POINT ( 'NONE',  ( 22.88613837897879932, -18.98757059450120011, -32.14999999999999858 ) ) ;
#9386 = CARTESIAN_POINT ( 'NONE',  ( 57.50723798014340105, 13.88381064843590096, -25.33268340738889890 ) ) ;
#9387 = CARTESIAN_POINT ( 'NONE',  ( 11.80006687032470047, 34.19580789139209998, -17.88619248980069898 ) ) ;
#9389 = CARTESIAN_POINT ( 'NONE',  ( 15.82997274079101224, 19.88381105532299387, -21.91305730704999988 ) ) ;
#9388 = CARTESIAN_POINT ( 'NONE',  ( 13.92801754073780174, 19.97389345277590067, -22.96894028473249705 ) ) ;
#9390 = CARTESIAN_POINT ( 'NONE',  ( 23.49471107943040238, -48.44626589137899941, -41.74835364838589413 ) ) ;
#9391 = CARTESIAN_POINT ( 'NONE',  ( 48.57851549001960478, 22.81624679364150055, -54.74774495437689836 ) ) ;
#9392 = ORIENTED_EDGE ( 'NONE', *, *, #16449, .T. ) ;
#9393 = CARTESIAN_POINT ( 'NONE',  ( 23.16321757722399965, -15.04018605219599891, -66.82115454642129748 ) ) ;
#9394 = ORIENTED_EDGE ( 'NONE', *, *, #28430, .T. ) ;
#9395 = CARTESIAN_POINT ( 'NONE',  ( 16.13393739769620083, -15.61618894467929941, 7.849999999999999645 ) ) ;
#9396 = DIRECTION ( 'NONE',  ( 0.000000000000000000, 0.000000000000000000, -1.000000000000000000 ) ) ;
#9397 = CYLINDRICAL_SURFACE ( 'NONE', #42985, 1.000000000000001110 ) ;
#9399 = CARTESIAN_POINT ( 'NONE',  ( 55.68001326603900480, 15.01258945603300177, -25.63522347839200322 ) ) ;
#9398 = CARTESIAN_POINT ( 'NONE',  ( 84.44784216359251161, 11.88381105532070059, -47.47585302082339354 ) ) ;
#9400 = CARTESIAN_POINT ( 'NONE',  ( 9.114236225456030738, -16.29909021797989865, -65.42195104672009620 ) ) ;
#9401 = DIRECTION ( 'NONE',  ( -0.6918010270571991471, -0.3994115091971301434, -0.6015661104845211327 ) ) ;
#9402 = CARTESIAN_POINT ( 'NONE',  ( 56.29021670269609956, -45.11618894467940066, -14.97294918829250143 ) ) ;
#9403 = CARTESIAN_POINT ( 'NONE',  ( 9.807863572223928017, -20.47798425270724465, -80.58399865991046340 ) ) ;
#9404 = EDGE_LOOP ( 'NONE', ( #7598, #15528, #2198, #45694, #28518 ) ) ;
#9405 = ADVANCED_FACE ( 'NONE', ( #31063 ), #43400, .T. ) ;
#9406 = EDGE_LOOP ( 'NONE', ( #44022, #21565, #31894, #49331 ) ) ;
#9407 = CARTESIAN_POINT ( 'NONE',  ( 11.50001307143430118, -64.98824575801700121, -16.62227806134499986 ) ) ;
#9408 = CARTESIAN_POINT ( 'NONE',  ( 12.95715363918909979, 34.28281642642240001, -47.67656520517239471 ) ) ;
#9409 = CARTESIAN_POINT ( 'NONE',  ( 13.39314902935926099, -8.114200813603156703, -38.89594400110460271 ) ) ;
#9410 = CIRCLE ( 'NONE', #26964, 5.999999999999998224 ) ;
#9411 = CARTESIAN_POINT ( 'NONE',  ( 24.04470022272198193, -15.61619473591594698, -59.79232576333501470 ) ) ;
#9412 = CARTESIAN_POINT ( 'NONE',  ( 61.98540824044656006, 0.9838110553206419473, -61.18283208257727779 ) ) ;
#9413 = CIRCLE ( 'NONE', #37005, 17.09468304687054996 ) ;
#9414 = ORIENTED_EDGE ( 'NONE', *, *, #26096, .T. ) ;
#9415 = CARTESIAN_POINT ( 'NONE',  ( -19.05153563686570095, -33.04232519026420078, -51.54856132249189216 ) ) ;
#9416 = DIRECTION ( 'NONE',  ( 0.000000000000000000, 0.000000000000000000, 1.000000000000000000 ) ) ;
#9417 = CARTESIAN_POINT ( 'NONE',  ( 47.94498215251270068, 23.43361079511839762, -55.53475709714179942 ) ) ;
#9418 = CARTESIAN_POINT ( 'NONE',  ( 72.69742484592399023, 1.402336724396409995, -68.91862208776170462 ) ) ;
#9419 = CARTESIAN_POINT ( 'NONE',  ( 50.47459759387780309, -50.28724450852030259, -76.14999999999999147 ) ) ;
#9420 = CARTESIAN_POINT ( 'NONE',  ( -18.86606260230390220, 19.38381105532060289, 16.85000000000000142 ) ) ;
#9421 = ORIENTED_EDGE ( 'NONE', *, *, #48044, .F. ) ;
#9422 =( NAMED_UNIT ( * ) SI_UNIT ( $, .STERADIAN. ) SOLID_ANGLE_UNIT ( ) );
#9423 = CARTESIAN_POINT ( 'NONE',  ( 65.43042069958036677, 17.98087126524680102, -74.20351669811765305 ) ) ;
#9424 = VERTEX_POINT ( 'NONE', #47089 ) ;
#9425 = CARTESIAN_POINT ( 'NONE',  ( 4.133937397696209715, -22.54439217495480108, -47.64999999999999858 ) ) ;
#9426 = CARTESIAN_POINT ( 'NONE',  ( 45.64502415131030233, -46.12165179014160543, -9.406922201967550023 ) ) ;
#9427 = CARTESIAN_POINT ( 'NONE',  ( 10.29329494695989844, -20.85771957553910028, -36.77968578276969680 ) ) ;
#9428 = CARTESIAN_POINT ( 'NONE',  ( 13.72898021142920122, -51.28551575856799616, -22.65893573105330105 ) ) ;
#9429 = CARTESIAN_POINT ( 'NONE',  ( 54.00166005263069735, 19.61159079012060147, -76.07248000621819983 ) ) ;
#9430 = ADVANCED_FACE ( 'NONE', ( #42894 ), #39207, .T. ) ;
#9431 = CARTESIAN_POINT ( 'NONE',  ( 47.43599255125010217, -54.63612274721339901, -74.14999999999999147 ) ) ;
#9432 = ORIENTED_EDGE ( 'NONE', *, *, #39582, .T. ) ;
#9433 = CARTESIAN_POINT ( 'NONE',  ( 54.90608630352579667, 14.46110100129650000, -15.60660465066449909 ) ) ;
#9434 = CARTESIAN_POINT ( 'NONE',  ( 57.19702055511909577, -50.61594403054400004, -53.75054411264890319 ) ) ;
#9435 = CARTESIAN_POINT ( 'NONE',  ( 52.57286858291280396, -49.85400817756870140, -48.51318051594920178 ) ) ;
#9436 = CARTESIAN_POINT ( 'NONE',  ( 9.736239135216329998, -12.64768492468660099, -37.98546363926389802 ) ) ;
#9437 = CARTESIAN_POINT ( 'NONE',  ( 34.00893739769620083, -11.50256827670329862, -35.14999999999999858 ) ) ;
#9438 = VERTEX_POINT ( 'NONE', #38960 ) ;
#9439 = CARTESIAN_POINT ( 'NONE',  ( 46.39504675003949785, 21.75098124655080056, -76.14870548336060097 ) ) ;
#9440 = CARTESIAN_POINT ( 'NONE',  ( 65.19259745005730622, 1.384447124000270035, -60.97624892474630087 ) ) ;
#9441 = CARTESIAN_POINT ( 'NONE',  ( 75.16123461437827302, -29.48656911042399287, -11.85229885355600565 ) ) ;
#9442 = AXIS2_PLACEMENT_3D ( 'NONE', #8185, #48530, #8965 ) ;
#9443 = CIRCLE ( 'NONE', #21942, 48.00000000000000000 ) ;
#9444 = CARTESIAN_POINT ( 'NONE',  ( 12.36320305067610015, 33.31445045643330616, -15.76422791930239953 ) ) ;
#9445 = CARTESIAN_POINT ( 'NONE',  ( 20.00857004538559991, -22.63715434125480286, -81.84667608724390675 ) ) ;
#9446 = DIRECTION ( 'NONE',  ( -1.000000000000000000, 0.000000000000000000, 0.000000000000000000 ) ) ;
#9448 = CARTESIAN_POINT ( 'NONE',  ( 45.09311312900799606, -39.18053832272051551, -65.04754641029070683 ) ) ;
#9447 = CARTESIAN_POINT ( 'NONE',  ( 64.81979753630260177, 0.8904513541338869853, -60.64834380034769623 ) ) ;
#9449 = CARTESIAN_POINT ( 'NONE',  ( 61.16806598196220079, 14.05986850724769965, -46.71992872349159853 ) ) ;
#9450 = CARTESIAN_POINT ( 'NONE',  ( -12.74467463197679962, -57.05710031237479996, -53.24963421316559931 ) ) ;
#9451 = ORIENTED_EDGE ( 'NONE', *, *, #11914, .F. ) ;
#9452 = B_SPLINE_CURVE_WITH_KNOTS ( 'NONE', 3,
 ( #18153, #14996, #34119, #46215, #2423, #34641, #42269, #6366, #38604, #22328, #30964, #27047, #46994, #38334, #7147, #22841, #18408, #6623, #23099, #50646, #34383, #2951, #18921, #30712, #50395, #46734, #39117, #3211, #30452, #10561 ),
 .UNSPECIFIED., .F., .F.,
 ( 4, 2, 2, 2, 2, 2, 2, 2, 2, 2, 2, 2, 2, 2, 4 ),
 ( -1.979714999999999961E-13, 0.09067111850398298922, 0.2140247704412500118, 0.2911208029020420085, 0.3773788185767790737, 0.4312900783734900378, 0.4852013381702010020, 0.5283303460075698954, 0.5714593538449389554, 0.6404657663847290738, 0.6753592001671930856, 0.7102526339496559871, 0.7544412783218740204, 0.8251431093174219633, 0.8625801567471780285 ),
 .UNSPECIFIED. ) ;
#9453 = CARTESIAN_POINT ( 'NONE',  ( 53.37783364382759999, -49.37513790283500015, -48.82822306731589634 ) ) ;
#9454 = ORIENTED_EDGE ( 'NONE', *, *, #29710, .T. ) ;
#9455 = CARTESIAN_POINT ( 'NONE',  ( 57.46922327009529852, -45.13092459265400436, -25.53935936133710172 ) ) ;
#9456 = CARTESIAN_POINT ( 'NONE',  ( 47.65668213871590098, -54.52839204276340013, -55.15716614278580465 ) ) ;
#9457 = CARTESIAN_POINT ( 'NONE',  ( 56.70381597338830204, 14.06601603320560123, -25.50387274212789634 ) ) ;
#9458 = CARTESIAN_POINT ( 'NONE',  ( 16.36944352332099939, -22.66507394177369861, -32.94218931063619493 ) ) ;
#9459 = CARTESIAN_POINT ( 'NONE',  ( 50.39461195648269864, 18.90258328430419965, -76.14999999999999147 ) ) ;
#9460 = CARTESIAN_POINT ( 'NONE',  ( 53.03535125111080362, 18.33408603822369898, -48.94674794257169737 ) ) ;
#9461 = CARTESIAN_POINT ( 'NONE',  ( 71.39250861737149023, 1.096110717717199812, -70.63920630446268945 ) ) ;
#9462 = CARTESIAN_POINT ( 'NONE',  ( 60.28107860282390362, -45.75696393620810198, -47.25802466845119909 ) ) ;
#9463 = CARTESIAN_POINT ( 'NONE',  ( 71.85433366084710372, -45.11618894467940066, -14.09557305447640019 ) ) ;
#9464 = VECTOR ( 'NONE', #45884, 1000.000000000000000 ) ;
#9465 = ORIENTED_EDGE ( 'NONE', *, *, #45307, .T. ) ;
#9466 = ADVANCED_FACE ( 'NONE', ( #19022 ), #41011, .T. ) ;
#9467 = CARTESIAN_POINT ( 'NONE',  ( 14.29369635269939920, -8.396756332995028771, -74.48789696905259916 ) ) ;
#9468 = CARTESIAN_POINT ( 'NONE',  ( 72.80537809983910336, 1.383767307422960169, -68.70744520365728647 ) ) ;
#9469 = CARTESIAN_POINT ( 'NONE',  ( 47.51629483024640166, -54.56948809585979632, -54.66793506916069845 ) ) ;
#9470 = CARTESIAN_POINT ( 'NONE',  ( 61.75019796695539753, 14.88381105532069881, -28.15000000000000213 ) ) ;
#9471 = CARTESIAN_POINT ( 'NONE',  ( 16.13393739769620083, -15.61618894467929941, -28.45282021618999835 ) ) ;
#9472 = CARTESIAN_POINT ( 'NONE',  ( 60.69770788394099981, 14.26247553725569972, -47.37008640455089648 ) ) ;
#9474 = ADVANCED_FACE ( 'NONE', ( #28161 ), #48624, .T. ) ;
#9473 = CARTESIAN_POINT ( 'NONE',  ( 71.50564047255809896, 1.187296498006439993, -60.79044767480839795 ) ) ;
#9475 = DIRECTION ( 'NONE',  ( -0.4999999999999998890, 0.8660254037844387076, 0.000000000000000000 ) ) ;
#9476 = CARTESIAN_POINT ( 'NONE',  ( 71.86457203492498991, 0.9897451961560271849, -60.94993607748450160 ) ) ;
#9477 = DIRECTION ( 'NONE',  ( 0.000000000000000000, 0.000000000000000000, -1.000000000000000000 ) ) ;
#9478 = ADVANCED_FACE ( 'NONE', ( #12724 ), #34698, .T. ) ;
#9479 = CARTESIAN_POINT ( 'NONE',  ( 64.80090148641970416, 1.186614556332910020, -70.53308468150621025 ) ) ;
#9480 = ORIENTED_EDGE ( 'NONE', *, *, #40847, .T. ) ;
#9481 = CARTESIAN_POINT ( 'NONE',  ( 9.744582219142259305, -63.29038400323761238, -46.29748084500919703 ) ) ;
#9482 = DIRECTION ( 'NONE',  ( 1.000000000000000000, 0.000000000000000000, 0.000000000000000000 ) ) ;
#9483 = ORIENTED_EDGE ( 'NONE', *, *, #24609, .T. ) ;
#9484 = CARTESIAN_POINT ( 'NONE',  ( 11.13393739769479929, -63.52234716422830729, -43.76018014099159359 ) ) ;
#9485 = DIRECTION ( 'NONE',  ( 0.8320502943378423888, -5.155044000000003308E-14, -0.5547001962252312568 ) ) ;
#9486 = CARTESIAN_POINT ( 'NONE',  ( 12.14988109189271626, -22.52875461132841650, -70.17433619596677374 ) ) ;
#9487 = CARTESIAN_POINT ( 'NONE',  ( 52.81902780364940497, 19.43027145643710085, -76.50043241533330729 ) ) ;
#9488 = CIRCLE ( 'NONE', #35423, 1.999999999999998224 ) ;
#9489 = VERTEX_POINT ( 'NONE', #24993 ) ;
#9490 = AXIS2_PLACEMENT_3D ( 'NONE', #50736, #6205, #31057 ) ;
#9491 = DIRECTION ( 'NONE',  ( -1.000000000000000000, -2.362305513541788125E-32, -1.430038757655089944E-15 ) ) ;
#9492 = CARTESIAN_POINT ( 'NONE',  ( 14.13393739769619906, -41.61618894467930119, -35.14999999999999858 ) ) ;
#9493 = CARTESIAN_POINT ( 'NONE',  ( 11.66815189201670400, -41.66761415519156486, -34.89146800830130246 ) ) ;
#9494 = CARTESIAN_POINT ( 'NONE',  ( 11.08608504019470153, -22.13553758030240104, -50.50205474731569666 ) ) ;
#9495 = CARTESIAN_POINT ( 'NONE',  ( -23.86606260230380272, -15.61618894467908092, -48.64999999999999858 ) ) ;
#9496 = CARTESIAN_POINT ( 'NONE',  ( 41.65893704031727651, -37.56744562278856137, -82.02500123744080440 ) ) ;
#9497 = ADVANCED_FACE ( 'NONE', ( #653 ), #12128, .F. ) ;
#9498 = VERTEX_POINT ( 'NONE', #16381 ) ;
#9499 = CARTESIAN_POINT ( 'NONE',  ( 57.34776334542480214, -45.81180625069929846, -26.27178910182970029 ) ) ;
#9500 = CARTESIAN_POINT ( 'NONE',  ( 8.684961965424408348, -15.47669408973130167, -45.23861751603709536 ) ) ;
#9501 = CARTESIAN_POINT ( 'NONE',  ( 24.04462826173309153, -15.61618628916268392, -33.50766512250601181 ) ) ;
#9502 = AXIS2_PLACEMENT_3D ( 'NONE', #48320, #28378, #44386 ) ;
#9503 = CARTESIAN_POINT ( 'NONE',  ( 13.42153893133809994, 20.57176844745109889, -74.52171359303420672 ) ) ;
#9504 = CARTESIAN_POINT ( 'NONE',  ( 16.13393739769620083, -15.61618894467929941, 10.84999999999999964 ) ) ;
#9505 = CARTESIAN_POINT ( 'NONE',  ( 82.46791274550251671, -45.09332969728169616, -46.45744338702549925 ) ) ;
#9506 = EDGE_CURVE ( 'NONE', #11807, #31098, #19149, .T. ) ;
#9507 = CARTESIAN_POINT ( 'NONE',  ( 12.11646325030310045, -8.416006850870608957, -50.84566773101410320 ) ) ;
#9508 = ORIENTED_EDGE ( 'NONE', *, *, #20873, .T. ) ;
#9509 = CARTESIAN_POINT ( 'NONE',  ( 54.36039143410459928, -47.84659789142740038, -25.99973999818690018 ) ) ;
#9510 = CARTESIAN_POINT ( 'NONE',  ( -2.727866001178802513, -15.61618894467929941, 17.07360679774999923 ) ) ;
#9511 = CARTESIAN_POINT ( 'NONE',  ( 7.094823580868710344, 28.68663061054669683, -12.04540313013450081 ) ) ;
#9512 = CIRCLE ( 'NONE', #37112, 4.999999999969890752 ) ;
#9513 = CARTESIAN_POINT ( 'NONE',  ( 10.61751707702059910, -64.82563018155620682, -22.25048313876769868 ) ) ;
#9514 = CARTESIAN_POINT ( 'NONE',  ( 73.26121012496899709, 0.8838110553206759423, -62.53374032209040223 ) ) ;
#9515 = AXIS2_PLACEMENT_3D ( 'NONE', #46333, #22706, #42128 ) ;
#9516 = ORIENTED_EDGE ( 'NONE', *, *, #48224, .T. ) ;
#9517 = CARTESIAN_POINT ( 'NONE',  ( -7.614741595775099903, -45.32579099379800169, -5.329995886356219792 ) ) ;
#9518 = CIRCLE ( 'NONE', #12850, 9.999999999999998224 ) ;
#9519 = CARTESIAN_POINT ( 'NONE',  ( 47.45990050842959818, 23.38532434082769740, -54.77936059081219611 ) ) ;
#9520 = CARTESIAN_POINT ( 'NONE',  ( -11.59939519670759189, -33.93743706034221219, -49.87766020311142512 ) ) ;
#9521 = CARTESIAN_POINT ( 'NONE',  ( 63.45453858566830974, 1.370853092582090094, -62.43091793016829882 ) ) ;
#9522 = FACE_OUTER_BOUND ( 'NONE', #20569, .T. ) ;
#9523 = CARTESIAN_POINT ( 'NONE',  ( 11.10018436985160051, 33.80960200586510211, -17.19464589430749868 ) ) ;
#9524 = CARTESIAN_POINT ( 'NONE',  ( 9.543075519110143290, -17.38747768618387113, -53.36948666754615545 ) ) ;
#9525 = CARTESIAN_POINT ( 'NONE',  ( 52.94585586128479093, 18.36771476006709847, -48.75076952771310346 ) ) ;
#9526 = CARTESIAN_POINT ( 'NONE',  ( 8.222937397696199469, -15.61618894467929941, -32.14999999999999858 ) ) ;
#9527 = CARTESIAN_POINT ( 'NONE',  ( 58.73840381835399427, -46.66147107097890512, -47.90022353259229249 ) ) ;
#9528 = CARTESIAN_POINT ( 'NONE',  ( 22.89191656196409497, -15.97301087214540338, -66.46960767138124027 ) ) ;
#9529 = CARTESIAN_POINT ( 'NONE',  ( 52.59105628395929699, 20.91324755812640035, -53.43271834460720271 ) ) ;
#9530 = CARTESIAN_POINT ( 'NONE',  ( 63.45118475302019334, 1.239064938996009779, -69.25399354804109464 ) ) ;
#9531 = CARTESIAN_POINT ( 'NONE',  ( 22.90114886013774864, -15.61618877916400017, -48.45281860778688809 ) ) ;
#9532 = ORIENTED_EDGE ( 'NONE', *, *, #11168, .T. ) ;
#9533 = CARTESIAN_POINT ( 'NONE',  ( 9.367009201240112048, -16.00442573649115374, -73.82892668254670809 ) ) ;
#9534 = CARTESIAN_POINT ( 'NONE',  ( 8.959210788195541397, 31.93568363525710296, -46.63329613156509623 ) ) ;
#9535 = DIRECTION ( 'NONE',  ( 1.000000000000000000, 2.460964292799963328E-14, 0.000000000000000000 ) ) ;
#9536 = CARTESIAN_POINT ( 'NONE',  ( 67.94623181482140239, -30.09959995773170149, -17.85819628216900057 ) ) ;
#9537 = EDGE_CURVE ( 'NONE', #24151, #2565, #22631, .T. ) ;
#9538 = CARTESIAN_POINT ( 'NONE',  ( 17.93516875359370388, 20.31584378320569684, -75.38352342698830455 ) ) ;
#9539 = ORIENTED_EDGE ( 'NONE', *, *, #4678, .T. ) ;
#9540 = VERTEX_POINT ( 'NONE', #50434 ) ;
#9541 = CARTESIAN_POINT ( 'NONE',  ( 15.10238578887267735, 12.66681598883027426, -61.51477253168943804 ) ) ;
#9542 = EDGE_LOOP ( 'NONE', ( #35628, #18676, #50838, #32161 ) ) ;
#9543 = CARTESIAN_POINT ( 'NONE',  ( 10.41833236504899851, -64.35094718373520095, -46.41941406982350316 ) ) ;
#9544 = CARTESIAN_POINT ( 'NONE',  ( 56.67773033073410005, -45.66254785057299870, -26.04367575654990219 ) ) ;
#9545 = CARTESIAN_POINT ( 'NONE',  ( 24.04492097598215850, -15.63439488930047716, -77.50840237685744682 ) ) ;
#9546 = DIRECTION ( 'NONE',  ( 0.000000000000000000, 0.000000000000000000, -1.000000000000000000 ) ) ;
#9547 = CARTESIAN_POINT ( 'NONE',  ( 61.40746854249709941, 14.07231923713010069, -47.19815667451499763 ) ) ;
#9548 = DIRECTION ( 'NONE',  ( 0.4743737082415241391, -0.8803235683140518963, 0.000000000000000000 ) ) ;
#9549 = ORIENTED_EDGE ( 'NONE', *, *, #35058, .F. ) ;
#9550 = CARTESIAN_POINT ( 'NONE',  ( 46.35743359015805254, 6.957031320103493677, -58.53251102570533959 ) ) ;
#9551 = EDGE_LOOP ( 'NONE', ( #7594, #18130, #24053, #5523, #32250, #25099 ) ) ;
#9552 = CARTESIAN_POINT ( 'NONE',  ( 50.44925730351350524, -45.58854146516910077, -12.26883546960940130 ) ) ;
#9553 = CARTESIAN_POINT ( 'NONE',  ( -0.9510857394171997603, -26.69247394909374904, -59.64999999999999147 ) ) ;
#9554 = FACE_OUTER_BOUND ( 'NONE', #1362, .T. ) ;
#9555 = ORIENTED_EDGE ( 'NONE', *, *, #51762, .T. ) ;
#9556 = DIRECTION ( 'NONE',  ( 1.000000000000000000, 0.000000000000000000, 0.000000000000000000 ) ) ;
#9557 = CARTESIAN_POINT ( 'NONE',  ( 46.57724752952230318, -53.42760099267549379, -76.07728942632040514 ) ) ;
#9558 = CARTESIAN_POINT ( 'NONE',  ( 61.13405154998650204, 14.40638383414069956, -47.71032547765840093 ) ) ;
#9559 = CARTESIAN_POINT ( 'NONE',  ( 48.87615309687829779, 13.88381105525199999, -9.792211629500439329 ) ) ;
#9560 = CARTESIAN_POINT ( 'NONE',  ( 20.13393739768869750, 24.18330853958710236, -76.14999999999999147 ) ) ;
#9561 = CARTESIAN_POINT ( 'NONE',  ( -1.733483264138872437, -50.41034150931718472, -6.209623304567350566 ) ) ;
#9562 = CARTESIAN_POINT ( 'NONE',  ( 58.48388423183219942, 13.89519089340790181, -25.73063636213230154 ) ) ;
#9563 = EDGE_CURVE ( 'NONE', #22762, #16412, #7928, .T. ) ;
#9564 = CARTESIAN_POINT ( 'NONE',  ( 11.96663413069190085, -8.966351979459819432, -76.60931421723039136 ) ) ;
#9565 = VERTEX_POINT ( 'NONE', #34157 ) ;
#9567 = EDGE_CURVE ( 'NONE', #10507, #1081, #14132, .T. ) ;
#9566 = DIRECTION ( 'NONE',  ( 0.000000000000000000, 0.000000000000000000, 1.000000000000000000 ) ) ;
#9568 = CARTESIAN_POINT ( 'NONE',  ( 73.08672326322148649, 0.8966068345641480253, -62.26318953425310099 ) ) ;
#9569 = CARTESIAN_POINT ( 'NONE',  ( 76.80638706214371325, -40.88990971753789694, -14.54769496735189982 ) ) ;
#9570 = CARTESIAN_POINT ( 'NONE',  ( 72.85189580008329813, 1.309820314133779862, -69.05029809067748658 ) ) ;
#9571 = EDGE_CURVE ( 'NONE', #38625, #26843, #46253, .T. ) ;
#9572 = CARTESIAN_POINT ( 'NONE',  ( 10.85466640530910176, -64.96697012893029921, -17.55961383758990024 ) ) ;
#9573 = CARTESIAN_POINT ( 'NONE',  ( 8.223439258000311725, -15.61632852289070073, -42.50766849176289952 ) ) ;
#9574 = CARTESIAN_POINT ( 'NONE',  ( 20.99558011316242201, -9.289995339025649557, -59.50070245799219748 ) ) ;
#9575 = CARTESIAN_POINT ( 'NONE',  ( 49.07734691198550081, -53.89406825560470082, -54.92337139623040088 ) ) ;
#9576 = CARTESIAN_POINT ( 'NONE',  ( 42.35079386031210191, -44.32234244509449894, -5.113119501825009294 ) ) ;
#9577 = AXIS2_PLACEMENT_3D ( 'NONE', #14937, #30391, #43253 ) ;
#9578 = CARTESIAN_POINT ( 'NONE',  ( 24.04225747343017972, -15.83852975785987560, -33.51661210754224385 ) ) ;
#9579 = CARTESIAN_POINT ( 'NONE',  ( 18.78671361505629633, -51.59709463796549755, -74.36013246830410139 ) ) ;
#9580 = CARTESIAN_POINT ( 'NONE',  ( 13.89790909569722643, -39.31946990788019747, -75.56421356237308373 ) ) ;
#9581 = VERTEX_POINT ( 'NONE', #5642 ) ;
#9582 = CARTESIAN_POINT ( 'NONE',  ( 15.56802502463160032, -8.187431476276259446, -44.54314102700439548 ) ) ;
#9583 = CARTESIAN_POINT ( 'NONE',  ( 64.03801787523769917, 1.197080272271600077, -61.30148670604589967 ) ) ;
#9584 = VERTEX_POINT ( 'NONE', #49411 ) ;
#9585 = CARTESIAN_POINT ( 'NONE',  ( 16.13393739769620083, -15.61618894467929941, -54.64999999999999858 ) ) ;
#9586 = CARTESIAN_POINT ( 'NONE',  ( 60.59128431671459936, -45.75012338594650174, -47.69436703140129907 ) ) ;
#9587 = CARTESIAN_POINT ( 'NONE',  ( 12.20533024450969961, -21.47354372396169708, -75.53523696341939342 ) ) ;
#9588 = CARTESIAN_POINT ( 'NONE',  ( 44.13393739769620083, -36.11618894467930119, -34.64999999999999858 ) ) ;
#9590 = CARTESIAN_POINT ( 'NONE',  ( 22.90070561427262064, -15.61618657793558818, -56.45282510079097449 ) ) ;
#9589 = CARTESIAN_POINT ( 'NONE',  ( 43.52531948755864732, 8.681712052945677272, -68.95854737653661459 ) ) ;
#9591 = CARTESIAN_POINT ( 'NONE',  ( 51.19516171219699885, -51.09621740586149485, -76.13919816896859061 ) ) ;
#9592 = FACE_OUTER_BOUND ( 'NONE', #34127, .T. ) ;
#9593 = EDGE_CURVE ( 'NONE', #38190, #18993, #42573, .T. ) ;
#9594 = ORIENTED_EDGE ( 'NONE', *, *, #359, .T. ) ;
#9595 = VERTEX_POINT ( 'NONE', #6665 ) ;
#9596 = VERTEX_POINT ( 'NONE', #6411 ) ;
#9597 = ORIENTED_EDGE ( 'NONE', *, *, #14901, .T. ) ;
#9598 = CARTESIAN_POINT ( 'NONE',  ( 61.05611720366390216, -45.35089833204299481, -46.88541463101370255 ) ) ;
#9599 = CARTESIAN_POINT ( 'NONE',  ( 52.95029351598290646, -49.64428300453829479, -49.05315204363950699 ) ) ;
#9600 = CARTESIAN_POINT ( 'NONE',  ( 66.70013194292150160, -29.76883965895079953, -17.02746303015019791 ) ) ;
#9601 =( BOUNDED_CURVE ( )  B_SPLINE_CURVE ( 2, ( #23961, #7762, #15876 ),
 .UNSPECIFIED., .F., .T. ) 
 B_SPLINE_CURVE_WITH_KNOTS ( ( 3, 3 ),
 ( 0.2168422315592359872, 3.147551163859270140 ),
 .UNSPECIFIED. ) 
 CURVE ( )  GEOMETRIC_REPRESENTATION_ITEM ( )  RATIONAL_B_SPLINE_CURVE ( ( 1.000597593688249853, 1.004455541114980033, 1.003436844929630034 ) ) 
 REPRESENTATION_ITEM ( '' )  );
#9602 = CARTESIAN_POINT ( 'NONE',  ( 53.88967637140569877, -51.75719455529880264, -53.52284543613809831 ) ) ;
#9603 = VERTEX_POINT ( 'NONE', #29970 ) ;
#9604 = ORIENTED_EDGE ( 'NONE', *, *, #33939, .F. ) ;
#9605 = EDGE_LOOP ( 'NONE', ( #13089, #36284, #35297, #3585 ) ) ;
#9606 = CARTESIAN_POINT ( 'NONE',  ( 9.543025774841634501, -17.38729682769319851, -73.36947041500459932 ) ) ;
#9607 = VECTOR ( 'NONE', #29255, 1000.000000000000000 ) ;
#9608 = DIRECTION ( 'NONE',  ( -1.000000000000000000, 0.000000000000000000, 0.000000000000000000 ) ) ;
#9609 = DIRECTION ( 'NONE',  ( 0.000000000000000000, -1.000000000000000000, 0.000000000000000000 ) ) ;
#9610 = VERTEX_POINT ( 'NONE', #33904 ) ;
#9611 = CARTESIAN_POINT ( 'NONE',  ( 15.82777515116789679, 19.71296418728957889, -15.66098702019284516 ) ) ;
#9612 = CARTESIAN_POINT ( 'NONE',  ( 52.30891884663609659, -50.47057820349319712, -76.54990093660988748 ) ) ;
#9613 = CARTESIAN_POINT ( 'NONE',  ( 60.89998638923590590, 14.20032291693460103, -46.98170749212670216 ) ) ;
#9614 = CARTESIAN_POINT ( 'NONE',  ( 15.72727022423829979, -7.779010281307280117, -61.49599227461899176 ) ) ;
#9615 = DIRECTION ( 'NONE',  ( 0.3294064756440921449, -0.9441882088883224444, 0.000000000000000000 ) ) ;
#9616 = CARTESIAN_POINT ( 'NONE',  ( 42.44160469162459748, 13.71702471974399984, -5.942261413879579734 ) ) ;
#9617 = CARTESIAN_POINT ( 'NONE',  ( 41.87064575245250353, -44.48858809718330320, -5.149961107190939913 ) ) ;
#9618 = CARTESIAN_POINT ( 'NONE',  ( 72.33393739769618946, 1.883811055320669947, -62.44999999999999574 ) ) ;
#9619 = FACE_OUTER_BOUND ( 'NONE', #28390, .T. ) ;
#9620 = CARTESIAN_POINT ( 'NONE',  ( 64.07869229662848909, 1.409273244282670090, -69.84075035169790624 ) ) ;
#9621 = CARTESIAN_POINT ( 'NONE',  ( 47.05485148372110160, 8.151374499743630153, -53.95852907688490063 ) ) ;
#9622 = CARTESIAN_POINT ( 'NONE',  ( 66.37093321642988997, -0.5958227600134150537, -16.96665182656099802 ) ) ;
#9623 = EDGE_LOOP ( 'NONE', ( #43719, #40520, #50872, #5998, #28266, #51770 ) ) ;
#9625 = EDGE_CURVE ( 'NONE', #11039, #13741, #50172, .T. ) ;
#9624 = CARTESIAN_POINT ( 'NONE',  ( 14.98352178517470001, -52.93377250084219554, -76.14999999999999147 ) ) ;
#9626 = DIRECTION ( 'NONE',  ( -1.000000000000000000, 0.000000000000000000, 0.000000000000000000 ) ) ;
#9627 = EDGE_CURVE ( 'NONE', #39697, #15474, #2215, .T. ) ;
#9628 = CARTESIAN_POINT ( 'NONE',  ( 16.13393739769620083, -15.61618894467929941, -16.68902128623620129 ) ) ;
#9629 = CARTESIAN_POINT ( 'NONE',  ( 24.04478666521990959, -15.61618936535764668, -45.50767606031119783 ) ) ;
#9630 = CARTESIAN_POINT ( 'NONE',  ( 23.31206043505390113, -14.77700110635539943, -32.14999999999999858 ) ) ;
#9631 = DIRECTION ( 'NONE',  ( -0.6653150774946530177, -0.7465626883646704348, 0.000000000000000000 ) ) ;
#9632 = VECTOR ( 'NONE', #44736, 1000.000000000000000 ) ;
#9633 = CARTESIAN_POINT ( 'NONE',  ( 18.52893071939554659, -8.054308810067066560, -45.10530462550206465 ) ) ;
#9634 = CARTESIAN_POINT ( 'NONE',  ( 16.13393739769620083, -15.61618894467929941, 9.349999999999999645 ) ) ;
#9635 = CARTESIAN_POINT ( 'NONE',  ( 48.19073678848020137, 23.05382179323920155, -55.06660192028969902 ) ) ;
#9636 = ORIENTED_EDGE ( 'NONE', *, *, #36590, .T. ) ;
#9637 = CARTESIAN_POINT ( 'NONE',  ( 20.21022320103229930, -9.860630481422070659, -62.54333226898589260 ) ) ;
#9638 = ORIENTED_EDGE ( 'NONE', *, *, #10592, .T. ) ;
#9639 = CARTESIAN_POINT ( 'NONE',  ( 82.75389768041466709, 14.36255265567944406, -47.67226356402779430 ) ) ;
#9640 = CARTESIAN_POINT ( 'NONE',  ( 60.14148612135956284, -47.18849741077894322, -49.41070014483602080 ) ) ;
#9641 = CARTESIAN_POINT ( 'NONE',  ( 10.72266201305779987, -19.77491659247544220, -43.24448676293776828 ) ) ;
#9643 = CARTESIAN_POINT ( 'NONE',  ( 55.48825172393549821, 15.25629303179229979, -25.68709965441729892 ) ) ;
#9642 = CARTESIAN_POINT ( 'NONE',  ( 82.57306898050261168, 13.95576942188810143, -46.98632580443239704 ) ) ;
#9644 = CARTESIAN_POINT ( 'NONE',  ( 22.33192981211439943, -12.25056140624900003, -74.29447132584550673 ) ) ;
#9645 = CARTESIAN_POINT ( 'NONE',  ( 11.57186432615972471, 33.71257428197281314, -16.50172565923971035 ) ) ;
#9646 = CARTESIAN_POINT ( 'NONE',  ( 72.77398937677050128, 1.387412027389909985, -68.69511434646409498 ) ) ;
#9647 = CARTESIAN_POINT ( 'NONE',  ( 16.13393739769620083, -15.61618894467929941, -32.14999999999999858 ) ) ;
#9648 = EDGE_CURVE ( 'NONE', #18491, #3105, #26315, .T. ) ;
#9649 = B_SPLINE_SURFACE_WITH_KNOTS ( 'NONE', 3, 3, ( 
 ( #393, #39977, #32079, #48621, #31827, #24732, #15870, #32335, #36033, #20549, #12720, #8781, #48097, #47843 ),
 ( #20813, #24472, #12196, #28157, #44942, #912, #5121, #16908, #51768, #40484, #36282, #48355, #12448, #21073 ),
 ( #11949, #36544, #27904, #43908, #8002, #44160, #28418, #8257, #24208, #23954, #4576, #650, #16633, #37583 ),
 ( #5884, #49912, #33901, #1437, #17169, #38115, #29966, #45721, #5374, #21329, #30233, #14007, #42307, #2211 ),
 ( #9821, #5639, #25515, #49665, #6407, #17422, #33121, #21850, #37077, #29196, #17930, #46250, #37857, #21585 ),
 ( #10339, #37336, #45985, #33388, #49406, #22104, #10077, #13503, #41520, #1173, #9315, #13753, #45464, #41264 ),
 ( #29459, #25259, #18188, #9562, #49150, #14265, #13246, #1692, #45203, #17678, #33646, #34154, #29709, #1953 ),
 ( #42046, #25773, #50168, #26036, #26297, #41780, #6149, #22625, #47284, #27083, #50680, #23384, #35203, #47029 ),
 ( #43343, #11375, #30488, #38898, #43087, #51206, #34939, #34679, #35467, #7179, #15034, #31002, #34420, #2462 ) ),
 .UNSPECIFIED., .F., .F., .F.,
 ( 4, 1, 1, 1, 1, 1, 4 ),
 ( 4, 2, 2, 2, 2, 2, 4 ),
 ( -0.0005599991503559129851, 0.1666666666666670182, 0.3333333333333329818, 0.5000000000000000000, 0.6666666666666670737, 0.8333333333333330373, 1.000498765355949837 ),
 ( -1.222991916297710091, -1.090716821865840069, -0.9543772191326050924, -0.7362338547594379223, -0.4169048829278029777, -0.06920342394185401147, 0.0005257736236440000441 ),
 .UNSPECIFIED. ) ;
#9650 = DIRECTION ( 'NONE',  ( 0.000000000000000000, 0.000000000000000000, -1.000000000000000000 ) ) ;
#9651 = ORIENTED_EDGE ( 'NONE', *, *, #38361, .F. ) ;
#9652 = EDGE_CURVE ( 'NONE', #38817, #37903, #48102, .T. ) ;
#9653 = VERTEX_POINT ( 'NONE', #45988 ) ;
#9654 = CARTESIAN_POINT ( 'NONE',  ( 12.05299951489469912, -65.27260376066310243, -16.91217736885799994 ) ) ;
#9655 = CARTESIAN_POINT ( 'NONE',  ( 12.47552258722870100, 34.20483690453190206, -47.26471363895340261 ) ) ;
#9656 = CARTESIAN_POINT ( 'NONE',  ( 68.13393739769618662, -0.1661889446793599900, -100.2061629005786898 ) ) ;
#9657 = CARTESIAN_POINT ( 'NONE',  ( 17.92370450339619836, 19.88381105532299742, -74.14999999999999147 ) ) ;
#9658 = CARTESIAN_POINT ( 'NONE',  ( 50.97614579714448979, 4.031109038251211807, -76.38790111114094827 ) ) ;
#9659 = ORIENTED_EDGE ( 'NONE', *, *, #37388, .F. ) ;
#9660 = CARTESIAN_POINT ( 'NONE',  ( -22.69159524740030065, -18.52108238997520218, -54.49830448709099784 ) ) ;
#9661 = CARTESIAN_POINT ( 'NONE',  ( 49.10028735341099804, 22.39587775051610308, -54.20564384830549898 ) ) ;
#9662 = CARTESIAN_POINT ( 'NONE',  ( 59.33862398020649920, -2.694272193572899710, -15.68334875206189949 ) ) ;
#9663 = CARTESIAN_POINT ( 'NONE',  ( 51.38507923684370127, -50.52849113110060131, -76.23533798706770881 ) ) ;
#9664 = CARTESIAN_POINT ( 'NONE',  ( 22.27218754053139804, -53.83794553065759914, -34.69483829921989582 ) ) ;
#9665 = ORIENTED_EDGE ( 'NONE', *, *, #9685, .T. ) ;
#9666 = DIRECTION ( 'NONE',  ( 0.000000000000000000, 0.000000000000000000, 1.000000000000000000 ) ) ;
#9667 = CARTESIAN_POINT ( 'NONE',  ( 70.03247032090601465, 18.72622661238169783, -73.39853292320987066 ) ) ;
#9668 = EDGE_LOOP ( 'NONE', ( #46686, #7741, #26856, #32274 ) ) ;
#9669 = DIRECTION ( 'NONE',  ( 0.000000000000000000, 1.000000000000000000, 0.000000000000000000 ) ) ;
#9670 = DIRECTION ( 'NONE',  ( 0.000000000000000000, 0.000000000000000000, 1.000000000000000000 ) ) ;
#9671 = CONICAL_SURFACE ( 'NONE', #38967, 12.92820323027549989, 0.7481802937784480800 ) ;
#9672 = CARTESIAN_POINT ( 'NONE',  ( 23.39608499194349989, -12.64163689252930034, -37.88875081766039443 ) ) ;
#9673 = VECTOR ( 'NONE', #266, 1000.000000000000000 ) ;
#9674 = CARTESIAN_POINT ( 'NONE',  ( 13.81676756077919954, -51.22923098943019937, -22.59431933179259744 ) ) ;
#9675 = CARTESIAN_POINT ( 'NONE',  ( 55.47166349443130429, 19.51716785246549790, -75.55743771978688983 ) ) ;
#9676 = CARTESIAN_POINT ( 'NONE',  ( 47.62441105329040170, -54.51319350303420208, -74.50474471063260751 ) ) ;
#9677 = EDGE_LOOP ( 'NONE', ( #50660, #4391, #47407, #37236, #2350, #5404, #31482, #6795, #17655, #10276, #25627, #18586 ) ) ;
#9678 = CARTESIAN_POINT ( 'NONE',  ( 56.40317685213560139, 14.15597851795049955, -17.20359917593829735 ) ) ;
#9679 = DIRECTION ( 'NONE',  ( 0.000000000000000000, 0.000000000000000000, -1.000000000000000000 ) ) ;
#9680 = CARTESIAN_POINT ( 'NONE',  ( 57.36123083241410114, -50.13537925600150658, -52.61896061011599812 ) ) ;
#9681 = CARTESIAN_POINT ( 'NONE',  ( 52.62724176572390178, -49.81047453036210015, -48.67212384193049957 ) ) ;
#9682 = CARTESIAN_POINT ( 'NONE',  ( 13.85919928309939841, -8.940252629490180070, -36.24264715586419783 ) ) ;
#9683 = DIRECTION ( 'NONE',  ( 0.000000000000000000, 0.000000000000000000, -1.000000000000000000 ) ) ;
#9685 = EDGE_CURVE ( 'NONE', #43315, #5274, #17681, .T. ) ;
#9684 = CARTESIAN_POINT ( 'NONE',  ( 46.56240039978320056, 22.04143744298989915, -76.11243514202939764 ) ) ;
#9686 = MECHANICAL_DESIGN_GEOMETRIC_PRESENTATION_REPRESENTATION (  '', ( #4659 ), #7227 ) ;
#9687 = CARTESIAN_POINT ( 'NONE',  ( 65.00498282733049393, 1.269319268680890067, -60.73450645366879996 ) ) ;
#9688 = CARTESIAN_POINT ( 'NONE',  ( 75.15439417744582329, -29.05685264498805864, -11.81924130454197552 ) ) ;
#9689 = CARTESIAN_POINT ( 'NONE',  ( 9.807866499535744964, -10.75438988217695879, -57.00066478260036007 ) ) ;
#9690 = DIRECTION ( 'NONE',  ( 0.000000000000000000, -1.000000000000000000, 0.000000000000000000 ) ) ;
#9691 = CARTESIAN_POINT ( 'NONE',  ( 17.84637960111742672, -49.61616104255114834, -83.17357193461836573 ) ) ;
#9692 = AXIS2_PLACEMENT_3D ( 'NONE', #38061, #50888, #11061 ) ;
#9693 = CARTESIAN_POINT ( 'NONE',  ( 20.13393739769620083, -2.337132753317949785, -84.65000000000000568 ) ) ;
#9694 = CARTESIAN_POINT ( 'NONE',  ( 60.26929283095191892, -45.78778679473056457, -47.49574889169480940 ) ) ;
#9696 = CARTESIAN_POINT ( 'NONE',  ( 47.16590163426349847, -39.34201989322590975, -54.77441423021601707 ) ) ;
#9695 = DIRECTION ( 'NONE',  ( 1.000000000000000000, 0.000000000000000000, 0.000000000000000000 ) ) ;
#9697 = CARTESIAN_POINT ( 'NONE',  ( 61.29115875527060098, 13.99537663710240132, -46.49544470360039838 ) ) ;
#9698 = CARTESIAN_POINT ( 'NONE',  ( -26.88697088543599989, 10.64579088486830116, -56.26659592162459944 ) ) ;
#9699 = ORIENTED_EDGE ( 'NONE', *, *, #35323, .T. ) ;
#9700 = CARTESIAN_POINT ( 'NONE',  ( 52.94386163188770666, -49.60344564807929402, -48.82486940075439463 ) ) ;
#9701 = ORIENTED_EDGE ( 'NONE', *, *, #43755, .T. ) ;
#9702 = CARTESIAN_POINT ( 'NONE',  ( 58.77552830958769903, -45.11615816423340419, -25.67179826716159852 ) ) ;
#9703 = VECTOR ( 'NONE', #26050, 1000.000000000000114 ) ;
#9704 = CARTESIAN_POINT ( 'NONE',  ( 24.04460285965960864, -15.61618860597671876, -65.79233133698019742 ) ) ;
#9705 = CARTESIAN_POINT ( 'NONE',  ( 13.57018851586839858, 19.78829187941649792, -21.88591218289379725 ) ) ;
#9706 = CARTESIAN_POINT ( 'NONE',  ( 56.49550580218529916, 14.24991461377820023, -25.70480935931119859 ) ) ;
#9707 = CARTESIAN_POINT ( 'NONE',  ( 13.58977759548189823, -9.038209802311760299, -47.83534835059659684 ) ) ;
#9708 = CARTESIAN_POINT ( 'NONE',  ( 50.95182855010829570, 19.71852720125919944, -76.14999999999999147 ) ) ;
#9709 = CARTESIAN_POINT ( 'NONE',  ( 52.86125337422269865, 18.42614690627490148, -48.87400159313619952 ) ) ;
#9710 = CARTESIAN_POINT ( 'NONE',  ( 64.85866674173239232, 1.325841671674429900, -60.89969828258869455 ) ) ;
#9711 = CARTESIAN_POINT ( 'NONE',  ( 60.66054148094019638, -45.55815270253820159, -47.10566629212190293 ) ) ;
#9712 = CARTESIAN_POINT ( 'NONE',  ( 46.37947015900544301, 21.71088129867535699, -76.14999999999999147 ) ) ;
#9713 = ORIENTED_EDGE ( 'NONE', *, *, #41817, .F. ) ;
#9714 = CARTESIAN_POINT ( 'NONE',  ( 18.83398544718350109, -8.672383441297080608, -70.68538827799869750 ) ) ;
#9715 = EDGE_CURVE ( 'NONE', #38484, #15061, #23016, .T. ) ;
#9716 = CARTESIAN_POINT ( 'NONE',  ( 73.11516444234040080, 0.9966178393190270324, -68.98171082814549493 ) ) ;
#9717 = CARTESIAN_POINT ( 'NONE',  ( 47.41728684029249763, -54.64464118299699891, -54.77930846233410023 ) ) ;
#9718 = CARTESIAN_POINT ( 'NONE',  ( -3.204518369755029905, 17.10185219583640048, -4.296538310232840274 ) ) ;
#9719 = CARTESIAN_POINT ( 'NONE',  ( 73.13170780125059878, 0.9259537755896120048, -62.33000265676009377 ) ) ;
#9720 = CARTESIAN_POINT ( 'NONE',  ( 11.14146392936840080, -65.20891899316059437, -17.73105615079460051 ) ) ;
#9721 = CARTESIAN_POINT ( 'NONE',  ( 71.60339545440879760, 0.9065823421260970072, -60.75474143511929981 ) ) ;
#9722 = CARTESIAN_POINT ( 'NONE',  ( 24.04423775914019501, -15.72983825153451853, -75.79689790679616124 ) ) ;
#9723 = CARTESIAN_POINT ( 'NONE',  ( 11.27228755212498434, -9.290002421830825696, -45.08396659437083542 ) ) ;
#9724 = CARTESIAN_POINT ( 'NONE',  ( 24.04493739715903544, -15.62387967814676770, -45.50799847524913133 ) ) ;
#9725 = CARTESIAN_POINT ( 'NONE',  ( 64.99178804968069301, 1.386446979194299933, -70.29126806847389730 ) ) ;
#9726 = EDGE_LOOP ( 'NONE', ( #29683, #31179, #38900, #42346, #49887 ) ) ;
#9727 = FACE_OUTER_BOUND ( 'NONE', #42343, .T. ) ;
#9728 = CARTESIAN_POINT ( 'NONE',  ( 8.222950439209398610, -14.58054600011118396, -46.83399825817551232 ) ) ;
#9729 = ORIENTED_EDGE ( 'NONE', *, *, #1007, .F. ) ;
#9730 = CARTESIAN_POINT ( 'NONE',  ( 30.13393739769619728, -38.61618894467930119, -84.65000000000000568 ) ) ;
#9731 = LINE ( 'NONE', #17845, #36098 ) ;
#9732 = CARTESIAN_POINT ( 'NONE',  ( 22.73193228873973837, -14.04747040378604517, -50.37850237016653665 ) ) ;
#9733 = CARTESIAN_POINT ( 'NONE',  ( 52.12745817633830114, 19.40061496106389782, -76.37383754635089872 ) ) ;
#9734 = VERTEX_POINT ( 'NONE', #1957 ) ;
#9735 = CARTESIAN_POINT ( 'NONE',  ( 14.13393739769599833, 14.38381105532070059, -35.14999999999999858 ) ) ;
#9737 = CARTESIAN_POINT ( 'NONE',  ( 0.3209249304026170480, -15.61618894467929941, -35.14999999999999858 ) ) ;
#9736 = AXIS2_PLACEMENT_3D ( 'NONE', #45919, #45655, #30687 ) ;
#9738 = DIRECTION ( 'NONE',  ( -1.000000000000000000, 0.000000000000000000, 0.000000000000000000 ) ) ;
#9739 = CARTESIAN_POINT ( 'NONE',  ( 12.38999535182930067, -22.96231840264049850, -48.44236253966159467 ) ) ;
#9740 = CIRCLE ( 'NONE', #28985, 1.999999999999998446 ) ;
#9741 = CARTESIAN_POINT ( 'NONE',  ( 22.85153108731185867, -14.77300192338831408, -56.41308520645548441 ) ) ;
#9742 = CARTESIAN_POINT ( 'NONE',  ( 43.59785196581361078, -37.86270477977220850, -72.33041599445031977 ) ) ;
#9743 = ORIENTED_EDGE ( 'NONE', *, *, #47389, .T. ) ;
#9744 =( BOUNDED_CURVE ( )  B_SPLINE_CURVE ( 3, ( #13040, #24786, #21126, #32384 ),
 .UNSPECIFIED., .F., .T. ) 
 B_SPLINE_CURVE_WITH_KNOTS ( ( 4, 4 ),
 ( 4.856961825214290762, 7.709408789144880814 ),
 .UNSPECIFIED. ) 
 CURVE ( )  GEOMETRIC_REPRESENTATION_ITEM ( )  RATIONAL_B_SPLINE_CURVE ( ( 1.000000000000000000, 0.4293798293182609638, 0.4293798293182609638, 1.000000000000000000 ) ) 
 REPRESENTATION_ITEM ( '' )  );
#9745 = B_SPLINE_CURVE_WITH_KNOTS ( 'NONE', 3,
 ( #25956, #25439, #17854, #22026, #34080, #50087, #49588, #45640, #5301, #45122, #30153, #41441, #17092, #1358, #29887, #14182, #33044, #13177, #29125, #9233, #5558, #13677, #45905, #9992, #18359, #22287, #34339, #3429 ),
 .UNSPECIFIED., .F., .F.,
 ( 4, 2, 1, 1, 1, 1, 2, 2, 2, 2, 2, 2, 2, 2, 2, 4 ),
 ( 0.5000036253583125534, 0.5004919030679235714, 0.5009801807775345894, 0.5019567361967566255, 0.5039098470352006975, 0.5078160687120888417, 0.5156285120658652410, 0.5312533987734178176, 0.5625031721885233038, 0.6250027190187341652, 0.6875022658489451377, 0.7500018126791561102, 0.8125013595093670826, 0.8750009063395780551, 0.9375004531697890275, 1.000000000000000000 ),
 .UNSPECIFIED. ) ;
#9746 = CARTESIAN_POINT ( 'NONE',  ( 56.74295248199899788, -46.05519997842870339, -26.24922959646229970 ) ) ;
#9747 = CARTESIAN_POINT ( 'NONE',  ( 21.20762467232530213, -10.16051380365300005, -43.97111461901920393 ) ) ;
#9748 = VECTOR ( 'NONE', #6101, 1000.000000000000000 ) ;
#9749 = CARTESIAN_POINT ( 'NONE',  ( 8.916440530500569395, -14.98798906874889880, -32.14999999999999858 ) ) ;
#9750 = CIRCLE ( 'NONE', #11410, 16.60961179679779676 ) ;
#9751 = ADVANCED_FACE ( 'NONE', ( #49917 ), #18192, .F. ) ;
#9752 = CARTESIAN_POINT ( 'NONE',  ( 13.94115953390780049, 19.96087670211870346, -74.14993703734479880 ) ) ;
#9753 = ADVANCED_FACE ( 'NONE', ( #6152 ), #22108, .T. ) ;
#9754 = CARTESIAN_POINT ( 'NONE',  ( 9.366584228470589579, -15.61631960056659985, -37.84717978380999881 ) ) ;
#9755 = EDGE_CURVE ( 'NONE', #30578, #679, #21335, .T. ) ;
#9756 = CARTESIAN_POINT ( 'NONE',  ( 45.86654133577830095, -45.11728007697210785, -7.634490596206400248 ) ) ;
#9757 = CARTESIAN_POINT ( 'NONE',  ( 82.13853704237929776, 15.88381105532069704, -46.37203261889099792 ) ) ;
#9758 = EDGE_CURVE ( 'NONE', #4073, #46602, #21968, .T. ) ;
#9759 = CARTESIAN_POINT ( 'NONE',  ( 12.95136722755839997, -23.22236852585700007, -58.13380938886719917 ) ) ;
#9760 = ORIENTED_EDGE ( 'NONE', *, *, #29926, .T. ) ;
#9761 = CARTESIAN_POINT ( 'NONE',  ( 52.92251006689210158, -49.49947021432900129, -27.40003960897890067 ) ) ;
#9762 = CIRCLE ( 'NONE', #44929, 15.11955878774480233 ) ;
#9763 = CARTESIAN_POINT ( 'NONE',  ( 14.13974949994079999, -51.04257351792690400, -21.96874462324809940 ) ) ;
#9765 = CARTESIAN_POINT ( 'NONE',  ( 46.81384049422970151, -39.17204965157010577, -34.68207991959079806 ) ) ;
#9764 = CARTESIAN_POINT ( 'NONE',  ( 2.967561434627600025, 25.54483905069779937, -11.19253359192279973 ) ) ;
#9766 = DIRECTION ( 'NONE',  ( 0.000000000000000000, -1.000000000000000000, 0.000000000000000000 ) ) ;
#9767 = CARTESIAN_POINT ( 'NONE',  ( -23.86606260230395904, -35.74824341182122822, -53.92777777777786952 ) ) ;
#9768 = ORIENTED_EDGE ( 'NONE', *, *, #44527, .F. ) ;
#9769 = CARTESIAN_POINT ( 'NONE',  ( -10.43357540151349916, -42.79329260199609308, -6.008434035834979703 ) ) ;
#9770 = CARTESIAN_POINT ( 'NONE',  ( 47.63214245887139953, 23.26321908959739915, -54.67389918656080283 ) ) ;
#9771 = VECTOR ( 'NONE', #4524, 1000.000000000000000 ) ;
#9772 = EDGE_CURVE ( 'NONE', #36840, #39487, #32208, .T. ) ;
#9773 = CARTESIAN_POINT ( 'NONE',  ( 16.13393739769620083, -15.61618894467929941, 7.349999999999999645 ) ) ;
#9774 = CARTESIAN_POINT ( 'NONE',  ( 63.27605356278090198, 1.264489825601020190, -62.40944773533740175 ) ) ;
#9775 = LINE ( 'NONE', #42003, #19795 ) ;
#9776 = CARTESIAN_POINT ( 'NONE',  ( 41.66707738397720107, 13.41595190872300059, -5.278831649207059939 ) ) ;
#9777 = CARTESIAN_POINT ( 'NONE',  ( 51.84382618163579792, 18.03477920213529728, -77.06468978116740232 ) ) ;
#9778 = CARTESIAN_POINT ( 'NONE',  ( 16.13393739769620083, -15.61618894467929941, -11.05000000000000071 ) ) ;
#9779 = DIRECTION ( 'NONE',  ( -0.7071067811865475727, 0.000000000000000000, -0.7071067811865475727 ) ) ;
#9780 = FACE_OUTER_BOUND ( 'NONE', #7743, .T. ) ;
#9781 = CARTESIAN_POINT ( 'NONE',  ( 16.25297294464781572, -22.45082257738738107, -66.94693417945528324 ) ) ;
#9782 = CARTESIAN_POINT ( 'NONE',  ( 52.45962341386800176, 21.25014430318469749, -54.36149425316440187 ) ) ;
#9783 = EDGE_CURVE ( 'NONE', #6972, #31235, #25521, .T. ) ;
#9784 = CARTESIAN_POINT ( 'NONE',  ( 63.80708344237820739, 1.446931645112450093, -69.41713212316639670 ) ) ;
#9785 = DIRECTION ( 'NONE',  ( 0.000000000000000000, -1.000000000000000000, 0.000000000000000000 ) ) ;
#9786 = VERTEX_POINT ( 'NONE', #39663 ) ;
#9787 = DIRECTION ( 'NONE',  ( 0.000000000000000000, 0.000000000000000000, -1.000000000000000000 ) ) ;
#9788 = CARTESIAN_POINT ( 'NONE',  ( 10.97845908955850014, 31.98345705163180241, -44.74187252678620297 ) ) ;
#9789 = CYLINDRICAL_SURFACE ( 'NONE', #17604, 2.999999999999999112 ) ;
#9790 = AXIS2_PLACEMENT_3D ( 'NONE', #19369, #51089, #30889 ) ;
#9791 = CARTESIAN_POINT ( 'NONE',  ( 66.95998268897230332, -32.69201298692910029, -18.94774364808279898 ) ) ;
#9792 = CARTESIAN_POINT ( 'NONE',  ( 16.44143166354569630, -22.66232309404953327, -47.33329750477101783 ) ) ;
#9793 = AXIS2_PLACEMENT_3D ( 'NONE', #9504, #45400, #41453 ) ;
#9794 = EDGE_LOOP ( 'NONE', ( #7229, #15648 ) ) ;
#9795 = ORIENTED_EDGE ( 'NONE', *, *, #31917, .T. ) ;
#9796 = CARTESIAN_POINT ( 'NONE',  ( 11.27237287438952329, -21.94244001871098249, -80.21600237666562805 ) ) ;
#9797 = ORIENTED_EDGE ( 'NONE', *, *, #17749, .T. ) ;
#9798 = CARTESIAN_POINT ( 'NONE',  ( 9.965595104546959959, -63.68164282303038704, -46.24046655278920070 ) ) ;
#9799 = CARTESIAN_POINT ( 'NONE',  ( 57.29432520663860373, -45.62414914554469902, -26.18807222717889971 ) ) ;
#9800 = CARTESIAN_POINT ( 'NONE',  ( 9.366383648607859769, -15.61614502978449970, -45.45282021618989177 ) ) ;
#9801 = CARTESIAN_POINT ( 'NONE',  ( 16.65420337941489848, 19.88381105532299742, -20.15000000000000213 ) ) ;
#9802 = CARTESIAN_POINT ( 'NONE',  ( 6.784299814571713050, 1.742308277892916646, -84.65000000000000568 ) ) ;
#9803 = VERTEX_POINT ( 'NONE', #10858 ) ;
#9804 = EDGE_CURVE ( 'NONE', #1782, #21433, #3769, .T. ) ;
#9805 = CARTESIAN_POINT ( 'NONE',  ( 45.44635879492527408, 6.861525894367711764, -63.08783649271359906 ) ) ;
#9806 = ORIENTED_EDGE ( 'NONE', *, *, #32990, .T. ) ;
#9807 = CARTESIAN_POINT ( 'NONE',  ( 54.71777093172589446, -45.61739902857990359, -15.43676083049879999 ) ) ;
#9808 = VECTOR ( 'NONE', #27962, 1000.000000000000000 ) ;
#9809 = LINE ( 'NONE', #25249, #23780 ) ;
#9810 = CARTESIAN_POINT ( 'NONE',  ( 16.65427257814469897, 19.88381105411679783, -20.14977964541809996 ) ) ;
#9811 = CARTESIAN_POINT ( 'NONE',  ( 22.90074241486109585, -15.67170043082192343, -50.45542962239370866 ) ) ;
#9812 = VERTEX_POINT ( 'NONE', #51463 ) ;
#9813 = CARTESIAN_POINT ( 'NONE',  ( 16.13393739769620083, -15.61618894467929941, -6.189999999999999503 ) ) ;
#9814 = CARTESIAN_POINT ( 'NONE',  ( 46.77994874552049254, -53.89178638932320098, -75.86501933388160523 ) ) ;
#9815 = CARTESIAN_POINT ( 'NONE',  ( 41.23501606932020280, 13.88381301678689894, -6.199056208102949661 ) ) ;
#9816 = CARTESIAN_POINT ( 'NONE',  ( 51.00410689780089513, 21.58760788935499875, -53.76372497442359588 ) ) ;
#9817 = ADVANCED_FACE ( 'NONE', ( #34682 ), #43090, .T. ) ;
#9818 = EDGE_CURVE ( 'NONE', #11637, #10547, #49840, .T. ) ;
#9819 = PRODUCT_DEFINITION_SHAPE ( 'NONE', 'NONE',  #38253 ) ;
#9820 = CARTESIAN_POINT ( 'NONE',  ( 51.15928693312330466, 19.73279912208279896, -76.15045075665069874 ) ) ;
#9821 = CARTESIAN_POINT ( 'NONE',  ( 57.39038370734829897, 14.07100446516539982, -25.91661231449569769 ) ) ;
#9822 = ADVANCED_FACE ( 'NONE', ( #15563 ), #41875, .T. ) ;
#9823 = CARTESIAN_POINT ( 'NONE',  ( 19.44595729680459684, -8.501607272430129925, -76.92618994148479317 ) ) ;
#9824 = ORIENTED_EDGE ( 'NONE', *, *, #45017, .F. ) ;
#9825 = DIRECTION ( 'NONE',  ( 0.8204012560548797905, 0.5717882292104092823, 0.000000000000000000 ) ) ;
#9826 = CARTESIAN_POINT ( 'NONE',  ( -11.30871548113529990, -41.86345860935140450, -5.946230549336929627 ) ) ;
#9827 = CARTESIAN_POINT ( 'NONE',  ( 16.81199894099719927, -16.95676073769629610, -35.14999999999999858 ) ) ;
#9828 = CARTESIAN_POINT ( 'NONE',  ( 72.68207769252681771, 1.402020837641670070, -69.05263811644309158 ) ) ;
#9829 = CARTESIAN_POINT ( 'NONE',  ( 16.13393739769620083, -15.61618894467929941, -40.14999999999999858 ) ) ;
#9830 = CARTESIAN_POINT ( 'NONE',  ( 8.222919126920675836, -14.58077523142493526, -42.54932860275096118 ) ) ;
#9831 = CARTESIAN_POINT ( 'NONE',  ( 65.23632417210519918, 1.383928098097870096, -70.33743540642140601 ) ) ;
#9832 = CARTESIAN_POINT ( 'NONE',  ( 10.04852440032967209, -53.95817006707463293, -34.76477869314685876 ) ) ;
#9833 = CARTESIAN_POINT ( 'NONE',  ( 43.27084646103560317, -43.87227363443550132, -5.051381114840269859 ) ) ;
#9834 = LINE ( 'NONE', #38131, #18364 ) ;
#9836 = EDGE_CURVE ( 'NONE', #1162, #28912, #44114, .T. ) ;
#9835 = CARTESIAN_POINT ( 'NONE',  ( 38.67452568954060155, 4.883811055320659733, -81.65000000000000568 ) ) ;
#9837 = VERTEX_POINT ( 'NONE', #6996 ) ;
#9838 = CARTESIAN_POINT ( 'NONE',  ( 23.48471434990800333, -16.82976734642059924, -59.11942434271038849 ) ) ;
#9839 = CARTESIAN_POINT ( 'NONE',  ( 64.41203867946529726, 1.158194067776729952, -60.98980919032499770 ) ) ;
#9840 = ORIENTED_EDGE ( 'NONE', *, *, #50128, .F. ) ;
#9841 = CARTESIAN_POINT ( 'NONE',  ( 51.13393739769620083, 19.38381105532069881, 11.97999999999999865 ) ) ;
#9842 = CARTESIAN_POINT ( 'NONE',  ( 61.23205860893720143, -45.59110651710669515, -47.66442491677190674 ) ) ;
#9843 = CARTESIAN_POINT ( 'NONE',  ( 9.366701239804031687, -16.70366627111308944, -75.79601146438885451 ) ) ;
#9844 = DIRECTION ( 'NONE',  ( -3.191891195582396227E-12, 1.000000000000000000, 0.000000000000000000 ) ) ;
#9846 = CARTESIAN_POINT ( 'NONE',  ( 16.13393739769620083, -15.61618894467929941, -28.45282021618999835 ) ) ;
#9845 = CARTESIAN_POINT ( 'NONE',  ( 44.31510748265038302, 8.747601604831885425, -65.13307718246910838 ) ) ;
#9847 = CARTESIAN_POINT ( 'NONE',  ( 40.70150336865399510, -45.32906768026739996, -5.681035058216649780 ) ) ;
#9848 = ORIENTED_EDGE ( 'NONE', *, *, #23796, .F. ) ;
#9849 = ORIENTED_EDGE ( 'NONE', *, *, #29038, .F. ) ;
#9850 = ORIENTED_EDGE ( 'NONE', *, *, #1473, .T. ) ;
#9851 = CARTESIAN_POINT ( 'NONE',  ( -22.76297446149728998, -18.32468108091643089, -54.70357014338004831 ) ) ;
#9852 = CARTESIAN_POINT ( 'NONE',  ( 17.63393739769639978, 10.88381105532070059, -34.64999999999999858 ) ) ;
#9853 = CARTESIAN_POINT ( 'NONE',  ( 56.39371274214659735, -50.58610758163149512, -52.96141008474040035 ) ) ;
#9854 = EDGE_CURVE ( 'NONE', #25744, #9892, #27214, .T. ) ;
#9855 = VERTEX_POINT ( 'NONE', #22693 ) ;
#9856 = VERTEX_POINT ( 'NONE', #30035 ) ;
#9857 = DIRECTION ( 'NONE',  ( 1.000000000000000000, 0.000000000000000000, 0.000000000000000000 ) ) ;
#9858 = ADVANCED_FACE ( 'NONE', ( #17744 ), #6216, .T. ) ;
#9860 = FACE_OUTER_BOUND ( 'NONE', #21060, .T. ) ;
#9859 = VECTOR ( 'NONE', #4345, 1000.000000000000000 ) ;
#9861 = DIRECTION ( 'NONE',  ( 0.04251717301921900671, 0.000000000000000000, 0.9990957361526741076 ) ) ;
#9862 = ORIENTED_EDGE ( 'NONE', *, *, #39208, .T. ) ;
#9863 = CARTESIAN_POINT ( 'NONE',  ( 11.67619942398489918, -64.89165360645620240, -45.08494251881790404 ) ) ;
#9864 = CARTESIAN_POINT ( 'NONE',  ( 52.84397959254010146, -50.50345798787359541, -76.72969847629740059 ) ) ;
#9865 = CARTESIAN_POINT ( 'NONE',  ( 60.51067680394970694, 14.40429311637669940, -47.16814695452289641 ) ) ;
#9866 = CARTESIAN_POINT ( 'NONE',  ( 15.78203914809910025, -7.776360170156919160, -77.49821634947008420 ) ) ;
#9867 = CARTESIAN_POINT ( 'NONE',  ( 68.13393739769620083, -50.61618894467930119, -69.74999999999998579 ) ) ;
#9868 = CARTESIAN_POINT ( 'NONE',  ( 44.89324673519139708, 14.02190024633609866, -7.755622268330540692 ) ) ;
#9869 = CARTESIAN_POINT ( 'NONE',  ( 42.94731284509200009, -42.57349969409850132, -3.548345704167709780 ) ) ;
#9870 = DIRECTION ( 'NONE',  ( 1.000000000000000000, 0.000000000000000000, 0.000000000000000000 ) ) ;
#9871 = CARTESIAN_POINT ( 'NONE',  ( 65.36113773965780638, 1.378962859947149955, -18.37587875859610165 ) ) ;
#9872 = EDGE_CURVE ( 'NONE', #41037, #4059, #13816, .T. ) ;
#9873 = CARTESIAN_POINT ( 'NONE',  ( 64.60878109323620322, 1.379695757017360025, -70.20843506130859168 ) ) ;
#9874 = CARTESIAN_POINT ( 'NONE',  ( 46.56831964672900170, 8.771274579019829432, -54.63028235546250500 ) ) ;
#9875 = CARTESIAN_POINT ( 'NONE',  ( 68.36214382535489165, -0.4430383702800620438, -18.19623533484779898 ) ) ;
#9876 = EDGE_CURVE ( 'NONE', #5705, #27765, #40617, .T. ) ;
#9877 = VERTEX_POINT ( 'NONE', #29776 ) ;
#9878 = CARTESIAN_POINT ( 'NONE',  ( 15.05440318628160057, -53.11618894467930119, -76.14999999999999147 ) ) ;
#9879 = CARTESIAN_POINT ( 'NONE',  ( 47.18324198357289845, -54.80726809202429450, -54.61058319554170026 ) ) ;
#9880 = CARTESIAN_POINT ( 'NONE',  ( 46.21668119980922285, -40.10555969717534452, -55.90708416986943519 ) ) ;
#9881 = CARTESIAN_POINT ( 'NONE',  ( 10.61754762155600140, 33.59328422689429772, -18.17417937929459981 ) ) ;
#9882 = CIRCLE ( 'NONE', #8240, 0.4999999999562930175 ) ;
#9883 = CARTESIAN_POINT ( 'NONE',  ( 47.01289497786039817, -54.42182676496869931, -75.36291177546809195 ) ) ;
#9884 = CARTESIAN_POINT ( 'NONE',  ( 63.49151163952229382, 1.387131204727280132, -68.68796153961081075 ) ) ;
#9885 = CARTESIAN_POINT ( 'NONE',  ( 47.81335647231750130, -54.39749252970050009, -54.71582838609450050 ) ) ;
#9886 = PLANE ( 'NONE',  #48198 ) ;
#9887 = CARTESIAN_POINT ( 'NONE',  ( 56.35668072086730263, 19.46447099969040195, -53.18237273277000554 ) ) ;
#9888 = CARTESIAN_POINT ( 'NONE',  ( 8.428815148825032466, -17.68678772635738383, -46.70901315390379693 ) ) ;
#9889 = CARTESIAN_POINT ( 'NONE',  ( 47.93812309775100289, 23.11656297732089627, -54.78467533403669876 ) ) ;
#9890 = ORIENTED_EDGE ( 'NONE', *, *, #4974, .F. ) ;
#9891 = CARTESIAN_POINT ( 'NONE',  ( 20.92027185089429864, -10.43607681494890116, -74.58460979065598906 ) ) ;
#9892 = VERTEX_POINT ( 'NONE', #22431 ) ;
#9893 = DIRECTION ( 'NONE',  ( 0.000000000000000000, 0.000000000000000000, 1.000000000000000000 ) ) ;
#9894 = CARTESIAN_POINT ( 'NONE',  ( 83.07525789736615707, 14.27201180209920217, -47.60488146747717053 ) ) ;
#9895 = CARTESIAN_POINT ( 'NONE',  ( 10.22108565793575430, -19.02428243526157559, -43.28615345358821287 ) ) ;
#9897 = CARTESIAN_POINT ( 'NONE',  ( 65.03603135424580728, -29.76883965895079953, -19.52361391316370032 ) ) ;
#9896 = CARTESIAN_POINT ( 'NONE',  ( 84.32109122769391263, 12.72058013282260092, -47.41657241682830204 ) ) ;
#9898 = CARTESIAN_POINT ( 'NONE',  ( 21.87344586468049812, -11.51733529334000039, -78.25541787902638191 ) ) ;
#9899 = CARTESIAN_POINT ( 'NONE',  ( 68.13393739769618662, -25.01418894467940035, -65.65000000000000568 ) ) ;
#9900 = CARTESIAN_POINT ( 'NONE',  ( 0.6045892726184849408, -22.44175889786657763, -34.79644291222908237 ) ) ;
#9901 = CARTESIAN_POINT ( 'NONE',  ( 22.81411388107130733, -16.71917211157028760, -40.50489512194194930 ) ) ;
#9902 = DIRECTION ( 'NONE',  ( 1.000000000000000000, 0.000000000000000000, 0.000000000000000000 ) ) ;
#9903 = ORIENTED_EDGE ( 'NONE', *, *, #7102, .T. ) ;
#9904 = B_SPLINE_CURVE_WITH_KNOTS ( 'NONE', 3,
 ( #5015, #3982, #16029, #8168, #20452, #8427, #24112, #40132, #4226, #36442, #16534, #32486, #48514, #12618, #9718, #41167 ),
 .UNSPECIFIED., .F., .F.,
 ( 4, 2, 2, 2, 2, 2, 2, 4 ),
 ( -11.88254149278500016, -9.803096731538550657, -7.426588432971120035, -5.941270746366480004, -5.198611903064159989, -4.010357753780449563, -2.109151114926509862, 5.208278253121534362E-11 ),
 .UNSPECIFIED. ) ;
#9905 = ORIENTED_EDGE ( 'NONE', *, *, #15093, .T. ) ;
#9906 = DIRECTION ( 'NONE',  ( 0.000000000000000000, 0.000000000000000000, -1.000000000000000000 ) ) ;
#9907 = CARTESIAN_POINT ( 'NONE',  ( 11.54602910941480154, 33.64475169218199824, -45.95025651893509888 ) ) ;
#9908 = CARTESIAN_POINT ( 'NONE',  ( 15.54185229010079716, -7.651191642471210308, -38.98438864213744637 ) ) ;
#9909 = DIRECTION ( 'NONE',  ( 0.000000000000000000, 0.000000000000000000, -1.000000000000000000 ) ) ;
#9910 = ORIENTED_EDGE ( 'NONE', *, *, #26077, .T. ) ;
#9911 = CARTESIAN_POINT ( 'NONE',  ( -22.58910033241870252, -11.83175606744140040, -54.40873678327959340 ) ) ;
#9912 = DIRECTION ( 'NONE',  ( -1.000000000000000000, 0.000000000000000000, 0.000000000000000000 ) ) ;
#9913 = EDGE_CURVE ( 'NONE', #14240, #18792, #14787, .T. ) ;
#9914 = CARTESIAN_POINT ( 'NONE',  ( 53.26712897989530404, 18.16301094328009924, -48.90765490644029967 ) ) ;
#9915 = CARTESIAN_POINT ( 'NONE',  ( 64.47274453872979905, -1.570850956254630004, -16.41268983226810008 ) ) ;
#9916 = CARTESIAN_POINT ( 'NONE',  ( 51.67725368488709847, -50.05092317807059743, -76.49491248771630580 ) ) ;
#9917 = ADVANCED_FACE ( 'NONE', ( #4078 ), #43664, .F. ) ;
#9918 = CARTESIAN_POINT ( 'NONE',  ( 56.87642604909630251, -50.51355556899029864, -53.02367019345480514 ) ) ;
#9919 = ORIENTED_EDGE ( 'NONE', *, *, #48631, .T. ) ;
#9920 = DIRECTION ( 'NONE',  ( 0.000000000000000000, 0.000000000000000000, -1.000000000000000000 ) ) ;
#9921 = CARTESIAN_POINT ( 'NONE',  ( 72.83393739769620367, 1.383811055320669947, -62.79342862858290886 ) ) ;
#9922 = ORIENTED_EDGE ( 'NONE', *, *, #35627, .T. ) ;
#9923 = CARTESIAN_POINT ( 'NONE',  ( 23.83903865329137517, -13.54551831327839650, -57.42433424745438941 ) ) ;
#9924 = AXIS2_PLACEMENT_3D ( 'NONE', #32843, #36275, #48089 ) ;
#9925 = CARTESIAN_POINT ( 'NONE',  ( 57.50723796702470025, -47.11618894467930119, -17.93019253464870033 ) ) ;
#9926 = VECTOR ( 'NONE', #36138, 1000.000000000000000 ) ;
#9927 = CARTESIAN_POINT ( 'NONE',  ( 21.09470678374900032, -9.535274976369610300, -37.73031295553310116 ) ) ;
#9928 = CARTESIAN_POINT ( 'NONE',  ( 13.32539517089530001, -51.13125742665909712, -21.90065997771110418 ) ) ;
#9929 = CARTESIAN_POINT ( 'NONE',  ( 56.72660940836590271, 19.43947700957160052, -74.52937665603549533 ) ) ;
#9930 = CARTESIAN_POINT ( 'NONE',  ( 47.20372080753160304, -53.97904105312669287, -75.66073271794819277 ) ) ;
#9931 = ORIENTED_EDGE ( 'NONE', *, *, #40499, .T. ) ;
#9932 = CARTESIAN_POINT ( 'NONE',  ( 56.03489956542599515, 14.32464527057259929, -16.86885345059799945 ) ) ;
#9933 = CARTESIAN_POINT ( 'NONE',  ( 47.75363926615540322, 23.23893620800870252, -54.94115012086979988 ) ) ;
#9934 = CARTESIAN_POINT ( 'NONE',  ( 57.03107162669589769, -50.22865659835970575, -52.68131389647400198 ) ) ;
#9935 = VECTOR ( 'NONE', #39593, 1000.000000000000000 ) ;
#9936 = CARTESIAN_POINT ( 'NONE',  ( 13.88552899772860094, -22.30103889375499904, -35.45045784522799437 ) ) ;
#9937 = CARTESIAN_POINT ( 'NONE',  ( 9.942021269482310686, -12.23939551960640060, -44.00610240009889651 ) ) ;
#9938 = EDGE_CURVE ( 'NONE', #27637, #45497, #11346, .T. ) ;
#9939 = EDGE_LOOP ( 'NONE', ( #48938, #49011, #682, #22348 ) ) ;
#9940 = CARTESIAN_POINT ( 'NONE',  ( 47.50503096094819711, 23.24249282884580126, -74.80880243014959774 ) ) ;
#9941 = CARTESIAN_POINT ( 'NONE',  ( 65.11408845474450402, 1.278021359705819870, -60.68135466038360448 ) ) ;
#9942 = CARTESIAN_POINT ( 'NONE',  ( 75.15838486831707144, -29.30899119363491678, -11.83853932060654657 ) ) ;
#9943 = CARTESIAN_POINT ( 'NONE',  ( 104.6856170952509757, -28.80002732851810521, -65.65000000000000568 ) ) ;
#9944 = DIRECTION ( 'NONE',  ( 1.000000000000000000, 0.000000000000000000, 0.000000000000000000 ) ) ;
#9945 = LINE ( 'NONE', #26683, #23078 ) ;
#9946 = CARTESIAN_POINT ( 'NONE',  ( -21.13107420191839836, -3.984212544564229574, -53.16029643437919816 ) ) ;
#9948 = CARTESIAN_POINT ( 'NONE',  ( 45.20206541413084267, -40.17273866886250744, -60.31333638933742947 ) ) ;
#9947 = FACE_OUTER_BOUND ( 'NONE', #32377, .T. ) ;
#9949 = CARTESIAN_POINT ( 'NONE',  ( 61.24542922434319792, 14.01933573698959989, -46.57808965542819379 ) ) ;
#9950 = CARTESIAN_POINT ( 'NONE',  ( 18.20461310658355458, -7.911087764067699091, -69.09100364078624068 ) ) ;
#9951 = CARTESIAN_POINT ( 'NONE',  ( -18.43754721997740020, 21.20956224061950124, -54.46408928706180319 ) ) ;
#9952 = ORIENTED_EDGE ( 'NONE', *, *, #13311, .F. ) ;
#9953 = CARTESIAN_POINT ( 'NONE',  ( 52.79145514622300084, -49.68335952808720180, -48.63147282162839957 ) ) ;
#9954 = ORIENTED_EDGE ( 'NONE', *, *, #3116, .T. ) ;
#9955 = AXIS2_PLACEMENT_3D ( 'NONE', #48346, #4838, #16109 ) ;
#9956 = CARTESIAN_POINT ( 'NONE',  ( 43.35873532115121520, 8.736805108720993474, -69.47954381186947614 ) ) ;
#9957 = CARTESIAN_POINT ( 'NONE',  ( 16.13393739769620083, -29.89477637979525682, -34.64999999999999858 ) ) ;
#9958 = CARTESIAN_POINT ( 'NONE',  ( 13.86896207300669914, 19.56934397777870061, -21.50766788832570242 ) ) ;
#9959 = FACE_OUTER_BOUND ( 'NONE', #40989, .T. ) ;
#9960 = AXIS2_PLACEMENT_3D ( 'NONE', #21863, #38914, #18975 ) ;
#9961 = CARTESIAN_POINT ( 'NONE',  ( 10.75784644233539922, -11.05108163637709850, -47.67691048846939594 ) ) ;
#9963 = CARTESIAN_POINT ( 'NONE',  ( 50.03007021624649298, 17.53271186393800107, -76.14999999999999147 ) ) ;
#9962 = VECTOR ( 'NONE', #25613, 999.9999999999998863 ) ;
#9964 = CARTESIAN_POINT ( 'NONE',  ( 52.97367359308089618, 18.36436387382549995, -48.91755406990360200 ) ) ;
#9965 = CARTESIAN_POINT ( 'NONE',  ( 64.95360084570980064, 1.395196698723390138, -61.05633982442969909 ) ) ;
#9966 = CARTESIAN_POINT ( 'NONE',  ( 60.58881092996779927, -45.59573434794560143, -47.13710661926510426 ) ) ;
#9967 = FACE_OUTER_BOUND ( 'NONE', #31922, .T. ) ;
#9968 = ORIENTED_EDGE ( 'NONE', *, *, #18404, .T. ) ;
#9969 = CARTESIAN_POINT ( 'NONE',  ( 10.14005877276480128, -11.19124675659010038, -72.26976689927128916 ) ) ;
#9970 = CARTESIAN_POINT ( 'NONE',  ( 72.96845534527879806, 1.188860127980290171, -69.06196878611640955 ) ) ;
#9971 = FACE_OUTER_BOUND ( 'NONE', #1381, .T. ) ;
#9972 = CARTESIAN_POINT ( 'NONE',  ( 73.11081010690780602, 1.190292248953970011, -62.47835652209879953 ) ) ;
#9973 = CARTESIAN_POINT ( 'NONE',  ( 11.89433743671910015, -65.43612263100310145, -18.12680249715119984 ) ) ;
#9974 = CARTESIAN_POINT ( 'NONE',  ( 52.85589143289909941, 18.41484964472969921, -48.63420543068689739 ) ) ;
#9975 = DIRECTION ( 'NONE',  ( 0.000000000000000000, -1.000000000000000000, 0.000000000000000000 ) ) ;
#9976 = CARTESIAN_POINT ( 'NONE',  ( 22.46010812062750972, -10.75451853965353877, -45.58397716830953783 ) ) ;
#9977 = CARTESIAN_POINT ( 'NONE',  ( 17.90525119180973235, -9.025334454543937568, -58.03615338440669547 ) ) ;
#9978 = CARTESIAN_POINT ( 'NONE',  ( 65.05887334876689465, 1.388715606738730068, -70.28003120372629553 ) ) ;
#9979 = ORIENTED_EDGE ( 'NONE', *, *, #40507, .F. ) ;
#9980 = CARTESIAN_POINT ( 'NONE',  ( 13.97463716302289960, -51.18681913639190384, -22.92153292251790120 ) ) ;
#9981 = ADVANCED_FACE ( 'NONE', ( #7767 ), #31579, .F. ) ;
#9982 = CARTESIAN_POINT ( 'NONE',  ( 18.20466502140901355, -7.911102438067278086, -47.37566600737606848 ) ) ;
#9983 = VERTEX_POINT ( 'NONE', #51528 ) ;
#9984 = DIRECTION ( 'NONE',  ( 0.000000000000000000, 0.000000000000000000, 1.000000000000000000 ) ) ;
#9985 = CARTESIAN_POINT ( 'NONE',  ( 57.24929578232330130, -50.61618894764249887, -53.91492796143979405 ) ) ;
#9986 = DIRECTION ( 'NONE',  ( 0.000000000000000000, 0.000000000000000000, 1.000000000000000000 ) ) ;
#9987 = CARTESIAN_POINT ( 'NONE',  ( 52.01032270792030232, 18.80640155979590133, -76.70782231553221209 ) ) ;
#9988 = VERTEX_POINT ( 'NONE', #36041 ) ;
#9989 = DIRECTION ( 'NONE',  ( 0.000000000000000000, -1.000000000000000000, 0.000000000000000000 ) ) ;
#9990 = PLANE ( 'NONE',  #18365 ) ;
#9991 = CARTESIAN_POINT ( 'NONE',  ( 22.87884895980263167, -15.05859401559651012, -72.42657743928000968 ) ) ;
#9992 = CARTESIAN_POINT ( 'NONE',  ( 9.807692171626330335, -10.75461346308925847, -43.00069361877111618 ) ) ;
#9993 = CARTESIAN_POINT ( 'NONE',  ( 23.07869059287449787, -11.17174037213440130, -51.61111978220640140 ) ) ;
#9994 = FACE_OUTER_BOUND ( 'NONE', #4056, .T. ) ;
#9995 = CARTESIAN_POINT ( 'NONE',  ( 45.40002876707641377, -38.08857925617063245, -63.31948497716211222 ) ) ;
#9996 = ORIENTED_EDGE ( 'NONE', *, *, #6082, .F. ) ;
#9997 = CIRCLE ( 'NONE', #16686, 50.00000000000000000 ) ;
#9998 = CARTESIAN_POINT ( 'NONE',  ( 24.04526736911255469, -15.61618908158827068, -41.79233198438217300 ) ) ;
#9999 = CARTESIAN_POINT ( 'NONE',  ( 23.51503556311359944, -14.60323105926780052, -46.18924468880049972 ) ) ;
#10000 = CIRCLE ( 'NONE', #24998, 40.00000000000000711 ) ;
#10001 = AXIS2_PLACEMENT_3D ( 'NONE', #10886, #34178, #50197 ) ;
#10002 = CARTESIAN_POINT ( 'NONE',  ( 9.759605446949429108, -12.60736725606209951, -32.14999999999999858 ) ) ;
#10003 = AXIS2_PLACEMENT_3D ( 'NONE', #1128, #17123, #21286 ) ;
#10004 = ADVANCED_FACE ( 'NONE', ( #43917 ), #23454, .T. ) ;
#10005 = CIRCLE ( 'NONE', #31753, 38.00000000000000711 ) ;
#10006 = MANIFOLD_SOLID_BREP ( 'Stock-MAS-691-1', #1694 ) ;
#10007 = EDGE_CURVE ( 'NONE', #31006, #38448, #13071, .T. ) ;
#10008 = CARTESIAN_POINT ( 'NONE',  ( 13.39996607787550076, 20.55443427335040241, -74.33583724502659607 ) ) ;
#10009 = CARTESIAN_POINT ( 'NONE',  ( 17.21347160910390173, -53.11618894467930119, -76.14999999999999147 ) ) ;
#10010 = CARTESIAN_POINT ( 'NONE',  ( 41.01790532569319225, -45.00796875502680194, -5.564953489975700052 ) ) ;
#10011 = FACE_OUTER_BOUND ( 'NONE', #41997, .T. ) ;
#10012 = CARTESIAN_POINT ( 'NONE',  ( 19.56137900467879831, -8.117164692171570550, -61.14412876928469842 ) ) ;
#10013 = VERTEX_POINT ( 'NONE', #11958 ) ;
#10014 = CARTESIAN_POINT ( 'NONE',  ( 53.56631670864459949, -48.76508776475549922, -26.51357180580690098 ) ) ;
#10015 = CARTESIAN_POINT ( 'NONE',  ( 54.09921394265249717, -50.74273564420649762, -76.27543683137730568 ) ) ;
#10017 = CARTESIAN_POINT ( 'NONE',  ( 41.94197894960735340, -39.75821015298250671, -76.61187673551151534 ) ) ;
#10016 = CARTESIAN_POINT ( 'NONE',  ( 5.772816392169699995, 28.52799414409169643, -13.89632254613010076 ) ) ;
#10018 = CARTESIAN_POINT ( 'NONE',  ( 9.580591039042646528, -13.34753578335990021, -51.95386955295301590 ) ) ;
#10019 = FACE_OUTER_BOUND ( 'NONE', #2121, .T. ) ;
#10020 = ORIENTED_EDGE ( 'NONE', *, *, #1490, .F. ) ;
#10021 = CARTESIAN_POINT ( 'NONE',  ( -7.453150335675089444, -45.41421344120890069, -5.042286980664930418 ) ) ;
#10022 = CARTESIAN_POINT ( 'NONE',  ( 47.42530979538980063, 23.40590081362070052, -54.75924875434800043 ) ) ;
#10023 = CARTESIAN_POINT ( 'NONE',  ( 23.39917416771469405, -12.38458952302793570, -65.65924184069716318 ) ) ;
#10024 = CARTESIAN_POINT ( 'NONE',  ( 63.16073670604789925, 0.9971903505820729485, -62.30620812933800323 ) ) ;
#10025 = DIRECTION ( 'NONE',  ( 1.000000000000000000, 0.000000000000000000, 0.000000000000000000 ) ) ;
#10026 = CARTESIAN_POINT ( 'NONE',  ( 11.93872965651339868, 33.96647849370500438, -16.76612700402739975 ) ) ;
#10027 = DIRECTION ( 'NONE',  ( 0.000000000000000000, 0.000000000000000000, -1.000000000000000000 ) ) ;
#10028 = DIRECTION ( 'NONE',  ( -1.000000000000000000, 0.000000000000000000, 0.000000000000000000 ) ) ;
#10029 = DIRECTION ( 'NONE',  ( 0.000000000000000000, 0.000000000000000000, -1.000000000000000000 ) ) ;
#10030 = DIRECTION ( 'NONE',  ( 1.000000000000000000, 0.000000000000000000, 0.000000000000000000 ) ) ;
#10031 = CARTESIAN_POINT ( 'NONE',  ( 22.90069627724530221, -15.67791111087114864, -66.45572291796443665 ) ) ;
#10032 = CARTESIAN_POINT ( 'NONE',  ( 54.69511575210409404, 20.01728140309300130, -53.07518616905519337 ) ) ;
#10033 = AXIS2_PLACEMENT_3D ( 'NONE', #26083, #45769, #10383 ) ;
#10034 = CARTESIAN_POINT ( 'NONE',  ( 63.32231416895070453, 0.9254875393589979682, -69.23491771966379815 ) ) ;
#10035 = AXIS2_PLACEMENT_3D ( 'NONE', #25043, #36086, #8836 ) ;
#10036 = CARTESIAN_POINT ( 'NONE',  ( 12.17742765526699955, -65.07456428805339499, -16.46016921340210004 ) ) ;
#10037 = DIRECTION ( 'NONE',  ( 0.2169304578186566079, 0.000000000000000000, -0.9761870601839527373 ) ) ;
#10038 = ORIENTED_EDGE ( 'NONE', *, *, #21315, .F. ) ;
#10039 = CARTESIAN_POINT ( 'NONE',  ( 19.65221995360836260, 22.80254658028719206, -17.14827763294746532 ) ) ;
#10040 = CARTESIAN_POINT ( 'NONE',  ( 10.97923803353369898, 32.08794574957100565, -44.74348915807490101 ) ) ;
#10041 = DIRECTION ( 'NONE',  ( 0.000000000000000000, 0.000000000000000000, 1.000000000000000000 ) ) ;
#10042 = AXIS2_PLACEMENT_3D ( 'NONE', #30202, #34909, #42273 ) ;
#10043 = CARTESIAN_POINT ( 'NONE',  ( 67.20512611029329264, -32.78246747541099637, -19.24941993779820137 ) ) ;
#10044 = CARTESIAN_POINT ( 'NONE',  ( 68.13393739769620083, -48.11618894467930119, -69.74999999999998579 ) ) ;
#10045 = ORIENTED_EDGE ( 'NONE', *, *, #40971, .F. ) ;
#10046 = ORIENTED_EDGE ( 'NONE', *, *, #33363, .F. ) ;
#10047 = CARTESIAN_POINT ( 'NONE',  ( 12.14992511062090763, -22.52877951279442925, -80.17433578879456491 ) ) ;
#10048 = EDGE_CURVE ( 'NONE', #6044, #42020, #26423, .T. ) ;
#10049 = CIRCLE ( 'NONE', #29995, 5.500000000000005329 ) ;
#10050 = CARTESIAN_POINT ( 'NONE',  ( 50.51115622925506443, -0.6041507554334789587, -16.31432736417265161 ) ) ;
#10051 = VERTEX_POINT ( 'NONE', #44171 ) ;
#10052 = CARTESIAN_POINT ( 'NONE',  ( 12.52502643766059975, -65.43529974157461027, -47.02089506534060348 ) ) ;
#10053 = CARTESIAN_POINT ( 'NONE',  ( 57.19937016862409962, -45.64255992831129305, -26.18060017548449991 ) ) ;
#10054 = CARTESIAN_POINT ( 'NONE',  ( 24.04493739344566094, -15.61648521757876473, -77.50768746891878891 ) ) ;
#10055 =( BOUNDED_SURFACE ( )  B_SPLINE_SURFACE ( 2, 3, ( 
 ( #24092, #1054, #40114, #32215, #36421, #36170, #40624, #28040, #48239, #33002, #8405, #20689, #8928, #24873, #49026, #40367, #528, #5256, #37218, #17307, #21472, #29341, #9948, #13635, #46129, #2612, #14398, #49284, #6024, #17809, #37733, #25912, #18583, #29594, #45343, #18068, #13381 ),
 ( #46391, #26176, #26433, #38251, #1831, #30109, #2344, #30366, #34297, #21984, #10478, #33783, #14139, #49792, #41926, #10216, #13884, #17561, #9448, #42451, #6538, #50313, #45598, #37994, #34036, #22501, #5762, #9696, #38513, #25396, #37472, #29844, #25656, #41398, #42187, #21726, #50046 ),
 ( #5516, #1570, #45864, #49543, #22243, #2090, #41659, #33530, #6286, #18318, #15440, #3902, #27472, #19616, #39543, #3392, #11513, #47163, #46908, #3645, #26959, #19359, #11774, #46650, #14656, #35074, #35607, #23783, #50566, #18837, #43473, #31391, #26687, #51080, #35340, #14914, #39284 ) ),
 .UNSPECIFIED., .F., .F., .T. ) 
 B_SPLINE_SURFACE_WITH_KNOTS ( ( 3, 3 ),
 ( 4, 3, 3, 3, 3, 3, 3, 3, 3, 3, 3, 3, 4 ),
 ( -0.3950274212275620145, 0.3825042522605620054 ),
 ( 1.319931596140740071, 1.327157646422050030, 1.335327538272319980, 1.343527953381050022, 1.351756755142390132, 1.360011799518540121, 1.368290935607660019, 1.376592006214460095, 1.384912848423149878, 1.392992571260399881, 1.393221429621980034, 1.393251294075019908, 1.399915485122189995 ),
 .UNSPECIFIED. ) 
 GEOMETRIC_REPRESENTATION_ITEM ( )  RATIONAL_B_SPLINE_SURFACE ( (
 ( 1.002404754520709984, 1.002404754520709984, 1.002404754520709984, 1.002404754520709984, 1.002404754520709984, 1.002404754520709984, 1.002404754520709984, 1.002404754520709984, 1.002404754520709984, 1.002404754520709984, 1.002404754520709984, 1.002404754520709984, 1.002404754520709984, 1.002404754520709984, 1.002404754520709984, 1.002404754520709984, 1.002404754520709984, 1.002404754520709984, 1.002404754520709984, 1.002404754520709984, 1.002404754520709984, 1.002404754520709984, 1.002404754520709984, 1.002404754520709984, 1.002404754520709984, 1.002404754520709984, 1.002404754520709984, 1.002404754520709984, 1.002404754520709984, 1.002404754520709984, 1.002404754520709984, 1.002404754520709984, 1.002404754520709984, 1.002404754520709984, 1.002404754520709984, 1.002404754520709984, 1.002404754520709984),
 ( 0.9265498347468470453, 0.9265498347725940054, 0.9265498347720859673, 0.9265498347720839689, 0.9265498347720839689, 0.9265498347721010663, 0.9265498347721010663, 0.9265498347721010663, 0.9265498347720839689, 0.9265498347720839689, 0.9265498347720839689, 0.9265498347720809713, 0.9265498347720809713, 0.9265498347720809713, 0.9265498347720950711, 0.9265498347720950711, 0.9265498347720950711, 0.9265498347720919625, 0.9265498347720919625, 0.9265498347720919625, 0.9265498347720960703, 0.9265498347720960703, 0.9265498347720960703, 0.9265498347720879657, 0.9265498347720879657, 0.9265498347720879657, 0.9265498347720839689, 0.9265498347720839689, 0.9265498347720839689, 0.9265498347720779737, 0.9265498347720779737, 0.9265498347720779737, 0.9265498347721010663, 0.9265498347721010663, 0.9265498347721010663, 0.9265498347721010663, 0.9265498347721010663),
 ( 1.000000000000000000, 1.000000000000000000, 1.000000000000000000, 1.000000000000000000, 1.000000000000000000, 1.000000000000000000, 1.000000000000000000, 1.000000000000000000, 1.000000000000000000, 1.000000000000000000, 1.000000000000000000, 1.000000000000000000, 1.000000000000000000, 1.000000000000000000, 1.000000000000000000, 1.000000000000000000, 1.000000000000000000, 1.000000000000000000, 1.000000000000000000, 1.000000000000000000, 1.000000000000000000, 1.000000000000000000, 1.000000000000000000, 1.000000000000000000, 1.000000000000000000, 1.000000000000000000, 1.000000000000000000, 1.000000000000000000, 1.000000000000000000, 1.000000000000000000, 1.000000000000000000, 1.000000000000000000, 1.000000000000000000, 1.000000000000000000, 1.000000000000000000, 1.000000000000000000, 1.000000000000000000) ) ) 
 REPRESENTATION_ITEM ( '' )  SURFACE ( )  );
#10056 = B_SPLINE_CURVE_WITH_KNOTS ( 'NONE', 3,
 ( #5693, #41324, #26352, #46050, #49973, #33704, #10137, #49721, #25829 ),
 .UNSPECIFIED., .F., .F.,
 ( 4, 1, 1, 1, 1, 1, 4 ),
 ( 0.4999989276629363544, 0.5443677341273740478, 0.6377213455942496445, 0.7310749570611245751, 0.8244285685279998388, 0.9177821799948754355, 1.000000000000000000 ),
 .UNSPECIFIED. ) ;
#10057 = CARTESIAN_POINT ( 'NONE',  ( 63.57044994947320760, 1.402336724397559964, -62.38137791222469986 ) ) ;
#10058 = ORIENTED_EDGE ( 'NONE', *, *, #51717, .F. ) ;
#10059 = CARTESIAN_POINT ( 'NONE',  ( 46.86172237601420676, 7.004961998947965895, -56.01103048085943215 ) ) ;
#10060 = ORIENTED_EDGE ( 'NONE', *, *, #21267, .T. ) ;
#10061 = CARTESIAN_POINT ( 'NONE',  ( 50.50428634387549920, -45.11618894460880114, -10.93747568071940002 ) ) ;
#10062 = B_SPLINE_CURVE_WITH_KNOTS ( 'NONE', 3,
 ( #51235, #51736, #23924, #31541, #15831, #7974, #47560, #8229 ),
 .UNSPECIFIED., .F., .F.,
 ( 4, 2, 2, 4 ),
 ( 0.04513248637320322471, 0.05146834907058789321, 0.06948743966080110634, 0.08616863070398819713 ),
 .UNSPECIFIED. ) ;
#10063 = CARTESIAN_POINT ( 'NONE',  ( 11.33624769261094123, -21.93600026410923931, -34.49903017084843526 ) ) ;
#10064 = CARTESIAN_POINT ( 'NONE',  ( 16.50880182599389912, 19.88028731614700106, -20.14980157100500335 ) ) ;
#10065 = CARTESIAN_POINT ( 'NONE',  ( 57.55751162049570269, -50.61618894467930119, -53.92796738110899923 ) ) ;
#10066 = EDGE_CURVE ( 'NONE', #3068, #30599, #33116, .T. ) ;
#10067 = CARTESIAN_POINT ( 'NONE',  ( 82.13853704237929776, 14.40950277491920062, -47.72348187592560009 ) ) ;
#10068 = CARTESIAN_POINT ( 'NONE',  ( 46.79115157945750525, -53.88453574729260254, -75.86421395400510903 ) ) ;
#10069 = CARTESIAN_POINT ( 'NONE',  ( 51.93064259432500052, 13.88381105527570014, -9.012790087523750771 ) ) ;
#10070 = CARTESIAN_POINT ( 'NONE',  ( 51.23808412325809769, 13.88381105532070059, -11.16296171910600066 ) ) ;
#10071 = ADVANCED_FACE ( 'NONE', ( #3315 ), #47599, .T. ) ;
#10072 = CARTESIAN_POINT ( 'NONE',  ( 16.13393739769620083, -15.61618894467929941, -8.849999999999999645 ) ) ;
#10073 = CIRCLE ( 'NONE', #2546, 10.27649999999999686 ) ;
#10074 = AXIS2_PLACEMENT_3D ( 'NONE', #3418, #11279, #43257 ) ;
#10075 = AXIS2_PLACEMENT_3D ( 'NONE', #5915, #16939, #32883 ) ;
#10076 = CARTESIAN_POINT ( 'NONE',  ( 52.14830235930340052, 19.90969062716179749, -76.06502807877821226 ) ) ;
#10077 = CARTESIAN_POINT ( 'NONE',  ( 59.63820723955320346, 13.92583137105579993, -26.24900372433129903 ) ) ;
#10078 = CARTESIAN_POINT ( 'NONE',  ( 21.27853140075309923, -21.54239352491439874, -77.55994138999369625 ) ) ;
#10079 = B_SPLINE_SURFACE_WITH_KNOTS ( 'NONE', 3, 3, ( 
 ( #8580, #20866, #32912, #28994, #40795, #4378, #13041, #194, #31879, #24266, #41061, #21128, #44994, #16965, #24522, #5173, #40028, #51819 ),
 ( #48406, #44731, #20346, #48671, #36596, #8060, #28211, #16689, #8309, #15923, #12775, #40286, #4630, #32385, #47898, #27953, #16432, #28730 ),
 ( #44212, #24787, #43956, #16171, #4120, #40540, #36332, #20601, #20096, #32129, #48148, #12249, #442, #12505, #28474, #13548, #13799, #42094 ),
 ( #6197, #22152, #33946, #17979, #37906, #18234, #17217, #9864, #46036, #2259, #38161, #49199, #21381, #49963, #33438, #34199, #21632, #37639 ),
 ( #21895, #25818, #1999, #30279, #50220, #13291, #41313, #49709, #17472, #9362, #41830, #9612, #29755, #45772, #37129, #49456, #33177, #1228 ),
 ( #14310, #17723, #14053, #46299, #29510, #30014, #1742, #10386, #5937, #45515, #25564, #10128, #33694, #26342, #42354, #26086, #6455, #41570 ),
 ( #29248, #25311, #5684, #45257, #5424, #37384, #1487, #30793, #15609, #38418, #34470, #47584, #10648, #39461, #47333, #50730, #43139, #34987 ),
 ( #11679, #22927, #23181, #22672, #50987, #43649, #11425, #38692, #3037, #15352, #2516, #14570, #26871, #10908, #46818, #42878, #3293, #3558 ),
 ( #6975, #35257, #18499, #51257, #50480, #26603, #38947, #42619, #2781, #19271, #31304, #19011, #27645, #15087, #6716, #7231, #27389, #43391 ),
 ( #30535, #23437, #7486, #31054, #47077, #11165, #31563, #19531, #22415, #35519, #46558, #51509, #27133, #39198, #18752, #34728, #14829, #7995 ) ),
 .UNSPECIFIED., .F., .F., .F.,
 ( 4, 1, 1, 1, 1, 1, 1, 4 ),
 ( 4, 2, 2, 2, 2, 2, 2, 2, 4 ),
 ( -7.333206230300000740E-05, 0.1428571428571430157, 0.2857142857142860315, 0.4285714285714289917, 0.5714285714285709528, 0.7142857142857139685, 0.8571428571428569843, 1.000000000000000000 ),
 ( -3.925943193499569883, -2.996312950063570124, -2.453668663398290040, -1.962934930718630122, -1.717568064378800052, -1.324981078235079934, -0.6968419004051140675, -0.06459440906511799974, 7.333206230300000740E-05 ),
 .UNSPECIFIED. ) ;
#10080 = EDGE_LOOP ( 'NONE', ( #19365, #43772, #41429, #45702, #26209 ) ) ;
#10081 = CARTESIAN_POINT ( 'NONE',  ( -21.36606260230379917, -62.11618894467930119, 10.84999999999999964 ) ) ;
#10082 = CARTESIAN_POINT ( 'NONE',  ( -10.65432657557460061, -41.72751226988879836, -4.619077395148970311 ) ) ;
#10083 = DIRECTION ( 'NONE',  ( -1.000000000000000000, 1.127159607568241538E-32, -7.935614746461580696E-16 ) ) ;
#10084 = CARTESIAN_POINT ( 'NONE',  ( 72.94808712738880274, 1.229084191802120030, -69.04069905742069579 ) ) ;
#10085 = CARTESIAN_POINT ( 'NONE',  ( 17.92370450347650035, -51.11618894467930119, -15.67980085856620143 ) ) ;
#10086 = DIRECTION ( 'NONE',  ( 0.000000000000000000, 0.7371541402007432131, -0.6757246285173443834 ) ) ;
#10087 = CARTESIAN_POINT ( 'NONE',  ( 22.46008452425022384, -10.75448613894550043, -43.29930417090383798 ) ) ;
#10088 = CARTESIAN_POINT ( 'NONE',  ( 41.73867463177359838, 12.46261384428329855, -3.496169909523889618 ) ) ;
#10089 = CARTESIAN_POINT ( 'NONE',  ( 10.22100000342511628, -19.02413601058341897, -79.28615302661654596 ) ) ;
#10090 = FACE_OUTER_BOUND ( 'NONE', #50471, .T. ) ;
#10091 = CARTESIAN_POINT ( 'NONE',  ( 31.00696234477200264, -15.61618894467929941, -7.225658350974740074 ) ) ;
#10092 = CARTESIAN_POINT ( 'NONE',  ( 22.90034300907618103, -15.71306550897696930, -62.45738519496880770 ) ) ;
#10093 = MANIFOLD_SOLID_BREP ( 'Stock-MAS-691-1', #14266 ) ;
#10094 = CARTESIAN_POINT ( 'NONE',  ( 18.63644253395800021, -51.46210362308070074, -74.58518005234699899 ) ) ;
#10095 = CARTESIAN_POINT ( 'NONE',  ( -21.36606260230379917, -53.11618894467930119, 17.35000000000000142 ) ) ;
#10096 = B_SPLINE_CURVE_WITH_KNOTS ( 'NONE', 3,
 ( #46672, #31160, #6831, #7089, #6562, #11016, #22267, #47188, #22527, #38802, #51102, #38276, #50334, #2896, #18861, #26987, #42993, #39061, #3414, #14422, #23040, #2366, #35102, #46414, #38539, #19122, #18607, #15202, #11275, #7341 ),
 .UNSPECIFIED., .F., .F.,
 ( 4, 2, 2, 2, 2, 2, 2, 2, 2, 2, 2, 2, 2, 2, 4 ),
 ( 0.000000000000000000, 0.04341623943293104748, 0.1253847836472181121, 0.1766151237811480201, 0.2170652101236044962, 0.2575152964660598065, 0.3375200487661945692, 0.3875230189537799963, 0.4375259891413642577, 0.5000297018758445011, 0.5625334146103245780, 0.6625393549854932118, 0.7519024652212540349, 0.8948834415984711077, 1.000000000000000000 ),
 .UNSPECIFIED. ) ;
#10097 = ORIENTED_EDGE ( 'NONE', *, *, #20873, .F. ) ;
#10098 = CARTESIAN_POINT ( 'NONE',  ( 8.700054830325658628, -15.12214004741750095, -50.08846620145769890 ) ) ;
#10099 = B_SPLINE_CURVE_WITH_KNOTS ( 'NONE', 3,
 ( #21762, #25946, #16822, #33308, #25433, #37254, #44860, #1351, #21508, #32768, #48793, #28857, #8964, #24908, #17342, #13417, #40921, #37507 ),
 .UNSPECIFIED., .F., .F.,
 ( 4, 2, 2, 2, 2, 2, 2, 2, 4 ),
 ( 0.000000000000000000, 0.06250019596748117301, 0.1250003919349623460, 0.1875005879024435329, 0.2500007838699246920, 0.3125009798374057679, 0.3750011758048868438, 0.4375013717723678641, 0.5000015677398489400 ),
 .UNSPECIFIED. ) ;
#10100 = CARTESIAN_POINT ( 'NONE',  ( 63.71470905091258885, 1.396295651964360118, -61.88579195298250113 ) ) ;
#10101 = VERTEX_POINT ( 'NONE', #32862 ) ;
#10102 = CARTESIAN_POINT ( 'NONE',  ( 1.761217661586780059, 24.33376534107589961, -11.00321056186240121 ) ) ;
#10103 = PLANE ( 'NONE',  #37676 ) ;
#10104 = DIRECTION ( 'NONE',  ( 0.000000000000000000, 0.000000000000000000, 1.000000000000000000 ) ) ;
#10105 = CARTESIAN_POINT ( 'NONE',  ( 22.90378022332593488, -19.73380898580985132, -61.68156799471553597 ) ) ;
#10107 = DIRECTION ( 'NONE',  ( 1.000000000000000000, 0.000000000000000000, 0.000000000000000000 ) ) ;
#10106 = CARTESIAN_POINT ( 'NONE',  ( 43.43658709381130478, 8.673818529245354014, -69.38805309085101669 ) ) ;
#10108 = LINE ( 'NONE', #38676, #6717 ) ;
#10109 = CARTESIAN_POINT ( 'NONE',  ( 60.23130391296999875, -45.78304229081430066, -47.24246919202539630 ) ) ;
#10110 = ORIENTED_EDGE ( 'NONE', *, *, #40111, .T. ) ;
#10111 = VERTEX_POINT ( 'NONE', #45214 ) ;
#10112 = EDGE_CURVE ( 'NONE', #20864, #7979, #47106, .T. ) ;
#10113 = ORIENTED_EDGE ( 'NONE', *, *, #38895, .F. ) ;
#10114 = CARTESIAN_POINT ( 'NONE',  ( 61.32175331331019663, -45.22151323983460003, -46.73009288909239700 ) ) ;
#10115 =( GEOMETRIC_REPRESENTATION_CONTEXT ( 3 ) GLOBAL_UNCERTAINTY_ASSIGNED_CONTEXT ( ( #2797 ) ) GLOBAL_UNIT_ASSIGNED_CONTEXT ( ( #44346, #23632, #43837 ) ) REPRESENTATION_CONTEXT ( 'NONE', 'WORKASPACE' ) );
#10116 = PLANE ( 'NONE',  #41602 ) ;
#10117 = CARTESIAN_POINT ( 'NONE',  ( 0.3209249304026170480, -50.71887597443840434, -35.14999999999999858 ) ) ;
#10118 = EDGE_CURVE ( 'NONE', #51599, #40270, #2249, .T. ) ;
#10119 = CIRCLE ( 'NONE', #20116, 6.049999999999999822 ) ;
#10120 = ORIENTED_EDGE ( 'NONE', *, *, #18442, .F. ) ;
#10121 = VECTOR ( 'NONE', #36978, 1000.000000000000114 ) ;
#10122 = ADVANCED_FACE ( 'NONE', ( #923 ), #40493, .T. ) ;
#10123 = ORIENTED_EDGE ( 'NONE', *, *, #36824, .T. ) ;
#10124 = CARTESIAN_POINT ( 'NONE',  ( 11.97521017558959855, -21.02746670928087624, -73.16111001709356287 ) ) ;
#10125 = CYLINDRICAL_SURFACE ( 'NONE', #6001, 1.000000000000000888 ) ;
#10126 = ORIENTED_EDGE ( 'NONE', *, *, #16820, .T. ) ;
#10127 = CARTESIAN_POINT ( 'NONE',  ( 23.44932479906633560, -18.73862524642187211, -49.63616815528890669 ) ) ;
#10128 = CARTESIAN_POINT ( 'NONE',  ( 52.12745821273779256, -50.63299286582169856, -76.37383754424429583 ) ) ;
#10129 = CARTESIAN_POINT ( 'NONE',  ( 60.29580587845369877, 14.52606445528390111, -47.36817177740100249 ) ) ;
#10130 = CARTESIAN_POINT ( 'NONE',  ( 15.27481131963929961, -7.815634478900291171, -71.47757758863500044 ) ) ;
#10131 = CARTESIAN_POINT ( 'NONE',  ( 51.63351621991599671, 19.38381105532069881, -66.86356675664690385 ) ) ;
#10132 = CARTESIAN_POINT ( 'NONE',  ( 46.03123730839019601, 13.88381105531820126, -7.582885970392889696 ) ) ;
#10133 = EDGE_CURVE ( 'NONE', #14240, #15334, #39879, .T. ) ;
#10134 = CARTESIAN_POINT ( 'NONE',  ( 41.54582571382449174, -43.96466023683059632, -4.072799765277079764 ) ) ;
#10135 = CARTESIAN_POINT ( 'NONE',  ( 56.44408186407410000, 14.18700613804810118, -25.29404973353000230 ) ) ;
#10136 = CARTESIAN_POINT ( 'NONE',  ( 64.54859588824778882, 1.318423743231420087, -70.26560465517479770 ) ) ;
#10137 = CARTESIAN_POINT ( 'NONE',  ( 9.835632201235332772, -18.71667422018026272, -33.70134154844654972 ) ) ;
#10138 = CARTESIAN_POINT ( 'NONE',  ( 57.24929578595760660, -50.61618894467930119, -74.14999999999999147 ) ) ;
#10139 = VERTEX_POINT ( 'NONE', #48895 ) ;
#10140 = CARTESIAN_POINT ( 'NONE',  ( 14.78260632833550048, -52.41676442117930179, -76.03098605356829864 ) ) ;
#10141 = CARTESIAN_POINT ( 'NONE',  ( 47.20997691013830178, -54.78608722903020123, -54.63758431345319622 ) ) ;
#10142 = CARTESIAN_POINT ( 'NONE',  ( 9.949440222648611609, 33.40288359691523112, -46.96299386723978131 ) ) ;
#10143 = CARTESIAN_POINT ( 'NONE',  ( 11.43204200623334188, 33.34744811472585013, -44.55415195547232088 ) ) ;
#10144 = AXIS2_PLACEMENT_3D ( 'NONE', #3912, #32418, #40061 ) ;
#10145 = AXIS2_PLACEMENT_3D ( 'NONE', #25691, #820, #9224 ) ;
#10147 = EDGE_CURVE ( 'NONE', #13586, #19842, #17849, .T. ) ;
#10146 = CARTESIAN_POINT ( 'NONE',  ( 47.18324198357279897, -54.80726809202429450, -74.17417149933299925 ) ) ;
#10148 = AXIS2_PLACEMENT_3D ( 'NONE', #45047, #32186, #28789 ) ;
#10149 = CARTESIAN_POINT ( 'NONE',  ( 63.40532295848070987, 1.369664981662509939, -68.74641178933899255 ) ) ;
#10150 = CARTESIAN_POINT ( 'NONE',  ( 47.93286353489659746, -54.34025906026520403, -54.74353221703739791 ) ) ;
#10151 = LINE ( 'NONE', #5198, #19767 ) ;
#10152 = CARTESIAN_POINT ( 'NONE',  ( 56.52536539877749533, 19.51942783438209972, -53.84278118897309895 ) ) ;
#10153 = CARTESIAN_POINT ( 'NONE',  ( 47.96474501199910634, 23.16479111562100002, -55.26734477448599847 ) ) ;
#10154 = ORIENTED_EDGE ( 'NONE', *, *, #40116, .T. ) ;
#10155 = CARTESIAN_POINT ( 'NONE',  ( 19.87062220799639789, -9.634571621335810576, -72.52491758300199365 ) ) ;
#10156 = ORIENTED_EDGE ( 'NONE', *, *, #48882, .F. ) ;
#10157 = CARTESIAN_POINT ( 'NONE',  ( 82.51390001523527928, 13.88631490708104366, -46.70336726651584769 ) ) ;
#10158 = CARTESIAN_POINT ( 'NONE',  ( 68.13393739769620083, -48.61618894467930119, -65.65000000000000568 ) ) ;
#10159 = CARTESIAN_POINT ( 'NONE',  ( 22.46012708036917616, -10.75454455491590089, -41.29933415321534795 ) ) ;
#10161 = CARTESIAN_POINT ( 'NONE',  ( 52.58045495532469715, 18.61321147008669996, -28.06440927671260255 ) ) ;
#10160 = CARTESIAN_POINT ( 'NONE',  ( 83.89463082533569604, 13.54987550622989900, -47.42987625071230440 ) ) ;
#10162 = CARTESIAN_POINT ( 'NONE',  ( 21.59580785173019990, -11.15406726996270237, -72.23477911819139763 ) ) ;
#10163 = LINE ( 'NONE', #14606, #10334 ) ;
#10164 = CARTESIAN_POINT ( 'NONE',  ( 56.84932592767829362, -50.65659099804129539, -74.14999999999999147 ) ) ;
#10165 = CARTESIAN_POINT ( 'NONE',  ( 0.8744179034472430168, -26.70287881417802467, 17.07360679774999923 ) ) ;
#10166 = ORIENTED_EDGE ( 'NONE', *, *, #10213, .T. ) ;
#10167 = DIRECTION ( 'NONE',  ( -0.3294064756440938657, 0.9441882088883216673, 2.329877999999999163E-14 ) ) ;
#10168 = ORIENTED_EDGE ( 'NONE', *, *, #42022, .F. ) ;
#10169 = ORIENTED_EDGE ( 'NONE', *, *, #42114, .T. ) ;
#10170 = FACE_OUTER_BOUND ( 'NONE', #30720, .T. ) ;
#10171 = CARTESIAN_POINT ( 'NONE',  ( 24.04493739770276761, -15.61615029164005364, -39.50766986057545438 ) ) ;
#10172 = ADVANCED_FACE ( 'NONE', ( #1182 ), #40243, .F. ) ;
#10173 = CARTESIAN_POINT ( 'NONE',  ( 0.8851803632885170137, 11.70999949991828259, -20.85710678118654471 ) ) ;
#10174 = DIRECTION ( 'NONE',  ( -1.000000000000000000, -0.000000000000000000, -0.000000000000000000 ) ) ;
#10175 = EDGE_LOOP ( 'NONE', ( #1772, #4817 ) ) ;
#10176 = ORIENTED_EDGE ( 'NONE', *, *, #47921, .T. ) ;
#10177 = EDGE_CURVE ( 'NONE', #34347, #7977, #19758, .T. ) ;
#10178 = CARTESIAN_POINT ( 'NONE',  ( -22.39805312675529692, -21.43557466898330333, -54.24260450001559519 ) ) ;
#10179 = DIRECTION ( 'NONE',  ( 0.4999999999999995004, -0.8660254037844390407, 0.000000000000000000 ) ) ;
#10180 = CARTESIAN_POINT ( 'NONE',  ( 52.66874163714970081, -49.78066393629400466, -48.73461952183779999 ) ) ;
#10181 = CARTESIAN_POINT ( 'NONE',  ( 47.41023719977609829, 23.44958313673180328, -54.95588507597090455 ) ) ;
#10182 = CARTESIAN_POINT ( 'NONE',  ( 62.18049626896419824, -1.322404863900719985, -16.13653024010810100 ) ) ;
#10183 = CARTESIAN_POINT ( 'NONE',  ( 51.47836095788819932, -49.80706049537930369, -76.47682165003159582 ) ) ;
#10184 = CARTESIAN_POINT ( 'NONE',  ( 57.91488495618810362, -49.39618335747870503, -51.80378965555370030 ) ) ;
#10185 = AXIS2_PLACEMENT_3D ( 'NONE', #44818, #37216, #29081 ) ;
#10186 = ORIENTED_EDGE ( 'NONE', *, *, #37866, .F. ) ;
#10187 = CARTESIAN_POINT ( 'NONE',  ( 24.04012322605720797, -15.32992855636913632, -33.78081268262912573 ) ) ;
#10189 = CARTESIAN_POINT ( 'NONE',  ( 68.13393739769630031, 16.88381105531719939, -74.20000000000000284 ) ) ;
#10188 = CONICAL_SURFACE ( 'NONE', #19820, 0.6299999999999977840, 0.7853981633974476129 ) ;
#10190 = VERTEX_POINT ( 'NONE', #6675 ) ;
#10191 = CARTESIAN_POINT ( 'NONE',  ( 8.223585368203801593, -15.61624251583899969, -52.79233150823699816 ) ) ;
#10192 = DIRECTION ( 'NONE',  ( 1.000000000000000000, 0.000000000000000000, 0.000000000000000000 ) ) ;
#10193 = AXIS2_PLACEMENT_3D ( 'NONE', #3100, #15405, #39252 ) ;
#10194 = CARTESIAN_POINT ( 'NONE',  ( 9.309817790229448775, -11.74086454863580009, -45.17689247551329146 ) ) ;
#10195 = CARTESIAN_POINT ( 'NONE',  ( 13.78851007908129844, -50.80050206934620149, -21.52764351545879862 ) ) ;
#10196 = CARTESIAN_POINT ( 'NONE',  ( 56.33747328523660514, 19.49822906174120263, -74.84828165003129641 ) ) ;
#10197 = CARTESIAN_POINT ( 'NONE',  ( 47.64143405400680109, -54.53488714545009941, -74.17417149933299925 ) ) ;
#10198 = ORIENTED_EDGE ( 'NONE', *, *, #33745, .T. ) ;
#10199 = CARTESIAN_POINT ( 'NONE',  ( 55.59517693494780133, 14.55448978459209997, -16.53159430204590308 ) ) ;
#10200 = CYLINDRICAL_SURFACE ( 'NONE', #42430, 7.910999999999997812 ) ;
#10201 = CARTESIAN_POINT ( 'NONE',  ( 57.07954902837180100, -50.30027628258600458, -52.78599242821820070 ) ) ;
#10202 = CARTESIAN_POINT ( 'NONE',  ( 22.78040901162220067, -13.25674531116569987, -42.73859950308109035 ) ) ;
#10203 = CARTESIAN_POINT ( 'NONE',  ( 16.65420337942459739, 19.88381105532299742, -15.67544741556190324 ) ) ;
#10204 = ORIENTED_EDGE ( 'NONE', *, *, #17325, .F. ) ;
#10205 = CARTESIAN_POINT ( 'NONE',  ( 47.47121842882930309, 23.19633386185850199, -74.94862672502200951 ) ) ;
#10206 = CARTESIAN_POINT ( 'NONE',  ( 65.07863563811220331, 1.331842543267529821, -60.79893402932049895 ) ) ;
#10207 = CARTESIAN_POINT ( 'NONE',  ( 75.29303414918550175, -36.26344722174416546, -12.49608819919907354 ) ) ;
#10208 = CARTESIAN_POINT ( 'NONE',  ( 12.66989959080678574, -65.46799403849351506, -23.46212470398215544 ) ) ;
#10209 = DIRECTION ( 'NONE',  ( 0.4156269377774581275, -0.5720614028176801424, 0.7071067811865482389 ) ) ;
#10210 = ADVANCED_FACE ( 'NONE', ( #33657 ), #18460, .T. ) ;
#10211 = DIRECTION ( 'NONE',  ( 0.000000000000000000, 0.7071067811865475727, 0.7071067811865475727 ) ) ;
#10213 = EDGE_CURVE ( 'NONE', #23799, #49749, #49924, .T. ) ;
#10212 = CARTESIAN_POINT ( 'NONE',  ( 82.27845167518849223, 13.94631328714430119, -46.87713584290389690 ) ) ;
#10214 = CARTESIAN_POINT ( 'NONE',  ( -0.004241732451505779607, 19.56172084038890091, -34.76917063876959446 ) ) ;
#10216 = CARTESIAN_POINT ( 'NONE',  ( 44.39799025600027704, -39.11365857096617304, -68.49055761514939888 ) ) ;
#10215 = CARTESIAN_POINT ( 'NONE',  ( -31.36606260230380272, 21.88381105532059934, 11.84999999999999964 ) ) ;
#10217 = DIRECTION ( 'NONE',  ( -1.000000000000000000, 0.000000000000000000, 0.000000000000000000 ) ) ;
#10218 = FACE_OUTER_BOUND ( 'NONE', #24511, .T. ) ;
#10219 = CARTESIAN_POINT ( 'NONE',  ( 12.78938691692309959, 32.28743192295770115, -45.78213823142860406 ) ) ;
#10220 = ADVANCED_FACE ( 'NONE', ( #14015 ), #5577, .T. ) ;
#10221 = EDGE_LOOP ( 'NONE', ( #2106, #44075, #34839, #45438 ) ) ;
#10222 = VECTOR ( 'NONE', #26279, 1000.000000000000000 ) ;
#10223 = CARTESIAN_POINT ( 'NONE',  ( 53.03535128242899788, -49.56646391233060456, -48.94674795462399430 ) ) ;
#10224 = VECTOR ( 'NONE', #20842, 1000.000000000000000 ) ;
#10225 = ORIENTED_EDGE ( 'NONE', *, *, #39034, .F. ) ;
#10226 = CARTESIAN_POINT ( 'NONE',  ( 47.22924368751841229, 8.040797879301941009, -54.71938430924458885 ) ) ;
#10227 = LINE ( 'NONE', #30374, #932 ) ;
#10228 = CARTESIAN_POINT ( 'NONE',  ( 13.72477621988739926, 19.74414037213060169, -21.83795113765379980 ) ) ;
#10229 = CARTESIAN_POINT ( 'NONE',  ( 56.23669252666629603, 14.33142556199779882, -25.29918085107650327 ) ) ;
#10230 = CARTESIAN_POINT ( 'NONE',  ( 18.88997640609209938, -22.10824622113840121, -44.82502897017909049 ) ) ;
#10231 = CARTESIAN_POINT ( 'NONE',  ( 29.06532888865369912, -26.71461010031690009, -34.89721277419639733 ) ) ;
#10232 = CARTESIAN_POINT ( 'NONE',  ( 53.15063587404129919, 18.30021473852120195, -49.06766776400879593 ) ) ;
#10233 = CARTESIAN_POINT ( 'NONE',  ( 64.76518258084500701, 1.097545367735389910, -60.73071135393688991 ) ) ;
#10234 = DIRECTION ( 'NONE',  ( 0.000000000000000000, 0.000000000000000000, 1.000000000000000000 ) ) ;
#10235 = ORIENTED_EDGE ( 'NONE', *, *, #10454, .F. ) ;
#10236 = CARTESIAN_POINT ( 'NONE',  ( 13.63212480980059915, -23.05444693688020052, -35.89078365052999686 ) ) ;
#10237 = DIRECTION ( 'NONE',  ( 0.000000000000000000, 0.000000000000000000, 1.000000000000000000 ) ) ;
#10238 = CARTESIAN_POINT ( 'NONE',  ( 14.15300983787075673, -7.927875040723331601, -81.21199936902040406 ) ) ;
#10239 = CARTESIAN_POINT ( 'NONE',  ( 73.10458614724748827, 1.096044978595170027, -62.36169201816110075 ) ) ;
#10240 = CARTESIAN_POINT ( 'NONE',  ( 11.04564840984290086, -65.17882761888340326, -17.95839446281759777 ) ) ;
#10241 = PLANE ( 'NONE',  #48076 ) ;
#10242 = CARTESIAN_POINT ( 'NONE',  ( 24.04492500005543576, -15.63237907448977637, -75.79297730590246829 ) ) ;
#10243 = CARTESIAN_POINT ( 'NONE',  ( 71.42462519098059204, 0.8888742037077599356, -60.63285689971630177 ) ) ;
#10244 = CARTESIAN_POINT ( 'NONE',  ( 21.54530318899829311, -11.45757911204534807, -58.24448665876980868 ) ) ;
#10245 = EDGE_CURVE ( 'NONE', #36323, #31006, #45758, .T. ) ;
#10246 = CARTESIAN_POINT ( 'NONE',  ( 64.98165955279610273, 1.327322800621349996, -70.45801890699070213 ) ) ;
#10247 = ORIENTED_EDGE ( 'NONE', *, *, #22619, .F. ) ;
#10248 = CARTESIAN_POINT ( 'NONE',  ( 10.49110564618760044, -63.26315525827371289, -45.62557459999030129 ) ) ;
#10249 = CARTESIAN_POINT ( 'NONE',  ( 22.90003758132117184, -14.80394619968367209, -32.41496898898599710 ) ) ;
#10250 = ORIENTED_EDGE ( 'NONE', *, *, #15517, .F. ) ;
#10251 = DIRECTION ( 'NONE',  ( 0.8340645993220362486, 0.5516667872527503125, 0.000000000000000000 ) ) ;
#10252 = CARTESIAN_POINT ( 'NONE',  ( 57.36123083241199794, 18.90300136664210129, -52.61896061011540127 ) ) ;
#10253 = CARTESIAN_POINT ( 'NONE',  ( 46.35275103504449845, -52.90993241930539881, -76.14999999999999147 ) ) ;
#10254 = CARTESIAN_POINT ( 'NONE',  ( 52.34620960925839483, 18.68177451820979940, -77.13858428499739261 ) ) ;
#10255 = ORIENTED_EDGE ( 'NONE', *, *, #27786, .T. ) ;
#10256 = CARTESIAN_POINT ( 'NONE',  ( 11.71633470187599180, -65.33094175621533850, -47.42091646568417929 ) ) ;
#10257 = B_SPLINE_SURFACE_WITH_KNOTS ( 'NONE', 3, 3, ( 
 ( #49784, #21974, #41916, #26167, #9941, #37986, #2081, #34028, #45591, #25647 ),
 ( #21203, #41137, #49277, #1820, #33522, #50038, #5755, #22234, #18310, #45335 ),
 ( #30095, #13876, #37209, #21464, #1310, #13369, #29335, #38242, #21712, #46122 ),
 ( #9440, #50305, #17801, #10206, #42177, #25389, #29836, #41391, #14390, #37463 ),
 ( #1561, #17549, #49534, #29586, #9687, #11504, #31127, #27204, #47153, #39273 ),
 ( #22749, #35598, #39534, #27461, #23515, #34551, #3378, #43464, #51069, #19350 ),
 ( #7565, #35332, #19607, #3635, #18575, #15170, #30615, #15683, #10724, #6798 ),
 ( #14904, #38769, #14647, #15431, #31382, #51584, #51331, #31637, #10468, #30869 ),
 ( #18827, #26424, #47409, #42441, #35065, #26678, #6530, #46639, #22492, #38500 ),
 ( #50813, #2602, #46896, #50555, #42700, #2862, #34810, #10987, #11242, #26951 ),
 ( #42956, #7055, #23005, #39026, #3121, #43215, #19088, #7306, #23258, #41940 ),
 ( #357, #41672, #42202, #12412, #1845, #30123, #5778, #4805, #21740, #46142 ),
 ( #33797, #4537, #37748, #606, #20772, #36761, #10233, #872, #17823, #40446 ),
 ( #20510, #6041, #16592, #9710, #34049, #14155, #18081, #16866, #50059, #49806 ),
 ( #9965, #8743, #36503, #25925, #26192, #48317, #28899, #38007, #24691, #13899 ),
 ( #12943, #29857, #40707, #32544, #36248, #20256, #16339, #32295, #32813, #28376 ) ),
 .UNSPECIFIED., .F., .F., .F.,
 ( 4, 2, 2, 2, 2, 2, 2, 4 ),
 ( 4, 1, 1, 1, 1, 1, 1, 4 ),
 ( -4.528785000000000087E-15, 0.07216186899280399580, 0.1546325764131560032, 0.2061767685508759940, 0.2319488646197360171, 0.2731842183299119653, 0.3391607842661930050, 0.4123535371017559847 ),
 ( 0.000000000000000000, 0.1428571428571430157, 0.2857142857142860315, 0.4285714285714289917, 0.5714285714285709528, 0.7142857142857139685, 0.8571428571428569843, 1.000000000000000000 ),
 .UNSPECIFIED. ) ;
#10258 = CARTESIAN_POINT ( 'NONE',  ( 57.55751162087899786, 18.85811933572220056, -52.57651812407429759 ) ) ;
#10259 = DIRECTION ( 'NONE',  ( 0.000000000000000000, 0.000000000000000000, -1.000000000000000000 ) ) ;
#10260 = CARTESIAN_POINT ( 'NONE',  ( 9.532069060239026115, -20.02275000618190148, -66.32023582542863949 ) ) ;
#10261 = CARTESIAN_POINT ( 'NONE',  ( 8.075524310527260496, -13.87128247942689896, -62.86020799324039388 ) ) ;
#10262 = CARTESIAN_POINT ( 'NONE',  ( 20.11812604725867359, -22.52867784916062277, -47.84100274957454957 ) ) ;
#10263 = CARTESIAN_POINT ( 'NONE',  ( 45.71767653649329333, -38.12345008805129254, -61.73130295846522841 ) ) ;
#10264 = ORIENTED_EDGE ( 'NONE', *, *, #44465, .F. ) ;
#10265 = CARTESIAN_POINT ( 'NONE',  ( 57.07405361051419845, -45.88223445567830083, -26.24937779502229773 ) ) ;
#10266 = CARTESIAN_POINT ( 'NONE',  ( 11.96399840028469974, -21.79019109587850167, -44.92174179178260118 ) ) ;
#10267 = TOROIDAL_SURFACE ( 'NONE', #28642, 18.00000000000000000, 2.000000000000000000 ) ;
#10268 = CARTESIAN_POINT ( 'NONE',  ( 53.23493483693680162, -49.52411911180049486, -49.16095918439189916 ) ) ;
#10269 = CARTESIAN_POINT ( 'NONE',  ( 9.170653946503200871, -13.93511158109739867, -32.14999999999999858 ) ) ;
#10270 = CARTESIAN_POINT ( 'NONE',  ( 24.44780054039034667, -21.65656408986289705, -18.58999999999999986 ) ) ;
#10271 = CARTESIAN_POINT ( 'NONE',  ( 14.20218124254490100, 20.03470611338460472, -74.90176971618339508 ) ) ;
#10272 = CARTESIAN_POINT ( 'NONE',  ( 8.428884225131936248, -13.54533900620925202, -50.87566462626018904 ) ) ;
#10273 = CARTESIAN_POINT ( 'NONE',  ( 45.18655670870639796, -45.12046577740490250, -7.327032537671530399 ) ) ;
#10274 = CARTESIAN_POINT ( 'NONE',  ( 10.43684629066897074, -10.04834157992367771, -60.75387912627691378 ) ) ;
#10275 = CARTESIAN_POINT ( 'NONE',  ( 8.046702716277120970, -14.01015161116950125, -62.57006952842979075 ) ) ;
#10276 = ORIENTED_EDGE ( 'NONE', *, *, #36418, .T. ) ;
#10277 = CARTESIAN_POINT ( 'NONE',  ( 54.20225837649419987, -48.03317578680400146, -26.08669670602439794 ) ) ;
#10278 = EDGE_CURVE ( 'NONE', #47824, #20725, #46522, .T. ) ;
#10279 = CARTESIAN_POINT ( 'NONE',  ( 55.75888635692119522, -50.73156338577249613, -75.40713992321559545 ) ) ;
#10281 = CARTESIAN_POINT ( 'NONE',  ( 42.18259662932334919, -39.78407723318860434, -75.44989511367202795 ) ) ;
#10280 = CARTESIAN_POINT ( 'NONE',  ( 3.573464422544550434, 25.59147421693169733, -10.25614976361119979 ) ) ;
#10282 = DIRECTION ( 'NONE',  ( -0.3044500358626250902, -0.5455827667248117629, 0.7808006277636730941 ) ) ;
#10283 = DIRECTION ( 'NONE',  ( -1.000000000000000000, 0.000000000000000000, 0.000000000000000000 ) ) ;
#10284 = EDGE_CURVE ( 'NONE', #39070, #33614, #27333, .T. ) ;
#10285 = ORIENTED_EDGE ( 'NONE', *, *, #46075, .F. ) ;
#10286 = CARTESIAN_POINT ( 'NONE',  ( 14.75122905864259160, 21.64019614509532730, -76.12465453342632316 ) ) ;
#10287 = CARTESIAN_POINT ( 'NONE',  ( 47.42217282182370752, 23.41203903866150071, -54.87062249528260338 ) ) ;
#10288 = DIRECTION ( 'NONE',  ( 0.000000000000000000, 0.000000000000000000, 1.000000000000000000 ) ) ;
#10289 = CARTESIAN_POINT ( 'NONE',  ( 17.63393739769620083, -32.15793020853440254, -34.64999999999999858 ) ) ;
#10290 = CARTESIAN_POINT ( 'NONE',  ( 61.00623573019170465, 14.14465591030429970, -46.89457832669390314 ) ) ;
#10291 = CARTESIAN_POINT ( 'NONE',  ( 11.74995128003140010, 34.02380396729650158, -17.00864127458340036 ) ) ;
#10292 = CARTESIAN_POINT ( 'NONE',  ( 51.68242196497799767, 17.78920151642020286, -76.95384497402039869 ) ) ;
#10293 = CARTESIAN_POINT ( 'NONE',  ( 53.26662649590710430, 18.19965403720820163, -48.79175420715170475 ) ) ;
#10294 = DIRECTION ( 'NONE',  ( 0.000000000000000000, 0.000000000000000000, 1.000000000000000000 ) ) ;
#10295 = CARTESIAN_POINT ( 'NONE',  ( 58.76885703184290577, -46.69396177055759978, -47.97628940940079900 ) ) ;
#10296 = CARTESIAN_POINT ( 'NONE',  ( 52.71556874917159519, 18.49758023621189906, -28.15002987606190032 ) ) ;
#10297 = CARTESIAN_POINT ( 'NONE',  ( 55.62530649940679695, 19.78524991857049997, -53.26680650779459825 ) ) ;
#10298 = AXIS2_PLACEMENT_3D ( 'NONE', #17054, #33008, #49031 ) ;
#10299 = CARTESIAN_POINT ( 'NONE',  ( 63.25226693078700180, 1.024253516290730026, -69.12311412914529285 ) ) ;
#10300 = DIRECTION ( 'NONE',  ( 0.000000000000000000, 0.000000000000000000, 1.000000000000000000 ) ) ;
#10301 = B_SPLINE_CURVE_WITH_KNOTS ( 'NONE', 3,
 ( #29756, #48941, #29511, #1230, #37641, #9364, #13044, #44996 ),
 .UNSPECIFIED., .F., .F.,
 ( 4, 2, 2, 4 ),
 ( 0.05028014561794270920, 0.06097673919875580550, 0.07774712209399009533, 0.08013618654945309228 ),
 .UNSPECIFIED. ) ;
#10302 = CARTESIAN_POINT ( 'NONE',  ( 56.32402052750479982, -45.11618894467940066, -10.15270052037220161 ) ) ;
#10303 = CARTESIAN_POINT ( 'NONE',  ( 19.51692496783413944, 22.41474627964059962, -16.78241351213016586 ) ) ;
#10304 = CARTESIAN_POINT ( 'NONE',  ( 10.49444742495719929, 32.12130227714850150, -45.62689257694430012 ) ) ;
#10305 = VECTOR ( 'NONE', #50139, 999.9999999999998863 ) ;
#10306 = CARTESIAN_POINT ( 'NONE',  ( 72.89288316602700490, 1.231980527807239989, -62.16651341217360027 ) ) ;
#10307 = DIRECTION ( 'NONE',  ( -1.000000000000000000, 0.000000000000000000, 0.000000000000000000 ) ) ;
#10308 = EDGE_CURVE ( 'NONE', #46894, #30043, #18199, .T. ) ;
#10309 = DIRECTION ( 'NONE',  ( 0.000000000000000000, -1.000000000000000000, 0.000000000000000000 ) ) ;
#10310 = VERTEX_POINT ( 'NONE', #34432 ) ;
#10311 = ORIENTED_EDGE ( 'NONE', *, *, #35907, .T. ) ;
#10312 = CARTESIAN_POINT ( 'NONE',  ( 48.02894741700589520, 23.13744333908360318, -55.28037973459740329 ) ) ;
#10313 = EDGE_CURVE ( 'NONE', #11745, #19040, #41422, .T. ) ;
#10314 = CARTESIAN_POINT ( 'NONE',  ( 76.55694930642907536, 0.1129182662885630517, -13.47282127292171516 ) ) ;
#10315 = ORIENTED_EDGE ( 'NONE', *, *, #9099, .F. ) ;
#10316 = CARTESIAN_POINT ( 'NONE',  ( 12.94329929307280125, -65.51432672297359261, -47.65575625725580267 ) ) ;
#10317 = CARTESIAN_POINT ( 'NONE',  ( 56.04095368967779933, -46.04400048969489490, -25.92328318301699852 ) ) ;
#10318 = CARTESIAN_POINT ( 'NONE',  ( 57.77564497937559906, -31.65172285061208868, -17.11446609406731767 ) ) ;
#10319 = CARTESIAN_POINT ( 'NONE',  ( 68.13393739845098196, -29.66618894467940137, -89.64999999979866629 ) ) ;
#10320 = ORIENTED_EDGE ( 'NONE', *, *, #40036, .F. ) ;
#10321 = CARTESIAN_POINT ( 'NONE',  ( 11.89321892218980103, 34.20364954172580241, -22.25048313876769868 ) ) ;
#10322 = CARTESIAN_POINT ( 'NONE',  ( 45.84154099693467543, 6.904674428428495325, -61.11197212361961562 ) ) ;
#10323 = CARTESIAN_POINT ( 'NONE',  ( -14.38189736085656278, 8.722225734311907175, -47.59448514485664816 ) ) ;
#10324 = ORIENTED_EDGE ( 'NONE', *, *, #40709, .T. ) ;
#10325 = CARTESIAN_POINT ( 'NONE',  ( 45.64501526700150436, -46.12166612246060282, -9.406926139117178565 ) ) ;
#10326 = AXIS2_PLACEMENT_3D ( 'NONE', #7250, #10926, #27405 ) ;
#10327 = CARTESIAN_POINT ( 'NONE',  ( 52.08182673490480141, 1.850722219266808910, -19.98516726105009411 ) ) ;
#10328 = CARTESIAN_POINT ( 'NONE',  ( 16.19818216288450330, 19.87900877640220187, -21.03492549853969962 ) ) ;
#10329 = CARTESIAN_POINT ( 'NONE',  ( 22.90054308430137553, -16.11587269579376169, -48.87067656418971495 ) ) ;
#10330 = CARTESIAN_POINT ( 'NONE',  ( 16.49581108810665953, -22.37396559151951436, -46.93579869999577170 ) ) ;
#10331 = CARTESIAN_POINT ( 'NONE',  ( 71.83406239697100659, 11.38381102407110035, -68.85000000076199456 ) ) ;
#10332 = CARTESIAN_POINT ( 'NONE',  ( 47.23192694729809915, -54.73625513866609538, -74.50311761397450994 ) ) ;
#10333 = CARTESIAN_POINT ( 'NONE',  ( 45.26119862906019620, 13.15965671286969929, -5.724999702673090773 ) ) ;
#10334 = VECTOR ( 'NONE', #50516, 1000.000000000000000 ) ;
#10335 = CARTESIAN_POINT ( 'NONE',  ( 51.37525108058719070, 21.43002075209610169, -53.68096604571569941 ) ) ;
#10336 = CIRCLE ( 'NONE', #46374, 0.4999999999999983902 ) ;
#10337 = AXIS2_PLACEMENT_3D ( 'NONE', #48016, #16040, #32499 ) ;
#10338 = CARTESIAN_POINT ( 'NONE',  ( 53.68570370402219538, 19.91397335543889824, -75.73808979149589504 ) ) ;
#10339 = CARTESIAN_POINT ( 'NONE',  ( 57.42077085024149596, 13.96450533941020034, -25.73600857157110156 ) ) ;
#10340 = CARTESIAN_POINT ( 'NONE',  ( 10.07106228387759828, -10.02832118826320063, -36.74469800169000422 ) ) ;
#10341 = VERTEX_POINT ( 'NONE', #14529 ) ;
#10342 = DIRECTION ( 'NONE',  ( -0.4439767838698117641, 0.8960382890170590642, 0.000000000000000000 ) ) ;
#10343 = ADVANCED_FACE ( 'NONE', ( #22636 ), #21593, .T. ) ;
#10344 = CARTESIAN_POINT ( 'NONE',  ( -4.193175284732109986, -49.34067351630189791, -7.780658117633309168 ) ) ;
#10345 = DIRECTION ( 'NONE',  ( 7.935614746461580696E-16, 6.060292087350920604E-16, -1.000000000000000000 ) ) ;
#10346 = DIRECTION ( 'NONE',  ( 0.000000000000000000, 1.000000000000000000, 0.000000000000000000 ) ) ;
#10347 = DIRECTION ( 'NONE',  ( 7.719205000000000365E-17, 1.062456999999999985E-16, 1.000000000000000000 ) ) ;
#10348 = DIRECTION ( 'NONE',  ( 0.000000000000000000, 6.470469973722704271E-12, 1.000000000000000000 ) ) ;
#10349 = CARTESIAN_POINT ( 'NONE',  ( 82.25807818787700398, -45.12248685479210053, -46.55740799543180231 ) ) ;
#10350 = CARTESIAN_POINT ( 'NONE',  ( 16.13393739769620083, -15.61618894467929941, 5.856814007409659517 ) ) ;
#10351 = CARTESIAN_POINT ( 'NONE',  ( 42.84544925580660646, 11.76657522153120183, -4.190148907829390090 ) ) ;
#10352 = CARTESIAN_POINT ( 'NONE',  ( 65.07026117056300052, 1.388189907116970101, -70.28386057589730740 ) ) ;
#10353 = DIRECTION ( 'NONE',  ( 1.000000000000000000, 0.000000000000000000, 0.000000000000000000 ) ) ;
#10354 = CARTESIAN_POINT ( 'NONE',  ( 44.89329732587840027, 2.479591951453110177, -35.14498018237689791 ) ) ;
#10355 = AXIS2_PLACEMENT_3D ( 'NONE', #47935, #35617, #16208 ) ;
#10356 = CARTESIAN_POINT ( 'NONE',  ( 75.73620089847491954, -43.35142246084668471, -13.49567144614401748 ) ) ;
#10357 = DIRECTION ( 'NONE',  ( 0.000000000000000000, -1.000000000000000000, 0.000000000000000000 ) ) ;
#10358 = ORIENTED_EDGE ( 'NONE', *, *, #47034, .F. ) ;
#10359 = CARTESIAN_POINT ( 'NONE',  ( 9.058892520694989514, -13.28157241797509869, -58.16879716994699834 ) ) ;
#10360 =( BOUNDED_CURVE ( )  B_SPLINE_CURVE ( 2, ( #25035, #45250, #2446 ),
 .UNSPECIFIED., .F., .T. ) 
 B_SPLINE_CURVE_WITH_KNOTS ( ( 3, 3 ),
 ( 1.104980434577240045, 2.168627590050209886 ),
 .UNSPECIFIED. ) 
 CURVE ( )  GEOMETRIC_REPRESENTATION_ITEM ( )  RATIONAL_B_SPLINE_CURVE ( ( 1.323085463760209857, 1.425426480542939967, 1.425426480542939967 ) ) 
 REPRESENTATION_ITEM ( '' )  );
#10361 = CARTESIAN_POINT ( 'NONE',  ( 63.82110572780499780, 1.345243094457279964, -61.64184835600830326 ) ) ;
#10362 = VERTEX_POINT ( 'NONE', #42320 ) ;
#10363 = CARTESIAN_POINT ( 'NONE',  ( 17.01976292083999809, -22.38318504511303075, -68.91115224776299897 ) ) ;
#10364 = DIRECTION ( 'NONE',  ( 0.000000000000000000, 1.000000000000000000, 0.000000000000000000 ) ) ;
#10365 = DIRECTION ( 'NONE',  ( 0.8857883891771956009, -0.4640893551880597712, 2.775557561562888578E-17 ) ) ;
#10366 = CARTESIAN_POINT ( 'NONE',  ( 47.79865291297670638, -54.41610742667179323, -54.75837665837189405 ) ) ;
#10367 = CARTESIAN_POINT ( 'NONE',  ( 22.90122612410699077, -15.61618894223031440, -74.45282020639018583 ) ) ;
#10368 = CARTESIAN_POINT ( 'NONE',  ( 9.166869512392668895, -16.70799882457410135, -81.23899999999999011 ) ) ;
#10369 = CARTESIAN_POINT ( 'NONE',  ( 44.88826907266649613, -46.10884305417119577, -8.898922653467518984 ) ) ;
#10370 = ORIENTED_EDGE ( 'NONE', *, *, #19521, .T. ) ;
#10371 = ORIENTED_EDGE ( 'NONE', *, *, #2403, .F. ) ;
#10372 = EDGE_CURVE ( 'NONE', #34590, #14522, #9762, .T. ) ;
#10373 = EDGE_LOOP ( 'NONE', ( #759, #11531, #29434, #29577, #47910, #31877, #14689 ) ) ;
#10374 = CARTESIAN_POINT ( 'NONE',  ( 8.222988179026620159, -15.61639226004780134, -48.50766849176299189 ) ) ;
#10375 = DIRECTION ( 'NONE',  ( 0.000000000000000000, 0.000000000000000000, -1.000000000000000000 ) ) ;
#10376 = CIRCLE ( 'NONE', #1991, 1.500000000000001332 ) ;
#10377 = VECTOR ( 'NONE', #40047, 1000.000000000000000 ) ;
#10378 = ORIENTED_EDGE ( 'NONE', *, *, #25769, .F. ) ;
#10379 = VERTEX_POINT ( 'NONE', #37592 ) ;
#10380 = CARTESIAN_POINT ( 'NONE',  ( 22.90092678307498986, -15.63002908252453516, -72.45347661182641730 ) ) ;
#10381 = DIRECTION ( 'NONE',  ( 0.000000000000000000, 1.000000000000000000, 0.000000000000000000 ) ) ;
#10382 = APPLICATION_CONTEXT ( 'automotive_design' ) ;
#10383 = DIRECTION ( 'NONE',  ( 0.000000000000000000, -1.000000000000000000, 0.000000000000000000 ) ) ;
#10384 = ORIENTED_EDGE ( 'NONE', *, *, #46563, .T. ) ;
#10385 = CARTESIAN_POINT ( 'NONE',  ( 24.04461900158476340, -15.61617122039998051, -49.50766513674645353 ) ) ;
#10386 = CARTESIAN_POINT ( 'NONE',  ( 52.52866731283389612, -50.77248804783529579, -76.33211553913280056 ) ) ;
#10387 = CARTESIAN_POINT ( 'NONE',  ( 60.56229479663769411, 14.39144051458180051, -47.32503848654899770 ) ) ;
#10388 = CARTESIAN_POINT ( 'NONE',  ( 20.40194918913540079, -22.20184175512399705, -74.32945910692518510 ) ) ;
#10389 = FACE_OUTER_BOUND ( 'NONE', #50725, .T. ) ;
#10390 = VECTOR ( 'NONE', #19069, 1000.000000000000000 ) ;
#10391 = CARTESIAN_POINT ( 'NONE',  ( 41.33192651172240062, 13.52043771225929980, -5.349971584196499208 ) ) ;
#10392 = CARTESIAN_POINT ( 'NONE',  ( 41.74201990413180141, -44.07933325136760061, -4.572451439087529934 ) ) ;
#10393 = DIRECTION ( 'NONE',  ( -1.000000000000000000, 0.000000000000000000, 0.000000000000000000 ) ) ;
#10394 = CARTESIAN_POINT ( 'NONE',  ( 65.04849531401515605, 1.029538923565187059, -17.85480804919157194 ) ) ;
#10395 = B_SPLINE_CURVE_WITH_KNOTS ( 'NONE', 3,
 ( #10816, #26775, #51422, #42793, #11333, #50644, #6888, #18403, #27297, #38601, #14994, #31470, #43305, #14478 ),
 .UNSPECIFIED., .F., .F.,
 ( 4, 2, 2, 1, 1, 2, 2, 4 ),
 ( 0.4756219748450489226, 0.6067164811337820707, 0.6722637342781461189, 0.7050373608503291978, 0.7214241741364214588, 0.7296175807794663681, 0.7378109874225112774, 1.000000000000000000 ),
 .UNSPECIFIED. ) ;
#10396 = CARTESIAN_POINT ( 'NONE',  ( 64.57410506046470289, 0.9210617359723509701, -70.48005104816739674 ) ) ;
#10397 = DIRECTION ( 'NONE',  ( 0.000000000000000000, 0.000000000000000000, -1.000000000000000000 ) ) ;
#10398 = LINE ( 'NONE', #2791, #45158 ) ;
#10399 = CARTESIAN_POINT ( 'NONE',  ( 19.80339606041890121, -8.679199590085181271, -50.94238055261769915 ) ) ;
#10400 = ORIENTED_EDGE ( 'NONE', *, *, #50166, .F. ) ;
#10401 = CARTESIAN_POINT ( 'NONE',  ( 14.57450527953789887, -52.55982454884319566, -76.04476946176040997 ) ) ;
#10402 = ADVANCED_FACE ( 'NONE', ( #6157 ), #22114, .T. ) ;
#10403 = VECTOR ( 'NONE', #13910, 1000.000000000000000 ) ;
#10404 = CARTESIAN_POINT ( 'NONE',  ( 57.55751162087899786, 19.37927774188059971, -53.76309025933280594 ) ) ;
#10405 = CARTESIAN_POINT ( 'NONE',  ( 44.56408710588276278, -39.99924422512690825, -63.92564782215845298 ) ) ;
#10406 = EDGE_CURVE ( 'NONE', #6632, #43432, #20281, .T. ) ;
#10407 = LINE ( 'NONE', #17998, #11724 ) ;
#10408 = EDGE_CURVE ( 'NONE', #17150, #47191, #46582, .T. ) ;
#10409 = CARTESIAN_POINT ( 'NONE',  ( 46.89823403300989924, -54.16139584019150277, -75.66073271794819277 ) ) ;
#10410 = ADVANCED_FACE ( 'NONE', ( #45730 ), #19988, .T. ) ;
#10411 = CARTESIAN_POINT ( 'NONE',  ( 63.29194469617720387, 1.263903724274369811, -68.92034810279041324 ) ) ;
#10412 = CARTESIAN_POINT ( 'NONE',  ( 22.46010835836494479, -20.47785901973523792, -52.00066279612408948 ) ) ;
#10413 = DIRECTION ( 'NONE',  ( -1.000000000000000000, 0.000000000000000000, 0.000000000000000000 ) ) ;
#10414 = CARTESIAN_POINT ( 'NONE',  ( 48.19306574706310897, 22.95973674188289948, -54.68274065309989851 ) ) ;
#10415 = ORIENTED_EDGE ( 'NONE', *, *, #49170, .F. ) ;
#10416 = CARTESIAN_POINT ( 'NONE',  ( 11.18221182729259944, -20.63843675327109750, -77.59492917107350252 ) ) ;
#10417 = ORIENTED_EDGE ( 'NONE', *, *, #18193, .F. ) ;
#10418 = CARTESIAN_POINT ( 'NONE',  ( 71.19761362482960010, 1.388189907116970101, -70.28386057589720792 ) ) ;
#10419 = DIRECTION ( 'NONE',  ( 0.000000000000000000, 0.000000000000000000, 1.000000000000000000 ) ) ;
#10420 = DIRECTION ( 'NONE',  ( -1.000000000000000000, 0.000000000000000000, 0.000000000000000000 ) ) ;
#10422 = ADVANCED_FACE ( 'NONE', ( #47543 ), #23905, .F. ) ;
#10421 = CARTESIAN_POINT ( 'NONE',  ( 15.09849997108853081, -7.705175646165889347, -40.96600124313015101 ) ) ;
#10424 = CARTESIAN_POINT ( 'NONE',  ( 53.18037562183940281, 17.96329376868539995, -26.81634874583109962 ) ) ;
#10423 = FACE_OUTER_BOUND ( 'NONE', #47002, .T. ) ;
#10425 = CARTESIAN_POINT ( 'NONE',  ( 23.17183048500919895, -16.07513071938780058, -80.47354794880780560 ) ) ;
#10426 = CARTESIAN_POINT ( 'NONE',  ( 12.95169883137720035, -21.91030696805099964, -79.49618351660049598 ) ) ;
#10427 = CARTESIAN_POINT ( 'NONE',  ( 9.807866034005373379, -10.75439047797270398, -67.00066434089428924 ) ) ;
#10428 = CARTESIAN_POINT ( 'NONE',  ( 17.90512202794597130, -22.20708004173628325, -40.86942847551643609 ) ) ;
#10429 = ORIENTED_EDGE ( 'NONE', *, *, #51512, .T. ) ;
#10430 = CARTESIAN_POINT ( 'NONE',  ( 8.731180243531696306, -48.92556967366426335, -34.79644561402096770 ) ) ;
#10431 = AXIS2_PLACEMENT_3D ( 'NONE', #33576, #9237, #8973 ) ;
#10432 = EDGE_CURVE ( 'NONE', #24006, #14961, #29822, .T. ) ;
#10433 = ORIENTED_EDGE ( 'NONE', *, *, #21909, .T. ) ;
#10434 = CARTESIAN_POINT ( 'NONE',  ( 11.92574115021280079, -64.84651890715629463, -16.17905523991749916 ) ) ;
#10435 = DIRECTION ( 'NONE',  ( 0.5685928097855380559, -0.5944782866685500711, -0.5685928097855370567 ) ) ;
#10436 = DIRECTION ( 'NONE',  ( 0.000000000000000000, 0.000000000000000000, -1.000000000000000000 ) ) ;
#10437 = DIRECTION ( 'NONE',  ( 0.000000000000000000, 1.000000000000000000, 0.000000000000000000 ) ) ;
#10438 = EDGE_LOOP ( 'NONE', ( #24391, #19135 ) ) ;
#10439 = ORIENTED_EDGE ( 'NONE', *, *, #30870, .T. ) ;
#10440 = CARTESIAN_POINT ( 'NONE',  ( -20.85360007628929679, -28.79220445502869907, -53.09923876720240088 ) ) ;
#10441 = CYLINDRICAL_SURFACE ( 'NONE', #19530, 7.910999999999997812 ) ;
#10442 = AXIS2_PLACEMENT_3D ( 'NONE', #30178, #46198, #10282 ) ;
#10443 = CARTESIAN_POINT ( 'NONE',  ( 52.94229166988520063, 18.29346755790560053, -48.62158860753390144 ) ) ;
#10444 = CARTESIAN_POINT ( 'NONE',  ( 63.51857099600739787, -1.340451266368759775, -16.28959496159560061 ) ) ;
#10445 = CARTESIAN_POINT ( 'NONE',  ( 50.72813273197049710, -50.14449156618339742, -76.16412224154011312 ) ) ;
#10446 = CARTESIAN_POINT ( 'NONE',  ( 56.85281608942280229, -50.03689262213919875, -52.32211952640530228 ) ) ;
#10447 = AXIS2_PLACEMENT_3D ( 'NONE', #14348, #15129, #11203 ) ;
#10448 = ORIENTED_EDGE ( 'NONE', *, *, #10867, .T. ) ;
#10449 = CARTESIAN_POINT ( 'NONE',  ( 22.30993167481387829, -10.65456815221859976, -33.57690324825782113 ) ) ;
#10450 = CARTESIAN_POINT ( 'NONE',  ( 68.13393739769706769, 17.98087126524489321, -74.20351669811762463 ) ) ;
#10451 = ORIENTED_EDGE ( 'NONE', *, *, #8533, .F. ) ;
#10452 = CARTESIAN_POINT ( 'NONE',  ( 29.11900864776890074, -26.73446727828369873, -35.02873218748179340 ) ) ;
#10453 = CARTESIAN_POINT ( 'NONE',  ( 4.133937397696209715, -22.54439217495480108, -47.64999999999999858 ) ) ;
#10454 = EDGE_CURVE ( 'NONE', #47128, #8235, #7614, .T. ) ;
#10455 = CARTESIAN_POINT ( 'NONE',  ( 10.15194052115590040, -10.53657666019890016, -47.23658468316739345 ) ) ;
#10456 = CARTESIAN_POINT ( 'NONE',  ( 12.94104881845139943, -50.63124966762359946, -21.36191658295230411 ) ) ;
#10457 = CARTESIAN_POINT ( 'NONE',  ( 55.79982945748940182, 19.45001043779030070, -75.57654528039118702 ) ) ;
#10458 = B_SPLINE_CURVE_WITH_KNOTS ( 'NONE', 3,
 ( #1739, #11160, #46815, #46555, #50984, #3811, #19526, #6970, #10645, #38689, #2775, #19008, #7746, #22669 ),
 .UNSPECIFIED., .F., .F.,
 ( 4, 2, 2, 2, 2, 2, 4 ),
 ( -0.1848816165265140254, -0.1844538286700970198, -0.1648065685561440064, -0.1461169962912039766, -0.1247799312927769938, -0.1076800599504059985, -0.09475412375652510211 ),
 .UNSPECIFIED. ) ;
#10459 = CARTESIAN_POINT ( 'NONE',  ( 47.51349502337109953, -54.40873673668700405, -74.95072482230889932 ) ) ;
#10460 = CARTESIAN_POINT ( 'NONE',  ( 56.63496331945069784, 14.03594713436370078, -17.14577433238509840 ) ) ;
#10461 = CARTESIAN_POINT ( 'NONE',  ( 22.90093739416913721, -14.73039380284950539, -78.41115054280928121 ) ) ;
#10462 = CARTESIAN_POINT ( 'NONE',  ( 82.24885268122095283, 13.88381105532070059, -46.39515304430425147 ) ) ;
#10463 = CARTESIAN_POINT ( 'NONE',  ( 16.44143166354569630, -22.66232309404950129, -47.33329750477099651 ) ) ;
#10464 = CARTESIAN_POINT ( 'NONE',  ( 15.59821405493169877, -8.583724250529140676, -44.32297812435340489 ) ) ;
#10465 = VERTEX_POINT ( 'NONE', #27093 ) ;
#10466 = VECTOR ( 'NONE', #11296, 1000.000000000000000 ) ;
#10467 = CARTESIAN_POINT ( 'NONE',  ( 46.52265252981779753, 21.89525509478169951, -76.13729948142909620 ) ) ;
#10468 = CARTESIAN_POINT ( 'NONE',  ( 64.82166782235130142, 0.9254905997697669973, -60.64710470602509673 ) ) ;
#10469 = B_SPLINE_CURVE_WITH_KNOTS ( 'NONE', 3,
 ( #32297, #36764, #4540, #23921, #39944, #40963, #36249, #20001, #35996, #16085, #4286, #48066, #20259, #360, #16341, #20513, #24693, #44638 ),
 .UNSPECIFIED., .F., .F.,
 ( 4, 2, 2, 2, 2, 2, 2, 2, 4 ),
 ( 0.000000000000000000, 0.06249995567227221299, 0.1249999113445444260, 0.1874998670168166459, 0.2499998226890888520, 0.3124997783613610580, 0.3749997340336332918, 0.4374996897059054701, 0.4999996453781777039 ),
 .UNSPECIFIED. ) ;
#10470 = CARTESIAN_POINT ( 'NONE',  ( 12.14990001803155550, -8.703612571396122988, -50.84100084934565444 ) ) ;
#10471 = CARTESIAN_POINT ( 'NONE',  ( 20.63393739769599833, 10.38381105532070059, -54.64999999999999858 ) ) ;
#10472 = CARTESIAN_POINT ( 'NONE',  ( 29.02733844998730106, -4.531842835453759655, -34.83948955561429983 ) ) ;
#10473 = DIRECTION ( 'NONE',  ( 1.000000000000000000, 0.000000000000000000, 0.000000000000000000 ) ) ;
#10474 = EDGE_CURVE ( 'NONE', #33592, #51185, #34678, .T. ) ;
#10475 = CARTESIAN_POINT ( 'NONE',  ( 82.13853704237929776, 14.41618746881323965, -47.73077426926469968 ) ) ;
#10476 = CARTESIAN_POINT ( 'NONE',  ( -9.348116653862801329, 14.36157061842440008, -43.27560221459960133 ) ) ;
#10478 = CARTESIAN_POINT ( 'NONE',  ( 43.23834971915461978, -38.99408868500810854, -74.22024637953136050 ) ) ;
#10477 = CARTESIAN_POINT ( 'NONE',  ( 52.66500432174891699, 18.87072468935784642, -77.26040935145131527 ) ) ;
#10479 = AXIS2_PLACEMENT_3D ( 'NONE', #45794, #37924, #30299 ) ;
#10480 = CARTESIAN_POINT ( 'NONE',  ( 11.35667226720235057, -21.95685860877812701, -32.49793281473952788 ) ) ;
#10481 = CARTESIAN_POINT ( 'NONE',  ( 20.11805868952936294, -8.703659767395480529, -69.17433723350387709 ) ) ;
#10482 = CARTESIAN_POINT ( 'NONE',  ( -17.94291051752509958, 20.26287486693599860, -52.69725456403749320 ) ) ;
#10483 = ORIENTED_EDGE ( 'NONE', *, *, #50004, .T. ) ;
#10484 = CARTESIAN_POINT ( 'NONE',  ( 52.94725100682300223, -49.60502802665939726, -48.86448480421770313 ) ) ;
#10485 = ORIENTED_EDGE ( 'NONE', *, *, #47406, .T. ) ;
#10486 = CARTESIAN_POINT ( 'NONE',  ( 45.21445506089588662, 8.926488757556171549, -60.31552598061868764 ) ) ;
#10487 = CARTESIAN_POINT ( 'NONE',  ( 17.16956942387501783, -23.52717687085633713, -74.25066484796637667 ) ) ;
#10488 = CARTESIAN_POINT ( 'NONE',  ( 13.95360802883759987, 19.96225614441449991, -22.78639309220759657 ) ) ;
#10489 = CARTESIAN_POINT ( 'NONE',  ( 56.78892056362640517, 14.01480988326609811, -25.36526022269899983 ) ) ;
#10490 = CARTESIAN_POINT ( 'NONE',  ( 20.93696492682870058, -10.45155098534270088, -44.19127752167009504 ) ) ;
#10491 = CARTESIAN_POINT ( 'NONE',  ( -3.366062602303800055, -15.61618894467929941, -44.64999999999999858 ) ) ;
#10492 = CARTESIAN_POINT ( 'NONE',  ( 53.58092488844219758, 18.16693936222939953, -49.20716744093490291 ) ) ;
#10493 = CARTESIAN_POINT ( 'NONE',  ( 55.62883302160090437, -45.78101872142640616, -16.58062561592149819 ) ) ;
#10494 = CYLINDRICAL_SURFACE ( 'NONE', #2099, 2.999999999999942712 ) ;
#10495 = ORIENTED_EDGE ( 'NONE', *, *, #8515, .T. ) ;
#10496 = CARTESIAN_POINT ( 'NONE',  ( 23.79519762219460333, -13.91564786734519998, -39.21797875520189791 ) ) ;
#10497 = EDGE_CURVE ( 'NONE', #32691, #16071, #48542, .T. ) ;
#10498 = CARTESIAN_POINT ( 'NONE',  ( 73.01385068780759013, 0.9098571636355680115, -69.14090909090950277 ) ) ;
#10499 = CARTESIAN_POINT ( 'NONE',  ( 9.984444803807511093, 33.07180274346050197, -46.65389492738129462 ) ) ;
#10500 = CARTESIAN_POINT ( 'NONE',  ( 73.13683269167120216, 0.9254905997697669973, -62.33773042465509917 ) ) ;
#10501 = CARTESIAN_POINT ( 'NONE',  ( 6.365687397696198957, -15.61618894467929941, -18.08174999999999955 ) ) ;
#10502 = CARTESIAN_POINT ( 'NONE',  ( 14.13393739769619906, -32.62399965035220362, -35.14999999999999858 ) ) ;
#10503 = CARTESIAN_POINT ( 'NONE',  ( 11.25620920242847234, -21.92965579961755296, -76.50142983389866913 ) ) ;
#10504 = CARTESIAN_POINT ( 'NONE',  ( 15.24822751835945489, -8.849178269573220845, -57.91115341978882469 ) ) ;
#10505 = ORIENTED_EDGE ( 'NONE', *, *, #31267, .T. ) ;
#10506 = CARTESIAN_POINT ( 'NONE',  ( 64.75883903758510485, 0.9989215084294049696, -70.60223669534690316 ) ) ;
#10507 = VERTEX_POINT ( 'NONE', #15311 ) ;
#10508 = CIRCLE ( 'NONE', #3022, 2.999999999999999112 ) ;
#10509 = CARTESIAN_POINT ( 'NONE',  ( 10.49276773230469928, -63.30748148486130589, -45.62583636195460457 ) ) ;
#10510 = CARTESIAN_POINT ( 'NONE',  ( 22.14986259033789651, -18.71508664667078747, -32.60422815991633172 ) ) ;
#10511 = ORIENTED_EDGE ( 'NONE', *, *, #36196, .T. ) ;
#10512 = PLANE ( 'NONE',  #30856 ) ;
#10513 = FACE_OUTER_BOUND ( 'NONE', #44871, .T. ) ;
#10514 = CARTESIAN_POINT ( 'NONE',  ( 52.78679726808729811, 19.08802767016269897, -76.98734330701118722 ) ) ;
#10515 = ORIENTED_EDGE ( 'NONE', *, *, #28540, .T. ) ;
#10516 = DIRECTION ( 'NONE',  ( 2.867428237999167073E-28, -3.637457002807960330E-11, -1.000000000000000000 ) ) ;
#10517 = LINE ( 'NONE', #38292, #4983 ) ;
#10518 = DIRECTION ( 'NONE',  ( 0.000000000000000000, 0.000000000000000000, -1.000000000000000000 ) ) ;
#10519 = CARTESIAN_POINT ( 'NONE',  ( 20.11804697652824814, -8.703652762251346431, -69.45900026522410542 ) ) ;
#10520 = EDGE_CURVE ( 'NONE', #28130, #42929, #6442, .T. ) ;
#10521 = B_SPLINE_SURFACE_WITH_KNOTS ( 'NONE', 3, 3, ( 
 ( #34331, #35112, #6844, #30660, #46684, #10252 ),
 ( #46943, #50348, #6576, #30403, #26997, #43003 ),
 ( #51112, #46165, #10771, #22539, #22793, #38813 ),
 ( #18874, #31170, #19133, #50080, #26211, #34596 ),
 ( #6321, #7100, #14433, #27246, #47197, #22018 ),
 ( #18104, #38030, #34071, #11284, #2649, #34857 ),
 ( #18353, #50856, #38550, #23051, #26729, #46425 ),
 ( #22278, #11029, #42747, #26470, #39072, #14949 ),
 ( #43262, #2123, #14175, #38288, #18618, #2378 ),
 ( #50601, #19650, #21121, #44019, #6, #15983 ),
 ( #25034, #32902, #35643, #27767, #15722, #13033 ),
 ( #51628, #4178, #49192, #37123, #1219, #47958 ),
 ( #15472, #28986, #23298, #39319, #43509, #11545 ),
 ( #31937, #31423, #44985, #5165, #9086, #31679 ),
 ( #36858, #47702, #35891, #41053, #12061, #3680 ),
 ( #17210, #28012, #8121, #33170, #3423, #24066 ) ),
 .UNSPECIFIED., .F., .F., .F.,
 ( 4, 2, 2, 2, 2, 2, 2, 4 ),
 ( 4, 1, 1, 4 ),
 ( 0.2986826642956370015, 0.3113669960630360278, 0.6672149915636490514, 0.8896199887515309213, 1.000822487345470080, 1.178746485095780061, 1.463424881496269814, 1.779239977503060066 ),
 ( 0.000000000000000000, 0.3333333333333329818, 0.6666666666666670737, 1.000000000000000000 ),
 .UNSPECIFIED. ) ;
#10522 = CARTESIAN_POINT ( 'NONE',  ( 21.79099334230729923, -9.617819324901351052, -59.53301288856840046 ) ) ;
#10523 = ADVANCED_FACE ( 'NONE', ( #38908 ), #18020, .T. ) ;
#10524 = CARTESIAN_POINT ( 'NONE',  ( 8.222734977135019108, -15.61599928274970139, -66.79233150823698395 ) ) ;
#10525 = CARTESIAN_POINT ( 'NONE',  ( 45.05447910683652424, -38.04890345680490782, -65.04729142848933066 ) ) ;
#10526 = EDGE_LOOP ( 'NONE', ( #3326, #33878, #43112, #7132 ) ) ;
#10527 = CARTESIAN_POINT ( 'NONE',  ( 0.1155611319282749960, -51.17475502668380472, -35.14999999933320396 ) ) ;
#10528 = CARTESIAN_POINT ( 'NONE',  ( 22.65619759003989842, -12.01524243181439999, -58.07208434834339528 ) ) ;
#10529 = CARTESIAN_POINT ( 'NONE',  ( 9.300370600410550637, -13.57546037233679925, -32.14999999999999858 ) ) ;
#10530 = CARTESIAN_POINT ( 'NONE',  ( 9.366403394718119557, -15.61612932825470068, -61.45282021618999124 ) ) ;
#10531 = CARTESIAN_POINT ( 'NONE',  ( 13.50448204009659925, 20.38750180725810068, -74.54610039094001195 ) ) ;
#10532 = CYLINDRICAL_SURFACE ( 'NONE', #2227, 2.000000000000040856 ) ;
#10533 = EDGE_CURVE ( 'NONE', #9855, #9438, #47893, .T. ) ;
#10534 = CARTESIAN_POINT ( 'NONE',  ( 41.12837288530710111, -45.19325662561399781, -5.806229973785479892 ) ) ;
#10535 = CARTESIAN_POINT ( 'NONE',  ( 16.97276188636949712, 12.56821928479469896, -59.64999999999999147 ) ) ;
#10536 = CIRCLE ( 'NONE', #40632, 0.4934432872204244647 ) ;
#10537 = CARTESIAN_POINT ( 'NONE',  ( 8.923001793905660506, -11.61804832347029937, -60.66881518290298914 ) ) ;
#10538 = EDGE_CURVE ( 'NONE', #1610, #22194, #26610, .T. ) ;
#10539 = ORIENTED_EDGE ( 'NONE', *, *, #34824, .T. ) ;
#10540 = CARTESIAN_POINT ( 'NONE',  ( 53.34500566076300032, -49.01310193610019894, -26.65466145037910195 ) ) ;
#10541 = AXIS2_PLACEMENT_3D ( 'NONE', #33202, #32668, #49220 ) ;
#10542 = CARTESIAN_POINT ( 'NONE',  ( 55.66015518744840307, -50.79683962258500429, -75.28107449616210545 ) ) ;
#10544 = CARTESIAN_POINT ( 'NONE',  ( 41.57151345658783015, -39.71737154464926789, -78.39838314987487422 ) ) ;
#10543 = CARTESIAN_POINT ( 'NONE',  ( 12.28762636745939929, 33.23782178623170580, -15.69519614581730060 ) ) ;
#10545 = CARTESIAN_POINT ( 'NONE',  ( 29.99034385824719706, -15.61618894467929941, -32.14999999999999858 ) ) ;
#10546 = PLANE ( 'NONE',  #26506 ) ;
#10547 = VERTEX_POINT ( 'NONE', #38236 ) ;
#10548 = CARTESIAN_POINT ( 'NONE',  ( -6.924872749838059782, -45.82389030641969896, -4.775471299587530360 ) ) ;
#10549 = CARTESIAN_POINT ( 'NONE',  ( 47.50940371821619834, 23.35937273273760084, -54.84160031900390209 ) ) ;
#10550 = CYLINDRICAL_SURFACE ( 'NONE', #44622, 1.999999999999997335 ) ;
#10551 = CARTESIAN_POINT ( 'NONE',  ( 63.25409997666370288, 1.100585178971990041, -62.22139992353060478 ) ) ;
#10552 = CARTESIAN_POINT ( 'NONE',  ( 57.48608977619462479, 13.88381019371527358, -25.33088771662052352 ) ) ;
#10553 = CARTESIAN_POINT ( 'NONE',  ( 11.63839622733459933, 33.75269855431290011, -16.51998659929800084 ) ) ;
#10554 = CARTESIAN_POINT ( 'NONE',  ( 51.79630865696839948, 18.05475250901589845, -76.98491570867250289 ) ) ;
#10555 = CARTESIAN_POINT ( 'NONE',  ( 52.86217581337979965, 18.41155708171960015, -48.67083718181420693 ) ) ;
#10556 = CARTESIAN_POINT ( 'NONE',  ( 19.36032775985367138, 24.25318110953120510, -75.71503644620106854 ) ) ;
#10557 = CARTESIAN_POINT ( 'NONE',  ( 16.13393739769620083, -15.61618894467929941, -15.76422791930239953 ) ) ;
#10558 = CARTESIAN_POINT ( 'NONE',  ( 56.55526382498660354, 14.97959948432539967, -26.26696731187869815 ) ) ;
#10559 = CARTESIAN_POINT ( 'NONE',  ( 49.93953522581040261, 22.20567224523410133, -54.35118285553540574 ) ) ;
#10560 = CARTESIAN_POINT ( 'NONE',  ( 8.222412332301150428, -15.61630761206940043, -38.79233150823699816 ) ) ;
#10561 = CARTESIAN_POINT ( 'NONE',  ( 52.56521937542130019, 18.62941943741099848, -48.47378147059570352 ) ) ;
#10562 = CARTESIAN_POINT ( 'NONE',  ( 60.34831028877889736, -45.11618894467940066, -11.22201639935360085 ) ) ;
#10563 = CARTESIAN_POINT ( 'NONE',  ( 71.07527734533519492, 1.384447124000270035, -60.97624892474630087 ) ) ;
#10564 = CARTESIAN_POINT ( 'NONE',  ( 10.97767197991529997, 31.88305279702909800, -44.74312619248830458 ) ) ;
#10565 = CARTESIAN_POINT ( 'NONE',  ( 72.83816022157699877, 1.310552739454540205, -62.22324284883860201 ) ) ;
#10566 = AXIS2_PLACEMENT_3D ( 'NONE', #42510, #6596, #18306 ) ;
#10567 = CARTESIAN_POINT ( 'NONE',  ( 16.13393739769620083, -15.61618894467929941, -10.44999999999999929 ) ) ;
#10568 = B_SPLINE_CURVE_WITH_KNOTS ( 'NONE', 3,
 ( #23873, #311, #19453, #68, #23618, #8181, #31735, #35439, #31484, #11868, #39382, #31996, #19192, #15782, #24123, #47509, #23111, #48270 ),
 .UNSPECIFIED., .F., .F.,
 ( 4, 2, 2, 2, 2, 2, 2, 2, 4 ),
 ( 0.4999998584714454020, 0.5624998761625147337, 0.6249998938535841209, 0.6874999115446533970, 0.7499999292357226732, 0.8124999469267920604, 0.8749999646178614476, 0.9374999823089307238, 1.000000000000000000 ),
 .UNSPECIFIED. ) ;
#10569 = VECTOR ( 'NONE', #23462, 1000.000000000000000 ) ;
#10570 = CARTESIAN_POINT ( 'NONE',  ( 12.65210637300620533, 24.23198390231812027, -75.47957398526430950 ) ) ;
#10571 = ORIENTED_EDGE ( 'NONE', *, *, #40387, .T. ) ;
#10572 = VERTEX_POINT ( 'NONE', #34274 ) ;
#10573 = DIRECTION ( 'NONE',  ( -1.000000000000000000, 0.000000000000000000, 0.000000000000000000 ) ) ;
#10574 = CARTESIAN_POINT ( 'NONE',  ( 76.80229243761525026, 9.607667892824617084, -14.53004134039231054 ) ) ;
#10575 = B_SPLINE_CURVE_WITH_KNOTS ( 'NONE', 3,
 ( #50066, #46150, #14161, #29360, #38272, #26197, #17070, #13402, #13153, #33022, #29103, #42208, #49568, #17831, #37755, #38014, #41420, #49047, #25933, #45101, #5279, #25418, #9208, #1593, #25160, #21230, #5538, #17328, #33291, #6047, #21493, #17581, #1853, #33551, #29615, #45618, #25677, #41679 ),
 .UNSPECIFIED., .F., .F.,
 ( 4, 2, 1, 1, 1, 1, 2, 2, 2, 2, 2, 2, 2, 2, 2, 2, 2, 2, 2, 2, 4 ),
 ( 0.5000031186356694857, 0.5004913968401268898, 0.5009796750445841829, 0.5019562314534988801, 0.5039093442713282744, 0.5078155699069871742, 0.5156280211783047518, 0.5312529237209401289, 0.5625027288062107722, 0.6250023389767520587, 0.6875019491472932343, 0.7187517542325639885, 0.7500015593178346318, 0.7812513644031052751, 0.8125011694883760294, 0.8437509745736466726, 0.8750007796589173159, 0.9062505847441879592, 0.9375003898294587135, 0.9687501949147294678, 1.000000000000000000 ),
 .UNSPECIFIED. ) ;
#10576 = ORIENTED_EDGE ( 'NONE', *, *, #50096, .T. ) ;
#10577 = CARTESIAN_POINT ( 'NONE',  ( 12.87764532066540113, -65.50708823514179358, -47.55684977079440046 ) ) ;
#10578 = CARTESIAN_POINT ( 'NONE',  ( 57.19388132582110273, -45.22028251464379878, -25.72059501569479778 ) ) ;
#10579 = CARTESIAN_POINT ( 'NONE',  ( 10.72257032501696727, -19.77479894534321403, -45.24450163928270996 ) ) ;
#10580 = FACE_OUTER_BOUND ( 'NONE', #23945, .T. ) ;
#10581 = EDGE_LOOP ( 'NONE', ( #23735, #51053, #1152 ) ) ;
#10582 = DIRECTION ( 'NONE',  ( 0.006865953067580490843, 0.7399621225138561798, -0.6726134966927608261 ) ) ;
#10583 = CARTESIAN_POINT ( 'NONE',  ( 45.75929793348244345, 6.895754709389400716, -61.52319716619024348 ) ) ;
#10584 = AXIS2_PLACEMENT_3D ( 'NONE', #30877, #27212, #51340 ) ;
#10585 = CARTESIAN_POINT ( 'NONE',  ( 10.64863409883700029, 32.21085600226960111, -23.66469670114080159 ) ) ;
#10586 = ORIENTED_EDGE ( 'NONE', *, *, #23622, .T. ) ;
#10587 = CARTESIAN_POINT ( 'NONE',  ( 9.211626495204299658, -11.13686624773779954, -34.97514425884639877 ) ) ;
#10588 = EDGE_CURVE ( 'NONE', #17098, #50522, #45981, .T. ) ;
#10589 = CARTESIAN_POINT ( 'NONE',  ( 9.205734167420709824, -3.616188944679339823, -32.14999999999999858 ) ) ;
#10590 = CARTESIAN_POINT ( 'NONE',  ( 14.24082757525529885, 19.87036215778640269, -22.22799665057820206 ) ) ;
#10591 =( LENGTH_UNIT ( ) NAMED_UNIT ( * ) SI_UNIT ( .MILLI., .METRE. ) );
#10592 = EDGE_CURVE ( 'NONE', #30733, #2407, #2594, .T. ) ;
#10593 = CARTESIAN_POINT ( 'NONE',  ( 16.14884424877395830, -22.38317489321702070, -46.95212254701444721 ) ) ;
#10594 = FACE_OUTER_BOUND ( 'NONE', #46496, .T. ) ;
#10595 = CARTESIAN_POINT ( 'NONE',  ( 47.35703446467029210, -54.65209995708080015, -74.50157339271500234 ) ) ;
#10596 = CARTESIAN_POINT ( 'NONE',  ( 83.63329919740728258, -44.53040215208500996, -46.55718455497714103 ) ) ;
#10597 = DIRECTION ( 'NONE',  ( 0.000000000000000000, 0.000000000000000000, -1.000000000000000000 ) ) ;
#10599 = VECTOR ( 'NONE', #43606, 1000.000000000000000 ) ;
#10598 = CARTESIAN_POINT ( 'NONE',  ( 51.98443725223810219, 20.13520455629999972, -75.98853295767520422 ) ) ;
#10600 = CARTESIAN_POINT ( 'NONE',  ( 65.30823856897173130, -30.98971297456273177, -16.78605249253913811 ) ) ;
#10601 = CARTESIAN_POINT ( 'NONE',  ( 8.668407554846540464, -19.11598675061409836, -34.36813006978140095 ) ) ;
#10602 = ADVANCED_FACE ( 'NONE', ( #50030 ), #10200, .T. ) ;
#10603 = ORIENTED_EDGE ( 'NONE', *, *, #291, .T. ) ;
#10604 = CARTESIAN_POINT ( 'NONE',  ( 22.90020510100978157, -14.99288303432257052, -48.81786394348062430 ) ) ;
#10605 = CARTESIAN_POINT ( 'NONE',  ( -4.080334501795739754, -49.41737491467630150, -7.291472505024230166 ) ) ;
#10606 = CARTESIAN_POINT ( 'NONE',  ( 76.51282310243020390, -29.88146092617099825, -13.28268384058759999 ) ) ;
#10607 = DIRECTION ( 'NONE',  ( 0.000000000000000000, 3.054848041326975067E-12, -1.000000000000000000 ) ) ;
#10608 = CARTESIAN_POINT ( 'NONE',  ( 71.54045699608269615, 0.8986939045430379913, -60.71074964625670134 ) ) ;
#10609 = CARTESIAN_POINT ( 'NONE',  ( 19.93042841486727923, -55.43540767232475730, -75.02878472486347050 ) ) ;
#10610 = CARTESIAN_POINT ( 'NONE',  ( 12.95491128060830022, 18.65448050664010182, -82.14319696191608955 ) ) ;
#10611 = CIRCLE ( 'NONE', #48234, 6.000000000000005329 ) ;
#10612 = DIRECTION ( 'NONE',  ( 0.000000000000000000, 0.000000000000000000, -1.000000000000000000 ) ) ;
#10613 = CARTESIAN_POINT ( 'NONE',  ( 72.33393739769618946, 1.883811055320669947, -68.84999999999999432 ) ) ;
#10614 = CARTESIAN_POINT ( 'NONE',  ( 41.85352073560179775, 12.59900291848219922, -4.272019243654880505 ) ) ;
#10615 = CARTESIAN_POINT ( 'NONE',  ( 47.64143404728118014, -54.53488714831495798, -74.17417149932109055 ) ) ;
#10616 = CARTESIAN_POINT ( 'NONE',  ( 9.895190454276159286, -53.60841447722820163, -34.64999999999999858 ) ) ;
#10617 = AXIS2_PLACEMENT_3D ( 'NONE', #15494, #23578, #22815 ) ;
#10618 = CARTESIAN_POINT ( 'NONE',  ( 57.55751162087899786, 18.85811933572220056, -52.57651812407429759 ) ) ;
#10619 = CARTESIAN_POINT ( 'NONE',  ( 75.97446932798683861, -43.32575349481732019, -13.61806422801180005 ) ) ;
#10620 = CARTESIAN_POINT ( 'NONE',  ( 18.02758775305530037, -52.17195122215589720, -75.81086730487160708 ) ) ;
#10621 = CARTESIAN_POINT ( 'NONE',  ( 52.30020358789180079, -52.26933069182599212, -53.48872967491809760 ) ) ;
#10622 = ORIENTED_EDGE ( 'NONE', *, *, #50099, .T. ) ;
#10623 = CARTESIAN_POINT ( 'NONE',  ( 21.73894157828249973, -20.52440883318790199, -49.29627689082150255 ) ) ;
#10624 = CARTESIAN_POINT ( 'NONE',  ( 63.75661388851530376, 1.112168069084249922, -61.55316875389540598 ) ) ;
#10625 = VERTEX_POINT ( 'NONE', #41641 ) ;
#10626 = CARTESIAN_POINT ( 'NONE',  ( 20.29258866489369595, -21.02752359692314243, -68.74448518055469037 ) ) ;
#10627 = FACE_OUTER_BOUND ( 'NONE', #6353, .T. ) ;
#10628 = DIRECTION ( 'NONE',  ( 0.8090169943749457859, 0.5877852522924753575, 0.000000000000000000 ) ) ;
#10629 = CARTESIAN_POINT ( 'NONE',  ( 45.75938509646260854, 8.847270729488906582, -58.12753028167146141 ) ) ;
#10630 = CARTESIAN_POINT ( 'NONE',  ( 10.83684432477319959, -19.82762902495380075, -81.23899999999999011 ) ) ;
#10631 = CARTESIAN_POINT ( 'NONE',  ( 41.30043219516269914, -45.59471617425819545, -6.243955610188449690 ) ) ;
#10632 = ORIENTED_EDGE ( 'NONE', *, *, #37930, .T. ) ;
#10633 = EDGE_LOOP ( 'NONE', ( #38717, #12669, #42907, #35563, #5110 ) ) ;
#10634 = TOROIDAL_SURFACE ( 'NONE', #580, 16.60961179679779676, 0.5000000000000000000 ) ;
#10635 = ORIENTED_EDGE ( 'NONE', *, *, #2069, .T. ) ;
#10636 = DIRECTION ( 'NONE',  ( 0.01091231665325478536, -0.06889765579810422369, -0.9975640502598241977 ) ) ;
#10637 = CARTESIAN_POINT ( 'NONE',  ( 61.24171035206370561, -45.28669213153539630, -47.00360896229330621 ) ) ;
#10638 = DIRECTION ( 'NONE',  ( 0.000000000000000000, -1.000000000000000000, 0.000000000000000000 ) ) ;
#10639 = CARTESIAN_POINT ( 'NONE',  ( 82.71777775636080321, -45.49271782872658321, -47.55444199374405656 ) ) ;
#10640 = CIRCLE ( 'NONE', #46633, 6.100000000000001421 ) ;
#10641 = ORIENTED_EDGE ( 'NONE', *, *, #25470, .F. ) ;
#10642 = VERTEX_POINT ( 'NONE', #5750 ) ;
#10643 = DIRECTION ( 'NONE',  ( 0.000000000000000000, 0.000000000000000000, 1.000000000000000000 ) ) ;
#10644 = ADVANCED_FACE ( 'NONE', ( #26159 ), #45846, .T. ) ;
#10645 = CARTESIAN_POINT ( 'NONE',  ( 45.20352061843870217, -33.45237892079950370, -34.80811307016849554 ) ) ;
#10646 = ORIENTED_EDGE ( 'NONE', *, *, #21525, .F. ) ;
#10647 = DIRECTION ( 'NONE',  ( 1.000000000000000000, 0.000000000000000000, 0.000000000000000000 ) ) ;
#10648 = CARTESIAN_POINT ( 'NONE',  ( 51.83018430297099854, -50.77522728973830368, -76.24313691376478630 ) ) ;
#10649 = CARTESIAN_POINT ( 'NONE',  ( 60.58781920018089551, 14.36667126140370065, -47.22968683208149088 ) ) ;
#10650 = B_SPLINE_CURVE_WITH_KNOTS ( 'NONE', 3,
 ( #9900, #25857, #50517, #14608, #23219, #30575, #46856, #34238 ),
 .UNSPECIFIED., .F., .F.,
 ( 4, 2, 2, 4 ),
 ( 0.05028014561811239985, 0.06097673919894460587, 0.07774712209420850395, 0.08013618654967340216 ),
 .UNSPECIFIED. ) ;
#10651 = DIRECTION ( 'NONE',  ( 0.000000000000000000, 0.000000000000000000, -1.000000000000000000 ) ) ;
#10652 = CARTESIAN_POINT ( 'NONE',  ( 42.87450601165679842, -42.77519057968400062, -3.882344406266829751 ) ) ;
#10653 = CARTESIAN_POINT ( 'NONE',  ( 65.17764324051411506, 0.4654656955129265472, -17.21758742400660580 ) ) ;
#10654 = CARTESIAN_POINT ( 'NONE',  ( -21.36606260230379917, -53.11618894467930119, 11.84999999999999964 ) ) ;
#10655 = CARTESIAN_POINT ( 'NONE',  ( 64.84151977724279448, 1.394090247237909974, -70.24155908324229358 ) ) ;
#10656 = CARTESIAN_POINT ( 'NONE',  ( -18.86606260230360022, -50.61618894467959962, 16.85000000000000142 ) ) ;
#10657 = CARTESIAN_POINT ( 'NONE',  ( 11.63393739769602320, 10.38381105532059934, -35.01561944896759826 ) ) ;
#10658 = CARTESIAN_POINT ( 'NONE',  ( 10.40061235411570095, -10.25748274562010032, -52.52675917389010607 ) ) ;
#10659 = EDGE_CURVE ( 'NONE', #15707, #11818, #34135, .T. ) ;
#10660 = ORIENTED_EDGE ( 'NONE', *, *, #18802, .F. ) ;
#10661 = CARTESIAN_POINT ( 'NONE',  ( 14.95914443809330052, -52.95108609461500748, -76.14999999999999147 ) ) ;
#10662 = CARTESIAN_POINT ( 'NONE',  ( 57.48430709216129486, 19.22299575600860067, -53.13654412953230377 ) ) ;
#10663 = EDGE_CURVE ( 'NONE', #27942, #49694, #11498, .T. ) ;
#10664 = CARTESIAN_POINT ( 'NONE',  ( 71.86857605226019530, 1.394112346783849876, -70.08832560374550269 ) ) ;
#10665 = CARTESIAN_POINT ( 'NONE',  ( 44.85304072945612575, -40.02002747739808797, -62.52602019059866478 ) ) ;
#10666 = CARTESIAN_POINT ( 'NONE',  ( 11.67619942398430055, 33.65927571709689659, -45.08494251881550241 ) ) ;
#10667 =( BOUNDED_CURVE ( )  B_SPLINE_CURVE ( 3, ( #20068, #36309, #9070, #16663 ),
 .UNSPECIFIED., .F., .T. ) 
 B_SPLINE_CURVE_WITH_KNOTS ( ( 4, 4 ),
 ( 0.3056162491274368453, 0.3752708228560562298 ),
 .UNSPECIFIED. ) 
 CURVE ( )  GEOMETRIC_REPRESENTATION_ITEM ( )  RATIONAL_B_SPLINE_CURVE ( ( 1.000000000000000000, 0.9995957275622165961, 0.9995957275622165961, 1.000000000000000000 ) ) 
 REPRESENTATION_ITEM ( '' )  );
#10668 = DIRECTION ( 'NONE',  ( 0.3294064756440788777, -0.9441882088883267743, 0.000000000000000000 ) ) ;
#10669 = FACE_OUTER_BOUND ( 'NONE', #7113, .T. ) ;
#10670 = CARTESIAN_POINT ( 'NONE',  ( 47.75973331525239729, -54.48449617083259966, -55.18290192981469744 ) ) ;
#10671 = CARTESIAN_POINT ( 'NONE',  ( 24.03409986133361187, -15.19376807180136346, -45.49067444776833469 ) ) ;
#10672 = CARTESIAN_POINT ( 'NONE',  ( -5.673894890943248726, -46.74181062968316525, -4.529014140242093589 ) ) ;
#10673 = CARTESIAN_POINT ( 'NONE',  ( 48.07327434400980337, 23.08200056603829964, -54.91761349180919893 ) ) ;
#10674 = EDGE_LOOP ( 'NONE', ( #21833, #6180 ) ) ;
#10675 = CARTESIAN_POINT ( 'NONE',  ( 21.66930937907060084, -19.98679716348209823, -75.05992337703780493 ) ) ;
#10676 = ORIENTED_EDGE ( 'NONE', *, *, #33262, .T. ) ;
#10678 = CARTESIAN_POINT ( 'NONE',  ( 71.48855272380100701, 0.8936201581567889685, -70.62461353540280129 ) ) ;
#10677 = B_SPLINE_SURFACE_WITH_KNOTS ( 'NONE', 3, 3, ( 
 ( #15761, #31714, #43801, #23848, #4473, #32740, #36430, #48768, #538, #28567, #12342, #12095, #16524, #21218 ),
 ( #24363, #28050, #4216, #20190, #32473, #25148, #40123, #37229, #47995, #16272, #40892, #28828, #41152, #36180 ),
 ( #28306, #36690, #4733, #32225, #24102, #5003, #40634, #1326, #44053, #8416, #44833, #31975, #9196, #45088 ),
 ( #12605, #8938, #287, #40376, #44567, #5266, #20700, #48248, #20442, #8158, #12872, #44307, #791, #33010 ),
 ( #49033, #24881, #13141, #16792, #48503, #29090, #8668, #20963, #24623, #36963, #1061, #17057, #37743, #42461 ),
 ( #34309, #22254, #29349, #6036, #5773, #9706, #49557, #1841, #17819, #26445, #33793, #50055, #37481, #49293 ),
 ( #38261, #41409, #6548, #13644, #21993, #41936, #17570, #9457, #42198, #25921, #38524, #45354, #45607, #14150 ),
 ( #46401, #30376, #38003, #49802, #46138, #5527, #25666, #29853, #10489, #2101, #1581, #21736, #22513, #34045 ),
 ( #18077, #18328, #41668, #50322, #10229, #14408, #30119, #33539, #17314, #33278, #26187, #13391, #6296, #13895 ) ),
 .UNSPECIFIED., .F., .F., .F.,
 ( 4, 1, 1, 1, 1, 1, 4 ),
 ( 4, 2, 2, 2, 2, 2, 4 ),
 ( -1.457552082500000009E-05, 0.1666666666666670182, 0.3333333333333329818, 0.5000000000000000000, 0.6666666666666670737, 0.8333333333333330373, 1.000000000000000000 ),
 ( -0.9973649408979550213, -0.8379246112468560215, -0.6064737235837710516, -0.4618169187943430010, -0.3171601140049140066, -0.03213823312263499460, 0.07935366520894500397 ),
 .UNSPECIFIED. ) ;
#10679 = DIRECTION ( 'NONE',  ( 1.000000000000000000, 0.000000000000000000, 0.000000000000000000 ) ) ;
#10680 = VECTOR ( 'NONE', #8990, 1000.000000000000000 ) ;
#10681 = CARTESIAN_POINT ( 'NONE',  ( 61.13393739769620083, -43.11618894467930119, -84.38499399519520239 ) ) ;
#10683 = CARTESIAN_POINT ( 'NONE',  ( 14.63288374505910028, 0.9265147500385738644, -34.64999999999999858 ) ) ;
#10682 = DIRECTION ( 'NONE',  ( -1.000000000000000000, 0.000000000000000000, 0.000000000000000000 ) ) ;
#10684 = CARTESIAN_POINT ( 'NONE',  ( 16.68233526804289824, -8.584701301767282189, -73.97759560159100545 ) ) ;
#10685 = CARTESIAN_POINT ( 'NONE',  ( 37.33393739769619657, -15.61618894467929941, -10.44999999999999929 ) ) ;
#10686 = CARTESIAN_POINT ( 'NONE',  ( 16.13393739769620083, -1.759782484128330049, -35.14999999999999858 ) ) ;
#10687 = DIRECTION ( 'NONE',  ( 0.000000000000000000, -1.000000000000000000, 0.000000000000000000 ) ) ;
#10688 = ORIENTED_EDGE ( 'NONE', *, *, #16903, .T. ) ;
#10689 = CYLINDRICAL_SURFACE ( 'NONE', #43989, 5.499999999999998224 ) ;
#10690 = ORIENTED_EDGE ( 'NONE', *, *, #16449, .F. ) ;
#10691 = CARTESIAN_POINT ( 'NONE',  ( 12.26572565712860019, -64.61660037486478814, -15.83807272483589834 ) ) ;
#10692 = CARTESIAN_POINT ( 'NONE',  ( 16.13393739769620083, -15.61618894467929941, -35.02873218748179340 ) ) ;
#10693 = DIRECTION ( 'NONE',  ( -0.3863301728269175062, -0.9223605572462019175, 3.330669073875470114E-16 ) ) ;
#10694 = CARTESIAN_POINT ( 'NONE',  ( 10.68300311294020055, -64.60342289521591397, -46.54418054629820034 ) ) ;
#10695 = ORIENTED_EDGE ( 'NONE', *, *, #33201, .T. ) ;
#10696 = VERTEX_POINT ( 'NONE', #19852 ) ;
#10697 = CARTESIAN_POINT ( 'NONE',  ( 71.60705152684150221, 1.024253516290730026, -60.76832953309080665 ) ) ;
#10698 = CARTESIAN_POINT ( 'NONE',  ( 82.35517546691707480, -45.10830561011249529, -46.40108830999478329 ) ) ;
#10699 = CARTESIAN_POINT ( 'NONE',  ( 52.57890812028310279, -49.84736177554090375, -48.49303208760839823 ) ) ;
#10700 = EDGE_CURVE ( 'NONE', #50146, #24819, #15932, .T. ) ;
#10701 = CARTESIAN_POINT ( 'NONE',  ( 52.74869365736800120, 18.89386278705310218, -49.96575957230339782 ) ) ;
#10702 = DIRECTION ( 'NONE',  ( 0.000000000000000000, 1.000000000000000000, 0.000000000000000000 ) ) ;
#10703 = CARTESIAN_POINT ( 'NONE',  ( 50.84617524815230638, -48.84160893671730008, -76.31370213948670767 ) ) ;
#10704 = ADVANCED_FACE ( 'NONE', ( #24015 ), #14268, .T. ) ;
#10705 = CARTESIAN_POINT ( 'NONE',  ( 59.87419911194779587, -46.57917323255409769, -48.56273897241279514 ) ) ;
#10706 = ORIENTED_EDGE ( 'NONE', *, *, #6040, .T. ) ;
#10707 = CYLINDRICAL_SURFACE ( 'NONE', #32469, 6.766999999999998572 ) ;
#10708 = DIRECTION ( 'NONE',  ( 0.1686178020941689892, 0.6660492713794449182, -0.7265992051412129005 ) ) ;
#10709 = ORIENTED_EDGE ( 'NONE', *, *, #22346, .F. ) ;
#10710 = FACE_OUTER_BOUND ( 'NONE', #24595, .T. ) ;
#10711 = DIRECTION ( 'NONE',  ( 0.000000000000000000, 0.000000000000000000, 1.000000000000000000 ) ) ;
#10712 = CARTESIAN_POINT ( 'NONE',  ( 9.073062699144459842, -12.19116396915949885, -39.15625371467830007 ) ) ;
#10713 = CARTESIAN_POINT ( 'NONE',  ( 13.58983010028589966, -51.22113851962519959, -22.27008681093980158 ) ) ;
#10714 = CARTESIAN_POINT ( 'NONE',  ( 47.46038822159390236, -54.33963646450610696, -75.12137911381070410 ) ) ;
#10715 = CARTESIAN_POINT ( 'NONE',  ( 56.29010337146409881, 14.04964247742699968, -16.36031652423400118 ) ) ;
#10716 = CARTESIAN_POINT ( 'NONE',  ( 10.14913760601130122, 32.10609558527020369, -45.99399621147029649 ) ) ;
#10717 = CARTESIAN_POINT ( 'NONE',  ( 56.87125376272950206, -50.65201878316320006, -53.85479923535680058 ) ) ;
#10718 = CIRCLE ( 'NONE', #31593, 34.41780050634729804 ) ;
#10719 = CARTESIAN_POINT ( 'NONE',  ( 22.22400857603370028, -12.05900013647219993, -40.67890729542689598 ) ) ;
#10720 = FACE_OUTER_BOUND ( 'NONE', #33360, .T. ) ;
#10721 = ORIENTED_EDGE ( 'NONE', *, *, #14122, .F. ) ;
#10722 = CARTESIAN_POINT ( 'NONE',  ( 46.88052044270690288, 22.39196474760659683, -75.96172452672209374 ) ) ;
#10723 = AXIS2_PLACEMENT_3D ( 'NONE', #32045, #48067, #28124 ) ;
#10724 = CARTESIAN_POINT ( 'NONE',  ( 64.84489409100200419, 0.9242073871622918935, -60.63177898966700496 ) ) ;
#10725 = EDGE_CURVE ( 'NONE', #6259, #10739, #14757, .T. ) ;
#10726 = CARTESIAN_POINT ( 'NONE',  ( 43.24976358433020351, -46.00069318273389740, -7.760792318163260539 ) ) ;
#10727 = CARTESIAN_POINT ( 'NONE',  ( 17.16957227836324762, -7.705201425624105482, -57.33399802158175618 ) ) ;
#10728 = CARTESIAN_POINT ( 'NONE',  ( 74.93037820153030282, 13.88381105528979909, -15.31096251095349992 ) ) ;
#10729 = DIRECTION ( 'NONE',  ( 0.000000000000000000, -1.000000000000000000, 0.000000000000000000 ) ) ;
#10730 = DIRECTION ( 'NONE',  ( 0.9200120562340469155, 0.3918900565005459247, 8.326672684688669123E-17 ) ) ;
#10731 = LINE ( 'NONE', #26685, #28457 ) ;
#10733 = DIRECTION ( 'NONE',  ( 1.000000000000000000, 0.000000000000000000, 0.000000000000000000 ) ) ;
#10732 = CARTESIAN_POINT ( 'NONE',  ( 52.75990468010462564, 18.93640155443588213, -77.25922080063452313 ) ) ;
#10734 = CARTESIAN_POINT ( 'NONE',  ( 24.04441141871755505, -15.51763852015655054, -71.50370833047819019 ) ) ;
#10735 = CARTESIAN_POINT ( 'NONE',  ( 20.99560978300444702, -9.290019194129630620, -69.21600402986263134 ) ) ;
#10736 = CARTESIAN_POINT ( 'NONE',  ( -0.08095109960242620473, 30.16966275033259848, -48.64221216126279757 ) ) ;
#10737 = ORIENTED_EDGE ( 'NONE', *, *, #5067, .F. ) ;
#10738 = CARTESIAN_POINT ( 'NONE',  ( 52.75620357935920168, -49.71340975552000430, -48.74712242243199967 ) ) ;
#10739 = VERTEX_POINT ( 'NONE', #8845 ) ;
#10740 = CARTESIAN_POINT ( 'NONE',  ( 40.80250930014859279, 8.415445928904281558, -82.01417162886387757 ) ) ;
#10741 = CARTESIAN_POINT ( 'NONE',  ( -21.36606260230379917, -63.11618894467929408, 11.84999999999999964 ) ) ;
#10742 = CARTESIAN_POINT ( 'NONE',  ( 13.61605761131730041, 20.15014681539719987, -22.70458626188970186 ) ) ;
#10743 = CARTESIAN_POINT ( 'NONE',  ( 16.13393739769620083, -15.61618894467929941, -32.14999999999999858 ) ) ;
#10744 = CARTESIAN_POINT ( 'NONE',  ( 21.65517505013649924, -20.00463895372590173, -44.66659110805180433 ) ) ;
#10745 = DIRECTION ( 'NONE',  ( 0.000000000000000000, 0.000000000000000000, -1.000000000000000000 ) ) ;
#10746 = CARTESIAN_POINT ( 'NONE',  ( 53.41300596567459280, 18.22585793593439618, -49.19565812895479695 ) ) ;
#10747 = CARTESIAN_POINT ( 'NONE',  ( 55.40266554404109911, -45.95720592209579536, -16.47441024969080203 ) ) ;
#10748 = LINE ( 'NONE', #50837, #13121 ) ;
#10749 = EDGE_LOOP ( 'NONE', ( #30352, #35044, #17065, #23477 ) ) ;
#10750 = CARTESIAN_POINT ( 'NONE',  ( 8.531823529735639511, -17.56416556716440169, -36.20765937478439866 ) ) ;
#10751 = B_SPLINE_CURVE_WITH_KNOTS ( 'NONE', 3,
 ( #32184, #29050, #41112, #4172, #36387, #48200, #31932, #17016 ),
 .UNSPECIFIED., .F., .F.,
 ( 4, 2, 2, 4 ),
 ( 0.5031119562093512299, 0.6273339671570132836, 0.7515559781046754484, 1.000000000000000000 ),
 .UNSPECIFIED. ) ;
#10752 = B_SPLINE_CURVE_WITH_KNOTS ( 'NONE', 3,
 ( #39666, #3774, #36231, #19740, #35733, #51716 ),
 .UNSPECIFIED., .F., .F.,
 ( 4, 2, 4 ),
 ( 0.2774707949478909530, 0.5953712600656003717, 1.000000000000000000 ),
 .UNSPECIFIED. ) ;
#10753 = CYLINDRICAL_SURFACE ( 'NONE', #35313, 7.910999999999997812 ) ;
#10754 = CARTESIAN_POINT ( 'NONE',  ( 10.75750387234210059, 33.63386303445160053, -46.91033328174970052 ) ) ;
#10755 = CARTESIAN_POINT ( 'NONE',  ( 73.17063711417530669, 1.097895768572089814, -62.46942512468480402 ) ) ;
#10756 = B_SPLINE_CURVE_WITH_KNOTS ( 'NONE', 3,
 ( #564, #12369, #40146, #32251, #12635, #24389, #23620, #51690, #11871, #44080, #48273, #44333, #51439, #39900 ),
 .UNSPECIFIED., .F., .F.,
 ( 4, 2, 2, 2, 2, 2, 4 ),
 ( -8.605215961916560019, -8.065295816869170409, -6.871057665605490250, -6.124658821065700032, -5.378259976525890274, -4.302607981395680348, -4.009099514081210458 ),
 .UNSPECIFIED. ) ;
#10757 = CARTESIAN_POINT ( 'NONE',  ( 11.92216765568469761, -65.43848403456330232, -17.95790456665970325 ) ) ;
#10758 = CARTESIAN_POINT ( 'NONE',  ( 53.36496928958640495, 18.14812949222240235, -48.76946463831470169 ) ) ;
#10759 = CARTESIAN_POINT ( 'NONE',  ( 19.40270147970599979, -49.11618894467930829, -34.64999999999999858 ) ) ;
#10760 = CARTESIAN_POINT ( 'NONE',  ( 20.81696382897727915, -10.69163607886408052, -62.19491938749155935 ) ) ;
#10761 = AXIS2_PLACEMENT_3D ( 'NONE', #28729, #44730, #1486 ) ;
#10762 = CARTESIAN_POINT ( 'NONE',  ( 47.18324681005260146, -54.80726426785999905, -54.61059023070370699 ) ) ;
#10763 = ORIENTED_EDGE ( 'NONE', *, *, #44287, .T. ) ;
#10764 = CYLINDRICAL_SURFACE ( 'NONE', #19268, 0.4999999999999967248 ) ;
#10765 = ORIENTED_EDGE ( 'NONE', *, *, #11492, .T. ) ;
#10766 = CARTESIAN_POINT ( 'NONE',  ( 10.13805148651129961, -63.16689821662900783, -45.99545731505420321 ) ) ;
#10767 = EDGE_CURVE ( 'NONE', #8568, #5979, #43287, .T. ) ;
#10768 = CARTESIAN_POINT ( 'NONE',  ( -15.33935108854906026, 14.52970908907092529, 17.35000000000000142 ) ) ;
#10769 = ORIENTED_EDGE ( 'NONE', *, *, #14598, .F. ) ;
#10770 = CARTESIAN_POINT ( 'NONE',  ( 3.892469389394924484, -8.548574094810398094, -34.70142521051216278 ) ) ;
#10771 = CARTESIAN_POINT ( 'NONE',  ( 57.28557293208299939, 19.34652869517200102, -53.44460714490739406 ) ) ;
#10772 = CARTESIAN_POINT ( 'NONE',  ( 52.38320845594909514, 19.05065453847920054, -76.75839862161949156 ) ) ;
#10773 = ORIENTED_EDGE ( 'NONE', *, *, #49, .F. ) ;
#10774 = EDGE_CURVE ( 'NONE', #44502, #9603, #49136, .T. ) ;
#10775 = CARTESIAN_POINT ( 'NONE',  ( 16.13393739769620083, -15.61618894467929941, -54.64999999999999858 ) ) ;
#10776 = CARTESIAN_POINT ( 'NONE',  ( -21.36606260230379917, 21.88381105532059934, 10.84999999999999964 ) ) ;
#10777 = CARTESIAN_POINT ( 'NONE',  ( 83.62685953798910532, -44.53601850760680492, -46.55427990986279241 ) ) ;
#10778 = PLANE ( 'NONE',  #49631 ) ;
#10779 = EDGE_CURVE ( 'NONE', #51599, #6854, #49207, .T. ) ;
#10780 = CARTESIAN_POINT ( 'NONE',  ( 23.61751225746720095, -19.07723320532340239, -67.93021958131190274 ) ) ;
#10781 = CARTESIAN_POINT ( 'NONE',  ( 13.55743739769620149, -15.61618894467929941, -31.39999999999999858 ) ) ;
#10782 = CARTESIAN_POINT ( 'NONE',  ( 43.33111814803011441, -37.82550818684872240, -73.66403162998959431 ) ) ;
#10783 = ORIENTED_EDGE ( 'NONE', *, *, #50470, .T. ) ;
#10784 = ORIENTED_EDGE ( 'NONE', *, *, #15013, .F. ) ;
#10785 = CARTESIAN_POINT ( 'NONE',  ( 59.34499803081114777, -2.440885846858634078, -15.68015151901639648 ) ) ;
#10786 = CARTESIAN_POINT ( 'NONE',  ( 15.26659807257079926, -8.216566231308268797, -55.69551641643479911 ) ) ;
#10787 = EDGE_CURVE ( 'NONE', #16095, #6632, #548, .T. ) ;
#10788 = CARTESIAN_POINT ( 'NONE',  ( 8.886858354639530333, -15.19560952241709906, -32.14999999999999858 ) ) ;
#10789 = CARTESIAN_POINT ( 'NONE',  ( 10.46514124946499713, -11.84713790509142228, -61.63947181667826669 ) ) ;
#10790 = CARTESIAN_POINT ( 'NONE',  ( 45.90332635223469993, -45.11618894461400231, -7.776724400097649870 ) ) ;
#10791 = EDGE_CURVE ( 'NONE', #22762, #36880, #15408, .T. ) ;
#10792 = CARTESIAN_POINT ( 'NONE',  ( 14.14886614762350092, -32.59522544870679894, -35.02873218748179340 ) ) ;
#10793 = CARTESIAN_POINT ( 'NONE',  ( 41.72084690663209727, -44.94167883794940366, -5.743073974472929777 ) ) ;
#10794 = CARTESIAN_POINT ( 'NONE',  ( 14.74094437746738784, -7.760244216757398839, -60.95208477195205887 ) ) ;
#10795 = CIRCLE ( 'NONE', #19970, 5.499999999999998224 ) ;
#10797 = CIRCLE ( 'NONE', #11661, 34.55616290057869833 ) ;
#10796 = CARTESIAN_POINT ( 'NONE',  ( 16.09925802146080187, -7.371098402433019281, -67.00632966799250312 ) ) ;
#10798 = CARTESIAN_POINT ( 'NONE',  ( 21.11367553470149971, -21.58581933017369892, -32.14999999999999858 ) ) ;
#10799 = CARTESIAN_POINT ( 'NONE',  ( 53.99835063712060190, -51.20425914811980306, -75.55396929121511107 ) ) ;
#10801 = CARTESIAN_POINT ( 'NONE',  ( 41.55168008675715896, -39.71505707655544626, -78.49431477701308779 ) ) ;
#10800 = CARTESIAN_POINT ( 'NONE',  ( -2.478971262080560400, 19.85746904953009917, -8.032436426861050194 ) ) ;
#10802 = CARTESIAN_POINT ( 'NONE',  ( 49.60431418108288426, 21.56000271588285955, -52.10968937064622963 ) ) ;
#10803 = ORIENTED_EDGE ( 'NONE', *, *, #45929, .F. ) ;
#10804 = CARTESIAN_POINT ( 'NONE',  ( 13.88455142272560039, 20.94377921756336036, -75.56421430877985301 ) ) ;
#10805 = CARTESIAN_POINT ( 'NONE',  ( 47.60546839679840758, 23.29237299805700090, -54.74821169702579482 ) ) ;
#10806 = ADVANCED_FACE ( 'NONE', ( #451 ), #16441, .F. ) ;
#10807 = CARTESIAN_POINT ( 'NONE',  ( 41.60145709364243061, -44.81526105809438576, -5.503720813836787684 ) ) ;
#10808 = CARTESIAN_POINT ( 'NONE',  ( 84.02702888070515996, -44.63621333882932873, -47.45289756505584933 ) ) ;
#10809 = CARTESIAN_POINT ( 'NONE',  ( 61.15817508718350126, 14.37771941245649998, -47.69147225523349931 ) ) ;
#10810 = CARTESIAN_POINT ( 'NONE',  ( 12.02928806124960026, 34.13296712403600708, -17.22609667956750101 ) ) ;
#10811 = DIRECTION ( 'NONE',  ( 0.5720614028176839172, 0.4156269377774525209, 0.7071067811865484609 ) ) ;
#10812 = CARTESIAN_POINT ( 'NONE',  ( 52.83531650484950148, 18.42562942600509857, -48.55819829956829636 ) ) ;
#10813 = DIRECTION ( 'NONE',  ( -0.4640893551880601597, 0.8857883891771953788, 0.000000000000000000 ) ) ;
#10814 = CARTESIAN_POINT ( 'NONE',  ( 24.04526354826459666, -15.61618910718878794, -73.50766907743336276 ) ) ;
#10815 = CARTESIAN_POINT ( 'NONE',  ( 56.29817967269709555, 14.91712830013440083, -26.17903964292329988 ) ) ;
#10816 = CARTESIAN_POINT ( 'NONE',  ( 50.95940558857264335, 4.060833044306336070, -76.37898308257572921 ) ) ;
#10817 = CARTESIAN_POINT ( 'NONE',  ( 20.11805645080274019, -8.703658428487978327, -37.45900026128192906 ) ) ;
#10818 = CARTESIAN_POINT ( 'NONE',  ( 12.13696592144739839, -65.16745155981689663, -16.64705455763589725 ) ) ;
#10819 = CARTESIAN_POINT ( 'NONE',  ( 18.08251218718420716, 10.43523626583289321, -34.89146800830123851 ) ) ;
#10820 = CARTESIAN_POINT ( 'NONE',  ( 71.11795458202399800, 1.382840740411490188, -60.95335679887120506 ) ) ;
#10821 = CARTESIAN_POINT ( 'NONE',  ( 10.48644968250219911, 31.91257630746710561, -45.62816686667009947 ) ) ;
#10822 = CARTESIAN_POINT ( 'NONE',  ( 68.13393739769618662, -1.666188944679350081, -65.65000000000000568 ) ) ;
#10823 = CARTESIAN_POINT ( 'NONE',  ( 12.56262532525460074, -39.78532101326960202, -74.14999999999999147 ) ) ;
#10824 = CARTESIAN_POINT ( 'NONE',  ( 12.40077008615062404, 24.20909747964150682, -75.14569893024719249 ) ) ;
#10825 = VERTEX_POINT ( 'NONE', #40550 ) ;
#10826 = ORIENTED_EDGE ( 'NONE', *, *, #1873, .F. ) ;
#10827 = CARTESIAN_POINT ( 'NONE',  ( 16.13393739769620083, -15.61618894467929941, -81.23899999999999011 ) ) ;
#10828 = CARTESIAN_POINT ( 'NONE',  ( 76.49445432434755787, -3.248734881417176368, -13.20352109380791461 ) ) ;
#10829 = ORIENTED_EDGE ( 'NONE', *, *, #38391, .F. ) ;
#10830 = CARTESIAN_POINT ( 'NONE',  ( 12.39116069916539864, -65.38104303664570693, -46.54587262935750402 ) ) ;
#10831 = CARTESIAN_POINT ( 'NONE',  ( 56.92567216073919667, -45.20107943371309744, -25.36893163837739706 ) ) ;
#10832 = CARTESIAN_POINT ( 'NONE',  ( 0.6614253361915152229, -8.772027323367371565, -34.75586992539665943 ) ) ;
#10833 = EDGE_CURVE ( 'NONE', #47191, #371, #44098, .T. ) ;
#10834 = CIRCLE ( 'NONE', #775, 1.999999999999998224 ) ;
#10835 = CARTESIAN_POINT ( 'NONE',  ( 63.50390619396989678, 1.388715606738730068, -68.72506404892941134 ) ) ;
#10836 = VERTEX_POINT ( 'NONE', #25054 ) ;
#10837 = DIRECTION ( 'NONE',  ( 0.000000000000000000, 0.000000000000000000, -1.000000000000000000 ) ) ;
#10838 = CIRCLE ( 'NONE', #14146, 14.49999999999999822 ) ;
#10839 = CARTESIAN_POINT ( 'NONE',  ( 44.10370407306162832, 6.698676713549935435, -69.80110960494087635 ) ) ;
#10840 = PLANE ( 'NONE',  #50415 ) ;
#10841 = CIRCLE ( 'NONE', #47642, 4.959400861452849085 ) ;
#10842 = AXIS2_PLACEMENT_3D ( 'NONE', #28631, #24166, #8737 ) ;
#10843 = EDGE_CURVE ( 'NONE', #36140, #15955, #44479, .T. ) ;
#10844 = VERTEX_POINT ( 'NONE', #5944 ) ;
#10845 = CARTESIAN_POINT ( 'NONE',  ( 13.60927945319200028, -7.767060182887570718, -37.19327432862769456 ) ) ;
#10846 = DIRECTION ( 'NONE',  ( -0.4439767838698117641, 0.8960382890170590642, 0.000000000000000000 ) ) ;
#10847 = CARTESIAN_POINT ( 'NONE',  ( 26.52624224310950396, -21.61618894467929763, -22.14999999999999858 ) ) ;
#10848 = CARTESIAN_POINT ( 'NONE',  ( 13.64424757191504867, -21.92950919661451081, -51.07239313048388851 ) ) ;
#10849 = CARTESIAN_POINT ( 'NONE',  ( 62.49253998539199983, -29.48318676728260002, -16.12968574675709732 ) ) ;
#10850 = CARTESIAN_POINT ( 'NONE',  ( 63.11679429741250402, 0.8888742037077599356, -62.35931220671560027 ) ) ;
#10851 = CARTESIAN_POINT ( 'NONE',  ( 47.18783699164220025, -54.49278665692580148, -75.11697231728020085 ) ) ;
#10852 = CARTESIAN_POINT ( 'NONE',  ( 49.41736058582200286, 13.88381311221330172, -8.069193831786499516 ) ) ;
#10853 = B_SPLINE_CURVE_WITH_KNOTS ( 'NONE', 3,
 ( #8242, #12706, #6847, #14953, #2652, #22796, #35115, #11032, #38819, #23054, #27000, #22024, #18622, #34075, #19136, #14179, #10256, #2908, #18356, #26216, #18108, #38554 ),
 .UNSPECIFIED., .F., .F.,
 ( 4, 2, 2, 2, 2, 2, 2, 2, 2, 2, 4 ),
 ( 0.000000000000000000, 0.09821630342860182550, 0.2339808679556865390, 0.3375000544871513131, 0.4375000462626749687, 0.5000000411223781693, 0.6250000308417832384, 0.7117379798405728542, 0.7984759288393613597, 0.9372566472374248558, 1.000000000000000000 ),
 .UNSPECIFIED. ) ;
#10854 = CARTESIAN_POINT ( 'NONE',  ( 27.13393739769620083, 7.383811055320659733, -59.64999999999999147 ) ) ;
#10855 = LINE ( 'NONE', #23136, #45678 ) ;
#10856 = CARTESIAN_POINT ( 'NONE',  ( 17.11601836966919876, -7.830158814151449320, -78.82744428701180084 ) ) ;
#10857 = VERTEX_POINT ( 'NONE', #13807 ) ;
#10858 = CARTESIAN_POINT ( 'NONE',  ( 12.86517331568619937, 17.88381105532060289, -34.64999999999999858 ) ) ;
#10859 = CARTESIAN_POINT ( 'NONE',  ( 4.773425314697229638, -58.71548316886770635, -13.16258282087829912 ) ) ;
#10860 = CARTESIAN_POINT ( 'NONE',  ( 76.74972829916860917, 9.566990831016390473, -14.30201763231599976 ) ) ;
#10861 = CARTESIAN_POINT ( 'NONE',  ( 31.79224979287389985, 4.883811055320679273, -84.65000000000000568 ) ) ;
#10862 = DIRECTION ( 'NONE',  ( 0.000000000000000000, 0.000000000000000000, -1.000000000000000000 ) ) ;
#10863 = AXIS2_PLACEMENT_3D ( 'NONE', #20896, #45281, #37662 ) ;
#10864 = TOROIDAL_SURFACE ( 'NONE', #39288, 31.45861873485090143, 3.000000000000000000 ) ;
#10865 = CARTESIAN_POINT ( 'NONE',  ( 9.367097141674031846, -15.61601956221279863, -71.84717978381000592 ) ) ;
#10866 = CARTESIAN_POINT ( 'NONE',  ( 22.46011653503687810, -20.47784780404496274, -38.00066731914451168 ) ) ;
#10867 = EDGE_CURVE ( 'NONE', #20094, #34780, #28471, .T. ) ;
#10868 = VECTOR ( 'NONE', #9201, 1000.000000000000000 ) ;
#10869 = CARTESIAN_POINT ( 'NONE',  ( 82.45925359270579236, -45.27638716885540049, -47.17632001488509985 ) ) ;
#10870 = LINE ( 'NONE', #21150, #12252 ) ;
#10871 = CARTESIAN_POINT ( 'NONE',  ( 41.26856152876109718, 13.06989385214870047, -4.473876091761409768 ) ) ;
#10872 = DIRECTION ( 'NONE',  ( 0.000000000000000000, 0.000000000000000000, 1.000000000000000000 ) ) ;
#10873 = CARTESIAN_POINT ( 'NONE',  ( 49.40539548389170221, -53.49785366682009879, -54.15746054660930042 ) ) ;
#10874 = CARTESIAN_POINT ( 'NONE',  ( 70.83745409581581498, -49.21324915460289162, -70.54648330188271643 ) ) ;
#10875 = EDGE_CURVE ( 'NONE', #12879, #6259, #24742, .T. ) ;
#10876 = AXIS2_PLACEMENT_3D ( 'NONE', #45227, #16658, #37610 ) ;
#10877 = CARTESIAN_POINT ( 'NONE',  ( 76.38705314788980161, -43.26417677700779763, -13.94855457485863148 ) ) ;
#10878 = CARTESIAN_POINT ( 'NONE',  ( 18.45990697330769947, -52.11465364279959545, -75.47164421335219231 ) ) ;
#10879 = CARTESIAN_POINT ( 'NONE',  ( 60.34831028877889736, -45.11618894467940066, -11.22201639935360085 ) ) ;
#10880 = EDGE_CURVE ( 'NONE', #16411, #29700, #17732, .T. ) ;
#10881 = EDGE_LOOP ( 'NONE', ( #6182, #49377, #17694, #43633 ) ) ;
#10882 = CARTESIAN_POINT ( 'NONE',  ( 20.03694594417709851, -9.270070554321430123, -56.74285641080169995 ) ) ;
#10883 = CARTESIAN_POINT ( 'NONE',  ( 63.75644714388239720, 1.054781932184780002, -61.54608750241579429 ) ) ;
#10884 = ORIENTED_EDGE ( 'NONE', *, *, #44385, .F. ) ;
#10885 = FACE_OUTER_BOUND ( 'NONE', #32887, .T. ) ;
#10886 = CARTESIAN_POINT ( 'NONE',  ( 16.13393739769620083, -15.61618894467929941, -11.54999999999999893 ) ) ;
#10887 = CARTESIAN_POINT ( 'NONE',  ( 73.08275130671789555, 1.274277262446050107, -68.71132524057000523 ) ) ;
#10888 = CARTESIAN_POINT ( 'NONE',  ( 17.90524883137746670, -9.025333787991407064, -74.03615355641134954 ) ) ;
#10889 = CARTESIAN_POINT ( 'NONE',  ( 9.828799619648670216, -18.43223393006180189, -81.23899999999999011 ) ) ;
#10890 = CARTESIAN_POINT ( 'NONE',  ( 44.57967080629300227, -45.59411579619229826, -8.202780460755210612 ) ) ;
#10891 = VERTEX_POINT ( 'NONE', #46566 ) ;
#10892 = ORIENTED_EDGE ( 'NONE', *, *, #36955, .T. ) ;
#10893 = ORIENTED_EDGE ( 'NONE', *, *, #42079, .F. ) ;
#10894 = CARTESIAN_POINT ( 'NONE',  ( 29.13393739769619728, 1.883811055320659955, -53.85091742636659973 ) ) ;
#10895 = CARTESIAN_POINT ( 'NONE',  ( 23.38451280374270169, -13.27842595937890025, -81.23899999999999011 ) ) ;
#10896 = DIRECTION ( 'NONE',  ( 0.000000000000000000, 1.000000000000000000, 0.000000000000000000 ) ) ;
#10897 = EDGE_LOOP ( 'NONE', ( #2128, #31425, #41254, #48885 ) ) ;
#10898 = ADVANCED_FACE ( 'NONE', ( #9619 ), #25574, .T. ) ;
#10899 = CARTESIAN_POINT ( 'NONE',  ( 8.222935796957566268, -14.58065318844518288, -52.54933528575815416 ) ) ;
#10900 = ORIENTED_EDGE ( 'NONE', *, *, #25246, .F. ) ;
#10901 = CARTESIAN_POINT ( 'NONE',  ( 15.09843553512047265, -7.705183434958806643, -63.25066585830453647 ) ) ;
#10902 = CIRCLE ( 'NONE', #37631, 0.5000000000000000000 ) ;
#10903 = CARTESIAN_POINT ( 'NONE',  ( 68.13393739769618662, -28.66618894467939782, -31.09383709942130380 ) ) ;
#10904 = CONICAL_SURFACE ( 'NONE', #16718, 12.92820323027549989, 0.7481802937784480800 ) ;
#10905 = CIRCLE ( 'NONE', #22586, 19.50000000000000000 ) ;
#10906 = ORIENTED_EDGE ( 'NONE', *, *, #39474, .F. ) ;
#10907 = DIRECTION ( 'NONE',  ( 0.000000000000000000, -1.000000000000000000, 0.000000000000000000 ) ) ;
#10908 = CARTESIAN_POINT ( 'NONE',  ( 51.41094422139000386, -50.88107716530349478, -76.16757073797020894 ) ) ;
#10909 = AXIS2_PLACEMENT_3D ( 'NONE', #48589, #21040, #881 ) ;
#10910 = CARTESIAN_POINT ( 'NONE',  ( 60.86666111963769765, 14.22176795161809970, -47.11612196671629960 ) ) ;
#10911 = CIRCLE ( 'NONE', #15090, 2.999999999999998668 ) ;
#10912 = CARTESIAN_POINT ( 'NONE',  ( 38.67452568954060155, 6.328436186825659782, -84.65000000000000568 ) ) ;
#10913 = CARTESIAN_POINT ( 'NONE',  ( 41.39168606550949647, -44.20447096405560217, -4.419064217266010175 ) ) ;
#10914 = CARTESIAN_POINT ( 'NONE',  ( 16.13393739769620083, -15.61618894467929941, 9.349999999999999645 ) ) ;
#10915 = CARTESIAN_POINT ( 'NONE',  ( -2.895883735633389744, 17.91114786048130014, -5.678499123949679372 ) ) ;
#10916 = CARTESIAN_POINT ( 'NONE',  ( 64.46842165375500144, 0.9408120350972830614, -70.40100145642890084 ) ) ;
#10917 = DIRECTION ( 'NONE',  ( -1.224646799147358138E-16, 1.000000000000000000, 6.060292087350919618E-16 ) ) ;
#10918 = CARTESIAN_POINT ( 'NONE',  ( 17.84258640648128136, -51.34461569807859860, -75.09855816271016238 ) ) ;
#10919 = CARTESIAN_POINT ( 'NONE',  ( 10.34713824738410004, -20.91710431630430023, -52.05144558750829731 ) ) ;
#10920 = ORIENTED_EDGE ( 'NONE', *, *, #2144, .F. ) ;
#10921 = CARTESIAN_POINT ( 'NONE',  ( 43.81052300022479784, 14.82244714638200023, -8.159011786981970715 ) ) ;
#10922 = CARTESIAN_POINT ( 'NONE',  ( 71.63754647491310834, 1.424120032877639996, -70.11997829442159968 ) ) ;
#10923 = CARTESIAN_POINT ( 'NONE',  ( 44.44775996439803123, -39.99043000850869589, -64.48947138781548460 ) ) ;
#10924 = CARTESIAN_POINT ( 'NONE',  ( 13.95190178771939848, 19.57559525226260178, -21.48693983945959829 ) ) ;
#10925 = CARTESIAN_POINT ( 'NONE',  ( 21.12141086460500006, -10.88484145508220102, -32.14999999999999858 ) ) ;
#10926 = DIRECTION ( 'NONE',  ( 0.000000000000000000, 0.000000000000000000, -1.000000000000000000 ) ) ;
#10927 = CARTESIAN_POINT ( 'NONE',  ( 63.28685848367280897, 1.187931651339009909, -69.04190732916428885 ) ) ;
#10928 = CARTESIAN_POINT ( 'NONE',  ( 48.07907502642350295, -54.29565632080440452, -54.84628907412789545 ) ) ;
#10929 = CARTESIAN_POINT ( 'NONE',  ( 24.04374919936876154, -15.46808838925558405, -45.50171747978662040 ) ) ;
#10930 = ADVANCED_FACE ( 'NONE', ( #38425 ), #14318, .T. ) ;
#10931 = CARTESIAN_POINT ( 'NONE',  ( -7.651755816028718904, -45.25221342046138773, -4.961742080343907624 ) ) ;
#10932 = CARTESIAN_POINT ( 'NONE',  ( 47.71148510080310245, 23.26888792098559833, -55.04989704333419809 ) ) ;
#10933 = ADVANCED_FACE ( 'NONE', ( #34477 ), #23168, .T. ) ;
#10934 = ORIENTED_EDGE ( 'NONE', *, *, #41452, .T. ) ;
#10935 = CARTESIAN_POINT ( 'NONE',  ( 15.69653675527930226, -8.576924789068980814, -76.32742627405558267 ) ) ;
#10936 = VERTEX_POINT ( 'NONE', #21390 ) ;
#10937 = CARTESIAN_POINT ( 'NONE',  ( 71.41841232404479456, 1.186701509386330011, -70.56202332290359891 ) ) ;
#10938 = AXIS2_PLACEMENT_3D ( 'NONE', #35246, #22142, #38153 ) ;
#10939 = CARTESIAN_POINT ( 'NONE',  ( 17.16955428432172681, -23.52717903123599896, -57.96600128679276054 ) ) ;
#10940 = CARTESIAN_POINT ( 'NONE',  ( 57.45452828658709876, -47.23787284142349563, -47.71980555553449932 ) ) ;
#10941 = DIRECTION ( 'NONE',  ( 1.000000000000000000, 0.000000000000000000, 0.000000000000000000 ) ) ;
#10943 = CARTESIAN_POINT ( 'NONE',  ( 20.88396115700760092, -10.40276075773470055, -58.58238571580489662 ) ) ;
#10942 = CARTESIAN_POINT ( 'NONE',  ( 40.83956339042367745, 8.397827017939304639, -81.92924210665236728 ) ) ;
#10944 = CIRCLE ( 'NONE', #51816, 38.61618927352878927 ) ;
#10945 = CARTESIAN_POINT ( 'NONE',  ( 16.13393739769309931, -15.61618894467859953, -3.187564294432039702 ) ) ;
#10946 = CARTESIAN_POINT ( 'NONE',  ( 24.04493742164818926, -14.58064954397486268, -67.75066253846064512 ) ) ;
#10947 = CARTESIAN_POINT ( 'NONE',  ( 9.221485035723937074, -11.63193652317346505, -66.67433469079290376 ) ) ;
#10948 = B_SPLINE_SURFACE_WITH_KNOTS ( 'NONE', 3, 3, ( 
 ( #14628, #5734, #41895, #10446, #2316, #37963, #26399, #30337, #5992, #49764, #30595, #14369 ),
 ( #17779, #34007, #2580, #46878, #34789, #18809, #46360, #38221, #13856, #10705, #21693, #37701 ),
 ( #42420, #21953, #2061, #50284, #29813, #42680, #34530, #50795, #46616, #46099, #38480, #26658 ),
 ( #6776, #9918, #18038, #6511, #30848, #10184, #22471, #18555, #26145, #25880, #1796, #14883 ),
 ( #10965, #22727, #50017, #42156, #38750, #14107, #30075, #26930, #33750, #45830, #22212, #6254 ),
 ( #50536, #18288, #2843, #34260, #7803, #11485, #39515, #23239, #22985, #27443, #32839, #48604 ) ),
 .UNSPECIFIED., .F., .F., .F.,
 ( 4, 1, 1, 4 ),
 ( 4, 2, 2, 2, 2, 4 ),
 ( -5.656587004999999529E-06, 0.3333333333333329818, 0.6666666666666670737, 1.000000000000000000 ),
 ( -8.926961658285021528, -8.407199725736200335, -7.356299760019170186, -5.674859814871930475, -2.984555902636349956, -0.2480234047818090093 ),
 .UNSPECIFIED. ) ;
#10949 = ORIENTED_EDGE ( 'NONE', *, *, #2592, .F. ) ;
#10950 = FACE_OUTER_BOUND ( 'NONE', #31861, .T. ) ;
#10951 = EDGE_LOOP ( 'NONE', ( #36004, #9394, #44241, #25462 ) ) ;
#10952 = EDGE_LOOP ( 'NONE', ( #25387, #45096, #2433, #6246 ) ) ;
#10953 = CARTESIAN_POINT ( 'NONE',  ( 12.00872700125690073, -64.88650295836660575, -16.20508613916799945 ) ) ;
#10954 = DIRECTION ( 'NONE',  ( -1.000000000000000000, 0.000000000000000000, 0.000000000000000000 ) ) ;
#10955 = CARTESIAN_POINT ( 'NONE',  ( 9.367432603602109609, -15.61609789975089946, -77.84717978380999170 ) ) ;
#10956 = CARTESIAN_POINT ( 'NONE',  ( 11.81871210215889967, -65.31307805416919621, -47.30065584137410184 ) ) ;
#10957 = ORIENTED_EDGE ( 'NONE', *, *, #45969, .T. ) ;
#10958 = ORIENTED_EDGE ( 'NONE', *, *, #4468, .T. ) ;
#10959 = ADVANCED_FACE ( 'NONE', ( #46306 ), #10634, .T. ) ;
#10960 = CARTESIAN_POINT ( 'NONE',  ( 24.04493430356115269, -15.62427093480796358, -55.50799714576009336 ) ) ;
#10961 = CARTESIAN_POINT ( 'NONE',  ( 57.05132883896109774, 14.65902881311749972, -26.24859059622079727 ) ) ;
#10962 = DIRECTION ( 'NONE',  ( 1.000000000000000000, 0.000000000000000000, 0.000000000000000000 ) ) ;
#10963 = ADVANCED_FACE ( 'NONE', ( #17480 ), #22629, .T. ) ;
#10964 = CARTESIAN_POINT ( 'NONE',  ( 65.38480309005331037, -0.6329806532248359874, -16.65168329525840107 ) ) ;
#10965 = CARTESIAN_POINT ( 'NONE',  ( 56.91683350687570453, -50.66367375722730060, -53.20180161368870131 ) ) ;
#10966 = EDGE_LOOP ( 'NONE', ( #29100, #35701, #21824, #29952 ) ) ;
#10967 = CARTESIAN_POINT ( 'NONE',  ( 18.58559990215474045, -8.073364231484838172, -33.39234495213820253 ) ) ;
#10968 = CYLINDRICAL_SURFACE ( 'NONE', #30927, 1.999999999999996669 ) ;
#10969 = ORIENTED_EDGE ( 'NONE', *, *, #31014, .T. ) ;
#10970 = CARTESIAN_POINT ( 'NONE',  ( 10.41791033310424375, -64.23844989214747159, -23.06400185344022802 ) ) ;
#10971 = CARTESIAN_POINT ( 'NONE',  ( 49.60975479626670648, -45.11618894467940066, -10.01352555637939901 ) ) ;
#10972 = CARTESIAN_POINT ( 'NONE',  ( 23.82331477792010332, -14.04767911172229944, -39.94844302531450353 ) ) ;
#10973 = CARTESIAN_POINT ( 'NONE',  ( 13.38498534606780055, -51.10135539216639700, -21.91519318942190253 ) ) ;
#10974 = CARTESIAN_POINT ( 'NONE',  ( 55.30868802464280520, 19.38381105532069881, -76.41966175253659799 ) ) ;
#10975 = CARTESIAN_POINT ( 'NONE',  ( 14.81467456660999993, -7.815966731016759539, -81.23899999999999011 ) ) ;
#10976 = CARTESIAN_POINT ( 'NONE',  ( 55.23395345995140104, 14.09343332238140079, -15.21757741273719944 ) ) ;
#10977 = CARTESIAN_POINT ( 'NONE',  ( 60.76024220928780295, -45.50591669753300295, -47.06490144688479660 ) ) ;
#10978 = AXIS2_PLACEMENT_3D ( 'NONE', #21735, #25664, #16791 ) ;
#10979 =( BOUNDED_CURVE ( )  B_SPLINE_CURVE ( 2, ( #11855, #36439, #43809 ),
 .UNSPECIFIED., .F., .T. ) 
 B_SPLINE_CURVE_WITH_KNOTS ( ( 3, 3 ),
 ( -1.071465066616890116, -0.1016765296687800468 ),
 .UNSPECIFIED. ) 
 CURVE ( )  GEOMETRIC_REPRESENTATION_ITEM ( )  RATIONAL_B_SPLINE_CURVE ( ( 1.000064779730289954, 1.000064447938610046, 1.000011648212760118 ) ) 
 REPRESENTATION_ITEM ( '' )  );
#10980 = CARTESIAN_POINT ( 'NONE',  ( 56.83258908092710016, -50.30522036972260480, -52.72698303625519856 ) ) ;
#10981 = VECTOR ( 'NONE', #6451, 1000.000000000000114 ) ;
#10982 = CARTESIAN_POINT ( 'NONE',  ( 19.76827833599989859, -21.66053548658279837, -47.17485964264358955 ) ) ;
#10983 = CARTESIAN_POINT ( 'NONE',  ( 46.67455644844360307, -39.87048571057250257, -54.56212092059809748 ) ) ;
#10984 = AXIS2_PLACEMENT_3D ( 'NONE', #19059, #10693, #19832 ) ;
#10985 = VERTEX_POINT ( 'NONE', #6592 ) ;
#10986 = CARTESIAN_POINT ( 'NONE',  ( 47.52155195348809968, 23.26505193837810026, -74.72489557265679139 ) ) ;
#10987 = CARTESIAN_POINT ( 'NONE',  ( 64.80222656955069738, 0.9966178393190270324, -60.66877295535580572 ) ) ;
#10988 = CARTESIAN_POINT ( 'NONE',  ( 23.60377752213929980, 17.56341275872070185, -34.96018206680729890 ) ) ;
#10989 = DIRECTION ( 'NONE',  ( -0.2260571801428161443, 1.249000902703300615E-16, 0.9741140340359945027 ) ) ;
#10990 = CARTESIAN_POINT ( 'NONE',  ( 12.14988595507787039, -8.703620529061049993, -46.84100228733535687 ) ) ;
#10991 = CARTESIAN_POINT ( 'NONE',  ( 82.33636559101309160, 14.30306463946360118, -47.60086789927839845 ) ) ;
#10992 = CARTESIAN_POINT ( 'NONE',  ( -15.89903062800279976, 7.092556714909539650, -48.83602070084049984 ) ) ;
#10993 = CARTESIAN_POINT ( 'NONE',  ( 24.04493739160588461, -16.65172911444284765, -57.83399790364183701 ) ) ;
#10994 = ADVANCED_FACE ( 'NONE', ( #51138 ), #9313, .T. ) ;
#10995 = CARTESIAN_POINT ( 'NONE',  ( 33.38393739769599478, 10.88381105532080007, -35.14999999999999858 ) ) ;
#10996 = CARTESIAN_POINT ( 'NONE',  ( 49.57944902481020222, 22.47411269264829770, -55.02902090455440032 ) ) ;
#10997 = ORIENTED_EDGE ( 'NONE', *, *, #47916, .T. ) ;
#10998 = CARTESIAN_POINT ( 'NONE',  ( 53.40905300656029908, -49.37518268217669970, -48.94487162954590076 ) ) ;
#10999 = ORIENTED_EDGE ( 'NONE', *, *, #22869, .F. ) ;
#11000 = CARTESIAN_POINT ( 'NONE',  ( 39.73155014768870785, 8.662390057901488305, -85.55364038000607252 ) ) ;
#11001 = CARTESIAN_POINT ( 'NONE',  ( 10.72267410870809456, -11.45744577544797238, -41.66115342960441836 ) ) ;
#11002 = CARTESIAN_POINT ( 'NONE',  ( 13.72890770306269914, 19.91029111355249626, -22.20512747466040082 ) ) ;
#11003 = CARTESIAN_POINT ( 'NONE',  ( 47.13393739769619373, -39.28050807707769820, -35.08812023096449906 ) ) ;
#11004 = CARTESIAN_POINT ( 'NONE',  ( 22.67903386406930011, -12.98859100311820036, -54.33130069781340410 ) ) ;
#11005 = CARTESIAN_POINT ( 'NONE',  ( 52.73507126972099712, 18.49830744958629936, -48.76328856354190577 ) ) ;
#11006 = CARTESIAN_POINT ( 'NONE',  ( 56.28192874346009233, -45.52819744086340137, -17.75909607022310155 ) ) ;
#11007 = CARTESIAN_POINT ( 'NONE',  ( 16.36911989528830347, 19.86384299893705574, -15.67312363240488260 ) ) ;
#11008 = VERTEX_POINT ( 'NONE', #38833 ) ;
#11009 = CARTESIAN_POINT ( 'NONE',  ( 8.301939929713778810, -16.11274090036949858, -38.26735158243850066 ) ) ;
#11010 = ORIENTED_EDGE ( 'NONE', *, *, #43328, .T. ) ;
#11011 = CARTESIAN_POINT ( 'NONE',  ( 73.03159560797669769, 0.9395704634982890990, -69.11607016250870572 ) ) ;
#11012 = CARTESIAN_POINT ( 'NONE',  ( 10.53031889316589975, 33.70290473908939788, -47.11352251503090116 ) ) ;
#11013 = CARTESIAN_POINT ( 'NONE',  ( 73.01377481872879116, 1.100585178972000033, -62.22139992353060478 ) ) ;
#11014 = VECTOR ( 'NONE', #9396, 1000.000000000000000 ) ;
#11015 = DIRECTION ( 'NONE',  ( 0.000000000000000000, 1.000000000000000000, 0.000000000000000000 ) ) ;
#11016 = CARTESIAN_POINT ( 'NONE',  ( 52.62851868536466071, -49.80923738442962900, -48.67162951074862320 ) ) ;
#11017 = DIRECTION ( 'NONE',  ( 0.000000000000000000, -1.000000000000000000, 0.000000000000000000 ) ) ;
#11018 = AXIS2_PLACEMENT_3D ( 'NONE', #44639, #41484, #41743 ) ;
#11019 = TOROIDAL_SURFACE ( 'NONE', #37764, 36.50000000076989437, 1.500000000038270054 ) ;
#11020 = CARTESIAN_POINT ( 'NONE',  ( 51.80256375288589510, -52.76240455486869507, -54.49703439224219892 ) ) ;
#11021 = ORIENTED_EDGE ( 'NONE', *, *, #12703, .T. ) ;
#11022 = CARTESIAN_POINT ( 'NONE',  ( 64.81907236522980043, 1.326666718054990035, -70.38086014838010840 ) ) ;
#11023 = ORIENTED_EDGE ( 'NONE', *, *, #15135, .T. ) ;
#11024 = CARTESIAN_POINT ( 'NONE',  ( 10.14177886503980019, -63.22230780886520307, -45.99369029958189969 ) ) ;
#11025 = CARTESIAN_POINT ( 'NONE',  ( 65.43393739769584272, 16.88381105531917825, -74.20000000000047180 ) ) ;
#11026 = VERTEX_POINT ( 'NONE', #49402 ) ;
#11027 = EDGE_CURVE ( 'NONE', #22139, #26146, #1433, .T. ) ;
#11028 = CARTESIAN_POINT ( 'NONE',  ( 8.222931483157154275, -16.52762990423480716, -44.75564699102723409 ) ) ;
#11029 = CARTESIAN_POINT ( 'NONE',  ( 56.94659877973650453, 19.40673623115929658, -53.72521299826679808 ) ) ;
#11030 = CARTESIAN_POINT ( 'NONE',  ( 54.17317666804649434, 19.38381105980860042, -77.01210127079860968 ) ) ;
#11031 = EDGE_LOOP ( 'NONE', ( #1588, #26272 ) ) ;
#11032 = CARTESIAN_POINT ( 'NONE',  ( 9.758904658578256175, -64.50914076886910209, -46.91371261186735353 ) ) ;
#11033 = CARTESIAN_POINT ( 'NONE',  ( 9.367366684597708826, -15.61630833865650025, -41.84717978380999170 ) ) ;
#11034 = CARTESIAN_POINT ( 'NONE',  ( 22.14986259033789651, -18.71508664667078747, -32.60422815991633172 ) ) ;
#11035 = CARTESIAN_POINT ( 'NONE',  ( 0.3209249304026170480, -20.69829881652800196, -34.64999999999999858 ) ) ;
#11036 = CARTESIAN_POINT ( 'NONE',  ( 9.886430078882730399, -10.23554099510050008, -63.01864585536759478 ) ) ;
#11037 = CARTESIAN_POINT ( 'NONE',  ( 11.27237428567958410, -21.94244108617342803, -48.21600222955554926 ) ) ;
#11038 = DIRECTION ( 'NONE',  ( 0.000000000000000000, -1.000000000000000000, 0.000000000000000000 ) ) ;
#11039 = VERTEX_POINT ( 'NONE', #22297 ) ;
#11040 = EDGE_LOOP ( 'NONE', ( #6129, #9651, #18527, #18102, #49119, #3863 ) ) ;
#11041 = CARTESIAN_POINT ( 'NONE',  ( 53.35699421374690132, -49.92639189236809472, -74.14999999999999147 ) ) ;
#11042 = CARTESIAN_POINT ( 'NONE',  ( 21.65368711269129776, -20.62009310932489825, -50.46706696623599697 ) ) ;
#11043 = VECTOR ( 'NONE', #45785, 1000.000000000000114 ) ;
#11044 = CARTESIAN_POINT ( 'NONE',  ( 49.90995254736770192, 13.88381105525079917, -10.51652384872640056 ) ) ;
#11045 = DIRECTION ( 'NONE',  ( 1.000000000000000000, 2.460964292799963328E-14, 0.000000000000000000 ) ) ;
#11046 = B_SPLINE_CURVE_WITH_KNOTS ( 'NONE', 3,
 ( #8601, #32157, #24033, #8087, #20121, #36114, #28236, #24550, #40564, #4658, #44759, #45537, #17747, #10412, #37410, #37157, #25843, #26363 ),
 .UNSPECIFIED., .F., .F.,
 ( 4, 2, 2, 2, 2, 2, 2, 2, 4 ),
 ( 0.000000000000000000, 0.06250016148259907034, 0.1250003229651981407, 0.1875004844477972110, 0.2500006459303962814, 0.3125008074129953517, 0.3750009688955944220, 0.4375011303781934924, 0.5000012918607925627 ),
 .UNSPECIFIED. ) ;
#11047 = FACE_OUTER_BOUND ( 'NONE', #48638, .T. ) ;
#11048 = CARTESIAN_POINT ( 'NONE',  ( 46.03121886948380137, -45.11618894467940066, -7.582877905987319700 ) ) ;
#11049 = CARTESIAN_POINT ( 'NONE',  ( 37.33393739769619657, -15.61618894467929941, -12.65000000000000036 ) ) ;
#11050 = AXIS2_PLACEMENT_3D ( 'NONE', #12862, #33528, #1052 ) ;
#11051 = B_SPLINE_CURVE_WITH_KNOTS ( 'NONE', 3,
 ( #44956, #9057, #4341, #25006, #24751, #20308, #21091, #36048, #41021, #20829 ),
 .UNSPECIFIED., .F., .F.,
 ( 4, 2, 2, 2, 4 ),
 ( -0.0004281134594814769946, 0.000000000000000000, 0.02012916873241540200, 0.03942875605163800173, 0.05028014561794270920 ),
 .UNSPECIFIED. ) ;
#11052 = CIRCLE ( 'NONE', #44523, 12.00000000000000000 ) ;
#11053 = CARTESIAN_POINT ( 'NONE',  ( 12.11414304660310037, 33.92875631211279597, -16.63763903706830405 ) ) ;
#11054 = CARTESIAN_POINT ( 'NONE',  ( 11.70687558403979978, -8.660339290823859670, -60.82725304503019714 ) ) ;
#11055 = CARTESIAN_POINT ( 'NONE',  ( 22.35155673883920002, -20.04374387662789658, -32.14999999999999858 ) ) ;
#11056 = CARTESIAN_POINT ( 'NONE',  ( 54.96130583373059864, -50.78188363031180330, -75.77346936485569984 ) ) ;
#11058 = CARTESIAN_POINT ( 'NONE',  ( 14.36260343933235717, -9.025338114671583867, -59.86946046379193831 ) ) ;
#11057 = CARTESIAN_POINT ( 'NONE',  ( -5.707727980563209513, 16.52479455181530099, -7.103282072075530529 ) ) ;
#11059 = EDGE_CURVE ( 'NONE', #41415, #13824, #46964, .T. ) ;
#11060 = LINE ( 'NONE', #18387, #38050 ) ;
#11061 = DIRECTION ( 'NONE',  ( 1.000000000000000000, 0.000000000000000000, 0.000000000000000000 ) ) ;
#11062 = EDGE_CURVE ( 'NONE', #26440, #3287, #21488, .T. ) ;
#11063 = ORIENTED_EDGE ( 'NONE', *, *, #40499, .F. ) ;
#11064 = CARTESIAN_POINT ( 'NONE',  ( 14.04522320185620821, 21.07288667591008391, -75.74021525116319253 ) ) ;
#11065 = ADVANCED_FACE ( 'NONE', ( #11047 ), #18637, .T. ) ;
#11066 = CARTESIAN_POINT ( 'NONE',  ( 47.58181567201759776, 23.31431080387180188, -54.81048423692320171 ) ) ;
#11067 = CARTESIAN_POINT ( 'NONE',  ( 46.03121886948380137, -45.11618894467940066, -7.582877905987319700 ) ) ;
#11068 = CARTESIAN_POINT ( 'NONE',  ( 63.40307724931621181, 1.326666718054969829, -62.33513496753349870 ) ) ;
#11069 = CARTESIAN_POINT ( 'NONE',  ( 51.13393739769620083, 19.38381105532069881, 17.35000000000000142 ) ) ;
#11070 = CARTESIAN_POINT ( 'NONE',  ( 11.41271396217749867, 33.75416681246609585, -16.69425700585249928 ) ) ;
#11071 = EDGE_CURVE ( 'NONE', #12691, #51462, #5621, .T. ) ;
#11072 = CARTESIAN_POINT ( 'NONE',  ( 51.21769383437759871, 18.09844762758200076, -76.45366765079749882 ) ) ;
#11073 = CARTESIAN_POINT ( 'NONE',  ( 52.83236039598959621, 18.42717821426129987, -48.53480049868939972 ) ) ;
#11074 = DIRECTION ( 'NONE',  ( 0.000000000000000000, 0.000000000000000000, 1.000000000000000000 ) ) ;
#11075 = CARTESIAN_POINT ( 'NONE',  ( 52.96846357502160174, -49.58824783477410136, -48.76456334744820253 ) ) ;
#11076 = CARTESIAN_POINT ( 'NONE',  ( 56.24187033329050678, 15.29152766842380018, -26.31653598774670044 ) ) ;
#11077 = CARTESIAN_POINT ( 'NONE',  ( 49.44978923146629768, 22.30861604384239882, -54.25462396068649440 ) ) ;
#11078 = CARTESIAN_POINT ( 'NONE',  ( 64.31441352423868807, -32.07208572738768027, -17.57633156439366573 ) ) ;
#11079 = DIRECTION ( 'NONE',  ( -0.5110015285683607855, -0.4887508954475661693, -0.7071067811865481278 ) ) ;
#11080 = CARTESIAN_POINT ( 'NONE',  ( 62.70348755430340049, -30.98672360713329965, -16.57902117255940055 ) ) ;
#11081 = CARTESIAN_POINT ( 'NONE',  ( 71.31451227301140250, 1.097895768572089814, -60.61330028352099930 ) ) ;
#11082 = CARTESIAN_POINT ( 'NONE',  ( 11.13393739769619906, 32.00438138744689809, -43.91353227418159832 ) ) ;
#11083 = CARTESIAN_POINT ( 'NONE',  ( 72.39815743494149558, 1.277726347179370059, -61.51551921202479889 ) ) ;
#11084 = EDGE_CURVE ( 'NONE', #22139, #23745, #2922, .T. ) ;
#11085 = CARTESIAN_POINT ( 'NONE',  ( 50.95939809116894992, -35.29322421015848477, -76.37898009206955408 ) ) ;
#11086 = DIRECTION ( 'NONE',  ( 0.000000000000000000, 0.7071067811865463515, -0.7071067811865487940 ) ) ;
#11087 = ORIENTED_EDGE ( 'NONE', *, *, #11824, .F. ) ;
#11088 = ORIENTED_EDGE ( 'NONE', *, *, #51596, .F. ) ;
#11089 = DIRECTION ( 'NONE',  ( 0.7071067811865470176, -8.659560562354926695E-17, 0.7071067811865480168 ) ) ;
#11090 = CARTESIAN_POINT ( 'NONE',  ( 49.99045098147789901, -1.393666479833739702, -15.95592623815259792 ) ) ;
#11091 = ORIENTED_EDGE ( 'NONE', *, *, #1783, .F. ) ;
#11092 = EDGE_CURVE ( 'NONE', #15209, #7516, #7119, .T. ) ;
#11093 = CARTESIAN_POINT ( 'NONE',  ( 57.46797901588330149, -45.11472323586909994, -25.39910589255679696 ) ) ;
#11094 = DIRECTION ( 'NONE',  ( 1.000000000000000000, 0.000000000000000000, 0.000000000000000000 ) ) ;
#11095 = AXIS2_PLACEMENT_3D ( 'NONE', #31606, #15650, #38993 ) ;
#11096 = CARTESIAN_POINT ( 'NONE',  ( 63.52011431889719972, 1.391252479931859964, -62.52735703481241103 ) ) ;
#11098 = ORIENTED_EDGE ( 'NONE', *, *, #40702, .T. ) ;
#11097 = B_SPLINE_CURVE_WITH_KNOTS ( 'NONE', 3,
 ( #38031, #5802, #31103, #30144, #26926, #2125, #49832, #6061, #45634, #5552, #21510, #9486, #18105, #25692, #13418, #37508, #34072, #50081 ),
 .UNSPECIFIED., .F., .F.,
 ( 4, 2, 2, 2, 2, 2, 2, 2, 4 ),
 ( 0.5000015563056314782, 0.5625013617674274879, 0.6250011672292233866, 0.6875009726910192853, 0.7500007781528152950, 0.8125005836146115268, 0.8750003890764076475, 0.9375001945382037682, 1.000000000000000000 ),
 .UNSPECIFIED. ) ;
#11099 = VECTOR ( 'NONE', #43515, 999.9999999999998863 ) ;
#11100 = CARTESIAN_POINT ( 'NONE',  ( 11.32935210725529274, -20.44672669700188905, -81.20178769548542164 ) ) ;
#11101 = CARTESIAN_POINT ( 'NONE',  ( 44.41528266476777986, 6.738903454959987549, -68.24327111710597649 ) ) ;
#11102 = DIRECTION ( 'NONE',  ( 0.000000000000000000, 1.000000000000000000, 0.000000000000000000 ) ) ;
#11103 = ORIENTED_EDGE ( 'NONE', *, *, #24509, .F. ) ;
#11104 = CARTESIAN_POINT ( 'NONE',  ( 19.84088292136570075, -22.98105655655680124, -38.14390150139109892 ) ) ;
#11105 = DIRECTION ( 'NONE',  ( -0.8090169943749478954, -0.5877852522924724710, 0.000000000000000000 ) ) ;
#11106 = CARTESIAN_POINT ( 'NONE',  ( 8.996606508577366768, -19.09621130954815271, -50.64797206822856879 ) ) ;
#11107 = CARTESIAN_POINT ( 'NONE',  ( 14.62654628050830041, -22.23316257708228605, -51.02402753104211541 ) ) ;
#11108 = CARTESIAN_POINT ( 'NONE',  ( 59.28138515986110235, -28.60838227528750011, -15.68089638718410050 ) ) ;
#11109 = DIRECTION ( 'NONE',  ( 0.000000000000000000, -1.000000000000000000, 0.000000000000000000 ) ) ;
#11110 = CARTESIAN_POINT ( 'NONE',  ( 47.16986572260749710, -54.60797753722280135, -74.94873378728740931 ) ) ;
#11111 = CARTESIAN_POINT ( 'NONE',  ( -1.143840380081567076, -15.61618894467929941, -35.76111111111109864 ) ) ;
#11112 = ADVANCED_FACE ( 'NONE', ( #50364 ), #21327, .T. ) ;
#11113 = CARTESIAN_POINT ( 'NONE',  ( 29.63393739769620083, -15.61618894467929941, -1.149999999999999911 ) ) ;
#11114 = CARTESIAN_POINT ( 'NONE',  ( 83.73985275199801492, -44.66878937119359705, -47.11072319708490141 ) ) ;
#11115 = CARTESIAN_POINT ( 'NONE',  ( 16.65420337845429799, 19.88381105532299742, -20.15000000000000213 ) ) ;
#11116 = CARTESIAN_POINT ( 'NONE',  ( 9.451848358669201033, -20.44687586599430063, -32.30843786212729896 ) ) ;
#11117 = ORIENTED_EDGE ( 'NONE', *, *, #4769, .T. ) ;
#11118 = CARTESIAN_POINT ( 'NONE',  ( 55.25527325933540368, -47.47676794944560186, -26.53763385803990005 ) ) ;
#11119 = CARTESIAN_POINT ( 'NONE',  ( 7.530214027689599909, -59.71025360061080534, -11.77218490757650038 ) ) ;
#11120 = CARTESIAN_POINT ( 'NONE',  ( 76.38557192511220251, -34.90188143910140184, -13.09796983512340063 ) ) ;
#11121 = CARTESIAN_POINT ( 'NONE',  ( 75.41849744931550958, 12.82902632849465974, -13.61737176862969534 ) ) ;
#11122 = CARTESIAN_POINT ( 'NONE',  ( 75.46827467797460542, -43.69088997238642946, -13.44466669527831293 ) ) ;
#11123 = CONICAL_SURFACE ( 'NONE', #27009, 7.500000000000000000, 0.7853981633974476129 ) ;
#11124 = CARTESIAN_POINT ( 'NONE',  ( 22.90093739769620029, -15.61618894467913243, -28.45282021618999835 ) ) ;
#11125 = CIRCLE ( 'NONE', #51262, 1.000000000000000000 ) ;
#11126 = CARTESIAN_POINT ( 'NONE',  ( 11.13393739769619906, -55.30245861064819479, -24.15000000000000213 ) ) ;
#11127 = CARTESIAN_POINT ( 'NONE',  ( 82.61192755713619817, -45.25363691089199847, -47.15270809369890515 ) ) ;
#11128 = CARTESIAN_POINT ( 'NONE',  ( 57.27556706372909900, -50.61618894467930119, -53.86432103813280037 ) ) ;
#11129 = CARTESIAN_POINT ( 'NONE',  ( 41.89087154105590116, 12.34395647913080118, -3.657595757375029955 ) ) ;
#11130 = EDGE_CURVE ( 'NONE', #34780, #29238, #50615, .T. ) ;
#11131 = LINE ( 'NONE', #27098, #34252 ) ;
#11132 = CARTESIAN_POINT ( 'NONE',  ( 71.76327752318150033, -45.11618894467940066, -14.40146755345420004 ) ) ;
#11133 = DIRECTION ( 'NONE',  ( 0.000000000000000000, 0.000000000000000000, -1.000000000000000000 ) ) ;
#11134 = CARTESIAN_POINT ( 'NONE',  ( 30.68460988201149675, -15.41618894468000356, -65.65000000000004832 ) ) ;
#11135 = CARTESIAN_POINT ( 'NONE',  ( 18.46964007651970263, -51.65733818267800359, -75.17186369576970151 ) ) ;
#11136 = CARTESIAN_POINT ( 'NONE',  ( 60.85049484021050148, -43.74509675106619966, -9.364400423546438645 ) ) ;
#11137 = CARTESIAN_POINT ( 'NONE',  ( 17.78999742675459927, -22.88008318389400131, -61.49599227461889939 ) ) ;
#11138 = CARTESIAN_POINT ( 'NONE',  ( 63.64445560419389381, 1.419970371293449940, -62.18985507218640407 ) ) ;
#11139 = ORIENTED_EDGE ( 'NONE', *, *, #22029, .T. ) ;
#11140 = CARTESIAN_POINT ( 'NONE',  ( 8.799473741179280495, 31.95986279266500318, -46.67015979934819825 ) ) ;
#11141 = DIRECTION ( 'NONE',  ( 0.7071067811865475727, 0.7071067811865475727, 0.000000000000000000 ) ) ;
#11142 = CARTESIAN_POINT ( 'NONE',  ( 73.15615143370008866, 1.097085799869280009, -68.85468201266050414 ) ) ;
#11143 = CARTESIAN_POINT ( 'NONE',  ( 46.39995713829783597, 8.883003650160496534, -55.01640863334984033 ) ) ;
#11144 = DIRECTION ( 'NONE',  ( 1.000000000000000000, 0.000000000000000000, 0.000000000000000000 ) ) ;
#11145 = CARTESIAN_POINT ( 'NONE',  ( 40.92026923330519850, -45.27152901351649916, -5.766248515459809987 ) ) ;
#11146 = ORIENTED_EDGE ( 'NONE', *, *, #5904, .F. ) ;
#11147 = CARTESIAN_POINT ( 'NONE',  ( 17.75132308693969918, 20.71403734715240219, -75.77237669558989808 ) ) ;
#11148 = VERTEX_POINT ( 'NONE', #10270 ) ;
#11149 = AXIS2_PLACEMENT_3D ( 'NONE', #21747, #45366, #18088 ) ;
#11150 = B_SPLINE_CURVE_WITH_KNOTS ( 'NONE', 3,
 ( #26898, #38715, #26364, #42382, #42645, #6742, #2808, #7000, #22952, #19297 ),
 .UNSPECIFIED., .F., .F.,
 ( 4, 1, 1, 1, 1, 1, 1, 4 ),
 ( 0.000000000000000000, 0.03929582389989015601, 0.1185147549635394842, 0.1977336860271887986, 0.2769526170908375162, 0.3561715481544868722, 0.4353904792181367278, 0.4999961688222710476 ),
 .UNSPECIFIED. ) ;
#11151 = ORIENTED_EDGE ( 'NONE', *, *, #8533, .T. ) ;
#11152 = EDGE_CURVE ( 'NONE', #14552, #30210, #35006, .T. ) ;
#11153 = CARTESIAN_POINT ( 'NONE',  ( 47.13393739769619373, 8.048130187719129580, -35.14999999999999858 ) ) ;
#11154 = CARTESIAN_POINT ( 'NONE',  ( 23.59018480163760145, -15.43460167357770096, -81.23899999999999011 ) ) ;
#11155 = CARTESIAN_POINT ( 'NONE',  ( -17.31035082052260776, -35.95763326800162929, -50.10886653532376300 ) ) ;
#11156 = VERTEX_POINT ( 'NONE', #34613 ) ;
#11157 = CARTESIAN_POINT ( 'NONE',  ( 69.63393739769620083, 11.88381105532070059, -71.50000000000000000 ) ) ;
#11158 = VERTEX_POINT ( 'NONE', #19153 ) ;
#11159 = DIRECTION ( 'NONE',  ( -1.000000000000000000, 0.000000000000000000, 0.000000000000000000 ) ) ;
#11160 = CARTESIAN_POINT ( 'NONE',  ( 45.34362094574520086, -33.92716053989970248, -34.64999999999999858 ) ) ;
#11161 = CIRCLE ( 'NONE', #15348, 5.999999999999998224 ) ;
#11162 = ORIENTED_EDGE ( 'NONE', *, *, #26788, .T. ) ;
#11163 = CARTESIAN_POINT ( 'NONE',  ( 44.69938546025573345, 1.937554778470574446, -44.09236103973196919 ) ) ;
#11165 = CARTESIAN_POINT ( 'NONE',  ( 52.32303883665399979, -51.41740952823399624, -75.90202711987829787 ) ) ;
#11164 = CIRCLE ( 'NONE', #47973, 3.500000000000003109 ) ;
#11166 = CARTESIAN_POINT ( 'NONE',  ( 60.31036077509780569, 14.53093637234490032, -47.43321563248520079 ) ) ;
#11167 = ADVANCED_FACE ( 'NONE', ( #45198 ), #38570, .T. ) ;
#11168 = EDGE_CURVE ( 'NONE', #9424, #26391, #16615, .T. ) ;
#11169 = DIRECTION ( 'NONE',  ( 0.9441240636101839723, 0.3295902797598760925, 0.000000000000000000 ) ) ;
#11170 = CARTESIAN_POINT ( 'NONE',  ( 18.13393739769620083, -49.55731444163359356, -34.64999999999999858 ) ) ;
#11171 = EDGE_CURVE ( 'NONE', #17972, #48341, #6337, .T. ) ;
#11172 = DIRECTION ( 'NONE',  ( -0.000000000000000000, 1.000000000000000000, 0.000000000000000000 ) ) ;
#11173 = CARTESIAN_POINT ( 'NONE',  ( -11.32734370190460105, 10.64934056395049922, -6.430192534648650593 ) ) ;
#11174 = DIRECTION ( 'NONE',  ( -0.3502816565540492477, 0.000000000000000000, 0.9366444154970182678 ) ) ;
#11175 = DIRECTION ( 'NONE',  ( -1.000000000000000000, 0.000000000000000000, 0.000000000000000000 ) ) ;
#11176 = CARTESIAN_POINT ( 'NONE',  ( 22.67019233514569976, -11.27290452205059879, -51.10081841474480058 ) ) ;
#11177 = ORIENTED_EDGE ( 'NONE', *, *, #19963, .F. ) ;
#11178 = CARTESIAN_POINT ( 'NONE',  ( 58.91181031229810117, 15.24198406853699872, -47.44472854892460134 ) ) ;
#11179 = CIRCLE ( 'NONE', #8655, 5.251829701412229490 ) ;
#11180 = CARTESIAN_POINT ( 'NONE',  ( 57.47665759692250020, 19.32680757954669915, -53.44461618367620304 ) ) ;
#11181 = CARTESIAN_POINT ( 'NONE',  ( 71.65351305086610978, 1.028860820851649871, -70.49907908372900067 ) ) ;
#11182 = CARTESIAN_POINT ( 'NONE',  ( 45.07384444018408942, -40.03565744828185302, -61.45441968810736455 ) ) ;
#11183 = CARTESIAN_POINT ( 'NONE',  ( 13.96942586498170158, 19.12044695617580103, -20.94633231277839869 ) ) ;
#11184 = EDGE_CURVE ( 'NONE', #12868, #35817, #43467, .T. ) ;
#11185 = DIRECTION ( 'NONE',  ( -0.7071067811865492381, 0.000000000000000000, 0.7071067811865457964 ) ) ;
#11186 = EDGE_CURVE ( 'NONE', #47210, #3678, #20391, .T. ) ;
#11187 = CARTESIAN_POINT ( 'NONE',  ( 63.39331655121669939, 1.326134026835569912, -68.94513744192749982 ) ) ;
#11188 = CARTESIAN_POINT ( 'NONE',  ( 48.03353091937740516, -54.28691148336039873, -54.73610278459779721 ) ) ;
#11189 = CARTESIAN_POINT ( 'NONE',  ( 23.87475871378720882, -13.95126914312736055, -45.44025617180926702 ) ) ;
#11190 = CARTESIAN_POINT ( 'NONE',  ( 56.37791565511199821, 19.35890332112400003, -52.96495788585040287 ) ) ;
#11191 = LINE ( 'NONE', #35013, #10569 ) ;
#11192 = EDGE_LOOP ( 'NONE', ( #46252, #38805, #44398, #14563 ) ) ;
#11193 = VECTOR ( 'NONE', #38981, 1000.000000000000114 ) ;
#11194 = CARTESIAN_POINT ( 'NONE',  ( 13.75882690376460005, -22.67774291531760156, -35.67062074787899206 ) ) ;
#11195 = TOROIDAL_SURFACE ( 'NONE', #24543, 17.07000000028409659, 3.569999999987189643 ) ;
#11196 = ORIENTED_EDGE ( 'NONE', *, *, #20132, .F. ) ;
#11197 = CARTESIAN_POINT ( 'NONE',  ( 71.25608535201600091, 1.369535599030039963, -70.36855090579189209 ) ) ;
#11198 = CARTESIAN_POINT ( 'NONE',  ( 14.06333627717456736, -23.32130915692496842, -58.09100141101665571 ) ) ;
#11199 = CARTESIAN_POINT ( 'NONE',  ( 49.02351734455767485, -53.72042385326151503, -54.35736896012733865 ) ) ;
#11200 = CARTESIAN_POINT ( 'NONE',  ( 50.03007040746459921, 17.53271468411620049, -76.14999999999999147 ) ) ;
#11202 = DIRECTION ( 'NONE',  ( 0.000000000000000000, 0.000000000000000000, 1.000000000000000000 ) ) ;
#11201 = DIRECTION ( 'NONE',  ( 1.000000000000000000, -1.703274131079987031E-27, 2.066387465239710029E-12 ) ) ;
#11203 = DIRECTION ( 'NONE',  ( 0.000000000000000000, 1.000000000000000000, 0.000000000000000000 ) ) ;
#11204 = CARTESIAN_POINT ( 'NONE',  ( 9.807841437222569070, -20.47795584766477717, -42.29933489389950552 ) ) ;
#11205 = DIRECTION ( 'NONE',  ( -1.000000000000000000, 0.000000000000000000, 0.000000000000000000 ) ) ;
#11206 = EDGE_LOOP ( 'NONE', ( #9996, #1617 ) ) ;
#11207 = FACE_OUTER_BOUND ( 'NONE', #2568, .T. ) ;
#11208 = ORIENTED_EDGE ( 'NONE', *, *, #47734, .T. ) ;
#11209 = VERTEX_POINT ( 'NONE', #21752 ) ;
#11210 = DIRECTION ( 'NONE',  ( 0.000000000000000000, 0.000000000000000000, -1.000000000000000000 ) ) ;
#11211 = FACE_OUTER_BOUND ( 'NONE', #3995, .T. ) ;
#11212 = LINE ( 'NONE', #27175, #29401 ) ;
#11213 = CARTESIAN_POINT ( 'NONE',  ( 10.93697074075429931, -64.96690227797920159, -46.97388299885609797 ) ) ;
#11214 = ORIENTED_EDGE ( 'NONE', *, *, #20724, .T. ) ;
#11215 = EDGE_LOOP ( 'NONE', ( #11578, #633, #46858, #35173 ) ) ;
#11216 = CARTESIAN_POINT ( 'NONE',  ( 12.16981617636240109, -50.04926268091029584, -21.14999999999999858 ) ) ;
#11217 = CARTESIAN_POINT ( 'NONE',  ( 56.71680104101439923, 14.84105079357200019, -26.25052735258839931 ) ) ;
#11218 = CARTESIAN_POINT ( 'NONE',  ( 56.30185301883670235, -50.62326390979490043, -52.97278795026579701 ) ) ;
#11219 = AXIS2_PLACEMENT_3D ( 'NONE', #29965, #26554, #37856 ) ;
#11220 = CARTESIAN_POINT ( 'NONE',  ( 10.22108795246918689, -12.20809152911458106, -35.61948642598461134 ) ) ;
#11221 = CARTESIAN_POINT ( 'NONE',  ( 61.00510007021379977, -1.210019244661300064, -16.05925380967549998 ) ) ;
#11222 = CARTESIAN_POINT ( 'NONE',  ( 51.70526341691190453, -49.35822289825209452, -76.83585704126669214 ) ) ;
#11223 = CARTESIAN_POINT ( 'NONE',  ( 72.60719124696490212, 0.9098571636355720083, -62.44999999999999574 ) ) ;
#11224 = VERTEX_POINT ( 'NONE', #18094 ) ;
#11225 = DIRECTION ( 'NONE',  ( 0.000000000000000000, 0.000000000000000000, 1.000000000000000000 ) ) ;
#11226 = DIRECTION ( 'NONE',  ( 0.000000000000000000, 1.000000000000000000, 0.000000000000000000 ) ) ;
#11227 = CARTESIAN_POINT ( 'NONE',  ( 22.04686225415732892, -12.20822244819830438, -52.28615139641824783 ) ) ;
#11228 = PLANE ( 'NONE',  #6077 ) ;
#11229 = CARTESIAN_POINT ( 'NONE',  ( 16.63475156800449994, -7.784462905139830191, -41.53282164658689624 ) ) ;
#11230 = EDGE_CURVE ( 'NONE', #13020, #51085, #8534, .T. ) ;
#11231 = CARTESIAN_POINT ( 'NONE',  ( 12.98723924364920101, -50.01451381740049840, -21.05373175809789998 ) ) ;
#11232 = DIRECTION ( 'NONE',  ( 0.000000000000000000, 0.000000000000000000, -1.000000000000000000 ) ) ;
#11233 = ADVANCED_FACE ( 'NONE', ( #17044, #28815 ), #44816, .T. ) ;
#11234 = CARTESIAN_POINT ( 'NONE',  ( 56.21309269942560150, 13.89837739344449830, -15.33240308013389885 ) ) ;
#11235 = CARTESIAN_POINT ( 'NONE',  ( 61.02222211035100230, -45.36865808718979309, -46.91825944054690467 ) ) ;
#11236 = CIRCLE ( 'NONE', #26246, 1.000000000000000888 ) ;
#11237 = CARTESIAN_POINT ( 'NONE',  ( 71.17189893730710537, 1.387131204727280132, -70.29242575817399086 ) ) ;
#11238 = CARTESIAN_POINT ( 'NONE',  ( 13.47700760496489991, -9.082944478799580779, -46.22423246988029888 ) ) ;
#11239 = CARTESIAN_POINT ( 'NONE',  ( 46.85975247610159755, -39.63543722116869361, -54.33484572181019701 ) ) ;
#11240 = VERTEX_POINT ( 'NONE', #9693 ) ;
#11241 = CARTESIAN_POINT ( 'NONE',  ( 13.39996378792660003, -51.78681560013630047, -74.34711752987760747 ) ) ;
#11242 = CARTESIAN_POINT ( 'NONE',  ( 64.79388653638659434, 0.9272522097098119254, -60.66559564092809609 ) ) ;
#11243 = DIRECTION ( 'NONE',  ( 0.000000000000000000, 0.000000000000000000, -1.000000000000000000 ) ) ;
#11244 = CARTESIAN_POINT ( 'NONE',  ( 17.91444327278706439, 19.90989047429554404, -74.52173647802152345 ) ) ;
#11245 = CARTESIAN_POINT ( 'NONE',  ( 8.222954944519177189, -14.58051301874622929, -46.54933521620945669 ) ) ;
#11246 = DIRECTION ( 'NONE',  ( -0.7071067811865476838, -0.7071067811865473507, 0.000000000000000000 ) ) ;
#11247 = EDGE_CURVE ( 'NONE', #22605, #45901, #857, .T. ) ;
#11248 = CARTESIAN_POINT ( 'NONE',  ( 82.54540508975100011, 13.91912072063600014, -46.85689288513360395 ) ) ;
#11249 = CARTESIAN_POINT ( 'NONE',  ( 72.50969334808389988, 1.026088617261680103, -69.75574693290749906 ) ) ;
#11251 = CARTESIAN_POINT ( 'NONE',  ( 11.67619456822290047, 33.65927054772580362, -23.88710972541020183 ) ) ;
#11250 = CARTESIAN_POINT ( 'NONE',  ( 53.07820085554459411, 19.12200233530915483, -77.22362300132772361 ) ) ;
#11252 = EDGE_CURVE ( 'NONE', #13982, #48724, #45965, .T. ) ;
#11253 = DIRECTION ( 'NONE',  ( 0.000000000000000000, 1.000000000000000000, 0.000000000000000000 ) ) ;
#11254 = FACE_OUTER_BOUND ( 'NONE', #18616, .T. ) ;
#11255 = ORIENTED_EDGE ( 'NONE', *, *, #44437, .F. ) ;
#11256 = CARTESIAN_POINT ( 'NONE',  ( 53.43952110370909736, -49.36024459135060027, -48.94167683225650478 ) ) ;
#11257 = EDGE_LOOP ( 'NONE', ( #47712, #13506 ) ) ;
#11258 = CARTESIAN_POINT ( 'NONE',  ( 45.05343097613845771, 6.588082144191076850, -65.00781254588196134 ) ) ;
#11259 = CARTESIAN_POINT ( 'NONE',  ( 14.36277944305668264, -22.20708534457719452, -75.03615355444333090 ) ) ;
#11260 = CARTESIAN_POINT ( 'NONE',  ( 13.87199023920160101, 19.96799697009089769, -22.54889071416870294 ) ) ;
#11261 = CARTESIAN_POINT ( 'NONE',  ( 14.19855276898660001, 24.33696219936630101, -76.14999999999999147 ) ) ;
#11262 = CARTESIAN_POINT ( 'NONE',  ( 20.01090992632330057, -21.50784768470290231, -58.76756083737610226 ) ) ;
#11263 = AXIS2_PLACEMENT_3D ( 'NONE', #36884, #21145, #40558 ) ;
#11264 = CARTESIAN_POINT ( 'NONE',  ( 52.89232545687240616, 18.42626852396410086, -48.97387498997640165 ) ) ;
#11265 = CARTESIAN_POINT ( 'NONE',  ( 55.29971770016739896, -46.05203773004579659, -16.43383186550930120 ) ) ;
#11266 = CARTESIAN_POINT ( 'NONE',  ( 53.46882080935260007, 17.64232885596709721, -26.54419876889340202 ) ) ;
#11267 = VERTEX_POINT ( 'NONE', #25909 ) ;
#11268 = VECTOR ( 'NONE', #50379, 1000.000000000000000 ) ;
#11269 = CARTESIAN_POINT ( 'NONE',  ( 18.87553618764729890, -8.262932233661949510, -38.90110303094750321 ) ) ;
#11270 = ORIENTED_EDGE ( 'NONE', *, *, #26536, .F. ) ;
#11271 = CARTESIAN_POINT ( 'NONE',  ( 11.94527162332230041, -65.41218007247690025, -17.48520172073260071 ) ) ;
#11272 = FACE_OUTER_BOUND ( 'NONE', #37201, .T. ) ;
#11273 = CARTESIAN_POINT ( 'NONE',  ( 72.76128204928120624, 1.388313565858570131, -62.46994910431339321 ) ) ;
#11274 = DIRECTION ( 'NONE',  ( 1.000000000000000000, 0.000000000000000000, 0.000000000000000000 ) ) ;
#11275 = CARTESIAN_POINT ( 'NONE',  ( 53.55176271296412693, -49.41894048401645989, -49.22385363220949017 ) ) ;
#11276 = CARTESIAN_POINT ( 'NONE',  ( 11.51160566532390028, -51.12796951774690513, -23.15000000000000213 ) ) ;
#11277 = CARTESIAN_POINT ( 'NONE',  ( 53.42313316096070253, -52.07210377827539816, -54.29429654136570349 ) ) ;
#11278 = VERTEX_POINT ( 'NONE', #41922 ) ;
#11279 = DIRECTION ( 'NONE',  ( -0.000000000000000000, -1.000000000000000000, -0.000000000000000000 ) ) ;
#11280 = CARTESIAN_POINT ( 'NONE',  ( 10.49009406874180073, -63.23676620627490053, -45.62574497862269851 ) ) ;
#11281 = CARTESIAN_POINT ( 'NONE',  ( 67.04038824939809160, 19.47158195952189885, -72.59354914830210248 ) ) ;
#11282 = ORIENTED_EDGE ( 'NONE', *, *, #19161, .F. ) ;
#11283 = CARTESIAN_POINT ( 'NONE',  ( 11.13393738245069642, -63.63465678867208197, -43.78329441304022396 ) ) ;
#11284 = CARTESIAN_POINT ( 'NONE',  ( 57.07649178892390296, 19.21884141067920027, -53.03413607196730339 ) ) ;
#11285 = VECTOR ( 'NONE', #36091, 1000.000000000000000 ) ;
#11286 = CARTESIAN_POINT ( 'NONE',  ( 23.99766558267342376, -14.69524935265806853, -49.47055337157053856 ) ) ;
#11287 =( BOUNDED_CURVE ( )  B_SPLINE_CURVE ( 3, ( #22069, #10819, #6624, #42013 ),
 .UNSPECIFIED., .F., .T. ) 
 B_SPLINE_CURVE_WITH_KNOTS ( ( 4, 4 ),
 ( 5.497787143782005614, 6.283185307179586232 ),
 .UNSPECIFIED. ) 
 CURVE ( )  GEOMETRIC_REPRESENTATION_ITEM ( )  RATIONAL_B_SPLINE_CURVE ( ( 1.000000000000000000, 0.9492530216741742466, 0.9492530216741742466, 1.000000000000000000 ) ) 
 REPRESENTATION_ITEM ( '' )  );
#11288 = ORIENTED_EDGE ( 'NONE', *, *, #17434, .F. ) ;
#11289 = CARTESIAN_POINT ( 'NONE',  ( 25.90218739769619916, -15.61618894467930119, -18.08174999999999955 ) ) ;
#11290 = CARTESIAN_POINT ( 'NONE',  ( 51.98443725223855694, 20.13520455629937445, -75.98853295767540317 ) ) ;
#11291 = CARTESIAN_POINT ( 'NONE',  ( 19.63028852933850388, -21.45851978622926381, -32.78102164913964600 ) ) ;
#11292 = CARTESIAN_POINT ( 'NONE',  ( 24.91854708852281419, -6.831579253852850364, -22.15000000000000924 ) ) ;
#11293 = CARTESIAN_POINT ( 'NONE',  ( 11.82717660292169803, -8.585219487162939700, -61.11739150984070079 ) ) ;
#11294 = VECTOR ( 'NONE', #41379, 1000.000000000000000 ) ;
#11295 = ADVANCED_FACE ( 'NONE', ( #21981 ), #11660, .F. ) ;
#11296 = DIRECTION ( 'NONE',  ( 0.000000000000000000, -1.000000000000000000, 0.000000000000000000 ) ) ;
#11297 = CARTESIAN_POINT ( 'NONE',  ( 46.74119668981005304, -38.22629118898348111, -56.61365389520171476 ) ) ;
#11298 = DIRECTION ( 'NONE',  ( 1.000000000000000000, 0.000000000000000000, 0.000000000000000000 ) ) ;
#11299 = ORIENTED_EDGE ( 'NONE', *, *, #50279, .T. ) ;
#11300 = VERTEX_POINT ( 'NONE', #49024 ) ;
#11301 = CYLINDRICAL_SURFACE ( 'NONE', #45963, 2.000000000000003997 ) ;
#11302 = CARTESIAN_POINT ( 'NONE',  ( 23.44411912466889802, -14.17815663496550016, -56.17083000281660077 ) ) ;
#11303 = CARTESIAN_POINT ( 'NONE',  ( 48.23725916559990168, 13.88381105525269987, -9.350495514648539341 ) ) ;
#11304 = CARTESIAN_POINT ( 'NONE',  ( 41.64265090550289727, -46.42699119286240261, -4.296538310234230273 ) ) ;
#11305 = CARTESIAN_POINT ( 'NONE',  ( 46.47158024012890110, 21.92595096433829838, -76.13722091323529639 ) ) ;
#11306 = VECTOR ( 'NONE', #27026, 1000.000000000000114 ) ;
#11307 = DIRECTION ( 'NONE',  ( 0.000000000000000000, 3.858025010473989332E-12, 1.000000000000000000 ) ) ;
#11308 = B_SPLINE_CURVE_WITH_KNOTS ( 'NONE', 3,
 ( #45487, #21606, #25539, #1716, #24492, #44700, #33668, #8805, #13777, #33410, #48911 ),
 .UNSPECIFIED., .F., .F.,
 ( 4, 1, 1, 1, 1, 1, 1, 1, 4 ),
 ( 0.000000000000000000, 0.009449720072804113427, 0.08866865113642231899, 0.1678875822000404916, 0.2471065132636587058, 0.3263254443272768923, 0.4055443753908951066, 0.4847633064545138759, 0.5000038964883081194 ),
 .UNSPECIFIED. ) ;
#11309 = CARTESIAN_POINT ( 'NONE',  ( 68.13393739769790614, -49.95860450174040324, -75.14853292321149070 ) ) ;
#11310 = CARTESIAN_POINT ( 'NONE',  ( 12.16177399483199828, 33.87933705409069773, -16.53048058984360225 ) ) ;
#11311 = CARTESIAN_POINT ( 'NONE',  ( 10.14973811047410024, -9.944145256573110103, -68.74914615139218199 ) ) ;
#11312 = EDGE_CURVE ( 'NONE', #40977, #3031, #49281, .T. ) ;
#11313 = CARTESIAN_POINT ( 'NONE',  ( 52.63509980015960110, -49.78733083141809601, -27.75246021167879817 ) ) ;
#11314 = CARTESIAN_POINT ( 'NONE',  ( 54.52355283502430439, -50.61618499730730036, -76.78771584484479718 ) ) ;
#11316 = CARTESIAN_POINT ( 'NONE',  ( 22.04683803730932112, -12.20817710762339559, -60.28613482586189321 ) ) ;
#11315 = CARTESIAN_POINT ( 'NONE',  ( -0.2630675345621850125, 21.64344005583900099, -7.960913005788690988 ) ) ;
#11318 = ADVANCED_FACE ( 'NONE', ( #37469 ), #32593, .T. ) ;
#11317 = CARTESIAN_POINT ( 'NONE',  ( 20.47328261930381643, 10.62527906362196717, -34.70142521051216988 ) ) ;
#11319 = FACE_OUTER_BOUND ( 'NONE', #1971, .T. ) ;
#11320 = CARTESIAN_POINT ( 'NONE',  ( -18.86606260230390220, 19.38381105532060289, 16.21999999999999886 ) ) ;
#11321 = ORIENTED_EDGE ( 'NONE', *, *, #1960, .T. ) ;
#11322 = CARTESIAN_POINT ( 'NONE',  ( 23.49471107959579896, 17.21388800241559736, -41.74835363994539961 ) ) ;
#11323 = CARTESIAN_POINT ( 'NONE',  ( 47.71564501992030216, 23.23377652775180024, -54.78142672066789487 ) ) ;
#11324 = CARTESIAN_POINT ( 'NONE',  ( 57.58883330952520652, -45.77669918862839893, -26.30132602238209927 ) ) ;
#11325 = CARTESIAN_POINT ( 'NONE',  ( 63.25144821230251324, 0.9425424353906030062, -62.16269173205530763 ) ) ;
#11326 = CARTESIAN_POINT ( 'NONE',  ( 61.18397614727650335, 14.12635359917990030, -47.22202979286220170 ) ) ;
#11327 = CARTESIAN_POINT ( 'NONE',  ( 14.41814848605539900, -8.366170860851109836, -75.65868704446700121 ) ) ;
#11328 = CARTESIAN_POINT ( 'NONE',  ( 51.57818300252989729, 18.30842999037989927, -76.64184120677319356 ) ) ;
#11329 = CARTESIAN_POINT ( 'NONE',  ( 52.79916028495409819, 18.44511419399770347, -48.53935649295149801 ) ) ;
#11330 = DIRECTION ( 'NONE',  ( 0.000000000000000000, -1.000000000000000000, 0.000000000000000000 ) ) ;
#11331 = CARTESIAN_POINT ( 'NONE',  ( -0.2240635586800976686, -45.43677584701738681, -34.96139953375227805 ) ) ;
#11332 = CARTESIAN_POINT ( 'NONE',  ( 52.81882390656510040, 18.43111101854420042, -28.02887802125319894 ) ) ;
#11333 = CARTESIAN_POINT ( 'NONE',  ( 50.68559394812662333, 4.538207541409860823, -76.25990402181635375 ) ) ;
#11334 = CARTESIAN_POINT ( 'NONE',  ( 22.07209798807642187, -20.84472431681153992, -61.73745665553851580 ) ) ;
#11335 = DIRECTION ( 'NONE',  ( 1.000000000000000000, 0.000000000000000000, 0.000000000000000000 ) ) ;
#11336 = LINE ( 'NONE', #39626, #33587 ) ;
#11337 = CARTESIAN_POINT ( 'NONE',  ( 58.93926773726619928, -28.47565881710299962, -15.64941876695289835 ) ) ;
#11338 = CARTESIAN_POINT ( 'NONE',  ( 71.21254218222989607, 1.330484379554840002, -60.80906431331560213 ) ) ;
#11339 = FACE_OUTER_BOUND ( 'NONE', #946, .T. ) ;
#11340 = CARTESIAN_POINT ( 'NONE',  ( 72.48245069165039922, 1.197080272271600077, -61.55408047754139744 ) ) ;
#11341 = DIRECTION ( 'NONE',  ( 0.000000000000000000, -1.000000000000000000, 0.000000000000000000 ) ) ;
#11342 = CARTESIAN_POINT ( 'NONE',  ( 21.66748157623074889, -11.66111095713660362, -66.25520808017488150 ) ) ;
#11343 = ORIENTED_EDGE ( 'NONE', *, *, #37973, .T. ) ;
#11344 = ORIENTED_EDGE ( 'NONE', *, *, #30139, .T. ) ;
#11345 = CARTESIAN_POINT ( 'NONE',  ( 16.35280278772694018, -15.45717393091348590, -41.53556505950739819 ) ) ;
#11346 = CIRCLE ( 'NONE', #42281, 6.766999999999998572 ) ;
#11347 = DIRECTION ( 'NONE',  ( 0.000000000000000000, 0.000000000000000000, 1.000000000000000000 ) ) ;
#11348 = VERTEX_POINT ( 'NONE', #50310 ) ;
#11349 = CARTESIAN_POINT ( 'NONE',  ( 56.67477918058570197, -45.29516814663779911, -25.36359513125130150 ) ) ;
#11350 = CARTESIAN_POINT ( 'NONE',  ( 22.39879365395156086, -20.46795300909408155, -77.71742782580190578 ) ) ;
#11351 = ORIENTED_EDGE ( 'NONE', *, *, #25299, .T. ) ;
#11352 = CARTESIAN_POINT ( 'NONE',  ( 22.52288591994712164, -13.38583005777697466, -80.34591106198659816 ) ) ;
#11353 = CARTESIAN_POINT ( 'NONE',  ( 44.20159454932027643, 6.711260822063675135, -69.31168125965361071 ) ) ;
#11354 = CARTESIAN_POINT ( 'NONE',  ( 11.24122293634809999, 33.45921853044769989, -23.69861594586010156 ) ) ;
#11355 = ORIENTED_EDGE ( 'NONE', *, *, #2480, .T. ) ;
#11356 = CARTESIAN_POINT ( 'NONE',  ( 49.92842301056370502, -45.11618894467940066, -10.23644921156189902 ) ) ;
#11357 = EDGE_CURVE ( 'NONE', #46486, #30000, #2341, .T. ) ;
#11358 = CARTESIAN_POINT ( 'NONE',  ( 51.87294918393343579, 1.517735892164268963, -18.77191922990750328 ) ) ;
#11359 = CARTESIAN_POINT ( 'NONE',  ( 18.25786897914040452, -23.25431244405651299, -50.20598339505968966 ) ) ;
#11360 =( LENGTH_UNIT ( ) NAMED_UNIT ( * ) SI_UNIT ( .MILLI., .METRE. ) );
#11361 = ADVANCED_FACE ( 'NONE', ( #6803 ), #14911, .T. ) ;
#11362 = CARTESIAN_POINT ( 'NONE',  ( 65.38525663775149610, -30.59946264837140006, -16.65175604392959841 ) ) ;
#11363 = B_SPLINE_CURVE_WITH_KNOTS ( 'NONE', 3,
 ( #27281, #43290, #7379, #23328, #39353, #3452, #28293, #782, #13132, #20433, #29082, #40882, #45078, #36679, #12333, #9188, #25140, #20955 ),
 .UNSPECIFIED., .F., .F.,
 ( 4, 2, 2, 2, 2, 2, 2, 2, 4 ),
 ( 0.000000000000000000, 0.2499999999999950595, 0.3749999999999915623, 0.4374999999999900080, 0.4687499999999898970, 0.4999999999999897859, 0.6249999999999922284, 0.7499999999999945599, 1.000000000000000000 ),
 .UNSPECIFIED. ) ;
#11364 = EDGE_CURVE ( 'NONE', #46679, #9855, #10841, .T. ) ;
#11365 = CARTESIAN_POINT ( 'NONE',  ( 63.23867883281550206, 0.9065823421260940096, -62.18054194328749418 ) ) ;
#11366 = CARTESIAN_POINT ( 'NONE',  ( 47.20687114674009877, -54.68447329799499812, -74.72520730820738777 ) ) ;
#11367 = CARTESIAN_POINT ( 'NONE',  ( 14.32661840841879908, -7.979413076383879755, -75.43852414181590404 ) ) ;
#11368 = CARTESIAN_POINT ( 'NONE',  ( 17.98749078828947745, -41.76263555408611694, -34.79644660940672907 ) ) ;
#11369 = CARTESIAN_POINT ( 'NONE',  ( 41.02379277421620429, 14.08177072860459944, -5.860738561689210258 ) ) ;
#11370 = EDGE_CURVE ( 'NONE', #48656, #32778, #29205, .T. ) ;
#11371 = VECTOR ( 'NONE', #16987, 1000.000000000000000 ) ;
#11372 = DIRECTION ( 'NONE',  ( 0.5516667872527503125, -0.8340645993220362486, 0.000000000000000000 ) ) ;
#11373 = CARTESIAN_POINT ( 'NONE',  ( 83.58813978703560110, -44.72666681364290042, -46.95981403914270658 ) ) ;
#11374 = ADVANCED_FACE ( 'NONE', ( #32408 ), #36111, .T. ) ;
#11375 = CARTESIAN_POINT ( 'NONE',  ( 57.75721184438519629, 13.88381124262000021, -25.37415236305640320 ) ) ;
#11376 = CARTESIAN_POINT ( 'NONE',  ( 19.82180142157249847, -22.29872327844429947, -81.62651318459289485 ) ) ;
#11377 = B_SPLINE_SURFACE_WITH_KNOTS ( 'NONE', 3, 3, ( 
 ( #10132, #17224, #26090, #33184, #42098, #5432, #49715, #30284, #9616, #13803, #21899, #25570, #45779, #6202, #37137, #10391 ),
 ( #22156, #37392, #41576, #38168, #13552, #1493, #14315, #5178, #45262, #21637, #33444, #2264, #37910, #29515, #5941, #5688 ),
 ( #37645, #1745, #17477, #1233, #17728, #46303, #18238, #49461, #49204, #29256, #34205, #45520, #50226, #17984, #21133, #13296 ),
 ( #14059, #9369, #41319, #9868, #33699, #29760, #25823, #41836, #21387, #25316, #30018, #2004, #33950, #49968, #46044, #39914 ),
 ( #20230, #4258, #31762, #23639, #51203, #48037, #6461, #22419, #15552, #47780, #7431, #39403, #35720, #15295, #28091, #40165 ),
 ( #51457, #8198, #19971, #19474, #19730, #12136, #11888, #44097, #84, #327, #16058, #43844, #24141, #38422, #15798, #32011 ),
 ( #36218, #2525, #16312, #19215, #32266, #51706, #27587, #43591, #48289, #7697, #23890, #11369, #35197, #27332, #12384, #3506 ),
 ( #42359, #31250, #47279, #39655, #43338, #35967, #23379, #35461, #31508, #4009, #47527, #11625, #3761, #27844, #7942, #4778 ),
 ( #17614, #5569, #41449, #17101, #8978, #36473, #33322, #44350, #8457, #840, #33053, #44607, #24665, #21008, #578, #13437 ) ),
 .UNSPECIFIED., .F., .F., .F.,
 ( 4, 1, 1, 1, 1, 1, 4 ),
 ( 4, 2, 2, 2, 2, 2, 2, 4 ),
 ( 0.000000000000000000, 0.1666666666666670182, 0.3333333333333329818, 0.5000000000000000000, 0.6666666666666670737, 0.8333333333333330373, 1.000018175590269953 ),
 ( -6.893240790936180140, -6.545934836083509900, -4.902226309511959812, -3.475139087181930098, -2.335777911127269846, -1.766097323099940164, -1.310352852678080104, -1.260096513052359812 ),
 .UNSPECIFIED. ) ;
#11378 = ORIENTED_EDGE ( 'NONE', *, *, #20506, .T. ) ;
#11379 = CARTESIAN_POINT ( 'NONE',  ( 56.24801412391880007, -46.41377194224050129, -26.27554225235660468 ) ) ;
#11380 = CARTESIAN_POINT ( 'NONE',  ( 5.823743871885240786, -59.81362112911330087, -13.76841564489329883 ) ) ;
#11381 = CARTESIAN_POINT ( 'NONE',  ( 75.27120125568490039, -12.48297921181119996, -11.39499376737289893 ) ) ;
#11383 = EDGE_CURVE ( 'NONE', #8604, #42604, #12273, .T. ) ;
#11382 = DIRECTION ( 'NONE',  ( 0.000000000000000000, 0.000000000000000000, 1.000000000000000000 ) ) ;
#11384 = LINE ( 'NONE', #44365, #49098 ) ;
#11385 = DIRECTION ( 'NONE',  ( -0.9876883405951387696, -0.1564344650402249015, 0.000000000000000000 ) ) ;
#11386 = CARTESIAN_POINT ( 'NONE',  ( 20.11810147990814457, -22.52869253661944526, -38.12566692794859335 ) ) ;
#11387 = CARTESIAN_POINT ( 'NONE',  ( 63.09706677394889596, 1.198183261254780030, -62.58868501588759869 ) ) ;
#11388 = CARTESIAN_POINT ( 'NONE',  ( 57.26468601612680231, -50.61618894467930119, -53.86352240777100064 ) ) ;
#11389 = CARTESIAN_POINT ( 'NONE',  ( 43.52841460851590227, 12.16320807519920066, -4.940445812209770082 ) ) ;
#11390 = DIRECTION ( 'NONE',  ( 0.000000000000000000, 0.000000000000000000, 1.000000000000000000 ) ) ;
#11391 = CYLINDRICAL_SURFACE ( 'NONE', #14048, 2.000000000000000000 ) ;
#11392 = CARTESIAN_POINT ( 'NONE',  ( 56.57055814460980514, -47.72537394096760011, -48.17140897430749646 ) ) ;
#11393 = DIRECTION ( 'NONE',  ( 0.000000000000000000, 0.000000000000000000, -1.000000000000000000 ) ) ;
#11394 = CARTESIAN_POINT ( 'NONE',  ( 19.54190960938017341, -21.52911196706135755, -62.78615272955352822 ) ) ;
#11395 = CARTESIAN_POINT ( 'NONE',  ( 18.31744345942739827, -52.17403775882070249, -75.62474771911479365 ) ) ;
#11396 = CARTESIAN_POINT ( 'NONE',  ( 50.32921795836180223, -43.79877554599289624, -6.640512624164829347 ) ) ;
#11397 = CARTESIAN_POINT ( 'NONE',  ( 18.37840078928829968, -8.512029710671050964, -64.66474951716369901 ) ) ;
#11398 = CARTESIAN_POINT ( 'NONE',  ( 24.04493739357032212, -14.58064507484895600, -77.75066183485554916 ) ) ;
#11399 = CARTESIAN_POINT ( 'NONE',  ( 63.41597899531610238, 1.309820314134120034, -62.24970190930920211 ) ) ;
#11400 = ORIENTED_EDGE ( 'NONE', *, *, #50754, .T. ) ;
#11401 = CARTESIAN_POINT ( 'NONE',  ( 88.13393739769620083, 17.38381105532069881, -65.65000000000000568 ) ) ;
#11402 = DIRECTION ( 'NONE',  ( 0.000000000000000000, -1.000000000000000000, 0.000000000000000000 ) ) ;
#11403 = CARTESIAN_POINT ( 'NONE',  ( 73.15108049798000422, 0.8888742037077609348, -68.94068779328439689 ) ) ;
#11404 = CARTESIAN_POINT ( 'NONE',  ( 45.86779753676328397, 8.854011588677400013, -57.59996879060989272 ) ) ;
#11405 = ADVANCED_FACE ( 'NONE', ( #8599 ), #2564, .T. ) ;
#11406 = VECTOR ( 'NONE', #18836, 1000.000000000000000 ) ;
#11407 = CARTESIAN_POINT ( 'NONE',  ( 11.35884076446889956, -9.662862216420530004, -81.23899999999999011 ) ) ;
#11408 = ORIENTED_EDGE ( 'NONE', *, *, #38654, .T. ) ;
#11409 = CARTESIAN_POINT ( 'NONE',  ( 18.05058737638259814, 20.91286242874560131, -75.79069550273320033 ) ) ;
#11410 = AXIS2_PLACEMENT_3D ( 'NONE', #51499, #3285, #19000 ) ;
#11411 = ORIENTED_EDGE ( 'NONE', *, *, #13957, .T. ) ;
#11412 = ORIENTED_EDGE ( 'NONE', *, *, #32524, .T. ) ;
#11413 = CARTESIAN_POINT ( 'NONE',  ( 56.92059784994150107, -45.11618894467940066, -15.82169481042769732 ) ) ;
#11414 = CARTESIAN_POINT ( 'NONE',  ( 23.53330766295639975, -16.05940602913920046, -81.23899999999999011 ) ) ;
#11415 = B_SPLINE_CURVE_WITH_KNOTS ( 'NONE', 3,
 ( #30842, #10698, #34255, #35038 ),
 .UNSPECIFIED., .F., .F.,
 ( 4, 4 ),
 ( 0.000000000000000000, 1.000000000000000000 ),
 .UNSPECIFIED. ) ;
#11416 = CARTESIAN_POINT ( 'NONE',  ( 9.221491376032949105, -11.63192568655906811, -72.95899817687167399 ) ) ;
#11417 = ORIENTED_EDGE ( 'NONE', *, *, #15680, .F. ) ;
#11418 = CARTESIAN_POINT ( 'NONE',  ( 14.22291958798985156, -9.076607112612990136, -79.86215060077572048 ) ) ;
#11419 = VERTEX_POINT ( 'NONE', #721 ) ;
#11420 = DIRECTION ( 'NONE',  ( 0.2260571801428170324, 0.000000000000000000, -0.9741140340359940586 ) ) ;
#11421 = DIRECTION ( 'NONE',  ( 0.000000000000000000, 0.000000000000000000, 1.000000000000000000 ) ) ;
#11422 = VERTEX_POINT ( 'NONE', #33460 ) ;
#11423 = EDGE_CURVE ( 'NONE', #17025, #7773, #41764, .T. ) ;
#11424 = CARTESIAN_POINT ( 'NONE',  ( 9.429374979154360403, -19.86130208636912542, -50.32791445271212183 ) ) ;
#11425 = CARTESIAN_POINT ( 'NONE',  ( 52.35627137497320405, -51.18167454132500183, -76.02218069147700419 ) ) ;
#11426 = CARTESIAN_POINT ( 'NONE',  ( 60.64220689335409986, 14.52815193633730040, -47.73569869354479778 ) ) ;
#11427 = AXIS2_PLACEMENT_3D ( 'NONE', #25859, #9650, #46600 ) ;
#11428 = EDGE_CURVE ( 'NONE', #12119, #28125, #5626, .T. ) ;
#11429 = AXIS2_PLACEMENT_3D ( 'NONE', #35092, #39557, #51093 ) ;
#11430 = CARTESIAN_POINT ( 'NONE',  ( 15.36759654800740016, 19.45617199961630206, -15.64999998510980106 ) ) ;
#11431 = DIRECTION ( 'NONE',  ( 1.000000000000000000, 8.701345253104295327E-30, 2.840828347717470042E-11 ) ) ;
#11432 = CARTESIAN_POINT ( 'NONE',  ( -4.916317923618620078, 16.33985541905360250, -5.410848070223339690 ) ) ;
#11433 =( BOUNDED_CURVE ( )  B_SPLINE_CURVE ( 3, ( #11566, #19668, #42765, #51139 ),
 .UNSPECIFIED., .F., .T. ) 
 B_SPLINE_CURVE_WITH_KNOTS ( ( 4, 4 ),
 ( 0.3709736340029385904, 0.5134355668666845673 ),
 .UNSPECIFIED. ) 
 CURVE ( )  GEOMETRIC_REPRESENTATION_ITEM ( )  RATIONAL_B_SPLINE_CURVE ( ( 1.000000000000000000, 0.9983094314627841692, 0.9983094314627841692, 1.000000000000000000 ) ) 
 REPRESENTATION_ITEM ( '' )  );
#11434 = CARTESIAN_POINT ( 'NONE',  ( 0.7461747575532640120, -22.48794087071790315, -34.70985242058460329 ) ) ;
#11435 = CIRCLE ( 'NONE', #32303, 1.999999999999999556 ) ;
#11436 = EDGE_CURVE ( 'NONE', #9073, #8299, #2447, .T. ) ;
#11437 = CARTESIAN_POINT ( 'NONE',  ( 9.367002091613079173, -15.61601527432330094, -39.84717978380999881 ) ) ;
#11438 = CARTESIAN_POINT ( 'NONE',  ( 22.03794483230869972, -20.78624159385250181, -49.51643979347250024 ) ) ;
#11439 = ORIENTED_EDGE ( 'NONE', *, *, #49546, .T. ) ;
#11440 = CIRCLE ( 'NONE', #6424, 0.4999999999856508115 ) ;
#11441 = CARTESIAN_POINT ( 'NONE',  ( 56.57438608668749680, -50.73277124350089906, -53.83822343189740423 ) ) ;
#11442 = CARTESIAN_POINT ( 'NONE',  ( 57.37416030811479573, 19.38381105532069881, -53.87117748315449717 ) ) ;
#11444 = ADVANCED_FACE ( 'NONE', ( #41854 ), #13428, .T. ) ;
#11443 = CARTESIAN_POINT ( 'NONE',  ( 71.66763488949699479, 0.9543424661145570864, -70.49936564611709855 ) ) ;
#11445 = CARTESIAN_POINT ( 'NONE',  ( 45.82950911773824032, -40.08398659257233732, -57.78639530639727440 ) ) ;
#11446 = DIRECTION ( 'NONE',  ( 0.000000000000000000, 0.9319748226751540798, -0.3625230060280524302 ) ) ;
#11447 = CARTESIAN_POINT ( 'NONE',  ( 12.28937881627030038, 18.77527563989950110, -21.14656491300549845 ) ) ;
#11448 = CARTESIAN_POINT ( 'NONE',  ( 63.33388541776019309, 1.264121749638649872, -68.99682374033621102 ) ) ;
#11449 = CARTESIAN_POINT ( 'NONE',  ( 48.88334854381270134, -54.00587892617620156, -55.28861537459440001 ) ) ;
#11450 = CARTESIAN_POINT ( 'NONE',  ( -18.43768031504652072, -52.44180990538531262, -54.46295789858312730 ) ) ;
#11451 = AXIS2_PLACEMENT_3D ( 'NONE', #50179, #30499, #14788 ) ;
#11452 = CARTESIAN_POINT ( 'NONE',  ( 53.29384558423090112, 19.31433099946569953, -48.47378032971769812 ) ) ;
#11453 = CARTESIAN_POINT ( 'NONE',  ( 47.81228839791550200, 23.19211001100039837, -54.83188706475510088 ) ) ;
#11454 = ORIENTED_EDGE ( 'NONE', *, *, #33456, .T. ) ;
#11455 = CARTESIAN_POINT ( 'NONE',  ( 10.33272111206849964, -19.62722883991240153, -79.65462137872758319 ) ) ;
#11456 = B_SPLINE_CURVE_WITH_KNOTS ( 'NONE', 3,
 ( #9340, #37615, #29487, #1980, #5664, #42074, #6176, #22135, #33673, #38142 ),
 .UNSPECIFIED., .F., .F.,
 ( 4, 1, 1, 1, 1, 1, 1, 4 ),
 ( 0.000000000000000000, 0.07025396515245213580, 0.1494728962160721542, 0.2286918272796876761, 0.3079107583433076667, 0.3871296894069435335, 0.4663486204705432625, 0.5000017723907246303 ),
 .UNSPECIFIED. ) ;
#11457 = ORIENTED_EDGE ( 'NONE', *, *, #29038, .T. ) ;
#11458 = CARTESIAN_POINT ( 'NONE',  ( 18.30675733062039967, 21.00530369360563299, -75.65677362367951275 ) ) ;
#11459 = CARTESIAN_POINT ( 'NONE',  ( 60.31614849589169580, -45.76049255903560464, -47.43342490989579829 ) ) ;
#11460 = VECTOR ( 'NONE', #9690, 1000.000000000000000 ) ;
#11461 = CARTESIAN_POINT ( 'NONE',  ( 56.23228709081130461, -47.87823924875339543, -47.98841366488070292 ) ) ;
#11462 = DIRECTION ( 'NONE',  ( 0.3535533905932784493, 0.6123724356957970238, 0.7071067811865430208 ) ) ;
#11464 = FACE_OUTER_BOUND ( 'NONE', #19895, .T. ) ;
#11463 = CARTESIAN_POINT ( 'NONE',  ( 82.91592277202030914, 14.33044519534860051, -47.63723459745410338 ) ) ;
#11465 = ADVANCED_FACE ( 'NONE', ( #46784 ), #26838, .T. ) ;
#11466 = CARTESIAN_POINT ( 'NONE',  ( 29.24327964038718619, 4.516725609936003139, -84.62771067598525576 ) ) ;
#11467 = LINE ( 'NONE', #7784, #41198 ) ;
#11468 = ORIENTED_EDGE ( 'NONE', *, *, #36349, .T. ) ;
#11469 = CARTESIAN_POINT ( 'NONE',  ( -1.120159439602289808, -49.66006368695019546, -9.067476037955330526 ) ) ;
#11470 = EDGE_CURVE ( 'NONE', #50723, #11026, #45132, .T. ) ;
#11471 = VERTEX_POINT ( 'NONE', #38386 ) ;
#11472 = ORIENTED_EDGE ( 'NONE', *, *, #18678, .F. ) ;
#11473 = FACE_OUTER_BOUND ( 'NONE', #11192, .T. ) ;
#11474 = CARTESIAN_POINT ( 'NONE',  ( 76.72600243236601614, -38.56416636073712567, -14.20129635329269213 ) ) ;
#11475 = CARTESIAN_POINT ( 'NONE',  ( 11.13041996959340096, -64.93485056432389513, -46.76691452483890288 ) ) ;
#11476 = AXIS2_PLACEMENT_3D ( 'NONE', #44846, #5280, #12619 ) ;
#11477 = VERTEX_POINT ( 'NONE', #42848 ) ;
#11478 = ORIENTED_EDGE ( 'NONE', *, *, #50164, .T. ) ;
#11479 = DIRECTION ( 'NONE',  ( 0.000000000000000000, 0.000000000000000000, 1.000000000000000000 ) ) ;
#11480 = DIRECTION ( 'NONE',  ( 0.4743737082415266926, 0.8803235683140505641, 0.000000000000000000 ) ) ;
#11481 = CARTESIAN_POINT ( 'NONE',  ( 21.68571409299283559, 1.614639264107643246, -34.79644660940672907 ) ) ;
#11482 = CARTESIAN_POINT ( 'NONE',  ( 55.80143501159730590, 17.65504461344360010, -53.84278118897309895 ) ) ;
#11483 = CARTESIAN_POINT ( 'NONE',  ( 59.21739082243699670, -2.567626630675630128, -15.67947117406909996 ) ) ;
#11484 = CARTESIAN_POINT ( 'NONE',  ( 51.51548137828859808, -48.78072553410009249, -76.79511588528808375 ) ) ;
#11485 = CARTESIAN_POINT ( 'NONE',  ( 58.12686860087589480, -49.47667484878260780, -51.90689371356720017 ) ) ;
#11486 = EDGE_CURVE ( 'NONE', #16929, #31343, #5818, .T. ) ;
#11487 = EDGE_LOOP ( 'NONE', ( #45954, #49086, #16890, #39999, #13486 ) ) ;
#11488 = CARTESIAN_POINT ( 'NONE',  ( 63.93393739769609141, 10.88381105532070059, -62.44999999999999574 ) ) ;
#11489 = CARTESIAN_POINT ( 'NONE',  ( 22.90103018812914115, -15.61618888866172483, -50.84718209631233066 ) ) ;
#11490 = DIRECTION ( 'NONE',  ( 1.000000000000000000, 0.000000000000000000, 0.000000000000000000 ) ) ;
#11491 = CARTESIAN_POINT ( 'NONE',  ( 46.63393739769619373, 4.883811055320659733, -35.14999999999999858 ) ) ;
#11492 = EDGE_CURVE ( 'NONE', #218, #50974, #22806, .T. ) ;
#11493 = CARTESIAN_POINT ( 'NONE',  ( 23.27962512014929786, -18.86055245155780113, -52.14815840911190037 ) ) ;
#11494 = CARTESIAN_POINT ( 'NONE',  ( 12.38542397377720050, -50.11868687779320197, -21.15108247198449831 ) ) ;
#11495 = CARTESIAN_POINT ( 'NONE',  ( 54.23304704891260286, 19.38381105532069881, -76.90112508198619423 ) ) ;
#11496 = DIRECTION ( 'NONE',  ( 0.000000000000000000, 0.000000000000000000, -1.000000000000000000 ) ) ;
#11497 = CARTESIAN_POINT ( 'NONE',  ( 56.46652749404960048, 14.04259878450300114, -16.69312833544830355 ) ) ;
#11498 = LINE ( 'NONE', #51325, #16483 ) ;
#11499 = CARTESIAN_POINT ( 'NONE',  ( 20.29259834648541627, -21.02751587290103075, -38.74448909963410870 ) ) ;
#11500 = CARTESIAN_POINT ( 'NONE',  ( 20.11167749483229983, -21.44028912359850025, -57.15644495665969771 ) ) ;
#11501 = DIRECTION ( 'NONE',  ( 1.000000000000000000, 2.460964292799963328E-14, 0.000000000000000000 ) ) ;
#11502 = EDGE_LOOP ( 'NONE', ( #6470, #19318, #9077, #8512, #34326, #50762 ) ) ;
#11503 = CARTESIAN_POINT ( 'NONE',  ( 47.46022130281730256, 23.07192592923020413, -75.17786410264480423 ) ) ;
#11504 = CARTESIAN_POINT ( 'NONE',  ( 64.96229391979498757, 1.190292248953970011, -60.67312729078840050 ) ) ;
#11505 = CARTESIAN_POINT ( 'NONE',  ( 45.07858682377059978, -46.11248607424209922, -9.026855431852869316 ) ) ;
#11506 = DIRECTION ( 'NONE',  ( 0.05023550054956202326, 0.000000000000000000, -0.9987374001630934250 ) ) ;
#11507 = CARTESIAN_POINT ( 'NONE',  ( 46.03122142033570441, 13.88381105532070059, -7.582879021622040305 ) ) ;
#11508 = CIRCLE ( 'NONE', #34938, 37.99999999999998579 ) ;
#11509 = CARTESIAN_POINT ( 'NONE',  ( 10.66246720348149957, -64.86660773051299600, -18.01843150775420099 ) ) ;
#11510 = CARTESIAN_POINT ( 'NONE',  ( 10.69832412674970001, 33.66039914567009816, -17.91220997198119846 ) ) ;
#11511 = DIRECTION ( 'NONE',  ( -0.1961161351381840723, -2.837236618486510447E-16, -0.9805806756909202226 ) ) ;
#11513 = CARTESIAN_POINT ( 'NONE',  ( 44.59825589618289854, -37.91486344825149502, -67.32301989359220329 ) ) ;
#11512 = CARTESIAN_POINT ( 'NONE',  ( 22.90093739769620029, -15.61618894467913243, -28.45282021618999835 ) ) ;
#11514 = CARTESIAN_POINT ( 'NONE',  ( 14.56862749054800510, -51.74825541291210129, -75.61049359297885530 ) ) ;
#11515 = CARTESIAN_POINT ( 'NONE',  ( 49.10486152449200148, 22.59225939694159990, -54.68079418519389634 ) ) ;
#11516 = ORIENTED_EDGE ( 'NONE', *, *, #40800, .T. ) ;
#11517 = CARTESIAN_POINT ( 'NONE',  ( 52.84810396677629996, -49.67168591043049730, -48.89993306498779901 ) ) ;
#11518 = ORIENTED_EDGE ( 'NONE', *, *, #11709, .T. ) ;
#11519 = CARTESIAN_POINT ( 'NONE',  ( 46.53888375069291783, 7.993794312659110446, -58.14357038517931642 ) ) ;
#11520 = CARTESIAN_POINT ( 'NONE',  ( 22.04686233763795755, -19.02415527507118398, -74.61948689269669899 ) ) ;
#11521 = CARTESIAN_POINT ( 'NONE',  ( 14.34417029580639991, 19.88381105532299742, -22.49240189291109715 ) ) ;
#11522 = DIRECTION ( 'NONE',  ( 0.000000000000000000, 0.000000000000000000, 1.000000000000000000 ) ) ;
#11523 = EDGE_CURVE ( 'NONE', #5858, #28005, #1562, .T. ) ;
#11524 = CARTESIAN_POINT ( 'NONE',  ( 17.49041801669580209, -8.695024373098599213, -54.01442497355889572 ) ) ;
#11525 = FACE_OUTER_BOUND ( 'NONE', #28910, .T. ) ;
#11526 = CARTESIAN_POINT ( 'NONE',  ( 54.76549198871529711, -46.18106625824350431, -15.95314268619899956 ) ) ;
#11527 = DIRECTION ( 'NONE',  ( 0.000000000000000000, -1.000000000000000000, 0.000000000000000000 ) ) ;
#11528 = EDGE_CURVE ( 'NONE', #45454, #22924, #22896, .T. ) ;
#11529 = ORIENTED_EDGE ( 'NONE', *, *, #49237, .T. ) ;
#11530 = CARTESIAN_POINT ( 'NONE',  ( 9.755795275148487988, -11.04387538940279967, -40.48548165221990303 ) ) ;
#11531 = ORIENTED_EDGE ( 'NONE', *, *, #47912, .F. ) ;
#11532 = EDGE_CURVE ( 'NONE', #37903, #48585, #4124, .T. ) ;
#11533 = CARTESIAN_POINT ( 'NONE',  ( 11.82896782150969983, -65.41720043581369737, -17.62577516534809874 ) ) ;
#11534 = CARTESIAN_POINT ( 'NONE',  ( 12.24650116540029998, 34.20510744208910126, -47.55800081758569320 ) ) ;
#11535 = CARTESIAN_POINT ( 'NONE',  ( 73.00002125581650603, 1.102139304147779830, -62.20100733290610151 ) ) ;
#11536 = CARTESIAN_POINT ( 'NONE',  ( 15.09828380796259495, -23.52717612394415170, -40.33401154759039997 ) ) ;
#11537 = CYLINDRICAL_SURFACE ( 'NONE', #24613, 6.049999999999999822 ) ;
#11538 = CARTESIAN_POINT ( 'NONE',  ( 11.13393739769619906, 32.24968758154479787, -24.15000000000000213 ) ) ;
#11539 = ORIENTED_EDGE ( 'NONE', *, *, #20567, .F. ) ;
#11540 = CARTESIAN_POINT ( 'NONE',  ( 47.40322300430479885, -54.65574458090379295, -74.14999999999999147 ) ) ;
#11541 = CARTESIAN_POINT ( 'NONE',  ( 11.10541238240669948, -63.19988511540091025, -44.25031800029979934 ) ) ;
#11542 = CARTESIAN_POINT ( 'NONE',  ( 65.43042069958039519, 17.98087126524892909, -71.50000000000090949 ) ) ;
#11543 = VERTEX_POINT ( 'NONE', #30504 ) ;
#11544 = CARTESIAN_POINT ( 'NONE',  ( 16.42164688025587793, -23.58948881890144733, -44.28055537063491442 ) ) ;
#11545 = CARTESIAN_POINT ( 'NONE',  ( 56.66762828431429710, 19.14715517649329968, -52.77094437924129977 ) ) ;
#11546 = CARTESIAN_POINT ( 'NONE',  ( 52.26507113521689973, 18.55109022033200006, -77.19475929129460212 ) ) ;
#11547 = EDGE_LOOP ( 'NONE', ( #3572, #41503, #30267, #41962 ) ) ;
#11548 = FILL_AREA_STYLE_COLOUR ( '', #17447 ) ;
#11549 = DIRECTION ( 'NONE',  ( 0.000000000000000000, 0.000000000000000000, -1.000000000000000000 ) ) ;
#11550 = CARTESIAN_POINT ( 'NONE',  ( 83.45566975099262663, -44.67438659557244307, -46.48562894644376797 ) ) ;
#11551 = AXIS2_PLACEMENT_3D ( 'NONE', #15939, #27721, #47656 ) ;
#11552 = CARTESIAN_POINT ( 'NONE',  ( 58.92073396209919878, -3.116188944679349593, -18.64999999999999858 ) ) ;
#11553 = EDGE_CURVE ( 'NONE', #20784, #31931, #746, .T. ) ;
#11554 = CARTESIAN_POINT ( 'NONE',  ( 22.84374255246390106, -10.82440067280909979, -77.59492917107350252 ) ) ;
#11555 = CARTESIAN_POINT ( 'NONE',  ( 52.11631747943250303, -52.62875743058319955, -46.39999999999999858 ) ) ;
#11556 = CARTESIAN_POINT ( 'NONE',  ( -1.266062602303798856, -15.61618894467929941, -10.44999999999999929 ) ) ;
#11557 = CIRCLE ( 'NONE', #29115, 2.999999999999998668 ) ;
#11558 = SHAPE_DEFINITION_REPRESENTATION ( #9819, #19070 ) ;
#11559 = ORIENTED_EDGE ( 'NONE', *, *, #2519, .T. ) ;
#11560 = EDGE_LOOP ( 'NONE', ( #37848, #20269, #7007, #39313 ) ) ;
#11561 = CARTESIAN_POINT ( 'NONE',  ( 15.84771036213319917, -23.06097019662070124, -54.74488924367149423 ) ) ;
#11562 = CARTESIAN_POINT ( 'NONE',  ( 52.88388587306730670, -49.67261804826029703, -49.00306437247580504 ) ) ;
#11563 = DIRECTION ( 'NONE',  ( -1.000000000000000000, 0.000000000000000000, 0.000000000000000000 ) ) ;
#11564 = CARTESIAN_POINT ( 'NONE',  ( 2.404741263826640107, -5.380232784273969671, -35.14999999999999858 ) ) ;
#11565 = CARTESIAN_POINT ( 'NONE',  ( 47.31505028482810360, 23.34690877818389865, -74.80618026387669772 ) ) ;
#11566 = CARTESIAN_POINT ( 'NONE',  ( 61.62036109055981115, 14.01986140997038888, -47.09707863094710945 ) ) ;
#11567 = DIRECTION ( 'NONE',  ( -1.000000000000000000, 0.000000000000000000, 0.000000000000000000 ) ) ;
#11568 = CARTESIAN_POINT ( 'NONE',  ( 12.23389792222850048, 33.66370788264119795, -16.17187715585779983 ) ) ;
#11569 = CARTESIAN_POINT ( 'NONE',  ( 22.92255752238139976, -20.29565018628549922, -69.69977332415550109 ) ) ;
#11570 = CARTESIAN_POINT ( 'NONE',  ( 52.57246135266289855, -49.85409740178759819, -27.98331546413460202 ) ) ;
#11571 = CARTESIAN_POINT ( 'NONE',  ( 55.76783084160810233, -50.62194379187450011, -76.00493532411560693 ) ) ;
#11573 = DIRECTION ( 'NONE',  ( 0.6888026391158250661, 0.7071067811865571207, 0.1598465650148950534 ) ) ;
#11572 = CARTESIAN_POINT ( 'NONE',  ( -10.38035879666180072, 11.60169614569439922, -5.947267209420609824 ) ) ;
#11574 = CARTESIAN_POINT ( 'NONE',  ( 63.48441347673288959, 1.386342629514219826, -68.66646381051069170 ) ) ;
#11575 = CARTESIAN_POINT ( 'NONE',  ( 61.19844447806200094, 14.05756157773689985, -46.92762932161960521 ) ) ;
#11576 = CARTESIAN_POINT ( 'NONE',  ( 22.35126475695520298, 22.42506970168830094, -34.65028073423250277 ) ) ;
#11577 = CYLINDRICAL_SURFACE ( 'NONE', #39849, 5.000000000000000000 ) ;
#11578 = ORIENTED_EDGE ( 'NONE', *, *, #20615, .F. ) ;
#11579 = CARTESIAN_POINT ( 'NONE',  ( 53.26900104180390372, -49.43078783544130062, -48.80948086996689739 ) ) ;
#11580 = CARTESIAN_POINT ( 'NONE',  ( 47.63850175670210518, 23.27425725622169850, -54.75827116794159366 ) ) ;
#11581 = VECTOR ( 'NONE', #10, 999.9999999999998863 ) ;
#11582 = CARTESIAN_POINT ( 'NONE',  ( 60.92349151070310143, -45.26865707020169793, -27.39016921351189993 ) ) ;
#11583 = CARTESIAN_POINT ( 'NONE',  ( 10.85782713917238063, -21.54498903828860179, -66.52372767296536438 ) ) ;
#11584 = CARTESIAN_POINT ( 'NONE',  ( 60.86406060055869460, 14.33749672913939932, -47.52785898179379842 ) ) ;
#11585 = CARTESIAN_POINT ( 'NONE',  ( 22.67920996314880000, -19.17513553729349951, -74.39118414744899610 ) ) ;
#11586 = CARTESIAN_POINT ( 'NONE',  ( 51.78078201309870110, 18.91896746419559960, -76.50453762827730486 ) ) ;
#11587 = CARTESIAN_POINT ( 'NONE',  ( 52.78558019943060486, 18.45415968697669840, -48.61477091151370189 ) ) ;
#11588 = CARTESIAN_POINT ( 'NONE',  ( 16.13393739769620083, -15.61618894467929941, -8.849999999999999645 ) ) ;
#11589 = CARTESIAN_POINT ( 'NONE',  ( 52.90855289046150034, -49.61963672099809486, -48.71990427169439641 ) ) ;
#11590 = EDGE_CURVE ( 'NONE', #31235, #6972, #51823, .T. ) ;
#11591 = CARTESIAN_POINT ( 'NONE',  ( 24.04483843941790866, -15.61617050235280679, -77.50767555791956909 ) ) ;
#11592 = CARTESIAN_POINT ( 'NONE',  ( 9.807706123504049245, -20.47778153303312365, -62.29930259591785813 ) ) ;
#11593 = CARTESIAN_POINT ( 'NONE',  ( 8.222932560853145390, -14.58067687905736953, -36.83399830530230190 ) ) ;
#11594 =( BOUNDED_CURVE ( )  B_SPLINE_CURVE ( 3, ( #40151, #48022, #27063, #3227 ),
 .UNSPECIFIED., .F., .T. ) 
 B_SPLINE_CURVE_WITH_KNOTS ( ( 4, 4 ),
 ( 2.117032425727450207, 2.581755039733875101 ),
 .UNSPECIFIED. ) 
 CURVE ( )  GEOMETRIC_REPRESENTATION_ITEM ( )  RATIONAL_B_SPLINE_CURVE ( ( 1.000000000000000000, 0.9820835707424604433, 0.9820835707424604433, 1.000000000000000000 ) ) 
 REPRESENTATION_ITEM ( '' )  );
#11595 = CARTESIAN_POINT ( 'NONE',  ( 22.04685567601379503, -19.02416774546152922, -70.61948949575641166 ) ) ;
#11596 = CARTESIAN_POINT ( 'NONE',  ( 58.94101292899819811, -28.10821987741100259, -15.65000625949619995 ) ) ;
#11597 = CARTESIAN_POINT ( 'NONE',  ( 71.30558087559749936, 1.190292248953970011, -60.67312729078840050 ) ) ;
#11598 = DIRECTION ( 'NONE',  ( 0.000000000000000000, 0.000000000000000000, 1.000000000000000000 ) ) ;
#11599 = CARTESIAN_POINT ( 'NONE',  ( 72.43598295795109721, 1.061277144319840104, -61.46676083746540087 ) ) ;
#11600 = CARTESIAN_POINT ( 'NONE',  ( 50.99271603304481459, -35.23405637081515351, -76.39685558562041479 ) ) ;
#11601 = FACE_OUTER_BOUND ( 'NONE', #1879, .T. ) ;
#11602 = EDGE_LOOP ( 'NONE', ( #43036, #16626, #35761, #19005 ) ) ;
#11603 = ORIENTED_EDGE ( 'NONE', *, *, #41265, .T. ) ;
#11604 = CARTESIAN_POINT ( 'NONE',  ( 40.92757333388379948, 13.18145061293710008, -3.805844904963549880 ) ) ;
#11605 = FACE_OUTER_BOUND ( 'NONE', #7734, .T. ) ;
#11606 = ORIENTED_EDGE ( 'NONE', *, *, #26721, .F. ) ;
#11607 = LINE ( 'NONE', #8444, #23508 ) ;
#11608 = CARTESIAN_POINT ( 'NONE',  ( 17.70136110659009532, -23.38214466260832225, -77.94427081745516261 ) ) ;
#11609 = VERTEX_POINT ( 'NONE', #13764 ) ;
#11610 = CARTESIAN_POINT ( 'NONE',  ( 11.93124446071863787, -20.97860508548876624, -81.16457539097082474 ) ) ;
#11611 = CARTESIAN_POINT ( 'NONE',  ( 43.70384182385213023, 6.645243339508008162, -71.80047792273670382 ) ) ;
#11612 = CARTESIAN_POINT ( 'NONE',  ( 10.87442115971020051, 33.42441897061950584, -23.33560984931230209 ) ) ;
#11613 = EDGE_CURVE ( 'NONE', #24756, #36035, #6225, .T. ) ;
#11614 = CARTESIAN_POINT ( 'NONE',  ( 12.44141513252709963, -22.98831137825300175, -32.44013846481049512 ) ) ;
#11615 = CARTESIAN_POINT ( 'NONE',  ( 45.30944071664330153, 2.566574815035449930, -34.65725502031740035 ) ) ;
#11616 = CARTESIAN_POINT ( 'NONE',  ( 24.04123512108865768, -15.87802979434204254, -49.80286409962939587 ) ) ;
#11617 = ADVANCED_FACE ( 'NONE', ( #10090 ), #26747, .F. ) ;
#11618 =( NAMED_UNIT ( * ) PLANE_ANGLE_UNIT ( ) SI_UNIT ( $, .RADIAN. ) );
#11619 = CARTESIAN_POINT ( 'NONE',  ( 60.85624101447609746, -29.02149448471999804, -15.89604434587320014 ) ) ;
#11620 = CARTESIAN_POINT ( 'NONE',  ( 14.41157406479737801, 20.07361857726730037, -75.01676221295032576 ) ) ;
#11621 = CARTESIAN_POINT ( 'NONE',  ( 47.21888195866840476, -54.18123867552319695, -75.46887108633241326 ) ) ;
#11622 = CARTESIAN_POINT ( 'NONE',  ( 14.32234953326219973, -23.25195328107799853, -72.58664262352560570 ) ) ;
#11623 = DIRECTION ( 'NONE',  ( 0.000000000000000000, -0.7071067811865582309, 0.7071067811865366926 ) ) ;
#11624 = AXIS2_PLACEMENT_3D ( 'NONE', #21066, #4314, #44413 ) ;
#11625 = CARTESIAN_POINT ( 'NONE',  ( 40.95780214525460394, 14.16802372685690159, -5.890450655994820650 ) ) ;
#11626 = AXIS2_PLACEMENT_3D ( 'NONE', #8687, #36980, #20206 ) ;
#11627 = LINE ( 'NONE', #11890, #4985 ) ;
#11628 = CARTESIAN_POINT ( 'NONE',  ( 82.66152712818241355, -45.35408509398140353, -47.35223793503389800 ) ) ;
#11629 = DIRECTION ( 'NONE',  ( 0.000000000000000000, 0.000000000000000000, -1.000000000000000000 ) ) ;
#11630 = CARTESIAN_POINT ( 'NONE',  ( 9.758119116160459683, -10.38821974528549852, -46.72628331570599869 ) ) ;
#11631 = ORIENTED_EDGE ( 'NONE', *, *, #6864, .F. ) ;
#11632 = CARTESIAN_POINT ( 'NONE',  ( 4.082512187184039298, -8.658295355271496518, -34.89146800830128115 ) ) ;
#11633 = CARTESIAN_POINT ( 'NONE',  ( 16.19673815768810243, -51.06918470345650007, -20.37207796061799669 ) ) ;
#11634 = CARTESIAN_POINT ( 'NONE',  ( 76.33997785262350533, -18.72318222815389888, -12.53642027154039873 ) ) ;
#11635 = DIRECTION ( 'NONE',  ( 1.000000000000000000, 0.000000000000000000, 0.000000000000000000 ) ) ;
#11636 = FACE_OUTER_BOUND ( 'NONE', #17368, .T. ) ;
#11637 = VERTEX_POINT ( 'NONE', #37874 ) ;
#11638 = CARTESIAN_POINT ( 'NONE',  ( -10.87046103729910129, -42.35940093361649161, -6.284374684026399649 ) ) ;
#11639 = CARTESIAN_POINT ( 'NONE',  ( 71.71126032029680175, 15.88381105532069704, -46.37203261889099792 ) ) ;
#11640 = CARTESIAN_POINT ( 'NONE',  ( 9.366859039486531202, -15.61635947376150035, -49.45282021618999835 ) ) ;
#11641 = CARTESIAN_POINT ( 'NONE',  ( 63.08005232011719698, 0.8859637708054489691, -62.41593972647859800 ) ) ;
#11642 = CARTESIAN_POINT ( 'NONE',  ( 57.55751162061849868, -50.19856700622089818, -52.70112124861869773 ) ) ;
#11643 = CARTESIAN_POINT ( 'NONE',  ( 41.70176497865799803, 13.04736526282390230, -4.832746521660269856 ) ) ;
#11644 = DIRECTION ( 'NONE',  ( 0.000000000000000000, 0.7071067811865457964, 0.7071067811865492381 ) ) ;
#11645 = CARTESIAN_POINT ( 'NONE',  ( 0.3198710486850440127, 15.01731126982059905, -34.64999999999999858 ) ) ;
#11646 = CARTESIAN_POINT ( 'NONE',  ( 63.63393739769619373, -53.11618894467930119, 11.84999999999999964 ) ) ;
#11647 = CARTESIAN_POINT ( 'NONE',  ( -0.2088566477600920512, -20.53519877086888812, -34.94807878368268206 ) ) ;
#11648 = EDGE_CURVE ( 'NONE', #42921, #17993, #40155, .T. ) ;
#11649 = CARTESIAN_POINT ( 'NONE',  ( 17.79719214914599945, -51.84692819978400280, -75.69083100613939052 ) ) ;
#11650 = DIRECTION ( 'NONE',  ( 0.000000000000000000, 0.000000000000000000, -1.000000000000000000 ) ) ;
#11651 = CARTESIAN_POINT ( 'NONE',  ( 19.92837444633610033, -22.02781446573479940, -63.39724662014580048 ) ) ;
#11652 = CARTESIAN_POINT ( 'NONE',  ( 15.09843720942611256, -7.705183231044903103, -77.25066340357626871 ) ) ;
#11653 = CARTESIAN_POINT ( 'NONE',  ( 53.40543070545079729, -53.45144757578069772, -56.07519854833829953 ) ) ;
#11654 = EDGE_LOOP ( 'NONE', ( #6195, #34187, #38976, #6959, #19717 ) ) ;
#11655 = CARTESIAN_POINT ( 'NONE',  ( 8.788582027835408539, 31.90262041517649649, -46.67125809046000029 ) ) ;
#11656 = DIRECTION ( 'NONE',  ( 0.000000000000000000, 0.000000000000000000, 1.000000000000000000 ) ) ;
#11657 = CARTESIAN_POINT ( 'NONE',  ( 72.89924231985609993, 1.371651820402770117, -68.64970267437179530 ) ) ;
#11658 = AXIS2_PLACEMENT_3D ( 'NONE', #20287, #8778, #40231 ) ;
#11659 = FACE_OUTER_BOUND ( 'NONE', #44112, .T. ) ;
#11660 = TOROIDAL_SURFACE ( 'NONE', #31699, 23.49999999909039872, 0.4999999999562930175 ) ;
#11661 = AXIS2_PLACEMENT_3D ( 'NONE', #29804, #49504, #41362 ) ;
#11662 = CARTESIAN_POINT ( 'NONE',  ( 9.052227180162510933, -14.02043803924360077, -81.23899999999999011 ) ) ;
#11663 = ORIENTED_EDGE ( 'NONE', *, *, #50105, .F. ) ;
#11664 = CARTESIAN_POINT ( 'NONE',  ( 17.36506832604939987, 21.76199957607230218, -76.14999999999999147 ) ) ;
#11665 = ORIENTED_EDGE ( 'NONE', *, *, #33909, .F. ) ;
#11666 = CONICAL_SURFACE ( 'NONE', #2452, 20.98392344168889778, 0.7480182347898678419 ) ;
#11667 = VERTEX_POINT ( 'NONE', #30246 ) ;
#11668 = CARTESIAN_POINT ( 'NONE',  ( 55.75441314946239402, -45.11618894467940066, -14.47055463458629987 ) ) ;
#11669 = CARTESIAN_POINT ( 'NONE',  ( 23.53254287302059922, -14.04113270188789997, -81.23899999999999011 ) ) ;
#11670 = CARTESIAN_POINT ( 'NONE',  ( 12.14991513904929121, -8.703604018978865042, -73.12566484550632140 ) ) ;
#11671 = ORIENTED_EDGE ( 'NONE', *, *, #41690, .T. ) ;
#11672 = CARTESIAN_POINT ( 'NONE',  ( 8.223605785152290792, -15.61620117245469963, -52.50766849176299900 ) ) ;
#11673 = ORIENTED_EDGE ( 'NONE', *, *, #39102, .F. ) ;
#11674 = DIRECTION ( 'NONE',  ( 0.000000000000000000, 0.000000000000000000, -1.000000000000000000 ) ) ;
#11675 = EDGE_CURVE ( 'NONE', #20725, #10696, #41832, .T. ) ;
#11676 = DIRECTION ( 'NONE',  ( 0.000000000000000000, 0.000000000000000000, 1.000000000000000000 ) ) ;
#11677 = VERTEX_POINT ( 'NONE', #39939 ) ;
#11678 = DIRECTION ( 'NONE',  ( 0.000000000000000000, 0.000000000000000000, -1.000000000000000000 ) ) ;
#11679 = CARTESIAN_POINT ( 'NONE',  ( 53.68570370335149988, -51.14635124491550755, -75.73808979161600519 ) ) ;
#11680 = CARTESIAN_POINT ( 'NONE',  ( 60.73825411176089517, 14.46861665316230017, -47.68938770369700109 ) ) ;
#11681 = CARTESIAN_POINT ( 'NONE',  ( 15.21636614235080032, 19.37178131641699963, -15.64999999240779971 ) ) ;
#11682 = CARTESIAN_POINT ( 'NONE',  ( 68.13393739769620083, -42.11618894467930119, -65.65000000000000568 ) ) ;
#11683 = CARTESIAN_POINT ( 'NONE',  ( -5.389730541883220205, 15.98232200020200189, -5.411213624794680044 ) ) ;
#11684 = AXIS2_PLACEMENT_3D ( 'NONE', #26052, #26316, #18978 ) ;
#11685 = VECTOR ( 'NONE', #8380, 1000.000000000000000 ) ;
#11686 = AXIS2_PLACEMENT_3D ( 'NONE', #51394, #19415, #3700 ) ;
#11687 = FACE_OUTER_BOUND ( 'NONE', #39532, .T. ) ;
#11688 = CARTESIAN_POINT ( 'NONE',  ( 76.87859641664680055, 11.88381105532059934, -14.85884654260030047 ) ) ;
#11689 = VECTOR ( 'NONE', #39230, 1000.000000000000000 ) ;
#11690 = CIRCLE ( 'NONE', #45999, 1.999999999999996669 ) ;
#11691 = CARTESIAN_POINT ( 'NONE',  ( 14.01353913340800084, -23.17202505883549790, -61.87459303939719746 ) ) ;
#11692 = ORIENTED_EDGE ( 'NONE', *, *, #47921, .F. ) ;
#11693 = CYLINDRICAL_SURFACE ( 'NONE', #19634, 0.9999999999999988898 ) ;
#11695 = AXIS2_PLACEMENT_3D ( 'NONE', #22130, #18474, #34707 ) ;
#11694 = CARTESIAN_POINT ( 'NONE',  ( 42.67728079040009703, 14.69073914472930120, -7.341720920331609612 ) ) ;
#11696 = CARTESIAN_POINT ( 'NONE',  ( 71.83183169758690667, 0.9828917932938358026, -70.37585607920048858 ) ) ;
#11697 = CARTESIAN_POINT ( 'NONE',  ( 42.31941830961962836, -39.79865067521480881, -74.78800917364183931 ) ) ;
#11698 = CARTESIAN_POINT ( 'NONE',  ( 13.79543417967160046, 19.20548902729790086, -21.08562091375049974 ) ) ;
#11699 = DIRECTION ( 'NONE',  ( -0.4316160343590931259, -0.9020574254913764634, 0.000000000000000000 ) ) ;
#11700 = CARTESIAN_POINT ( 'NONE',  ( 11.42275550116415417, -22.01442326570142782, -32.20961141529382132 ) ) ;
#11701 = CARTESIAN_POINT ( 'NONE',  ( 61.19897450384227966, 14.07984771058140616, -47.06085141197393540 ) ) ;
#11702 = CARTESIAN_POINT ( 'NONE',  ( 48.76197234853290041, -53.91797685349600044, -54.58489184698370167 ) ) ;
#11703 = CARTESIAN_POINT ( 'NONE',  ( 33.13393739769620083, -38.61618894467930119, -59.64999999999999147 ) ) ;
#11704 = EDGE_CURVE ( 'NONE', #50005, #41343, #4035, .T. ) ;
#11705 = CARTESIAN_POINT ( 'NONE',  ( 64.02817266311009803, 1.026090475080779996, -70.02573918086800120 ) ) ;
#11706 = CARTESIAN_POINT ( 'NONE',  ( 47.77433725855070179, 23.22049558335110220, -54.88289543892820177 ) ) ;
#11707 = ORIENTED_EDGE ( 'NONE', *, *, #4519, .F. ) ;
#11708 = CARTESIAN_POINT ( 'NONE',  ( 15.08788150892120150, -8.239708658262170360, -38.52250226616929751 ) ) ;
#11709 = EDGE_CURVE ( 'NONE', #23561, #22246, #21720, .T. ) ;
#11710 = DIRECTION ( 'NONE',  ( 0.000000000000000000, 0.000000000000000000, -1.000000000000000000 ) ) ;
#11711 = EDGE_LOOP ( 'NONE', ( #42204, #3650, #33418, #49256, #34141, #35359 ) ) ;
#11712 = CARTESIAN_POINT ( 'NONE',  ( 71.50060750274239751, 1.264689361399219836, -70.43884909106640180 ) ) ;
#11713 = CARTESIAN_POINT ( 'NONE',  ( 60.78914095713869159, -45.49441526409999881, -47.15145036089220554 ) ) ;
#11714 = CARTESIAN_POINT ( 'NONE',  ( 60.08410996676487770, 14.17546795341159971, -26.92089435490699501 ) ) ;
#11715 = CARTESIAN_POINT ( 'NONE',  ( 1.027904703268279984, -42.68661147989060112, -15.65000000000000036 ) ) ;
#11717 = DIRECTION ( 'NONE',  ( 0.000000000000000000, 0.000000000000000000, -1.000000000000000000 ) ) ;
#11716 = CARTESIAN_POINT ( 'NONE',  ( 41.73102901179257174, 8.502924699651416063, -77.62876425794036095 ) ) ;
#11718 = EDGE_CURVE ( 'NONE', #17773, #27518, #27100, .T. ) ;
#11719 = CARTESIAN_POINT ( 'NONE',  ( 16.13393739769620083, -15.61618894467929941, -35.14999999999999858 ) ) ;
#11720 = CARTESIAN_POINT ( 'NONE',  ( 12.14990643715953311, -8.703608940057563359, -66.84100088982287957 ) ) ;
#11721 = ORIENTED_EDGE ( 'NONE', *, *, #45388, .F. ) ;
#11722 = CARTESIAN_POINT ( 'NONE',  ( 0.07409199189653030426, 19.67928630151580194, -34.73152237081639981 ) ) ;
#11723 = ORIENTED_EDGE ( 'NONE', *, *, #9284, .F. ) ;
#11724 = VECTOR ( 'NONE', #17490, 1000.000000000000114 ) ;
#11725 = ORIENTED_EDGE ( 'NONE', *, *, #17544, .F. ) ;
#11726 = CARTESIAN_POINT ( 'NONE',  ( 15.52768592298719952, -22.64292490982440142, -59.37457502644110008 ) ) ;
#11727 = AXIS2_PLACEMENT_3D ( 'NONE', #12967, #21570, #33369 ) ;
#11728 = DIRECTION ( 'NONE',  ( 0.05355673487304403457, 0.9985648081870993620, 0.000000000000000000 ) ) ;
#11729 = AXIS2_PLACEMENT_3D ( 'NONE', #135, #32580, #16900 ) ;
#11730 = LINE ( 'NONE', #23743, #47830 ) ;
#11731 = CARTESIAN_POINT ( 'NONE',  ( 12.43884059054600044, -65.45834671174260677, -47.53658363125300212 ) ) ;
#11732 = AXIS2_PLACEMENT_3D ( 'NONE', #10567, #46740, #42540 ) ;
#11733 = EDGE_CURVE ( 'NONE', #48724, #13982, #46872, .T. ) ;
#11734 = ORIENTED_EDGE ( 'NONE', *, *, #17499, .F. ) ;
#11735 = AXIS2_PLACEMENT_3D ( 'NONE', #27695, #8047, #23746 ) ;
#11736 = CARTESIAN_POINT ( 'NONE',  ( 24.04492190160353005, -15.63236120819791175, -55.50832257871742570 ) ) ;
#11737 = CARTESIAN_POINT ( 'NONE',  ( 56.61928470354429521, -45.32411298099489727, -25.29356197036729981 ) ) ;
#11738 = CARTESIAN_POINT ( 'NONE',  ( 56.44265207942110152, -50.69875850325810518, -53.28298857138560152 ) ) ;
#11739 = CARTESIAN_POINT ( 'NONE',  ( 22.90085165683744250, -15.57936011607131555, -46.45109595593834939 ) ) ;
#11740 = CARTESIAN_POINT ( 'NONE',  ( 62.12101911243640018, -1.046128620244999974, -16.19753051798430121 ) ) ;
#11741 = EDGE_CURVE ( 'NONE', #42080, #10547, #15047, .T. ) ;
#11742 = CARTESIAN_POINT ( 'NONE',  ( 51.81471763238939587, -49.53261600392220743, -76.85964251417181003 ) ) ;
#11743 = DIRECTION ( 'NONE',  ( 0.000000000000000000, 0.000000000000000000, -1.000000000000000000 ) ) ;
#11744 =( BOUNDED_CURVE ( )  B_SPLINE_CURVE ( 2, ( #51755, #12185, #11937 ),
 .UNSPECIFIED., .F., .T. ) 
 B_SPLINE_CURVE_WITH_KNOTS ( ( 3, 3 ),
 ( 0.09013418061657679781, 2.097305204681399804 ),
 .UNSPECIFIED. ) 
 CURVE ( )  GEOMETRIC_REPRESENTATION_ITEM ( )  RATIONAL_B_SPLINE_CURVE ( ( 1.000760730681520050, 1.008874108821600002, 1.001093714212740071 ) ) 
 REPRESENTATION_ITEM ( '' )  );
#11745 = VERTEX_POINT ( 'NONE', #20253 ) ;
#11746 = B_SPLINE_CURVE_WITH_KNOTS ( 'NONE', 3,
 ( #48399, #33431, #49451, #12497, #44987, #28467, #24516, #28722, #24780, #4890, #19746, #19989, #48307, #48055, #12402, #28366, #40184, #24162, #44117, #24422, #23397, #4276, #7713, #39420, #44372 ),
 .UNSPECIFIED., .F., .F.,
 ( 4, 2, 2, 1, 1, 2, 2, 2, 2, 1, 1, 1, 2, 2, 4 ),
 ( 0.000000000000000000, 0.1250000000000000555, 0.1875000000000000833, 0.2187499999999996669, 0.2343749999999998890, 0.2421875000000003886, 0.2500000000000008882, 0.4999999999999942824, 0.6249999999999908962, 0.6874999999999883427, 0.7187499999999870104, 0.7343749999999861222, 0.7421874999999865663, 0.7499999999999870104, 1.000000000000000000 ),
 .UNSPECIFIED. ) ;
#11747 = FACE_OUTER_BOUND ( 'NONE', #37510, .T. ) ;
#11748 = CARTESIAN_POINT ( 'NONE',  ( 64.81199447428100768, 0.8910129994591419189, -70.64647704525310701 ) ) ;
#11749 = CARTESIAN_POINT ( 'NONE',  ( 9.221472665190642459, -19.60042021849464788, -54.34100233441036210 ) ) ;
#11750 = CARTESIAN_POINT ( 'NONE',  ( 10.25681452098029922, -20.81678259190509905, -52.78190985762079634 ) ) ;
#11751 = CARTESIAN_POINT ( 'NONE',  ( 13.73527021832320116, -50.20735446946800096, -20.93080062246840001 ) ) ;
#11752 = CARTESIAN_POINT ( 'NONE',  ( 56.11474826664630200, 19.38381105532069881, -75.99278311555809751 ) ) ;
#11753 = DIRECTION ( 'NONE',  ( 0.1961161351381840723, -2.713878504639270283E-16, 0.9805806756909202226 ) ) ;
#11754 = CARTESIAN_POINT ( 'NONE',  ( 11.19961949155312908, -65.24734059375452944, -18.17421237899869979 ) ) ;
#11755 = CARTESIAN_POINT ( 'NONE',  ( 8.830271178172500512, 17.88421590754769852, -34.68023162149810190 ) ) ;
#11756 = CARTESIAN_POINT ( 'NONE',  ( 22.04685790523001998, -19.02416357525799384, -38.61948949083011229 ) ) ;
#11757 = ADVANCED_FACE ( 'NONE', ( #39168 ), #8783, .T. ) ;
#11758 = CARTESIAN_POINT ( 'NONE',  ( 9.289762948636740347, -17.31907921868189959, -51.76955764433359519 ) ) ;
#11759 = CARTESIAN_POINT ( 'NONE',  ( 9.366859039486531202, -15.61635947376150035, -49.45282021618999835 ) ) ;
#11760 = ORIENTED_EDGE ( 'NONE', *, *, #2527, .T. ) ;
#11761 = CARTESIAN_POINT ( 'NONE',  ( 63.54731047306190561, 1.396834109478129804, -62.44999999999999574 ) ) ;
#11762 = DIRECTION ( 'NONE',  ( 1.000000000000000000, 0.000000000000000000, 0.000000000000000000 ) ) ;
#11763 = CIRCLE ( 'NONE', #52, 13.50000000000000000 ) ;
#11764 = CARTESIAN_POINT ( 'NONE',  ( 11.42523121511829132, 34.02364939928509102, -47.34553053285857516 ) ) ;
#11765 = CARTESIAN_POINT ( 'NONE',  ( 14.42528838908026323, -51.34461569805392145, -75.09855816266191653 ) ) ;
#11766 = VECTOR ( 'NONE', #43471, 1000.000000000000114 ) ;
#11767 = CARTESIAN_POINT ( 'NONE',  ( 13.08847648858512969, -8.234862729930275904, -54.88289519625694624 ) ) ;
#11768 = AXIS2_PLACEMENT_3D ( 'NONE', #34461, #38410, #26335 ) ;
#11770 = CIRCLE ( 'NONE', #32638, 7.000000000000000000 ) ;
#11769 = CARTESIAN_POINT ( 'NONE',  ( 22.72480788795719775, -13.84492799828816345, -76.36947556904178214 ) ) ;
#11771 = CARTESIAN_POINT ( 'NONE',  ( 10.98984918195399985, 33.92088487140379982, -18.13296861412510097 ) ) ;
#11772 = LINE ( 'NONE', #27470, #11766 ) ;
#11774 = CARTESIAN_POINT ( 'NONE',  ( 45.97697684862929890, -38.03835002546479416, -60.42395416268509933 ) ) ;
#11773 = DIRECTION ( 'NONE',  ( 0.000000000000000000, 0.000000000000000000, 1.000000000000000000 ) ) ;
#11775 = CARTESIAN_POINT ( 'NONE',  ( 9.342084535698248260, -63.49213292503509365, -16.98578758134890165 ) ) ;
#11776 = CARTESIAN_POINT ( 'NONE',  ( 49.22713800240349968, 22.39287771768360358, -54.29674177404830004 ) ) ;
#11777 = VERTEX_POINT ( 'NONE', #2169 ) ;
#11778 = CARTESIAN_POINT ( 'NONE',  ( 53.44638498043019581, -49.38818856033790183, -49.05897242516689971 ) ) ;
#11779 = ORIENTED_EDGE ( 'NONE', *, *, #30909, .T. ) ;
#11780 = CARTESIAN_POINT ( 'NONE',  ( 41.46338495793718693, 7.445976544050517454, -83.29850773724480462 ) ) ;
#11781 = CARTESIAN_POINT ( 'NONE',  ( 17.01980794770872407, -22.38317861683710319, -74.91115355591935554 ) ) ;
#11782 = CARTESIAN_POINT ( 'NONE',  ( 16.13393739769629676, -15.61618894467929941, -20.75000000000000000 ) ) ;
#11783 = DIRECTION ( 'NONE',  ( -1.000000000000000000, 0.000000000000000000, 0.000000000000000000 ) ) ;
#11784 = CARTESIAN_POINT ( 'NONE',  ( 10.23956942737700082, -11.74333664603669902, -51.63785704165039192 ) ) ;
#11786 = EDGE_CURVE ( 'NONE', #25615, #51745, #36053, .T. ) ;
#11785 = CARTESIAN_POINT ( 'NONE',  ( 52.63649320657160047, 18.56913157916169865, -48.66852570238020093 ) ) ;
#11787 = CARTESIAN_POINT ( 'NONE',  ( 55.99869819504039725, -45.41806919520020358, -16.36330855170579923 ) ) ;
#11788 = CARTESIAN_POINT ( 'NONE',  ( -21.36606260230379917, -53.11618894467930119, 17.35000000000000142 ) ) ;
#11789 = ORIENTED_EDGE ( 'NONE', *, *, #12983, .F. ) ;
#11790 = CARTESIAN_POINT ( 'NONE',  ( 23.14187571796059828, -19.14826321945789900, -41.43610882498329318 ) ) ;
#11791 = ORIENTED_EDGE ( 'NONE', *, *, #352, .T. ) ;
#11792 = CARTESIAN_POINT ( 'NONE',  ( 11.10349387995800008, -65.15484720641850913, -17.61839559469159866 ) ) ;
#11793 = CARTESIAN_POINT ( 'NONE',  ( 10.71073732096479958, 32.53643514237809597, -45.47433255531149854 ) ) ;
#11794 = CARTESIAN_POINT ( 'NONE',  ( 72.99182123261159916, 1.264489825601020190, -62.40944773533740175 ) ) ;
#11795 = CARTESIAN_POINT ( 'NONE',  ( 52.76718212758399318, -50.10714647214729922, -49.94264780762849654 ) ) ;
#11796 = CARTESIAN_POINT ( 'NONE',  ( 11.63041745226685286, -65.37747845517948520, -22.51826834756352014 ) ) ;
#11797 = CARTESIAN_POINT ( 'NONE',  ( 40.36721523010999846, -44.88645108046029719, -4.296538310233220415 ) ) ;
#11798 = ORIENTED_EDGE ( 'NONE', *, *, #41580, .F. ) ;
#11799 = CARTESIAN_POINT ( 'NONE',  ( 65.01129443250870565, 1.391252479931859964, -70.26382307879910627 ) ) ;
#11800 = CARTESIAN_POINT ( 'NONE',  ( 10.97887834524160056, -63.27147703799300160, -44.74240717694910074 ) ) ;
#11801 = CARTESIAN_POINT ( 'NONE',  ( 68.13393739769810509, 19.38381105532030091, -71.50000000000198952 ) ) ;
#11802 = ORIENTED_EDGE ( 'NONE', *, *, #24326, .T. ) ;
#11803 = CARTESIAN_POINT ( 'NONE',  ( 66.72561048563109409, -33.11618894467930829, -20.64999999980150136 ) ) ;
#11804 = CARTESIAN_POINT ( 'NONE',  ( 11.42703244249149819, -9.192886441045931889, -76.80656519119119707 ) ) ;
#11805 = AXIS2_PLACEMENT_3D ( 'NONE', #36214, #28026, #43520 ) ;
#11806 = DIRECTION ( 'NONE',  ( 0.000000000000000000, 0.000000000000000000, 1.000000000000000000 ) ) ;
#11807 = VERTEX_POINT ( 'NONE', #34379 ) ;
#11808 = CARTESIAN_POINT ( 'NONE',  ( 20.11806571293955059, -22.52871392151443786, -35.84099981003727464 ) ) ;
#11809 = CARTESIAN_POINT ( 'NONE',  ( 16.13393739769620083, -15.61618894467929941, -32.14999999999999858 ) ) ;
#11810 = AXIS2_PLACEMENT_3D ( 'NONE', #47862, #3838, #19812 ) ;
#11811 = FACE_OUTER_BOUND ( 'NONE', #18107, .T. ) ;
#11812 = CARTESIAN_POINT ( 'NONE',  ( 70.99050876911339003, 0.8838110553206759423, -70.34999999999999432 ) ) ;
#11813 = AXIS2_PLACEMENT_3D ( 'NONE', #16756, #255, #12573 ) ;
#11814 = CARTESIAN_POINT ( 'NONE',  ( 15.76421757133440060, -7.379318950180220327, -77.27805344681898703 ) ) ;
#11815 = DIRECTION ( 'NONE',  ( -0.4640893551880615475, -0.8857883891771946017, 0.000000000000000000 ) ) ;
#11816 = CARTESIAN_POINT ( 'NONE',  ( 46.08014022084859818, -38.16162640463598166, -59.91892963968066255 ) ) ;
#11817 = SHAPE_DEFINITION_REPRESENTATION ( #6925, #29764 ) ;
#11818 = VERTEX_POINT ( 'NONE', #50391 ) ;
#11819 = CARTESIAN_POINT ( 'NONE',  ( 23.56869833393620084, -15.13553977313539889, -68.21210752448669723 ) ) ;
#11820 = CARTESIAN_POINT ( 'NONE',  ( 52.97659487819839796, -49.63248385376320471, -49.06742264967090250 ) ) ;
#11821 = ADVANCED_FACE ( 'NONE', ( #34636 ), #38599, .T. ) ;
#11822 = CARTESIAN_POINT ( 'NONE',  ( 12.86517331568640010, -49.11618894467930829, -34.64999999999999858 ) ) ;
#11823 = CYLINDRICAL_SURFACE ( 'NONE', #1938, 0.9999999999999988898 ) ;
#11824 = EDGE_CURVE ( 'NONE', #23479, #16151, #18149, .T. ) ;
#11825 = CARTESIAN_POINT ( 'NONE',  ( 47.28692500774510421, 23.29813155386499801, -74.94563673128509151 ) ) ;
#11826 = DIRECTION ( 'NONE',  ( 1.000000000000000000, 0.000000000000000000, 0.000000000000000000 ) ) ;
#11827 = EDGE_CURVE ( 'NONE', #21370, #13586, #51042, .T. ) ;
#11828 = B_SPLINE_SURFACE_WITH_KNOTS ( 'NONE', 3, 3, ( 
 ( #19372, #51354, #3405, #22773, #35354, #35091, #15452, #47176, #46664, #6552, #11265, #31405, #47433, #11526, #34836, #22258 ),
 ( #23279, #30640, #2627, #27485, #38265, #46406, #38792, #50580, #46920, #10747, #2358, #22519, #26704, #23028, #42725, #2884 ),
 ( #18334, #6819, #34313, #27226, #50836, #50326, #30380, #10493, #14928, #14412, #26449, #42465, #38528, #18599, #15190, #3145 ),
 ( #30893, #11006, #26974, #42983, #7078, #51092, #39050, #31151, #43240, #39300, #3659, #19880, #40324, #32686, #20647, #4674 ),
 ( #24046, #20386, #31659, #35871, #4160, #36633, #16213, #11787, #31918, #735, #8357, #7845, #32170, #44512, #51864, #8616 ),
 ( #24564, #48186, #43744, #40578, #27746, #28515, #16732, #15964, #47939, #481, #12040, #48713, #16469, #12817, #48447, #19631 ),
 ( #27994, #43997, #23793, #8103, #40067, #43491, #20135, #24307, #39809, #23538, #3917, #12549, #36126, #12290, #7592, #39556 ),
 ( #231, #35621, #36374, #51609, #32424, #28251, #44249, #15703, #47683, #4419, #37424, #45813, #33220, #45551, #49238, #21422 ),
 ( #13332, #48980, #44773, #5976, #21932, #36906, #18018, #8878, #13085, #37681, #25602, #37944, #1006, #2038, #49999, #41351 ),
 ( #5715, #20909, #1780, #1524, #28772, #40838, #5212, #41609, #33984, #24830, #41873, #17510, #9402, #21671, #17006, #21165 ) ),
 .UNSPECIFIED., .F., .F., .F.,
 ( 4, 1, 1, 1, 1, 1, 1, 4 ),
 ( 4, 2, 2, 2, 2, 2, 2, 4 ),
 ( -1.163108567600000046E-05, 0.1428571428571430157, 0.2857142857142860315, 0.4285714285714289917, 0.5714285714285709528, 0.7142857142857139685, 0.8571428571428569843, 1.000000000000000000 ),
 ( -4.238739900490239521, -3.496950822258759750, -2.649205168377850139, -2.119364134702280023, -1.854443617864500071, -1.430570790924039937, -0.7523742678193099387, 1.163108567600000046E-05 ),
 .UNSPECIFIED. ) ;
#11829 = DIRECTION ( 'NONE',  ( 1.000000000000000000, 0.000000000000000000, 0.000000000000000000 ) ) ;
#11830 = CARTESIAN_POINT ( 'NONE',  ( 11.70888777237000156, 33.68434717559169655, -16.37375727425619942 ) ) ;
#11831 = CARTESIAN_POINT ( 'NONE',  ( 21.32529432998289920, -9.210524739417378370, -69.22445973777388417 ) ) ;
#11832 = CARTESIAN_POINT ( 'NONE',  ( 22.31435075509589794, -12.28517517030200068, -32.14999999999999858 ) ) ;
#11833 = CARTESIAN_POINT ( 'NONE',  ( 54.37045953228780348, -50.66722079764569742, -76.42819221719689438 ) ) ;
#11835 = DIRECTION ( 'NONE',  ( 0.000000000000000000, 0.000000000000000000, -1.000000000000000000 ) ) ;
#11834 = CARTESIAN_POINT ( 'NONE',  ( -3.470041707072629933, 18.86435022852390020, -8.135964718609921320 ) ) ;
#11836 = CARTESIAN_POINT ( 'NONE',  ( 63.44650199127489998, 1.383928098097870096, -68.54761322559109260 ) ) ;
#11837 = CARTESIAN_POINT ( 'NONE',  ( 61.30905961866820064, 13.99617788076260005, -46.74474789437339695 ) ) ;
#11838 = CARTESIAN_POINT ( 'NONE',  ( 8.222951331889666093, -14.58053946526866262, -78.54933523722530708 ) ) ;
#11839 = FACE_OUTER_BOUND ( 'NONE', #36451, .T. ) ;
#11840 = ORIENTED_EDGE ( 'NONE', *, *, #41839, .T. ) ;
#11841 = VECTOR ( 'NONE', #42390, 1000.000000000000000 ) ;
#11842 = CARTESIAN_POINT ( 'NONE',  ( 53.42190059083360154, -49.35067947775139885, -48.77466594535759725 ) ) ;
#11843 = CIRCLE ( 'NONE', #35247, 28.31678667024650409 ) ;
#11844 = CARTESIAN_POINT ( 'NONE',  ( 61.28606390168010165, -45.23047506471469603, -28.05549306702249979 ) ) ;
#11845 = CARTESIAN_POINT ( 'NONE',  ( 14.02640371334330816, -23.26397146298620200, -66.37784655330483474 ) ) ;
#11846 = CARTESIAN_POINT ( 'NONE',  ( 61.19909455212179950, 14.07977596102159978, -47.06069650264579707 ) ) ;
#11847 = VECTOR ( 'NONE', #33305, 1000.000000000000000 ) ;
#11848 = CARTESIAN_POINT ( 'NONE',  ( 23.22795750573990148, -17.89249571482650225, -72.33149193979500069 ) ) ;
#11849 = CARTESIAN_POINT ( 'NONE',  ( 52.22857431453229538, 18.58359186129870011, -77.10487740174788485 ) ) ;
#11851 = ADVANCED_FACE ( 'NONE', ( #9780 ), #46470, .F. ) ;
#11850 = CARTESIAN_POINT ( 'NONE',  ( 52.73517490894950299, 18.48512909520229996, -48.54844146395180360 ) ) ;
#11852 = CYLINDRICAL_SURFACE ( 'NONE', #51829, 0.4999999999999967248 ) ;
#11853 = CARTESIAN_POINT ( 'NONE',  ( -0.1032157185578773950, -45.55972716908853926, -34.85600551168373329 ) ) ;
#11854 = VERTEX_POINT ( 'NONE', #10814 ) ;
#11855 = CARTESIAN_POINT ( 'NONE',  ( -11.80944000494479873, 2.826328597561450273, -45.03554556751399929 ) ) ;
#11856 = CARTESIAN_POINT ( 'NONE',  ( 47.51836951350739469, -54.59047688859140379, -54.92482226801399747 ) ) ;
#11857 = CARTESIAN_POINT ( 'NONE',  ( 33.13393739769620083, -15.61618894467929941, -84.65000000000000568 ) ) ;
#11858 = FACE_OUTER_BOUND ( 'NONE', #32245, .T. ) ;
#11859 = CARTESIAN_POINT ( 'NONE',  ( 61.24027180500640100, -30.79518016777799971, -16.42551006422069904 ) ) ;
#11860 = CARTESIAN_POINT ( 'NONE',  ( 71.27608674571190761, 1.386446979194299933, -61.00873193152619933 ) ) ;
#11861 = CARTESIAN_POINT ( 'NONE',  ( 10.41791033310428816, 33.00607200278869868, -23.06400185344025644 ) ) ;
#11862 = CARTESIAN_POINT ( 'NONE',  ( 72.61842109033369752, 1.039769764133420038, -61.66260107181680183 ) ) ;
#11863 = FACE_OUTER_BOUND ( 'NONE', #11257, .T. ) ;
#11864 = CARTESIAN_POINT ( 'NONE',  ( 15.23359603239730653, -8.891264927876337154, -65.91044689600897755 ) ) ;
#11865 = VERTEX_POINT ( 'NONE', #29669 ) ;
#11866 = VERTEX_POINT ( 'NONE', #26773 ) ;
#11867 = CARTESIAN_POINT ( 'NONE',  ( 11.63393739769600010, 10.38381105532060111, -54.64999999999999858 ) ) ;
#11868 = CARTESIAN_POINT ( 'NONE',  ( 15.24822091983413763, -22.38319882176496378, -58.99448675312215329 ) ) ;
#11869 = B_SPLINE_CURVE_WITH_KNOTS ( 'NONE', 3,
 ( #27910, #47595, #8261, #40238, #23711, #32340, #4582, #39981, #4074, #16912, #41270 ),
 .UNSPECIFIED., .F., .F.,
 ( 4, 1, 1, 1, 1, 1, 1, 1, 4 ),
 ( 0.000000000000000000, 0.002466451932003523115, 0.08168538299555488935, 0.1609043140592600896, 0.2401232451228069165, 0.3193421761865211650, 0.3985611072500679919, 0.4777800383136148743, 0.5000039623326250071 ),
 .UNSPECIFIED. ) ;
#11870 = ORIENTED_EDGE ( 'NONE', *, *, #33759, .F. ) ;
#11871 = CARTESIAN_POINT ( 'NONE',  ( 12.10067309664009905, -65.23675881185819492, -45.96376834473689854 ) ) ;
#11872 = CARTESIAN_POINT ( 'NONE',  ( 0.9903310742082500617, -8.665933549137170289, -34.65032322548090349 ) ) ;
#11873 = CARTESIAN_POINT ( 'NONE',  ( 53.63393739769619373, 21.88381105532059934, 16.35000000000000142 ) ) ;
#11874 = ORIENTED_EDGE ( 'NONE', *, *, #3799, .T. ) ;
#11875 = CARTESIAN_POINT ( 'NONE',  ( 10.97710700053788280, 33.58282929631926095, -23.21943985317197701 ) ) ;
#11876 = CARTESIAN_POINT ( 'NONE',  ( 44.17051537087078117, 6.707271543636243116, -69.46706789229442336 ) ) ;
#11877 = CARTESIAN_POINT ( 'NONE',  ( 15.09846882468793616, -7.705179410057033884, -34.96600043974325445 ) ) ;
#11878 = CARTESIAN_POINT ( 'NONE',  ( 8.816801753752139703, -19.41648446266970396, -44.63985384860789907 ) ) ;
#11879 = DIRECTION ( 'NONE',  ( 0.000000000000000000, 0.000000000000000000, 1.000000000000000000 ) ) ;
#11880 = CARTESIAN_POINT ( 'NONE',  ( 24.04493739739171687, -15.61672302095869469, -49.79235199249318100 ) ) ;
#11881 = CARTESIAN_POINT ( 'NONE',  ( 59.91100987953519308, -28.69340720916260068, -15.76101076566429882 ) ) ;
#11882 = VECTOR ( 'NONE', #12725, 1000.000000000000114 ) ;
#11883 = CARTESIAN_POINT ( 'NONE',  ( 63.02029346573409185, 0.8838110553206740549, -62.51131646858519275 ) ) ;
#11884 = CARTESIAN_POINT ( 'NONE',  ( 22.51680126320929887, -19.45871121662710124, -32.40515068373069596 ) ) ;
#11885 = CONICAL_SURFACE ( 'NONE', #30256, 12.92820323027549989, 0.7481802937784480800 ) ;
#11886 = CARTESIAN_POINT ( 'NONE',  ( 62.13393739769620083, 0.8838110553206759423, -65.65000000000000568 ) ) ;
#11887 = CIRCLE ( 'NONE', #10193, 16.00000000000000000 ) ;
#11888 = CARTESIAN_POINT ( 'NONE',  ( 42.89817685944129977, 14.29758682696679983, -7.114970889050010072 ) ) ;
#11889 = EDGE_CURVE ( 'NONE', #637, #37798, #42791, .T. ) ;
#11890 = CARTESIAN_POINT ( 'NONE',  ( 83.89200044194980421, 19.38381105532069881, -53.92796738110899923 ) ) ;
#11891 = EDGE_CURVE ( 'NONE', #42867, #9498, #27577, .T. ) ;
#11892 = CARTESIAN_POINT ( 'NONE',  ( 83.27189663703491362, -44.88035785588050430, -46.76788818508799750 ) ) ;
#11893 = CARTESIAN_POINT ( 'NONE',  ( 64.67348939754930370, 1.419996320997050088, -70.13930819973541020 ) ) ;
#11894 = CARTESIAN_POINT ( 'NONE',  ( 8.286183717290461104, -13.08725974823009963, -42.60689890039779470 ) ) ;
#11895 = ORIENTED_EDGE ( 'NONE', *, *, #20981, .F. ) ;
#11896 = DIRECTION ( 'NONE',  ( 0.000000000000000000, 0.000000000000000000, 1.000000000000000000 ) ) ;
#11897 = CARTESIAN_POINT ( 'NONE',  ( 16.08016673437809985, -51.03387969365790156, -20.14986617604289876 ) ) ;
#11898 = CARTESIAN_POINT ( 'NONE',  ( 50.95029971905736943, -35.30930468315340676, -76.37425139971915655 ) ) ;
#11899 = DIRECTION ( 'NONE',  ( 0.000000000000000000, 0.000000000000000000, -1.000000000000000000 ) ) ;
#11900 = DIRECTION ( 'NONE',  ( 0.000000000000000000, 0.000000000000000000, -1.000000000000000000 ) ) ;
#11901 = VERTEX_POINT ( 'NONE', #17889 ) ;
#11902 = CARTESIAN_POINT ( 'NONE',  ( -6.924536278744959361, -46.06766666375389718, -5.623594431461650167 ) ) ;
#11903 = DIRECTION ( 'NONE',  ( 1.000000000000000000, 0.000000000000000000, 0.000000000000000000 ) ) ;
#11904 = DIRECTION ( 'NONE',  ( 0.000000000000000000, 0.000000000000000000, -1.000000000000000000 ) ) ;
#11905 = CARTESIAN_POINT ( 'NONE',  ( 63.13475262569159696, 0.9955677559369568996, -62.34557165980569948 ) ) ;
#11906 = CARTESIAN_POINT ( 'NONE',  ( 57.40560941794409899, -50.51630527438410212, -53.29417222457460213 ) ) ;
#11907 = CARTESIAN_POINT ( 'NONE',  ( 43.05690220861699657, 12.44174133896570034, -4.900907769916179824 ) ) ;
#11908 = ADVANCED_FACE ( 'NONE', ( #33860 ), #29922, .T. ) ;
#11909 = LINE ( 'NONE', #19495, #19054 ) ;
#11910 = CARTESIAN_POINT ( 'NONE',  ( 55.04426526048000312, -48.50067717176560222, -48.28429872967510050 ) ) ;
#11911 = CARTESIAN_POINT ( 'NONE',  ( 12.14969989039511944, -8.703725779495739445, -75.12571185134946461 ) ) ;
#11912 = CARTESIAN_POINT ( 'NONE',  ( 9.543046712767974782, -17.38737308065900322, -63.36948542607716206 ) ) ;
#11913 = CARTESIAN_POINT ( 'NONE',  ( 17.52125950177649827, -52.24941868644869913, -75.96018872839380265 ) ) ;
#11914 = EDGE_CURVE ( 'NONE', #7747, #13116, #4066, .T. ) ;
#11915 = AXIS2_PLACEMENT_3D ( 'NONE', #32628, #28977, #4881 ) ;
#11916 = CARTESIAN_POINT ( 'NONE',  ( 14.71419660400150065, -8.302432699283889050, -64.50631165503649811 ) ) ;
#11917 = PLANE ( 'NONE',  #20351 ) ;
#11918 = CARTESIAN_POINT ( 'NONE',  ( 22.09873218501700265, -19.37966938420589713, -80.63198581093500650 ) ) ;
#11919 = CARTESIAN_POINT ( 'NONE',  ( 63.37834727611930674, 0.9755120847815890173, -61.99042069074619832 ) ) ;
#11920 = EDGE_LOOP ( 'NONE', ( #44031, #36119, #36322, #35953 ) ) ;
#11921 = CARTESIAN_POINT ( 'NONE',  ( 8.804713206766638933, 31.98843531701869836, -46.67024040703379484 ) ) ;
#11922 = AXIS2_PLACEMENT_3D ( 'NONE', #39237, #3083, #31342 ) ;
#11923 = DIRECTION ( 'NONE',  ( -0.1961161351381836004, -1.134894647394604573E-15, -0.9805806756909204447 ) ) ;
#11924 = AXIS2_PLACEMENT_3D ( 'NONE', #20488, #49536, #23644 ) ;
#11925 = CARTESIAN_POINT ( 'NONE',  ( 9.847451328762401701, -11.61977205256459911, -81.23899999999999011 ) ) ;
#11926 = VERTEX_POINT ( 'NONE', #39877 ) ;
#11927 = CARTESIAN_POINT ( 'NONE',  ( 17.21347160910339724, 21.88381105532300097, -76.14999999999999147 ) ) ;
#11928 = ORIENTED_EDGE ( 'NONE', *, *, #10408, .F. ) ;
#11929 = ORIENTED_EDGE ( 'NONE', *, *, #41272, .F. ) ;
#11930 = CARTESIAN_POINT ( 'NONE',  ( -31.07316938349034885, 8.133811055320650851, 17.05710678118654755 ) ) ;
#11931 = CARTESIAN_POINT ( 'NONE',  ( 21.81516569332449862, -10.17359938674849928, -81.23899999999999011 ) ) ;
#11932 = CARTESIAN_POINT ( 'NONE',  ( 23.83903832650269905, -13.54551673756389363, -73.70899818572770812 ) ) ;
#11933 = VERTEX_POINT ( 'NONE', #31213 ) ;
#11934 = DIRECTION ( 'NONE',  ( 0.000000000000000000, -1.000000000000000000, 0.000000000000000000 ) ) ;
#11935 = EDGE_LOOP ( 'NONE', ( #3051, #49191, #5949, #12552 ) ) ;
#11936 = CARTESIAN_POINT ( 'NONE',  ( 14.29653415316120046, -8.806893203457351049, -42.26328591669919632 ) ) ;
#11937 = CARTESIAN_POINT ( 'NONE',  ( 18.13393739769630031, 1.391621760993470014, -35.14999999999999858 ) ) ;
#11938 = ORIENTED_EDGE ( 'NONE', *, *, #15841, .T. ) ;
#11939 = ORIENTED_EDGE ( 'NONE', *, *, #23058, .T. ) ;
#11940 = CARTESIAN_POINT ( 'NONE',  ( 46.40057797168859821, -53.02061573618119894, -76.14999999999999147 ) ) ;
#11941 = CARTESIAN_POINT ( 'NONE',  ( 61.18292228697600876, 14.26772679133280164, -47.53321244258839329 ) ) ;
#11942 = LINE ( 'NONE', #31308, #16322 ) ;
#11943 = EDGE_CURVE ( 'NONE', #24151, #425, #12976, .T. ) ;
#11944 = CARTESIAN_POINT ( 'NONE',  ( 16.13393739769629676, -15.61618894467929941, -20.75000000000000000 ) ) ;
#11945 = CARTESIAN_POINT ( 'NONE',  ( -5.359418298255730129, 15.90354631731749890, -5.235650387110280413 ) ) ;
#11946 = AXIS2_PLACEMENT_3D ( 'NONE', #36860, #4625, #32640 ) ;
#11947 = CIRCLE ( 'NONE', #41231, 0.5000000000000000000 ) ;
#11948 = DIRECTION ( 'NONE',  ( 0.000000000000000000, 0.000000000000000000, -1.000000000000000000 ) ) ;
#11949 = CARTESIAN_POINT ( 'NONE',  ( 57.34384300794079792, 14.38573366476320103, -26.19324057846490206 ) ) ;
#11950 = CARTESIAN_POINT ( 'NONE',  ( 15.59252480001009999, -7.787164702652099812, -60.76552800450640035 ) ) ;
#11951 = ORIENTED_EDGE ( 'NONE', *, *, #8678, .T. ) ;
#11952 = B_SPLINE_CURVE_WITH_KNOTS ( 'NONE', 3,
 ( #23635, #15547, #46763, #2725, #35194, #38892, #19470, #35457, #47275, #51452, #39399, #39651, #43334, #31504, #7426, #47523, #51197, #34932 ),
 .UNSPECIFIED., .F., .F.,
 ( 4, 2, 2, 2, 2, 2, 2, 2, 4 ),
 ( 0.000000000000000000, 0.06250013864589283596, 0.1250002772917856719, 0.1875004159376785218, 0.2500005545835713439, 0.3125006932294640549, 0.3750008318753568215, 0.4375009705212495326, 0.5000011091671422436 ),
 .UNSPECIFIED. ) ;
#11953 = CARTESIAN_POINT ( 'NONE',  ( 62.63393739769619373, -39.36618894467940066, 16.35000000000000142 ) ) ;
#11954 = CARTESIAN_POINT ( 'NONE',  ( -0.8677628140554130010, -51.96998285431273246, -20.56421356237309794 ) ) ;
#11955 = CARTESIAN_POINT ( 'NONE',  ( 72.48038400710301232, 1.530257664727401545, -68.84999999999999432 ) ) ;
#11956 = CARTESIAN_POINT ( 'NONE',  ( 72.06663613036050720, 1.456055805561079941, -69.85592311231539497 ) ) ;
#11957 = CARTESIAN_POINT ( 'NONE',  ( 42.59271315789397505, -39.82626481978887512, -73.46854499661243665 ) ) ;
#11958 = CARTESIAN_POINT ( 'NONE',  ( 46.63393739769619373, 7.878491304262099426, -34.64999999999999858 ) ) ;
#11959 = CARTESIAN_POINT ( 'NONE',  ( 12.44373459733649945, 18.75032477250240248, -21.13286269089030256 ) ) ;
#11960 = CARTESIAN_POINT ( 'NONE',  ( 47.01289654797179907, 23.18946113012230015, -75.36289900858220392 ) ) ;
#11961 = CARTESIAN_POINT ( 'NONE',  ( 48.65508916750899715, -53.94707814549249747, -54.55809205546240293 ) ) ;
#11962 = LINE ( 'NONE', #32607, #46568 ) ;
#11963 = AXIS2_PLACEMENT_3D ( 'NONE', #8915, #517, #16505 ) ;
#11964 = CARTESIAN_POINT ( 'NONE',  ( 59.01105867686166562, -2.461703131905387920, -15.68225890942153988 ) ) ;
#11965 = LINE ( 'NONE', #4862, #24584 ) ;
#11966 = EDGE_CURVE ( 'NONE', #8034, #20276, #2946, .T. ) ;
#11967 = CARTESIAN_POINT ( 'NONE',  ( 47.66581657685510010, 23.29145150881430126, -55.09436269531529717 ) ) ;
#11968 = EDGE_LOOP ( 'NONE', ( #48302, #46330, #46112, #41091 ) ) ;
#11969 = CARTESIAN_POINT ( 'NONE',  ( 19.44826417394619966, -21.62186115282320031, -81.18618737929101314 ) ) ;
#11970 = DIRECTION ( 'NONE',  ( -1.000000000000000000, 0.000000000000000000, 0.000000000000000000 ) ) ;
#11971 = ORIENTED_EDGE ( 'NONE', *, *, #43304, .T. ) ;
#11972 = CARTESIAN_POINT ( 'NONE',  ( 20.78393739769619941, -15.61618894467929941, -9.721247897589949005 ) ) ;
#11973 = CARTESIAN_POINT ( 'NONE',  ( 60.81220464489970823, -45.55367163794920060, -47.44138936351279767 ) ) ;
#11974 = CARTESIAN_POINT ( 'NONE',  ( 49.40539548398250247, -53.49785366680099941, -54.15746054658189479 ) ) ;
#11975 = FACE_OUTER_BOUND ( 'NONE', #242, .T. ) ;
#11977 = CARTESIAN_POINT ( 'NONE',  ( 24.04493741700738951, -14.58064883687476154, -35.75066221455982429 ) ) ;
#11976 = CARTESIAN_POINT ( 'NONE',  ( 41.47362262140879352, 8.473564071847876633, -78.87161307600275961 ) ) ;
#11978 = CARTESIAN_POINT ( 'NONE',  ( 30.03825186937055136, 4.383319667191443614, -84.60795687872310111 ) ) ;
#11979 = CARTESIAN_POINT ( 'NONE',  ( 14.06334626515088537, -7.911066143799638795, -66.92433398933782485 ) ) ;
#11980 = EDGE_LOOP ( 'NONE', ( #26269, #34173, #29449, #6708 ) ) ;
#11981 = CARTESIAN_POINT ( 'NONE',  ( 18.13393739769620083, -37.52509124488599923, -54.64999999999999858 ) ) ;
#11982 = ORIENTED_EDGE ( 'NONE', *, *, #4771, .F. ) ;
#11983 = ORIENTED_EDGE ( 'NONE', *, *, #5257, .F. ) ;
#11984 = CARTESIAN_POINT ( 'NONE',  ( 24.04493739769619864, -15.61618894467929941, -32.14999999999999858 ) ) ;
#11985 = DIRECTION ( 'NONE',  ( 0.000000000000000000, -1.000000000000000000, 0.000000000000000000 ) ) ;
#11986 = AXIS2_PLACEMENT_3D ( 'NONE', #48830, #45670, #1643 ) ;
#11987 = CARTESIAN_POINT ( 'NONE',  ( 76.40287782345053813, -19.96602362163603317, -12.80893705397542348 ) ) ;
#11988 = ORIENTED_EDGE ( 'NONE', *, *, #16122, .T. ) ;
#11989 = ORIENTED_EDGE ( 'NONE', *, *, #32012, .T. ) ;
#11990 = DIRECTION ( 'NONE',  ( 1.000000000000000000, 0.000000000000000000, 0.000000000000000000 ) ) ;
#11991 = DIRECTION ( 'NONE',  ( 0.000000000000000000, 0.000000000000000000, 1.000000000000000000 ) ) ;
#11992 = CARTESIAN_POINT ( 'NONE',  ( 46.68434392863400717, 16.15099216771209001, 16.85000000000000142 ) ) ;
#11993 = CARTESIAN_POINT ( 'NONE',  ( 20.19692254461188696, -10.17265177529750275, -46.15686990965734537 ) ) ;
#11994 = CARTESIAN_POINT ( 'NONE',  ( 58.92068922470849657, -3.124196156303379990, -15.65000643880829934 ) ) ;
#11995 = CARTESIAN_POINT ( 'NONE',  ( 51.57064462678510353, -49.04885115171509824, -76.80688256002839864 ) ) ;
#11996 = ORIENTED_EDGE ( 'NONE', *, *, #29368, .T. ) ;
#11997 = DIRECTION ( 'NONE',  ( -0.7226652920947608250, -0.6911981449639416075, 0.000000000000000000 ) ) ;
#11998 = FACE_OUTER_BOUND ( 'NONE', #29905, .T. ) ;
#11999 = CARTESIAN_POINT ( 'NONE',  ( 22.90093658489038475, -15.39729050644079678, -34.44252498390390826 ) ) ;
#12000 = LINE ( 'NONE', #20098, #42055 ) ;
#12001 = CARTESIAN_POINT ( 'NONE',  ( 11.32940628474790046, -21.82128591219670000, -50.72221764996669435 ) ) ;
#12002 = CARTESIAN_POINT ( 'NONE',  ( 13.29231789701340105, -50.60014296140869305, -21.35983077129230168 ) ) ;
#12003 = VECTOR ( 'NONE', #49740, 1000.000000000000000 ) ;
#12004 = EDGE_CURVE ( 'NONE', #48345, #14040, #35419, .T. ) ;
#12005 = CARTESIAN_POINT ( 'NONE',  ( 14.78993376734673149, -8.692590644934696797, -64.28614875239208004 ) ) ;
#12006 = CARTESIAN_POINT ( 'NONE',  ( 70.83393739769717001, -48.11618894467422081, -70.54999999999975557 ) ) ;
#12008 = EDGE_CURVE ( 'NONE', #17711, #25812, #28419, .T. ) ;
#12007 = CARTESIAN_POINT ( 'NONE',  ( 61.05532957801759864, -45.35430874236069343, -46.96571179725230394 ) ) ;
#12009 = EDGE_CURVE ( 'NONE', #1350, #10341, #3303, .T. ) ;
#12010 = CARTESIAN_POINT ( 'NONE',  ( 14.34417029198879945, -51.11618894467930119, -74.14999999999999147 ) ) ;
#12011 = CARTESIAN_POINT ( 'NONE',  ( 10.13629284140139930, -19.32709435317449831, -53.67081198986049628 ) ) ;
#12012 = CARTESIAN_POINT ( 'NONE',  ( 46.50679657349800067, -40.08028361939490480, -54.64999999999999858 ) ) ;
#12013 = EDGE_CURVE ( 'NONE', #39953, #23932, #15307, .T. ) ;
#12014 = ORIENTED_EDGE ( 'NONE', *, *, #36788, .F. ) ;
#12015 = CARTESIAN_POINT ( 'NONE',  ( 14.34420760053260047, -51.11618258419110106, -74.34711752987750799 ) ) ;
#12016 = CARTESIAN_POINT ( 'NONE',  ( 47.32074021863829927, -54.70663448010740382, -54.72782118794329875 ) ) ;
#12017 = CARTESIAN_POINT ( 'NONE',  ( 21.54527898443459932, -11.45754588894539516, -38.24448936043144442 ) ) ;
#12018 = CIRCLE ( 'NONE', #49698, 18.86180339887500068 ) ;
#12019 = CARTESIAN_POINT ( 'NONE',  ( 61.28610861176739633, 13.99802266614350010, -46.37203261889099792 ) ) ;
#12020 = AXIS2_PLACEMENT_3D ( 'NONE', #36200, #310, #47762 ) ;
#12021 = DIRECTION ( 'NONE',  ( 0.000000000000000000, 0.000000000000000000, -1.000000000000000000 ) ) ;
#12022 = EDGE_CURVE ( 'NONE', #31864, #37534, #45166, .T. ) ;
#12023 = CARTESIAN_POINT ( 'NONE',  ( 16.13393740247629893, -15.61618988478180015, -4.296538730098649950 ) ) ;
#12024 = DIRECTION ( 'NONE',  ( 0.000000000000000000, 0.000000000000000000, -1.000000000000000000 ) ) ;
#12025 = CARTESIAN_POINT ( 'NONE',  ( 17.07866728675466206, -7.737244263286628509, -65.04561884461543286 ) ) ;
#12027 = CARTESIAN_POINT ( 'NONE',  ( -3.547017152609819757, -48.75843093089891767, -5.665571190130843426 ) ) ;
#12026 = DIRECTION ( 'NONE',  ( 0.000000000000000000, 1.000000000000000000, 0.000000000000000000 ) ) ;
#12028 = FACE_OUTER_BOUND ( 'NONE', #14354, .T. ) ;
#12029 = EDGE_CURVE ( 'NONE', #38811, #5608, #29025, .T. ) ;
#12030 = CARTESIAN_POINT ( 'NONE',  ( 13.10176660314549935, 34.29157359959339857, -47.73582792185820267 ) ) ;
#12031 = ORIENTED_EDGE ( 'NONE', *, *, #14057, .F. ) ;
#12032 = CARTESIAN_POINT ( 'NONE',  ( 52.74572974338470033, -49.72478476443930617, -48.77972035026300546 ) ) ;
#12033 = ORIENTED_EDGE ( 'NONE', *, *, #6621, .F. ) ;
#12034 = CARTESIAN_POINT ( 'NONE',  ( 43.68113622443509314, 6.447734790222596324, -71.88154124489368257 ) ) ;
#12035 = CARTESIAN_POINT ( 'NONE',  ( 20.29261124649605819, -21.02750557501780548, -74.74448689122068856 ) ) ;
#12036 = DIRECTION ( 'NONE',  ( 0.000000000000000000, 0.000000000000000000, -1.000000000000000000 ) ) ;
#12037 = CARTESIAN_POINT ( 'NONE',  ( 83.13571748553259511, 13.71928646809350028, -46.75830440892689666 ) ) ;
#12038 = CARTESIAN_POINT ( 'NONE',  ( 12.53098345279100023, -21.67929718777690340, -55.12349000844969993 ) ) ;
#12039 = CARTESIAN_POINT ( 'NONE',  ( 53.23851273770399928, 18.29663818490410421, -49.17579072038760302 ) ) ;
#12040 = CARTESIAN_POINT ( 'NONE',  ( 55.98847043416329683, -45.29423959430500446, -15.93199093155540247 ) ) ;
#12041 = CARTESIAN_POINT ( 'NONE',  ( 52.90929476643909624, 18.25992211886340044, -27.14407627714519933 ) ) ;
#12042 = AXIS2_PLACEMENT_3D ( 'NONE', #11782, #4155, #28510 ) ;
#12043 = EDGE_LOOP ( 'NONE', ( #47705, #40848, #29163, #48593 ) ) ;
#12044 = CARTESIAN_POINT ( 'NONE',  ( 14.08945181123240076, -8.039459645705720803, -42.70361172200129118 ) ) ;
#12045 = ORIENTED_EDGE ( 'NONE', *, *, #48917, .F. ) ;
#12046 = CARTESIAN_POINT ( 'NONE',  ( 11.65058183552799953, -65.39170010508581754, -17.77752805455190099 ) ) ;
#12047 = CARTESIAN_POINT ( 'NONE',  ( 9.869349621126580985, 32.08736743983219952, -46.22151743497509813 ) ) ;
#12048 = CARTESIAN_POINT ( 'NONE',  ( 71.83393739769618946, 10.88381105532070059, -62.44999999999999574 ) ) ;
#12049 =( BOUNDED_CURVE ( )  B_SPLINE_CURVE ( 2, ( #28403, #44409, #40994 ),
 .UNSPECIFIED., .F., .T. ) 
 B_SPLINE_CURVE_WITH_KNOTS ( ( 3, 3 ),
 ( 0.09013418064983300115, 2.097305204717760052 ),
 .UNSPECIFIED. ) 
 CURVE ( )  GEOMETRIC_REPRESENTATION_ITEM ( )  RATIONAL_B_SPLINE_CURVE ( ( 1.000760730674089993, 1.008874108731790065, 1.001093714201390039 ) ) 
 REPRESENTATION_ITEM ( '' )  );
#12050 = CARTESIAN_POINT ( 'NONE',  ( 48.94887823264109272, -53.89549600984270228, -54.63676433852469927 ) ) ;
#12051 = CARTESIAN_POINT ( 'NONE',  ( 11.08250670836754459, -64.97041830570583443, -23.10046800189048710 ) ) ;
#12052 = CARTESIAN_POINT ( 'NONE',  ( 51.35161527711753848, 3.349069727626160287, -76.64881736422908887 ) ) ;
#12053 = EDGE_CURVE ( 'NONE', #51185, #18289, #29096, .T. ) ;
#12054 = ORIENTED_EDGE ( 'NONE', *, *, #21655, .T. ) ;
#12055 = CARTESIAN_POINT ( 'NONE',  ( 50.87748861976533021, -52.21589981770337374, -52.61226359342039416 ) ) ;
#12056 = CARTESIAN_POINT ( 'NONE',  ( 68.13393739769620083, 19.38381105532069881, -65.65000000000000568 ) ) ;
#12057 = AXIS2_PLACEMENT_3D ( 'NONE', #6114, #33615, #42014 ) ;
#12058 = CARTESIAN_POINT ( 'NONE',  ( 68.13393739769814772, 19.38381105532029736, -71.50000000000200373 ) ) ;
#12059 = ORIENTED_EDGE ( 'NONE', *, *, #4317, .F. ) ;
#12060 = CARTESIAN_POINT ( 'NONE',  ( 11.67619942398489918, -64.89165360645620240, -45.08494251881790404 ) ) ;
#12061 = CARTESIAN_POINT ( 'NONE',  ( 56.48517904086930486, 19.30797284152329851, -52.93690031776429805 ) ) ;
#12062 = DIRECTION ( 'NONE',  ( 1.000000000000000000, 0.000000000000000000, 0.000000000000000000 ) ) ;
#12063 = CARTESIAN_POINT ( 'NONE',  ( 15.69662371953226376, -7.686623656191616583, -48.99006696521935567 ) ) ;
#12064 = B_SPLINE_CURVE_WITH_KNOTS ( 'NONE', 3,
 ( #49450, #18429, #25303, #37378, #17465, #9168, #49015, #34021, #45329, #50031 ),
 .UNSPECIFIED., .F., .F.,
 ( 4, 1, 1, 1, 1, 1, 1, 4 ),
 ( 0.000000000000000000, 0.03008848090787212201, 0.1093074119714910891, 0.1885263430351258873, 0.2677452740987448787, 0.3469642051623627044, 0.4261831362259816403, 0.4999981796106400811 ),
 .UNSPECIFIED. ) ;
#12065 = ORIENTED_EDGE ( 'NONE', *, *, #45992, .F. ) ;
#12066 =( LENGTH_UNIT ( ) NAMED_UNIT ( * ) SI_UNIT ( .MILLI., .METRE. ) );
#12067 = DIRECTION ( 'NONE',  ( 0.000000000000000000, 0.000000000000000000, 1.000000000000000000 ) ) ;
#12068 = DIRECTION ( 'NONE',  ( 0.000000000000000000, 0.000000000000000000, 1.000000000000000000 ) ) ;
#12069 = CARTESIAN_POINT ( 'NONE',  ( 44.94022070389028300, 1.883811055320663064, -54.43277924001891677 ) ) ;
#12070 = CARTESIAN_POINT ( 'NONE',  ( 13.71480148060770077, -23.49847931751850183, -78.38711848170969176 ) ) ;
#12071 = CARTESIAN_POINT ( 'NONE',  ( 56.50083414075169941, 19.52878523282910450, -74.28948443064300022 ) ) ;
#12072 = ORIENTED_EDGE ( 'NONE', *, *, #39212, .F. ) ;
#12073 = EDGE_CURVE ( 'NONE', #13190, #11926, #46809, .T. ) ;
#12074 = CARTESIAN_POINT ( 'NONE',  ( 22.43708255015009811, -11.64415483200579970, -68.05366966235949633 ) ) ;
#12075 = LINE ( 'NONE', #43528, #2984 ) ;
#12076 = CARTESIAN_POINT ( 'NONE',  ( 10.40096277903999855, -20.74754741771700139, -32.14999999999999858 ) ) ;
#12077 = ADVANCED_FACE ( 'NONE', ( #49038 ), #17556, .F. ) ;
#12078 = VECTOR ( 'NONE', #23492, 1000.000000000000000 ) ;
#12079 = CARTESIAN_POINT ( 'NONE',  ( 47.37011575340810055, 23.44240931280840101, -74.19735651161070678 ) ) ;
#12080 = CYLINDRICAL_SURFACE ( 'NONE', #1660, 0.4999999999999994449 ) ;
#12081 = DIRECTION ( 'NONE',  ( 0.000000000000000000, 0.000000000000000000, 1.000000000000000000 ) ) ;
#12082 = CARTESIAN_POINT ( 'NONE',  ( 11.98449920102340016, 33.55497157401369890, -16.08642242877740003 ) ) ;
#12083 = CARTESIAN_POINT ( 'NONE',  ( 21.53907483071889928, -21.84252093382090010, -77.78010429264469394 ) ) ;
#12084 = CARTESIAN_POINT ( 'NONE',  ( 56.68744973047850522, -50.63300783658069548, -75.04390987627759557 ) ) ;
#12086 = DIRECTION ( 'NONE',  ( 0.000000000000000000, 0.000000000000000000, -1.000000000000000000 ) ) ;
#12085 = CARTESIAN_POINT ( 'NONE',  ( 57.34991680858041718, 19.38381105532069881, -53.92361874566621793 ) ) ;
#12087 = CARTESIAN_POINT ( 'NONE',  ( 63.17872741171709805, 1.188582381068100213, -68.85996346914730282 ) ) ;
#12088 = CARTESIAN_POINT ( 'NONE',  ( 61.30667203655529818, 14.01553559058869780, -46.90228508237380112 ) ) ;
#12089 = EDGE_CURVE ( 'NONE', #33592, #12246, #24209, .T. ) ;
#12090 = DIRECTION ( 'NONE',  ( 0.000000000000000000, 0.000000000000000000, -1.000000000000000000 ) ) ;
#12091 = ORIENTED_EDGE ( 'NONE', *, *, #20306, .T. ) ;
#12092 = CARTESIAN_POINT ( 'NONE',  ( 52.98014239974310158, -49.58212897128409935, -48.77045029443840463 ) ) ;
#12093 = CARTESIAN_POINT ( 'NONE',  ( 61.19443126428920010, -45.21152309989860640, -27.59429383128480140 ) ) ;
#12094 = CARTESIAN_POINT ( 'NONE',  ( 19.36025468743955358, -22.91325498030835206, -66.15954722856929493 ) ) ;
#12095 = CARTESIAN_POINT ( 'NONE',  ( 57.35253518667929740, 14.57826363733579988, -26.27218797145850004 ) ) ;
#12096 = CARTESIAN_POINT ( 'NONE',  ( 15.31832100281680020, -8.210686686118460642, -71.69774049128589866 ) ) ;
#12097 = CARTESIAN_POINT ( 'NONE',  ( 51.21390329036389488, 18.63858452962650247, -76.33091581055249719 ) ) ;
#12098 = CARTESIAN_POINT ( 'NONE',  ( 53.13943604555799993, 18.27600435916260224, -48.93645284067880397 ) ) ;
#12099 = CARTESIAN_POINT ( 'NONE',  ( 71.05099032166229733, 1.383136297697689976, -70.36878149631539259 ) ) ;
#12100 = CARTESIAN_POINT ( 'NONE',  ( -0.007164427059776000244, -45.70803162167019451, -34.77269723891829756 ) ) ;
#12101 = EDGE_LOOP ( 'NONE', ( #24128, #6702, #50192, #49381 ) ) ;
#12102 = DIRECTION ( 'NONE',  ( 0.000000000000000000, 0.000000000000000000, 1.000000000000000000 ) ) ;
#12103 = CARTESIAN_POINT ( 'NONE',  ( 47.70972474023349719, -54.46928834314500278, -54.77964464375110509 ) ) ;
#12104 = DIRECTION ( 'NONE',  ( 0.000000000000000000, 0.000000000000000000, -1.000000000000000000 ) ) ;
#12105 = CARTESIAN_POINT ( 'NONE',  ( 68.13393739769618662, -31.81618894467930403, -51.14999999999999858 ) ) ;
#12106 = CARTESIAN_POINT ( 'NONE',  ( 59.54770650857670233, -29.44221205149689879, -15.81971576896729736 ) ) ;
#12107 = CARTESIAN_POINT ( 'NONE',  ( 71.21710443884710173, 1.384378348444510243, -60.98758765055369935 ) ) ;
#12108 = CARTESIAN_POINT ( 'NONE',  ( 2.558369240368420172, -25.18609768228349921, -34.64999999999999858 ) ) ;
#12109 = CARTESIAN_POINT ( 'NONE',  ( 72.68564311439560299, 1.087300712305049988, -61.74844476645729685 ) ) ;
#12110 = ADVANCED_FACE ( 'NONE', ( #48509 ), #36435, .T. ) ;
#12111 = CARTESIAN_POINT ( 'NONE',  ( 51.35163416435118933, -34.58141209747533651, -76.64883399551484899 ) ) ;
#12112 = CARTESIAN_POINT ( 'NONE',  ( 64.98600614086839755, 1.191644800533210091, -70.64005307315139248 ) ) ;
#12113 = ORIENTED_EDGE ( 'NONE', *, *, #22211, .T. ) ;
#12114 = EDGE_CURVE ( 'NONE', #33533, #15737, #38471, .T. ) ;
#12115 = VERTEX_POINT ( 'NONE', #16529 ) ;
#12116 = CIRCLE ( 'NONE', #22931, 15.56227766016840164 ) ;
#12117 = CARTESIAN_POINT ( 'NONE',  ( 13.05521822061467319, 18.23736444591386174, -34.79644660940673617 ) ) ;
#12118 = CARTESIAN_POINT ( 'NONE',  ( 51.15515350355274649, 0.3890328154924098114, -17.08415396337089120 ) ) ;
#12119 = VERTEX_POINT ( 'NONE', #8944 ) ;
#12120 = CARTESIAN_POINT ( 'NONE',  ( 8.222917554388192940, -14.58078674515130757, -58.54932919163416472 ) ) ;
#12121 = CARTESIAN_POINT ( 'NONE',  ( 14.60414996492981388, -9.001304452785721111, -49.88044619144234559 ) ) ;
#12122 = EDGE_LOOP ( 'NONE', ( #42167, #47607, #36576, #9768 ) ) ;
#12123 = DIRECTION ( 'NONE',  ( 0.7071067811865457964, -0.7071067811865492381, 0.000000000000000000 ) ) ;
#12124 = CARTESIAN_POINT ( 'NONE',  ( 17.63499105033400127, 0.9265147500389789847, -34.64999999999999858 ) ) ;
#12125 = DIRECTION ( 'NONE',  ( 0.000000000000000000, 1.000000000000000000, 0.000000000000000000 ) ) ;
#12126 = CARTESIAN_POINT ( 'NONE',  ( 15.64915313475499836, -7.385289584685909681, -45.27360529711689452 ) ) ;
#12127 = CARTESIAN_POINT ( 'NONE',  ( 45.16599383043609350, 2.109473049736759975, -34.94655432540119477 ) ) ;
#12128 = CONICAL_SURFACE ( 'NONE', #17985, 3.567506086244481622, 0.04995839572194331335 ) ;
#12129 = CARTESIAN_POINT ( 'NONE',  ( 10.72320681404810117, 33.67578529855150293, -17.84617904793899967 ) ) ;
#12130 = B_SPLINE_CURVE_WITH_KNOTS ( 'NONE', 3,
 ( #10804, #30438, #11064, #39357, #31201, #10286, #42778, #2681 ),
 .UNSPECIFIED., .F., .F.,
 ( 4, 2, 2, 4 ),
 ( 0.5000003605096956516, 0.6249999999981298293, 0.8249999999991262101, 1.000000000000000000 ),
 .UNSPECIFIED. ) ;
#12131 = CARTESIAN_POINT ( 'NONE',  ( 0.000000000000000000, 0.000000000000000000, 0.000000000000000000 ) ) ;
#12132 = ORIENTED_EDGE ( 'NONE', *, *, #42673, .F. ) ;
#12133 = EDGE_CURVE ( 'NONE', #15707, #22659, #7495, .T. ) ;
#12134 = CARTESIAN_POINT ( 'NONE',  ( 22.46012250960815138, -20.47783959759377126, -42.00066438588036988 ) ) ;
#12135 = CARTESIAN_POINT ( 'NONE',  ( 16.12664591956130167, -8.165911054638401723, -35.73234578840269648 ) ) ;
#12136 = CARTESIAN_POINT ( 'NONE',  ( 43.28347309149560829, 14.32586227162870074, -7.371246978530599847 ) ) ;
#12137 = ADVANCED_FACE ( 'NONE', ( #36185, #16277 ), #28833, .T. ) ;
#12138 = CARTESIAN_POINT ( 'NONE',  ( 14.53578026856690109, 20.42331001517590394, -75.51792558472199346 ) ) ;
#12139 = LINE ( 'NONE', #4780, #24792 ) ;
#12140 = CARTESIAN_POINT ( 'NONE',  ( 82.57306898050271116, -45.18814731124680151, -46.98632580443239704 ) ) ;
#12141 = CARTESIAN_POINT ( 'NONE',  ( 64.12887023277500020, 1.457834087086459895, -69.79194131696009151 ) ) ;
#12142 = CARTESIAN_POINT ( 'NONE',  ( 9.432779887650410089, -10.81231459843210096, -40.70564455487080124 ) ) ;
#12143 = ORIENTED_EDGE ( 'NONE', *, *, #5646, .F. ) ;
#12144 = CARTESIAN_POINT ( 'NONE',  ( 52.84768130634319760, -49.63793414090860523, -27.92371165755740137 ) ) ;
#12145 = AXIS2_PLACEMENT_3D ( 'NONE', #31432, #51638, #15732 ) ;
#12146 = CARTESIAN_POINT ( 'NONE',  ( 15.72190426419749976, -50.88626546307889953, -20.14992017774540045 ) ) ;
#12147 = CARTESIAN_POINT ( 'NONE',  ( 50.87985442507742562, -35.43346530991949805, -76.33943627716247704 ) ) ;
#12148 = CARTESIAN_POINT ( 'NONE',  ( 22.46012609900209256, -20.47783468274219132, -64.00066659774759614 ) ) ;
#12149 = CARTESIAN_POINT ( 'NONE',  ( 22.90090025472304447, -15.64040673669522796, -56.45396410355146344 ) ) ;
#12150 = DIRECTION ( 'NONE',  ( 0.000000000000000000, -1.000000000000000000, 0.000000000000000000 ) ) ;
#12151 = ORIENTED_EDGE ( 'NONE', *, *, #37263, .F. ) ;
#12152 = FACE_OUTER_BOUND ( 'NONE', #17410, .T. ) ;
#12153 = CARTESIAN_POINT ( 'NONE',  ( 47.31649804177600060, 23.47503745077689885, -54.66794107860329177 ) ) ;
#12154 = CARTESIAN_POINT ( 'NONE',  ( 17.01981387517692568, -22.38317777230120953, -48.91115463206005387 ) ) ;
#12155 = CARTESIAN_POINT ( 'NONE',  ( 63.36863247553639411, 1.371651820402770117, -62.65029732562830844 ) ) ;
#12156 = CARTESIAN_POINT ( 'NONE',  ( 13.79563961991219934, 19.20557301982950094, -21.08562558918019647 ) ) ;
#12157 = CARTESIAN_POINT ( 'NONE',  ( 57.37198100508690857, -50.16664033240260068, -52.65631614168299990 ) ) ;
#12158 = CARTESIAN_POINT ( 'NONE',  ( 42.29463403588689374, 12.88442639002479950, -4.936190358464100036 ) ) ;
#12159 = FACE_OUTER_BOUND ( 'NONE', #8619, .T. ) ;
#12160 = DIRECTION ( 'NONE',  ( 0.000000000000000000, 0.000000000000000000, -1.000000000000000000 ) ) ;
#12161 = CARTESIAN_POINT ( 'NONE',  ( 55.51244966342819964, -48.25538224542870580, -48.24951049977990181 ) ) ;
#12162 = CARTESIAN_POINT ( 'NONE',  ( -0.05506254389775910169, -20.75690083494706428, -34.81434777529929647 ) ) ;
#12163 = CARTESIAN_POINT ( 'NONE',  ( 68.13393739769598767, -2.032350560839250253, -102.2016796975539989 ) ) ;
#12164 = CARTESIAN_POINT ( 'NONE',  ( 17.49174741965450153, -52.84830569448709525, -76.12661215459480957 ) ) ;
#12165 = CARTESIAN_POINT ( 'NONE',  ( 20.53650276133967267, 10.53025766472739555, -34.79644660940672907 ) ) ;
#12166 = CARTESIAN_POINT ( 'NONE',  ( 55.99539635179259989, -50.96576843986699856, -53.34422020842900025 ) ) ;
#12167 = VERTEX_POINT ( 'NONE', #32479 ) ;
#12168 = LINE ( 'NONE', #24179, #44298 ) ;
#12169 = DIRECTION ( 'NONE',  ( 0.000000000000000000, 1.000000000000000000, 0.000000000000000000 ) ) ;
#12170 = CARTESIAN_POINT ( 'NONE',  ( 12.11738391771149992, -9.045897184923541445, -81.23899999999999011 ) ) ;
#12171 = ORIENTED_EDGE ( 'NONE', *, *, #34954, .F. ) ;
#12172 = CARTESIAN_POINT ( 'NONE',  ( 17.36026107283840147, 21.75858530671060009, -76.14999999999999147 ) ) ;
#12173 = ADVANCED_FACE ( 'NONE', ( #8164 ), #4738, .T. ) ;
#12174 = ORIENTED_EDGE ( 'NONE', *, *, #37604, .T. ) ;
#12175 = EDGE_LOOP ( 'NONE', ( #43925, #46023 ) ) ;
#12176 = CARTESIAN_POINT ( 'NONE',  ( 61.62035637548115119, -45.25224449890009737, -47.09707516299204144 ) ) ;
#12177 = CARTESIAN_POINT ( 'NONE',  ( 22.01014902171679921, -19.63241407121610038, -81.23899999999999011 ) ) ;
#12178 = EDGE_CURVE ( 'NONE', #19324, #11300, #40972, .T. ) ;
#12179 = CARTESIAN_POINT ( 'NONE',  ( 8.222961468781386785, -14.58046525346367517, -72.83399817539567778 ) ) ;
#12180 = ORIENTED_EDGE ( 'NONE', *, *, #34150, .T. ) ;
#12181 = CIRCLE ( 'NONE', #47351, 2.000000000000000000 ) ;
#12182 = CYLINDRICAL_SURFACE ( 'NONE', #22405, 0.9999999999999991118 ) ;
#12183 = ORIENTED_EDGE ( 'NONE', *, *, #47577, .T. ) ;
#12184 = CARTESIAN_POINT ( 'NONE',  ( 11.47625293935331037, -64.64303150479236137, -23.97637485116214506 ) ) ;
#12185 = CARTESIAN_POINT ( 'NONE',  ( 18.13393739769630741, 3.536827986686112091, -43.67210485517633600 ) ) ;
#12186 = VERTEX_POINT ( 'NONE', #35287 ) ;
#12187 = ORIENTED_EDGE ( 'NONE', *, *, #22888, .F. ) ;
#12188 = CARTESIAN_POINT ( 'NONE',  ( 60.83133136721959744, 14.23629320661039976, -47.01992809069390233 ) ) ;
#12189 = FACE_OUTER_BOUND ( 'NONE', #42672, .T. ) ;
#12190 = CARTESIAN_POINT ( 'NONE',  ( 61.05085642621550335, 14.40809333551259996, -47.70073481199239751 ) ) ;
#12191 = EDGE_CURVE ( 'NONE', #40924, #16548, #20288, .T. ) ;
#12192 = CARTESIAN_POINT ( 'NONE',  ( 16.13393739769620083, -15.61618894467929941, -28.45282021618999835 ) ) ;
#12193 = CARTESIAN_POINT ( 'NONE',  ( 41.30229995814859478, -44.08664243540900429, -3.681965999269640299 ) ) ;
#12194 = CARTESIAN_POINT ( 'NONE',  ( -8.896400163295020036, 12.99350780695079877, -5.517956762993129871 ) ) ;
#12195 = CARTESIAN_POINT ( 'NONE',  ( 16.13393739769620083, -15.61618894467929941, -32.14999999999999858 ) ) ;
#12196 = CARTESIAN_POINT ( 'NONE',  ( 57.82760759097259751, 14.44856554515060054, -26.31132835932049829 ) ) ;
#12197 = CARTESIAN_POINT ( 'NONE',  ( 23.50277980578040271, -18.31561661513139683, -61.39927945301550238 ) ) ;
#12198 = ORIENTED_EDGE ( 'NONE', *, *, #34412, .T. ) ;
#12199 = AXIS2_PLACEMENT_3D ( 'NONE', #7131, #19167, #35407 ) ;
#12200 = CARTESIAN_POINT ( 'NONE',  ( 54.33950582513909922, 17.73388049035199998, -48.90971789431980454 ) ) ;
#12201 = CARTESIAN_POINT ( 'NONE',  ( 41.98716862695110308, 14.55766279460999968, -6.812372419885229569 ) ) ;
#12202 = LINE ( 'NONE', #27911, #2765 ) ;
#12203 = UNCERTAINTY_MEASURE_WITH_UNIT (LENGTH_MEASURE( 1.000000000000000082E-05 ), #16920, 'distance_accuracy_value', 'NONE');
#12204 = ADVANCED_BREP_SHAPE_REPRESENTATION ( '', ( #43885, #20940 ), #20155 ) ;
#12205 = CARTESIAN_POINT ( 'NONE',  ( 72.41971899104120780, 1.437400661353670062, -69.51820902033620087 ) ) ;
#12206 = CARTESIAN_POINT ( 'NONE',  ( 43.38138188210033519, -39.90126897775567016, -69.65496977589833705 ) ) ;
#12207 = DIRECTION ( 'NONE',  ( 0.000000000000000000, 0.000000000000000000, -1.000000000000000000 ) ) ;
#12208 = CARTESIAN_POINT ( 'NONE',  ( -0.2865249686166205234, -27.40594838884661044, -35.01561944896768352 ) ) ;
#12209 = CARTESIAN_POINT ( 'NONE',  ( 48.82583097700369734, -53.98510752664869727, -54.88051616806440336 ) ) ;
#12210 = CARTESIAN_POINT ( 'NONE',  ( -10.87564126230760131, 11.12160698687080185, -6.291562883898949465 ) ) ;
#12211 = CARTESIAN_POINT ( 'NONE',  ( 63.77506981661740326, 1.028299550205570068, -69.77396888106839867 ) ) ;
#12212 = FACE_OUTER_BOUND ( 'NONE', #617, .T. ) ;
#12213 = CARTESIAN_POINT ( 'NONE',  ( 56.56302216566690078, 13.88381105532070059, -15.29297957052069989 ) ) ;
#12214 = VERTEX_POINT ( 'NONE', #49807 ) ;
#12215 = CARTESIAN_POINT ( 'NONE',  ( 12.45840162589710154, -9.135669594468568633, -34.40311785086109353 ) ) ;
#12216 = CARTESIAN_POINT ( 'NONE',  ( 16.13393739769620083, -15.61618894467929941, -54.64999999999999858 ) ) ;
#12217 = EDGE_LOOP ( 'NONE', ( #14045, #32614, #12989, #8548, #30235, #36994 ) ) ;
#12218 = DIRECTION ( 'NONE',  ( -0.5897727341282554825, -0.3900873262218120252, 0.7071067811865473507 ) ) ;
#12219 = CARTESIAN_POINT ( 'NONE',  ( 61.04997942697300317, -45.41016238768720115, -47.26479615961620340 ) ) ;
#12220 = CARTESIAN_POINT ( 'NONE',  ( 23.53669455186048864, 17.69319178430572137, -34.79644561402099612 ) ) ;
#12221 = CARTESIAN_POINT ( 'NONE',  ( 16.13393739769620083, -15.61618894467929941, -54.64999999999999858 ) ) ;
#12223 = CARTESIAN_POINT ( 'NONE',  ( 23.83903818915907991, -13.54551600724768967, -35.70899566211102183 ) ) ;
#12222 = CARTESIAN_POINT ( 'NONE',  ( 41.85930995561587764, 8.516901924237213706, -77.01048204870357949 ) ) ;
#12224 = DIRECTION ( 'NONE',  ( 1.000000000000000000, 0.000000000000000000, 0.000000000000000000 ) ) ;
#12225 = CARTESIAN_POINT ( 'NONE',  ( 22.46010325183906176, -20.47786603196966837, -51.71599950768847265 ) ) ;
#12226 = ORIENTED_EDGE ( 'NONE', *, *, #18193, .T. ) ;
#12227 = CARTESIAN_POINT ( 'NONE',  ( 83.69028489729539899, -45.07031961188679503, -47.49660994411200221 ) ) ;
#12228 = ORIENTED_EDGE ( 'NONE', *, *, #12029, .T. ) ;
#12229 = EDGE_CURVE ( 'NONE', #21630, #38460, #14859, .T. ) ;
#12230 = ORIENTED_EDGE ( 'NONE', *, *, #22464, .T. ) ;
#12231 = ORIENTED_EDGE ( 'NONE', *, *, #29835, .T. ) ;
#12232 = CARTESIAN_POINT ( 'NONE',  ( 53.05496371557740076, -49.60060548025979443, -49.11011777256759814 ) ) ;
#12233 = CARTESIAN_POINT ( 'NONE',  ( 53.31390740451600152, -50.46142145313445582, -77.17777227673258267 ) ) ;
#12234 = CARTESIAN_POINT ( 'NONE',  ( 76.39343546571723209, -13.87943195375858529, -12.76821643264017325 ) ) ;
#12235 = CARTESIAN_POINT ( 'NONE',  ( 53.79565702846219466, -51.91342281481009735, -54.22862211494859963 ) ) ;
#12236 = AXIS2_PLACEMENT_3D ( 'NONE', #26675, #21710, #17797 ) ;
#12237 = ORIENTED_EDGE ( 'NONE', *, *, #45414, .F. ) ;
#12238 = ORIENTED_EDGE ( 'NONE', *, *, #20022, .F. ) ;
#12239 = CARTESIAN_POINT ( 'NONE',  ( 48.36908225894410407, 22.86152331119799896, -54.63163985339289752 ) ) ;
#12240 = CARTESIAN_POINT ( 'NONE',  ( 57.02670666273519373, -45.17403284636800009, -25.30271567922349973 ) ) ;
#12241 = CARTESIAN_POINT ( 'NONE',  ( 56.43116296087830364, -50.73498357634339584, -53.39631301164680366 ) ) ;
#12242 = CARTESIAN_POINT ( 'NONE',  ( 17.01980371681801074, -8.849198666827120974, -35.99448539802248348 ) ) ;
#12243 = CARTESIAN_POINT ( 'NONE',  ( 65.07836497255370034, 0.9425083649366529093, -17.72664388599960006 ) ) ;
#12244 = DIRECTION ( 'NONE',  ( 0.000000000000000000, 1.000000000000000000, 0.000000000000000000 ) ) ;
#12245 = ADVANCED_FACE ( 'NONE', ( #26904 ), #50767, .T. ) ;
#12246 = VERTEX_POINT ( 'NONE', #19305 ) ;
#12247 = B_SPLINE_CURVE_WITH_KNOTS ( 'NONE', 3,
 ( #39735, #38974, #3583, #35281, #27668, #47356, #3066, #27410, #7514, #43413, #23460, #43670, #3839, #19553, #35545, #28691, #16395, #28173 ),
 .UNSPECIFIED., .F., .F.,
 ( 4, 2, 2, 2, 2, 2, 2, 2, 4 ),
 ( 0.5000014860460771926, 0.5625013002903175297, 0.6250011145345578667, 0.6875009287787983148, 0.7500007430230386518, 0.8125005572672789889, 0.8750003715115193259, 0.9375001857557596630, 1.000000000000000000 ),
 .UNSPECIFIED. ) ;
#12248 = DIRECTION ( 'NONE',  ( 0.000000000000000000, 0.000000000000000000, 1.000000000000000000 ) ) ;
#12249 = CARTESIAN_POINT ( 'NONE',  ( 52.63065799377530141, -50.23288335026530405, -76.99620445994730744 ) ) ;
#12250 = CARTESIAN_POINT ( 'NONE',  ( 64.84324960441189489, 0.8888742037077579372, -70.66714310028379487 ) ) ;
#12251 = DIRECTION ( 'NONE',  ( -1.000000000000000000, 0.000000000000000000, 0.000000000000000000 ) ) ;
#12252 = VECTOR ( 'NONE', #37156, 1000.000000000000000 ) ;
#12253 = CARTESIAN_POINT ( 'NONE',  ( 16.79442214605479933, -23.43606793918860021, -58.48567289420149962 ) ) ;
#12254 = ADVANCED_FACE ( 'NONE', ( #45612 ), #25959, .T. ) ;
#12255 = CIRCLE ( 'NONE', #526, 10.00000000000000888 ) ;
#12256 = CARTESIAN_POINT ( 'NONE',  ( 12.82092494627180201, -50.09900319257889834, -21.11499762262549851 ) ) ;
#12257 = ADVANCED_FACE ( 'NONE', ( #34708 ), #50708, .T. ) ;
#12258 = CARTESIAN_POINT ( 'NONE',  ( 16.13393739769620083, -15.61618894467929941, -82.15000000000000568 ) ) ;
#12259 = CARTESIAN_POINT ( 'NONE',  ( 68.13393739769745139, -49.21324915460503036, -70.54648330188275906 ) ) ;
#12260 = CARTESIAN_POINT ( 'NONE',  ( 61.36964513858340098, -45.41361601159059092, -47.42035206001249747 ) ) ;
#12261 = DIRECTION ( 'NONE',  ( -1.000000000000000000, 0.000000000000000000, 0.000000000000000000 ) ) ;
#12262 = CARTESIAN_POINT ( 'NONE',  ( 23.15239633160939903, -16.31174150734070238, -52.87862267922439230 ) ) ;
#12263 = CARTESIAN_POINT ( 'NONE',  ( 8.784728771152170879, 23.70287936274029761, -46.67204636145419983 ) ) ;
#12264 = ORIENTED_EDGE ( 'NONE', *, *, #31014, .F. ) ;
#12265 = CARTESIAN_POINT ( 'NONE',  ( 13.50743972583810049, -51.62277378238770353, -74.57010117179498820 ) ) ;
#12266 = CARTESIAN_POINT ( 'NONE',  ( 47.31834723158630140, -54.70509784558640121, -54.64514906959579577 ) ) ;
#12267 = DIRECTION ( 'NONE',  ( 0.000000000000000000, 0.000000000000000000, 1.000000000000000000 ) ) ;
#12268 = CARTESIAN_POINT ( 'NONE',  ( 0.3209249304026240424, 19.48649808507980197, -34.64999999999999858 ) ) ;
#12269 = CARTESIAN_POINT ( 'NONE',  ( 68.13393739769620083, 1.883811055320649963, -65.65000000000000568 ) ) ;
#12270 = LINE ( 'NONE', #718, #21458 ) ;
#12271 = CIRCLE ( 'NONE', #19787, 4.000000000000050626 ) ;
#12272 = CARTESIAN_POINT ( 'NONE',  ( 15.24805376294812476, -8.849199263491749790, -75.91113090210829739 ) ) ;
#12273 = LINE ( 'NONE', #23521, #25000 ) ;
#12275 = CARTESIAN_POINT ( 'NONE',  ( 13.61938558678000000, -51.42721352342299923, -23.15000000000000213 ) ) ;
#12274 = CARTESIAN_POINT ( 'NONE',  ( 60.98011298598618168, 14.15834234790303370, -46.91885902330013636 ) ) ;
#12276 = CARTESIAN_POINT ( 'NONE',  ( 19.40270147970599979, -49.11618894467930829, -34.64999999999999858 ) ) ;
#12277 = DIRECTION ( 'NONE',  ( 0.000000000000000000, 0.000000000000000000, -1.000000000000000000 ) ) ;
#12278 = CARTESIAN_POINT ( 'NONE',  ( 48.51124500827120301, 22.78135976125399864, -54.58137771766570268 ) ) ;
#12279 = VERTEX_POINT ( 'NONE', #42070 ) ;
#12280 = CARTESIAN_POINT ( 'NONE',  ( 52.71531615687540295, -49.74189531715239809, -48.72996495230640335 ) ) ;
#12281 = VERTEX_POINT ( 'NONE', #18986 ) ;
#12282 = CARTESIAN_POINT ( 'NONE',  ( 41.41169172635818541, 6.152627909148373320, -83.24405656875323700 ) ) ;
#12283 = AXIS2_PLACEMENT_3D ( 'NONE', #3656, #11522, #11783 ) ;
#12284 = FACE_OUTER_BOUND ( 'NONE', #1798, .T. ) ;
#12285 = CARTESIAN_POINT ( 'NONE',  ( 41.03393739769614967, -15.61618894467929586, 4.449999999999957545 ) ) ;
#12287 = CARTESIAN_POINT ( 'NONE',  ( 55.70021556852680078, 15.31776400109049874, -26.09178003392089806 ) ) ;
#12286 = CARTESIAN_POINT ( 'NONE',  ( 83.10006388208910266, 13.66738427442989767, -46.45756164887520612 ) ) ;
#12288 = CARTESIAN_POINT ( 'NONE',  ( 18.84454860543339905, -22.12734441641509875, -60.82725304503019714 ) ) ;
#12289 = CARTESIAN_POINT ( 'NONE',  ( 53.55182622754160349, 18.18654131614419711, -49.22385694762949981 ) ) ;
#12290 = CARTESIAN_POINT ( 'NONE',  ( 55.53797971117669618, -45.20374984908950466, -15.09128669035350079 ) ) ;
#12291 = CARTESIAN_POINT ( 'NONE',  ( 41.64265090550289727, 15.19461330350370076, -4.296538310234210734 ) ) ;
#12292 = AXIS2_PLACEMENT_3D ( 'NONE', #30422, #46448, #38052 ) ;
#12293 = ORIENTED_EDGE ( 'NONE', *, *, #10147, .T. ) ;
#12294 = EDGE_CURVE ( 'NONE', #13585, #35594, #9181, .T. ) ;
#12295 = CARTESIAN_POINT ( 'NONE',  ( 21.37864584282510094, -9.778399850443678432, -43.02048744625579246 ) ) ;
#12296 = VERTEX_POINT ( 'NONE', #50964 ) ;
#12297 = CARTESIAN_POINT ( 'NONE',  ( 11.51051965274460009, -65.34949819799740567, -17.72953754264250037 ) ) ;
#12298 = CARTESIAN_POINT ( 'NONE',  ( 11.31462425921800019, 33.80730954441699510, -46.86167435056430719 ) ) ;
#12299 = CARTESIAN_POINT ( 'NONE',  ( 18.35639339474798959, 19.96346599773298536, -15.69083011943929407 ) ) ;
#12300 = CARTESIAN_POINT ( 'NONE',  ( 47.65699260619980038, -54.43196373011130618, -54.14466233815100082 ) ) ;
#12301 = CARTESIAN_POINT ( 'NONE',  ( 8.786667189176620596, 31.89283771814190160, -46.67161560189330061 ) ) ;
#12302 = LINE ( 'NONE', #48722, #23291 ) ;
#12303 = VERTEX_POINT ( 'NONE', #26325 ) ;
#12304 = DIRECTION ( 'NONE',  ( 0.000000000000000000, 0.000000000000000000, -1.000000000000000000 ) ) ;
#12305 = CARTESIAN_POINT ( 'NONE',  ( 11.10533145046600012, -63.13707322673510447, -44.25027853318809434 ) ) ;
#12306 = ADVANCED_BREP_SHAPE_REPRESENTATION ( '', ( #44299, #20940 ), #5952 ) ;
#12307 = CYLINDRICAL_SURFACE ( 'NONE', #39453, 0.4999999999999980571 ) ;
#12308 = ORIENTED_EDGE ( 'NONE', *, *, #48865, .F. ) ;
#12309 = CARTESIAN_POINT ( 'NONE',  ( 71.38118348160060123, 1.400446703426730055, -70.22110957219430816 ) ) ;
#12310 = CARTESIAN_POINT ( 'NONE',  ( 50.98563555873659681, -50.83528032372250038, -76.14999999999999147 ) ) ;
#12311 = ORIENTED_EDGE ( 'NONE', *, *, #43714, .T. ) ;
#12312 = CARTESIAN_POINT ( 'NONE',  ( 8.428818883866691536, -17.68680130685687857, -62.70899791641065946 ) ) ;
#12313 = PLANE ( 'NONE',  #43478 ) ;
#12314 = DIRECTION ( 'NONE',  ( 0.6888026391158391659, 0.7071067811865435759, 0.1598465650148942763 ) ) ;
#12315 = DIRECTION ( 'NONE',  ( 0.000000000000000000, 0.000000000000000000, -1.000000000000000000 ) ) ;
#12316 = CARTESIAN_POINT ( 'NONE',  ( 7.893032080596238842, -15.88114103568579871, -70.78210109960230056 ) ) ;
#12317 = CARTESIAN_POINT ( 'NONE',  ( 9.367445776641041277, -14.63655315608641239, -37.89327440229485688 ) ) ;
#12318 = CARTESIAN_POINT ( 'NONE',  ( 55.20045915843670059, 19.79101985246630235, -75.15517561605419417 ) ) ;
#12319 = APPLICATION_PROTOCOL_DEFINITION ( 'draft international standard', 'automotive_design', 1998, #7708 ) ;
#12320 = ADVANCED_FACE ( 'NONE', ( #2238 ), #18214, .T. ) ;
#12321 = ORIENTED_EDGE ( 'NONE', *, *, #49044, .F. ) ;
#12322 = CARTESIAN_POINT ( 'NONE',  ( 11.92096193908029989, -21.76090468995549898, -60.92396586663380020 ) ) ;
#12323 = VECTOR ( 'NONE', #4943, 999.9999999999998863 ) ;
#12324 = DIRECTION ( 'NONE',  ( 0.000000000000000000, 0.000000000000000000, 1.000000000000000000 ) ) ;
#12325 = CARTESIAN_POINT ( 'NONE',  ( 12.36961003038774365, 34.13847818779984777, -23.58850009407127502 ) ) ;
#12326 = CARTESIAN_POINT ( 'NONE',  ( 47.29375078065829996, 23.46074027222400105, -74.50151902752439526 ) ) ;
#12327 = CARTESIAN_POINT ( 'NONE',  ( 71.07527734533519492, 1.384447124000270035, -60.97624892474630087 ) ) ;
#12328 = CARTESIAN_POINT ( 'NONE',  ( 56.46551779669420057, -50.77616595281960343, -53.85225392423020452 ) ) ;
#12329 = DIRECTION ( 'NONE',  ( 0.000000000000000000, 0.7071067811865492381, 0.7071067811865457964 ) ) ;
#12330 = CARTESIAN_POINT ( 'NONE',  ( 22.42849628649389615, -10.29066088593869921, -71.28415194542799327 ) ) ;
#12331 = CARTESIAN_POINT ( 'NONE',  ( 56.95004443788039339, -50.62929017573570434, -74.61329603206479533 ) ) ;
#12333 = CARTESIAN_POINT ( 'NONE',  ( 29.92723726607434998, -35.62120283203830695, -84.60891090650764568 ) ) ;
#12332 = DIRECTION ( 'NONE',  ( 0.000000000000000000, 1.000000000000000000, 0.000000000000000000 ) ) ;
#12334 = CARTESIAN_POINT ( 'NONE',  ( 63.00666467042349694, 0.9212109678634080590, -68.76625967790960203 ) ) ;
#12335 = CARTESIAN_POINT ( 'NONE',  ( 61.29873811675859940, 13.99300715493670033, -46.60505303728890425 ) ) ;
#12336 = CARTESIAN_POINT ( 'NONE',  ( -32.24202920327260102, -25.12181407414389867, -55.86711240520629929 ) ) ;
#12337 = EDGE_LOOP ( 'NONE', ( #21183, #5575, #43546, #35895 ) ) ;
#12338 =( BOUNDED_CURVE ( )  B_SPLINE_CURVE ( 2, ( #18625, #11292, #39838 ),
 .UNSPECIFIED., .F., .T. ) 
 B_SPLINE_CURVE_WITH_KNOTS ( ( 3, 3 ),
 ( 1.104980434577240045, 2.168627590050209886 ),
 .UNSPECIFIED. ) 
 CURVE ( )  GEOMETRIC_REPRESENTATION_ITEM ( )  RATIONAL_B_SPLINE_CURVE ( ( 1.323085463760209857, 1.425426480542949959, 1.425426480542939967 ) ) 
 REPRESENTATION_ITEM ( '' )  );
#12339 = CARTESIAN_POINT ( 'NONE',  ( 53.05172806475840019, -49.54462323568909454, -48.80720635931050566 ) ) ;
#12340 = CARTESIAN_POINT ( 'NONE',  ( 61.48973982512229952, -45.14485638884580254, -27.91396448414770148 ) ) ;
#12341 = CYLINDRICAL_SURFACE ( 'NONE', #26860, 13.50000000000000178 ) ;
#12342 = CARTESIAN_POINT ( 'NONE',  ( 57.23047368777599786, 14.59927084644489881, -26.25848675732999737 ) ) ;
#12343 = CARTESIAN_POINT ( 'NONE',  ( 15.31418126070190056, -23.02123409518320329, -76.76775207935769174 ) ) ;
#12344 = CARTESIAN_POINT ( 'NONE',  ( 50.88311850049529284, 17.84955123746129857, -76.31540042328140316 ) ) ;
#12345 = CARTESIAN_POINT ( 'NONE',  ( 52.85389958694200629, 18.41787986729509896, -48.74486367440029966 ) ) ;
#12346 = CARTESIAN_POINT ( 'NONE',  ( 71.15549028777350316, 1.383161449028130097, -70.33386915736630840 ) ) ;
#12347 = CARTESIAN_POINT ( 'NONE',  ( -0.4410626023037830246, -8.356009309619699010, -35.14999999999999858 ) ) ;
#12348 = ORIENTED_EDGE ( 'NONE', *, *, #10133, .F. ) ;
#12349 = EDGE_CURVE ( 'NONE', #33931, #34264, #15063, .T. ) ;
#12350 = DIRECTION ( 'NONE',  ( -0.4999999999999985567, 0.8660254037844394848, 0.000000000000000000 ) ) ;
#12351 = CARTESIAN_POINT ( 'NONE',  ( 47.71647669724200114, -54.49282706777620433, -54.97429864921259934 ) ) ;
#12352 = DIRECTION ( 'NONE',  ( 1.000000000000000000, 0.000000000000000000, 0.000000000000000000 ) ) ;
#12353 = CARTESIAN_POINT ( 'NONE',  ( 11.73137203405252826, -41.76263555408610273, -34.79644660940672196 ) ) ;
#12354 = CARTESIAN_POINT ( 'NONE',  ( 58.65609766748040244, 17.55276584502570003, -51.15249613422370345 ) ) ;
#12356 = ADVANCED_FACE ( 'NONE', ( #43114 ), #7205, .T. ) ;
#12355 = CARTESIAN_POINT ( 'NONE',  ( 71.29701819511369365, 1.369719003397489976, -60.94773069968270107 ) ) ;
#12357 = FACE_OUTER_BOUND ( 'NONE', #15484, .T. ) ;
#12358 = CARTESIAN_POINT ( 'NONE',  ( 71.47028093172080787, 1.369286338573760142, -61.00325184746190388 ) ) ;
#12359 = CIRCLE ( 'NONE', #35779, 17.09468304687040785 ) ;
#12360 = CARTESIAN_POINT ( 'NONE',  ( 23.98146851043909678, -16.64924265148496829, -71.54932861355067075 ) ) ;
#12361 = EDGE_CURVE ( 'NONE', #11933, #43415, #29252, .T. ) ;
#12362 = CARTESIAN_POINT ( 'NONE',  ( 65.19259745005730622, 1.384447124000270035, -70.32375107525380997 ) ) ;
#12363 = ORIENTED_EDGE ( 'NONE', *, *, #34990, .F. ) ;
#12364 = VERTEX_POINT ( 'NONE', #26849 ) ;
#12365 = CIRCLE ( 'NONE', #17416, 1.416095994175718964 ) ;
#12366 = CARTESIAN_POINT ( 'NONE',  ( 49.85987176298878865, -29.64260838442978141, -15.88869185456543143 ) ) ;
#12367 = VERTEX_POINT ( 'NONE', #49940 ) ;
#12368 = CARTESIAN_POINT ( 'NONE',  ( 11.23030410197340068, -64.15300103173049706, -44.07781775651169909 ) ) ;
#12369 = CARTESIAN_POINT ( 'NONE',  ( 12.95205818299439926, -65.51487522592771029, -47.64438484965779708 ) ) ;
#12370 = CARTESIAN_POINT ( 'NONE',  ( 47.13393739769619373, 4.883811055320659733, -54.64999999999999858 ) ) ;
#12371 = ORIENTED_EDGE ( 'NONE', *, *, #18096, .F. ) ;
#12372 = CARTESIAN_POINT ( 'NONE',  ( 16.65420337941489848, 17.88381105532299742, -20.15000000000000213 ) ) ;
#12373 = CARTESIAN_POINT ( 'NONE',  ( 10.70456637417987622, -11.48191128173198905, -71.65978603205104491 ) ) ;
#12374 = EDGE_CURVE ( 'NONE', #7271, #31635, #21771, .T. ) ;
#12375 = CARTESIAN_POINT ( 'NONE',  ( 68.13393739769620083, 17.38381105532069881, -65.65000000000000568 ) ) ;
#12376 = CARTESIAN_POINT ( 'NONE',  ( 15.34132565853509966, -23.82316687122930077, -44.32297812435340489 ) ) ;
#12377 = CARTESIAN_POINT ( 'NONE',  ( 45.14919548887390022, 2.061487825409429764, -35.12503119152809461 ) ) ;
#12378 = CARTESIAN_POINT ( 'NONE',  ( 42.88323645452967270, -37.76021733457542240, -75.90348433167388009 ) ) ;
#12379 = CARTESIAN_POINT ( 'NONE',  ( 0.000000000000000000, 0.000000000000000000, 0.000000000000000000 ) ) ;
#12380 = EDGE_CURVE ( 'NONE', #31547, #1664, #28463, .T. ) ;
#12381 = ORIENTED_EDGE ( 'NONE', *, *, #19984, .T. ) ;
#12382 = CARTESIAN_POINT ( 'NONE',  ( 11.24784815691280038, -64.69222497390319404, -23.70517260836590268 ) ) ;
#12383 = CARTESIAN_POINT ( 'NONE',  ( 18.64389600481149856, -22.63094492865949903, -34.62328075351209122 ) ) ;
#12384 = CARTESIAN_POINT ( 'NONE',  ( 40.79813495724229711, 13.98026726342900083, -5.648533830653249765 ) ) ;
#12385 = CARTESIAN_POINT ( 'NONE',  ( 14.76083081978829981, 21.63336578114690312, -76.12563501418100032 ) ) ;
#12386 = DIRECTION ( 'NONE',  ( -0.1961161351384590468, 0.000000000000000000, -0.9805806756908651556 ) ) ;
#12387 = CARTESIAN_POINT ( 'NONE',  ( 83.53665286397169609, -44.61316599402150018, -46.51476939800770083 ) ) ;
#12388 = AXIS2_PLACEMENT_3D ( 'NONE', #2771, #31297, #31047 ) ;
#12389 = DIRECTION ( 'NONE',  ( 1.000000000000000000, 0.000000000000000000, 0.000000000000000000 ) ) ;
#12390 = EDGE_CURVE ( 'NONE', #35377, #10891, #1693, .T. ) ;
#12391 = CARTESIAN_POINT ( 'NONE',  ( 18.02280865088329875, -23.64207743741700085, -45.93409400506969575 ) ) ;
#12392 = ORIENTED_EDGE ( 'NONE', *, *, #1568, .T. ) ;
#12393 = B_SPLINE_CURVE_WITH_KNOTS ( 'NONE', 3,
 ( #30651, #9724, #26720, #17587, #21753, #6567, #33810, #26203, #14682, #46676, #42738, #2115, #6836, #14425, #37500, #26462, #25939, #37765, #42476, #1599, #13660, #6053, #38021, #2641, #33559, #49576, #25684, #14167 ),
 .UNSPECIFIED., .F., .F.,
 ( 4, 2, 2, 2, 2, 2, 2, 2, 2, 2, 2, 2, 2, 4 ),
 ( 0.5000053122294032537, 0.5625046482007277637, 0.6250039841720522737, 0.6875033201433767838, 0.7187529881290390943, 0.7500026561147015158, 0.7812523241003637153, 0.8125019920860261369, 0.8437516600716883364, 0.8750013280573507579, 0.9062509960430130684, 0.9375006640286753790, 0.9687503320143376895, 1.000000000000000000 ),
 .UNSPECIFIED. ) ;
#12394 = CARTESIAN_POINT ( 'NONE',  ( 52.83348354832899929, -49.61280751446100368, -27.68241839973370233 ) ) ;
#12395 = CARTESIAN_POINT ( 'NONE',  ( 15.79694611016350336, -50.96353045011390037, -20.52360778208860026 ) ) ;
#12396 = DIRECTION ( 'NONE',  ( 1.000000000000000000, 0.000000000000000000, 0.000000000000000000 ) ) ;
#12397 = CARTESIAN_POINT ( 'NONE',  ( 22.88773899167640025, -14.38585658271974133, -56.78929433555941841 ) ) ;
#12398 = DIRECTION ( 'NONE',  ( -0.2389682100435167045, 0.9710273912658683448, 0.000000000000000000 ) ) ;
#12399 = ORIENTED_EDGE ( 'NONE', *, *, #34409, .F. ) ;
#12400 = CARTESIAN_POINT ( 'NONE',  ( -7.446190786415279206, -45.59035109774320205, -5.628040487542099513 ) ) ;
#12401 = CARTESIAN_POINT ( 'NONE',  ( 47.24267966324089230, 23.52891476845359975, -54.64850595551979495 ) ) ;
#12402 = CARTESIAN_POINT ( 'NONE',  ( 16.63320969315425657, 18.38376875625361251, -83.23984175390957319 ) ) ;
#12403 = CARTESIAN_POINT ( 'NONE',  ( 63.13104210372130609, 0.9254905997697669973, -62.33773042465509917 ) ) ;
#12404 = CARTESIAN_POINT ( 'NONE',  ( 68.13393739769618662, -28.80002732851770020, -102.2016796975542690 ) ) ;
#12405 = CARTESIAN_POINT ( 'NONE',  ( 41.18706483287339637, 13.38317691818800093, -5.042666801615239613 ) ) ;
#12406 = CARTESIAN_POINT ( 'NONE',  ( 10.72261433029855127, -19.77485540986135604, -53.24448634458038754 ) ) ;
#12407 = CARTESIAN_POINT ( 'NONE',  ( 9.543105166377426229, -17.38758548366874024, -65.36948706771786988 ) ) ;
#12408 = CARTESIAN_POINT ( 'NONE',  ( 71.75685251123249486, 1.434949534324269971, -61.23975123050709612 ) ) ;
#12409 = B_SPLINE_CURVE_WITH_KNOTS ( 'NONE', 3,
 ( #17339, #13414, #16547, #41432, #48525, #44591, #20991, #8696, #24648 ),
 .UNSPECIFIED., .F., .F.,
 ( 4, 2, 1, 2, 4 ),
 ( 0.000000000000000000, 0.2496952128132839399, 0.3745428192199221629, 0.4369666224232462426, 0.4993904256265703223 ),
 .UNSPECIFIED. ) ;
#12410 = CARTESIAN_POINT ( 'NONE',  ( 56.37863599685000082, -47.94388181700620066, -48.46423989679689726 ) ) ;
#12411 = CARTESIAN_POINT ( 'NONE',  ( -0.2826210738582647375, -20.36873564196809738, -35.01222475787349708 ) ) ;
#12412 = CARTESIAN_POINT ( 'NONE',  ( 64.91481325068460251, 1.325839985408290067, -60.87288092506760506 ) ) ;
#12413 = CARTESIAN_POINT ( 'NONE',  ( 17.29410413645300437, -52.94069807145589834, -76.14999999999999147 ) ) ;
#12414 = ADVANCED_FACE ( 'NONE', ( #46012 ), #10103, .T. ) ;
#12415 = CARTESIAN_POINT ( 'NONE',  ( 15.24810681485378616, -22.38318503380609314, -60.99450452302099279 ) ) ;
#12416 = CARTESIAN_POINT ( 'NONE',  ( 68.13393739769620083, -43.11618894467930119, -73.60861006572370968 ) ) ;
#12417 = ORIENTED_EDGE ( 'NONE', *, *, #26721, .T. ) ;
#12418 = DIRECTION ( 'NONE',  ( 0.000000000000000000, 0.000000000000000000, -1.000000000000000000 ) ) ;
#12419 = CARTESIAN_POINT ( 'NONE',  ( 10.14396384489010039, 32.02340138881569231, -45.99320603557470122 ) ) ;
#12420 = DIRECTION ( 'NONE',  ( 1.000000000000000000, 0.000000000000000000, -1.224646799147353207E-16 ) ) ;
#12421 = CARTESIAN_POINT ( 'NONE',  ( 8.981108893502280921, -14.73393040951099842, -81.23899999999999011 ) ) ;
#12422 = EDGE_CURVE ( 'NONE', #30160, #47211, #18475, .T. ) ;
#12423 = ORIENTED_EDGE ( 'NONE', *, *, #47030, .T. ) ;
#12424 = CARTESIAN_POINT ( 'NONE',  ( 17.74772103310080240, 20.37930389448669644, -75.46937177410659103 ) ) ;
#12425 = EDGE_LOOP ( 'NONE', ( #27751, #35187, #25662, #15681 ) ) ;
#12426 = ORIENTED_EDGE ( 'NONE', *, *, #47696, .F. ) ;
#12427 = ORIENTED_EDGE ( 'NONE', *, *, #7933, .F. ) ;
#12428 = DIRECTION ( 'NONE',  ( 0.000000000000000000, 0.000000000000000000, 1.000000000000000000 ) ) ;
#12429 = DIRECTION ( 'NONE',  ( 0.5685928097855378338, 0.5944782866685498490, -0.5685928097855378338 ) ) ;
#12430 = CARTESIAN_POINT ( 'NONE',  ( 20.99565867520791329, -9.290058221069106281, -73.50066484993433846 ) ) ;
#12431 = ORIENTED_EDGE ( 'NONE', *, *, #4320, .T. ) ;
#12432 = VECTOR ( 'NONE', #50538, 1000.000000000000000 ) ;
#12433 = CARTESIAN_POINT ( 'NONE',  ( 51.13393739769659874, -50.61618894467899565, 10.84999999999999964 ) ) ;
#12434 = DIRECTION ( 'NONE',  ( 0.000000000000000000, 0.000000000000000000, 1.000000000000000000 ) ) ;
#12435 = ORIENTED_EDGE ( 'NONE', *, *, #14312, .F. ) ;
#12436 = CARTESIAN_POINT ( 'NONE',  ( 48.91612303624370384, -46.17268314339860069, -11.68043221219750016 ) ) ;
#12437 = CIRCLE ( 'NONE', #24978, 12.00000000000000000 ) ;
#12438 = CARTESIAN_POINT ( 'NONE',  ( 57.82770531258893243, -45.74095387556897663, -26.33626789187744421 ) ) ;
#12439 = EDGE_LOOP ( 'NONE', ( #7069, #6292, #41160, #47672, #43480, #37001 ) ) ;
#12440 = ORIENTED_EDGE ( 'NONE', *, *, #48631, .F. ) ;
#12441 = DIRECTION ( 'NONE',  ( 0.000000000000000000, 0.000000000000000000, 1.000000000000000000 ) ) ;
#12442 = LINE ( 'NONE', #12714, #40149 ) ;
#12443 = CARTESIAN_POINT ( 'NONE',  ( 60.81154475074989563, 14.44468362946420115, -47.68343931016890025 ) ) ;
#12444 = CARTESIAN_POINT ( 'NONE',  ( 53.62232554824719699, 14.37784769650350114, -14.60904475022659987 ) ) ;
#12445 = CARTESIAN_POINT ( 'NONE',  ( 15.09842766289428262, -23.52719350332821335, -68.33399707341648366 ) ) ;
#12446 = CARTESIAN_POINT ( 'NONE',  ( -10.45347530949710091, 11.54094627941979923, -5.983182295287229557 ) ) ;
#12447 = FACE_OUTER_BOUND ( 'NONE', #9623, .T. ) ;
#12448 = CARTESIAN_POINT ( 'NONE',  ( 61.30976794464369561, 13.98564738790680018, -28.10341086548599776 ) ) ;
#12449 = ADVANCED_FACE ( 'NONE', ( #46539, #10627 ), #35230, .T. ) ;
#12450 = CARTESIAN_POINT ( 'NONE',  ( 21.31981268913839855, -21.50630317487819809, -61.55771731514259670 ) ) ;
#12451 = ORIENTED_EDGE ( 'NONE', *, *, #31387, .F. ) ;
#12453 = ADVANCED_FACE ( 'NONE', ( #44391 ), #3272, .F. ) ;
#12452 = CARTESIAN_POINT ( 'NONE',  ( 59.69762033831859327, 14.85484429090200109, -47.57821500189280073 ) ) ;
#12454 = CARTESIAN_POINT ( 'NONE',  ( 40.93884659071979826, 14.21788489420559998, -5.915596512093559411 ) ) ;
#12455 = CARTESIAN_POINT ( 'NONE',  ( 53.99624024582704607, -50.67301592132088217, -76.54980271157616301 ) ) ;
#12456 = CARTESIAN_POINT ( 'NONE',  ( 72.66407988305761023, 1.091560265417719888, -69.57662740730940243 ) ) ;
#12457 = ADVANCED_FACE ( 'NONE', ( #8230 ), #3538, .T. ) ;
#12458 = CARTESIAN_POINT ( 'NONE',  ( 42.98926129872933188, -39.86518172765487122, -71.55095433749755784 ) ) ;
#12459 = AXIS2_PLACEMENT_3D ( 'NONE', #16688, #40794, #37128 ) ;
#12460 = CARTESIAN_POINT ( 'NONE',  ( 11.27227933505587032, -21.94236925040859632, -36.50066404204540049 ) ) ;
#12461 = AXIS2_PLACEMENT_3D ( 'NONE', #7831, #44497, #4656 ) ;
#12462 = CIRCLE ( 'NONE', #747, 5.251829701412240148 ) ;
#12463 = CARTESIAN_POINT ( 'NONE',  ( 46.91120985881580197, 22.91722024179730255, -75.65750144867429583 ) ) ;
#12464 = CARTESIAN_POINT ( 'NONE',  ( 48.72281879484769718, -54.07425847834139887, -55.27155626217439988 ) ) ;
#12465 = DIRECTION ( 'NONE',  ( 0.000000000000000000, 0.000000000000000000, -1.000000000000000000 ) ) ;
#12466 = CARTESIAN_POINT ( 'NONE',  ( 21.46302885113694359, -21.53080627074261955, -33.77437669800720244 ) ) ;
#12467 = CARTESIAN_POINT ( 'NONE',  ( 66.72561048563109409, -33.11618894467930829, -20.64999999980150136 ) ) ;
#12468 = CARTESIAN_POINT ( 'NONE',  ( 8.222373579151801337, -15.61629175287649929, -54.79233150823699816 ) ) ;
#12469 = VERTEX_POINT ( 'NONE', #39690 ) ;
#12470 = CARTESIAN_POINT ( 'NONE',  ( 22.78696485699360252, -18.96938443020880172, -41.21594592233239496 ) ) ;
#12471 = CARTESIAN_POINT ( 'NONE',  ( 13.13393739769619906, -49.61618894467939356, -35.14999999999999858 ) ) ;
#12472 = EDGE_LOOP ( 'NONE', ( #13638, #37318, #29600, #30053 ) ) ;
#12473 = CARTESIAN_POINT ( 'NONE',  ( 17.21347160910339724, 21.88381105532300097, -76.14999999999999147 ) ) ;
#12474 = CARTESIAN_POINT ( 'NONE',  ( 60.66957880285420401, -45.55654657165910493, -47.20039331182919540 ) ) ;
#12475 = CARTESIAN_POINT ( 'NONE',  ( 29.13393739769619728, -33.11618894467940066, -81.65000000000000568 ) ) ;
#12476 = CARTESIAN_POINT ( 'NONE',  ( 69.11290641955770297, -43.39767609583565644, -11.59169279273430497 ) ) ;
#12478 = CARTESIAN_POINT ( 'NONE',  ( 44.66180732667802999, -33.16299454025457294, -44.80531609597240106 ) ) ;
#12477 = CARTESIAN_POINT ( 'NONE',  ( 41.45690265626797810, 8.471601390023884903, -78.95241774151945435 ) ) ;
#12479 = CARTESIAN_POINT ( 'NONE',  ( -31.86606260230380627, -15.61618894467930474, -74.14999999999999147 ) ) ;
#12480 = FACE_OUTER_BOUND ( 'NONE', #16461, .T. ) ;
#12481 = EDGE_CURVE ( 'NONE', #32513, #39247, #50223, .T. ) ;
#12482 = ORIENTED_EDGE ( 'NONE', *, *, #17451, .T. ) ;
#12483 = CARTESIAN_POINT ( 'NONE',  ( 84.28893459517129827, -43.90990963716989626, -47.31525200062240089 ) ) ;
#12484 = VERTEX_POINT ( 'NONE', #27621 ) ;
#12485 = VERTEX_POINT ( 'NONE', #39177 ) ;
#12486 = ORIENTED_EDGE ( 'NONE', *, *, #27241, .T. ) ;
#12487 = CARTESIAN_POINT ( 'NONE',  ( -18.86606260230360022, -50.61618894467959962, 11.34999999999999964 ) ) ;
#12488 = CARTESIAN_POINT ( 'NONE',  ( 52.97651386206310065, -49.63284518666780087, -49.06832845556920120 ) ) ;
#12489 = CARTESIAN_POINT ( 'NONE',  ( 53.07820087960804756, -50.35438023692758236, -77.22362299732516533 ) ) ;
#12490 = CARTESIAN_POINT ( 'NONE',  ( 76.39890160524630858, -19.26235143558729135, -12.79181377051713753 ) ) ;
#12491 = CARTESIAN_POINT ( 'NONE',  ( 51.36789317581919789, -52.94755764699569767, -54.71052196913720422 ) ) ;
#12492 = AXIS2_PLACEMENT_3D ( 'NONE', #45061, #20413, #8386 ) ;
#12493 = EDGE_LOOP ( 'NONE', ( #47258, #17531, #37702, #26706 ) ) ;
#12494 = ORIENTED_EDGE ( 'NONE', *, *, #4010, .T. ) ;
#12495 = CARTESIAN_POINT ( 'NONE',  ( 47.84600491270340683, 23.14802384070760155, -54.72009433156399894 ) ) ;
#12496 = CARTESIAN_POINT ( 'NONE',  ( 57.33512764681800178, -45.12355306711239677, -25.31953145138690431 ) ) ;
#12497 = CARTESIAN_POINT ( 'NONE',  ( 13.99784741310209135, 18.38374537013401522, -83.13257468828133767 ) ) ;
#12498 = CARTESIAN_POINT ( 'NONE',  ( -10.36489612227181745, 11.27711771225501813, -2.281195398064152169 ) ) ;
#12499 = CARTESIAN_POINT ( 'NONE',  ( 23.98146842033044024, -14.58313461376996933, -59.75066739342922517 ) ) ;
#12500 = B_SPLINE_CURVE_WITH_KNOTS ( 'NONE', 3,
 ( #47428, #20128, #31400, #11520, #47678, #12035, #15698, #27481, #11781, #51858, #11259, #47934, #44243, #31912, #27740, #27988, #20379, #7587 ),
 .UNSPECIFIED., .F., .F.,
 ( 4, 2, 2, 2, 2, 2, 2, 2, 4 ),
 ( 0.5000000059040078382, 0.5625000051660068445, 0.6250000044280057399, 0.6875000036900047462, 0.7500000029520037526, 0.8125000022140027589, 0.8750000014760018763, 0.9375000007380009936, 1.000000000000000000 ),
 .UNSPECIFIED. ) ;
#12501 = CARTESIAN_POINT ( 'NONE',  ( 51.90728952832269982, -49.37557461706570194, -77.08409367958790881 ) ) ;
#12502 = AXIS2_PLACEMENT_3D ( 'NONE', #44024, #4441, #40091 ) ;
#12503 = EDGE_LOOP ( 'NONE', ( #44327, #25075, #42512, #24649 ) ) ;
#12504 = CARTESIAN_POINT ( 'NONE',  ( 12.36320305029179956, 33.31445045633500257, -15.76422791923680045 ) ) ;
#12505 = CARTESIAN_POINT ( 'NONE',  ( 52.35198176182720431, -50.04795459678859970, -76.97988188672849219 ) ) ;
#12506 = CARTESIAN_POINT ( 'NONE',  ( 11.17268199994810196, -10.96232122111623575, -33.69277564961296179 ) ) ;
#12507 = AXIS2_PLACEMENT_3D ( 'NONE', #6589, #34609, #34870 ) ;
#12508 = DIRECTION ( 'NONE',  ( 0.000000000000000000, 1.000000000000000000, 0.000000000000000000 ) ) ;
#12509 = AXIS2_PLACEMENT_3D ( 'NONE', #28056, #51165, #35687 ) ;
#12510 = CARTESIAN_POINT ( 'NONE',  ( 8.760241513115010648, -18.30233052570079977, -56.90129427292900033 ) ) ;
#12511 = B_SPLINE_CURVE_WITH_KNOTS ( 'NONE', 3,
 ( #47708, #27772, #43767, #12, #15990, #31942, #45319, #29061, #50022, #33757, #37706, #1803, #26150, #21187, #25628, #9923, #1546, #17784 ),
 .UNSPECIFIED., .F., .F.,
 ( 4, 2, 2, 2, 2, 2, 2, 2, 4 ),
 ( 0.000000000000000000, 0.06249993788804932004, 0.1249998757760986401, 0.1874998136641479740, 0.2499997515521972802, 0.3124996894402465863, 0.3749996273282959480, 0.4374995652163452542, 0.4999995031043945604 ),
 .UNSPECIFIED. ) ;
#12512 = DIRECTION ( 'NONE',  ( 0.000000000000000000, 0.000000000000000000, 1.000000000000000000 ) ) ;
#12513 = AXIS2_PLACEMENT_3D ( 'NONE', #31030, #20263, #3271 ) ;
#12514 = CARTESIAN_POINT ( 'NONE',  ( 41.35617304474619971, -44.65133728268560276, -5.195209045859010111 ) ) ;
#12515 = CARTESIAN_POINT ( 'NONE',  ( 18.34117720853386402, -51.20617678333719880, -15.69346472551720240 ) ) ;
#12516 = CARTESIAN_POINT ( 'NONE',  ( 56.43809645418499343, 13.88381105532070059, -15.14067943257860094 ) ) ;
#12517 = CARTESIAN_POINT ( 'NONE',  ( 4.082512187184037522, -22.57408253408722132, -34.89146800830128825 ) ) ;
#12518 = CARTESIAN_POINT ( 'NONE',  ( 22.90093740060443395, -16.50198292282657775, -38.49448988202613720 ) ) ;
#12519 = CARTESIAN_POINT ( 'NONE',  ( 15.98424424538390198, -22.66744068707240345, -53.35393626560600211 ) ) ;
#12520 = CARTESIAN_POINT ( 'NONE',  ( 24.04493740941656910, -14.58064971957864486, -41.75066428994564660 ) ) ;
#12521 = VERTEX_POINT ( 'NONE', #4044 ) ;
#12523 = EDGE_CURVE ( 'NONE', #14401, #50703, #44081, .T. ) ;
#12522 = CARTESIAN_POINT ( 'NONE',  ( 14.09775367411850056, -52.29987767205390270, -75.77396328158880578 ) ) ;
#12524 = CARTESIAN_POINT ( 'NONE',  ( 47.29427773876249574, -54.72467116367779738, -54.70583352925600451 ) ) ;
#12525 = PLANE ( 'NONE',  #12388 ) ;
#12526 = EDGE_CURVE ( 'NONE', #44367, #24387, #10911, .T. ) ;
#12527 = CARTESIAN_POINT ( 'NONE',  ( 20.29256778889454793, -10.20483762520559168, -38.16115576630075878 ) ) ;
#12528 = DIRECTION ( 'NONE',  ( 0.3569024281753349626, 0.000000000000000000, 0.9341416684649872515 ) ) ;
#12529 = CARTESIAN_POINT ( 'NONE',  ( 60.95893300201414178, -45.44404501095668536, -47.26315862579021143 ) ) ;
#12530 = CARTESIAN_POINT ( 'NONE',  ( 61.75019796695539753, 13.88381105532070059, -28.15000000000000213 ) ) ;
#12531 = CARTESIAN_POINT ( 'NONE',  ( 11.41644049898670055, 34.12404561335850417, -18.17421237887380414 ) ) ;
#12533 = CARTESIAN_POINT ( 'NONE',  ( 12.54923790319493726, -50.40993839913490149, -21.20205464686137020 ) ) ;
#12532 = DIRECTION ( 'NONE',  ( 0.6888026391158329487, -0.7071067811865494601, 0.1598465650148944150 ) ) ;
#12534 = CARTESIAN_POINT ( 'NONE',  ( 24.04492574745081868, -15.60216321284723762, -71.50710845886689526 ) ) ;
#12535 = DIRECTION ( 'NONE',  ( 0.000000000000000000, 0.000000000000000000, 1.000000000000000000 ) ) ;
#12536 = CARTESIAN_POINT ( 'NONE',  ( 48.75009304688830269, 22.82040167798450270, -55.10293387284019673 ) ) ;
#12537 = EDGE_LOOP ( 'NONE', ( #19038, #32818, #3844, #16139, #15072 ) ) ;
#12538 = CARTESIAN_POINT ( 'NONE',  ( 10.20031836582380080, -11.80374558653580053, -66.02896523578509402 ) ) ;
#12539 = VERTEX_POINT ( 'NONE', #20006 ) ;
#12540 = VECTOR ( 'NONE', #4094, 1000.000000000000000 ) ;
#12541 = CARTESIAN_POINT ( 'NONE',  ( 0.1457841021255935343, -15.61618894467929941, -34.68167779225149161 ) ) ;
#12542 = CARTESIAN_POINT ( 'NONE',  ( 65.25681082723269810, 1.383811055320669947, -60.95624653118409242 ) ) ;
#12543 = CARTESIAN_POINT ( 'NONE',  ( -23.31565607136580098, -47.38337005707097660, 11.34999999999999964 ) ) ;
#12545 = CARTESIAN_POINT ( 'NONE',  ( 54.22684962163910427, 16.84931794028459962, -26.38907994676030100 ) ) ;
#12544 = CARTESIAN_POINT ( 'NONE',  ( 83.88693549187640031, 13.20239946185910007, -47.02124945944449763 ) ) ;
#12546 = AXIS2_PLACEMENT_3D ( 'NONE', #4221, #5271, #543 ) ;
#12547 = CARTESIAN_POINT ( 'NONE',  ( 17.08797267472250070, -8.628172388687518790, -63.99601028757499677 ) ) ;
#12548 = CARTESIAN_POINT ( 'NONE',  ( 53.16274087092459411, 18.32513333159890223, -49.15255084583340306 ) ) ;
#12549 = CARTESIAN_POINT ( 'NONE',  ( 55.99720521707869381, -45.19575551719779583, -15.52253582168630075 ) ) ;
#12550 = EDGE_CURVE ( 'NONE', #32837, #21889, #20086, .T. ) ;
#12551 = CARTESIAN_POINT ( 'NONE',  ( 44.11147024075970080, 1.884029797248020000, -54.64999999999999858 ) ) ;
#12552 = ORIENTED_EDGE ( 'NONE', *, *, #31291, .T. ) ;
#12553 = AXIS2_PLACEMENT_3D ( 'NONE', #39566, #23041, #23289 ) ;
#12554 = EDGE_CURVE ( 'NONE', #19827, #14727, #5039, .T. ) ;
#12555 = ORIENTED_EDGE ( 'NONE', *, *, #26347, .F. ) ;
#12556 = CARTESIAN_POINT ( 'NONE',  ( 12.13696592144739839, -65.16745155981689663, -16.64705455763589725 ) ) ;
#12557 = CARTESIAN_POINT ( 'NONE',  ( 10.54842637916130066, 33.25339676159590141, -46.47926574070720562 ) ) ;
#12558 = CARTESIAN_POINT ( 'NONE',  ( 18.66493251958384647, 20.21052494929402243, -15.73461886919979413 ) ) ;
#12559 = CARTESIAN_POINT ( 'NONE',  ( 52.06890086575109677, -50.39494763447100212, -49.13506827049639725 ) ) ;
#12560 = B_SPLINE_CURVE_WITH_KNOTS ( 'NONE', 3,
 ( #2402, #18135, #18386, #9765, #17874, #34097, #34623, #14207, #25716, #29909 ),
 .UNSPECIFIED., .F., .F.,
 ( 4, 2, 2, 2, 4 ),
 ( 0.1205773112035685712, 0.1385876512664389881, 0.1499668177668040114, 0.1614008449072590057, 0.1617349454127599839 ),
 .UNSPECIFIED. ) ;
#12561 = CARTESIAN_POINT ( 'NONE',  ( 11.45862936884678973, -65.29787451153411837, -22.69679117090718279 ) ) ;
#12562 = DIRECTION ( 'NONE',  ( -0.8059588108975358489, 0.1342272854598799692, 0.5765530599820818392 ) ) ;
#12563 = ORIENTED_EDGE ( 'NONE', *, *, #43362, .F. ) ;
#12564 = CARTESIAN_POINT ( 'NONE',  ( 12.89984683830242673, 19.51084698340348922, -21.40242721859379671 ) ) ;
#12565 = CARTESIAN_POINT ( 'NONE',  ( 11.13393739769619906, -63.52234721269329754, -43.76018303787720498 ) ) ;
#12566 = CARTESIAN_POINT ( 'NONE',  ( 23.04645959055375215, -19.60032229269020831, -59.67434578082231411 ) ) ;
#12567 = CARTESIAN_POINT ( 'NONE',  ( 14.13393739769630031, 1.391621760993509982, -35.14999999999999858 ) ) ;
#12568 = CARTESIAN_POINT ( 'NONE',  ( 50.90853239270390418, -50.90159765347700471, -76.14999999999999147 ) ) ;
#12569 = CARTESIAN_POINT ( 'NONE',  ( 15.09838756275151539, -23.52718865851687013, -44.04936391593793843 ) ) ;
#12570 = ORIENTED_EDGE ( 'NONE', *, *, #12191, .F. ) ;
#12571 = CARTESIAN_POINT ( 'NONE',  ( 15.24822711595714253, -8.849178317015910622, -67.91115244803380335 ) ) ;
#12572 = DIRECTION ( 'NONE',  ( 0.000000000000000000, -1.000000000000000000, 0.000000000000000000 ) ) ;
#12573 = DIRECTION ( 'NONE',  ( 0.000000000000000000, 1.000000000000000000, 0.000000000000000000 ) ) ;
#12574 = CARTESIAN_POINT ( 'NONE',  ( 52.63898214176290224, 22.88375766151639823, -56.80548791163010236 ) ) ;
#12575 = CARTESIAN_POINT ( 'NONE',  ( 24.37910050976440246, -15.61849357583439968, -73.79242048001989929 ) ) ;
#12576 = DIRECTION ( 'NONE',  ( 0.000000000000000000, 1.000000000000000000, 0.000000000000000000 ) ) ;
#12577 = CARTESIAN_POINT ( 'NONE',  ( 55.44685761138700286, 19.71482051860210305, -75.10951000879100548 ) ) ;
#12578 = PRODUCT_CONTEXT ( 'NONE', #7708, 'mechanical' ) ;
#12579 = CARTESIAN_POINT ( 'NONE',  ( 46.66850325959620704, -53.37252818194050263, -76.07618347743780873 ) ) ;
#12580 = VERTEX_POINT ( 'NONE', #614 ) ;
#12581 = VECTOR ( 'NONE', #34145, 1000.000000000000000 ) ;
#12582 = CARTESIAN_POINT ( 'NONE',  ( 12.70463616226759918, -22.23030920680289668, -64.88491241981458302 ) ) ;
#12583 = CIRCLE ( 'NONE', #48566, 11.00000000000000000 ) ;
#12584 = CARTESIAN_POINT ( 'NONE',  ( 11.96660005458869946, 10.88381105532060111, -34.64999999999999858 ) ) ;
#12585 = CIRCLE ( 'NONE', #15914, 21.19999999999999929 ) ;
#12586 = CARTESIAN_POINT ( 'NONE',  ( 79.93393739769618378, 0.9838110553206419473, -65.65000000000000568 ) ) ;
#12588 = ADVANCED_FACE ( 'NONE', ( #12951 ), #880, .T. ) ;
#12587 = CARTESIAN_POINT ( 'NONE',  ( 47.29840941369229768, 23.06589208105410194, -75.29255935572381020 ) ) ;
#12589 = CARTESIAN_POINT ( 'NONE',  ( 67.35174094906719233, 16.63381105532069881, -50.14999999999999858 ) ) ;
#12590 = CARTESIAN_POINT ( 'NONE',  ( 75.04939620295748171, -15.61618894467929941, -11.30491871076499955 ) ) ;
#12591 = CARTESIAN_POINT ( 'NONE',  ( 41.43651938946120339, -44.81260903795949702, -5.462494701013549836 ) ) ;
#12592 = DIRECTION ( 'NONE',  ( 0.000000000000000000, -1.000000000000000000, 0.000000000000000000 ) ) ;
#12593 = CARTESIAN_POINT ( 'NONE',  ( 15.08112966403183997, -49.61614526831208849, -83.21862149199232306 ) ) ;
#12594 = DIRECTION ( 'NONE',  ( 1.000000000000000000, 0.000000000000000000, 0.000000000000000000 ) ) ;
#12596 = CARTESIAN_POINT ( 'NONE',  ( 2.422196078461530178, -5.407548561780520124, -35.02873218748179340 ) ) ;
#12595 = FACE_OUTER_BOUND ( 'NONE', #30895, .T. ) ;
#12597 = CARTESIAN_POINT ( 'NONE',  ( 63.24512423172760833, 1.266538207494809942, -68.83138049123679991 ) ) ;
#12598 = CARTESIAN_POINT ( 'NONE',  ( 61.55001819026519883, 13.91412166380790083, -46.61080972681389767 ) ) ;
#12599 = CARTESIAN_POINT ( 'NONE',  ( -29.85095995338080144, -36.05272250015970315, -56.22640780866669985 ) ) ;
#12600 = CIRCLE ( 'NONE', #29681, 9.000000000000007105 ) ;
#12601 = ORIENTED_EDGE ( 'NONE', *, *, #203, .T. ) ;
#12602 = CARTESIAN_POINT ( 'NONE',  ( 53.11114670112049652, -49.51349214730240078, -48.80212167156650338 ) ) ;
#12603 = CARTESIAN_POINT ( 'NONE',  ( 60.21567619441049857, -45.11618902539440512, -26.18204139926109875 ) ) ;
#12604 = DIRECTION ( 'NONE',  ( 0.000000000000000000, 0.000000000000000000, -1.000000000000000000 ) ) ;
#12605 = CARTESIAN_POINT ( 'NONE',  ( 56.17536208834479794, 14.86527153403829971, -26.07752106846319862 ) ) ;
#12606 = CARTESIAN_POINT ( 'NONE',  ( 13.77244605588369986, -8.765738305821798804, -81.62651318459289485 ) ) ;
#12607 = CARTESIAN_POINT ( 'NONE',  ( 50.31585484903259697, 17.65744928731360375, -76.16276048729488934 ) ) ;
#12608 = CARTESIAN_POINT ( 'NONE',  ( 53.28345105766870660, 18.19680193626409803, -48.89794168120269546 ) ) ;
#12609 = CARTESIAN_POINT ( 'NONE',  ( 71.15040120820690106, 1.386342629514219826, -70.29952392096339508 ) ) ;
#12610 = DIRECTION ( 'NONE',  ( -0.3487035033511790005, 0.9372330909387559528, 0.000000000000000000 ) ) ;
#12611 = CARTESIAN_POINT ( 'NONE',  ( 16.13393739769620083, -15.61618894467929941, -28.45282021618999835 ) ) ;
#12612 = ORIENTED_EDGE ( 'NONE', *, *, #47093, .T. ) ;
#12613 = DIRECTION ( 'NONE',  ( 0.000000000000000000, 0.000000000000000000, -1.000000000000000000 ) ) ;
#12614 = ADVANCED_FACE ( 'NONE', ( #49116 ), #17651, .T. ) ;
#12615 = CARTESIAN_POINT ( 'NONE',  ( 23.04644611198230209, -19.60034754886721586, -39.95900824456602152 ) ) ;
#12616 = CARTESIAN_POINT ( 'NONE',  ( 73.20448466830819712, 0.9214125008369580261, -68.85787081529349507 ) ) ;
#12617 = CARTESIAN_POINT ( 'NONE',  ( 47.53847576963629251, -54.58151887390520329, -54.98789247430620009 ) ) ;
#12618 = CARTESIAN_POINT ( 'NONE',  ( -3.777837493383019662, 16.75613853327890013, -4.322105422597779523 ) ) ;
#12619 = DIRECTION ( 'NONE',  ( 1.000000000000000000, 0.000000000000000000, 0.000000000000000000 ) ) ;
#12620 = CARTESIAN_POINT ( 'NONE',  ( 41.50224533218039369, 12.67611161623769966, -3.489448898335199889 ) ) ;
#12621 = CARTESIAN_POINT ( 'NONE',  ( 59.95492767597970385, 15.44492512077309954, -48.75686613284650406 ) ) ;
#12622 = CARTESIAN_POINT ( 'NONE',  ( 71.35306154470789863, 1.325839985408290067, -60.87288092506760506 ) ) ;
#12623 = DIRECTION ( 'NONE',  ( 1.000000000000000000, 0.000000000000000000, 0.000000000000000000 ) ) ;
#12624 = CARTESIAN_POINT ( 'NONE',  ( 71.77894708589589357, 1.045341414532560131, -60.89274515693429635 ) ) ;
#12625 = CIRCLE ( 'NONE', #42752, 2.999999999999999112 ) ;
#12626 = AXIS2_PLACEMENT_3D ( 'NONE', #26405, #35318, #11490 ) ;
#12627 = CARTESIAN_POINT ( 'NONE',  ( 8.222911478911663963, -16.65154701704570428, -72.46599137466046159 ) ) ;
#12628 = CARTESIAN_POINT ( 'NONE',  ( 64.86043556304430524, 0.9234936569010840923, -70.67837287176459427 ) ) ;
#12629 = VERTEX_POINT ( 'NONE', #33355 ) ;
#12630 = ORIENTED_EDGE ( 'NONE', *, *, #29278, .F. ) ;
#12631 = CARTESIAN_POINT ( 'NONE',  ( 57.03107157439150399, 18.99627872735710099, -52.68131390763750233 ) ) ;
#12632 = CARTESIAN_POINT ( 'NONE',  ( 68.13393739769618662, -28.80002732851770020, -29.09832030244573176 ) ) ;
#12633 = ORIENTED_EDGE ( 'NONE', *, *, #38152, .F. ) ;
#12634 = DIRECTION ( 'NONE',  ( 1.000000000000000000, 0.000000000000000000, 0.000000000000000000 ) ) ;
#12635 = CARTESIAN_POINT ( 'NONE',  ( 12.58828357193830172, -65.45077103634190507, -46.93561978748050478 ) ) ;
#12636 = DIRECTION ( 'NONE',  ( 0.000000000000000000, 0.000000000000000000, 1.000000000000000000 ) ) ;
#12637 = CARTESIAN_POINT ( 'NONE',  ( 51.41094451178410196, 19.64869940956030092, -76.16757071412951063 ) ) ;
#12638 = ORIENTED_EDGE ( 'NONE', *, *, #5162, .T. ) ;
#12639 = DIRECTION ( 'NONE',  ( 1.000000000000000000, 0.000000000000000000, 0.000000000000000000 ) ) ;
#12640 = CARTESIAN_POINT ( 'NONE',  ( 17.86241643334011187, -9.013718618831822127, -72.03414713418756321 ) ) ;
#12641 = CARTESIAN_POINT ( 'NONE',  ( 61.06898323382710458, 14.42329441383000166, -47.72188698851990551 ) ) ;
#12642 = CARTESIAN_POINT ( 'NONE',  ( 20.26051206097820057, -22.75440311940770144, -48.12548681540710049 ) ) ;
#12643 = CARTESIAN_POINT ( 'NONE',  ( 16.13393739769620083, -15.61618894467929941, 9.349999999999999645 ) ) ;
#12644 = CARTESIAN_POINT ( 'NONE',  ( 41.73321004121098809, -37.58017348599624086, -81.65362388221058154 ) ) ;
#12645 = ORIENTED_EDGE ( 'NONE', *, *, #19489, .T. ) ;
#12646 = CARTESIAN_POINT ( 'NONE',  ( 12.20062103054560154, -65.06698704065620120, -24.22096211478449845 ) ) ;
#12647 = CARTESIAN_POINT ( 'NONE',  ( 13.64647048605240087, -8.400295753671970900, -81.40635028194188294 ) ) ;
#12648 = CARTESIAN_POINT ( 'NONE',  ( 11.27217865805896935, -9.290084831313485836, -32.79933351145292875 ) ) ;
#12649 = ADVANCED_FACE ( 'NONE', ( #40969 ), #48847, .T. ) ;
#12650 = CARTESIAN_POINT ( 'NONE',  ( 14.72993406020890106, 21.17773733622360410, -76.03043890231919022 ) ) ;
#12651 = PRODUCT_DEFINITION_FORMATION_WITH_SPECIFIED_SOURCE ( 'ANY', '', #34076, .NOT_KNOWN. ) ;
#12652 = EDGE_CURVE ( 'NONE', #42937, #35762, #29166, .T. ) ;
#12653 = CARTESIAN_POINT ( 'NONE',  ( 24.04415599056204300, -15.73629021646003423, -59.79715706112911278 ) ) ;
#12654 = AXIS2_PLACEMENT_3D ( 'NONE', #21926, #14342, #30312 ) ;
#12655 =( BOUNDED_CURVE ( )  B_SPLINE_CURVE ( 3, ( #49920, #13759, #25264, #41271 ),
 .UNSPECIFIED., .F., .T. ) 
 B_SPLINE_CURVE_WITH_KNOTS ( ( 4, 4 ),
 ( 1.776356948991648501E-15, 0.7853981633974506105 ),
 .UNSPECIFIED. ) 
 CURVE ( )  GEOMETRIC_REPRESENTATION_ITEM ( )  RATIONAL_B_SPLINE_CURVE ( ( 1.000000000000000000, 0.9492530216741910110, 0.9492530216741910110, 1.000000000000000000 ) ) 
 REPRESENTATION_ITEM ( '' )  );
#12656 = EDGE_CURVE ( 'NONE', #14552, #35613, #21509, .T. ) ;
#12657 = CIRCLE ( 'NONE', #6834, 12.00000000000000000 ) ;
#12658 = CARTESIAN_POINT ( 'NONE',  ( 83.66217889154638954, -44.50588631589649680, -46.56966809452229938 ) ) ;
#12659 = CARTESIAN_POINT ( 'NONE',  ( 52.13393739769620083, -15.61618894467929941, 8.349999999999999645 ) ) ;
#12660 = EDGE_CURVE ( 'NONE', #27825, #36314, #25, .T. ) ;
#12661 = CARTESIAN_POINT ( 'NONE',  ( 23.90403299955350036, -12.85786788886049870, -43.39908821103399816 ) ) ;
#12662 = ORIENTED_EDGE ( 'NONE', *, *, #9872, .T. ) ;
#12663 = CARTESIAN_POINT ( 'NONE',  ( 55.73706246701259914, -46.50826300295120319, -26.08342414098009954 ) ) ;
#12664 = CARTESIAN_POINT ( 'NONE',  ( 15.33884134719679970, -50.95795189269119874, -21.05298682722330028 ) ) ;
#12665 = CARTESIAN_POINT ( 'NONE',  ( 75.67065349138719910, 10.96988367743719905, -13.30225599929439895 ) ) ;
#12666 = CARTESIAN_POINT ( 'NONE',  ( 11.27236956094300524, -21.94243751200594517, -64.50066548858299598 ) ) ;
#12667 = CARTESIAN_POINT ( 'NONE',  ( 9.367050196127319595, -15.61601677469269944, -55.84717978380999881 ) ) ;
#12668 = CARTESIAN_POINT ( 'NONE',  ( 48.01233081821040116, 14.92652286517469840, -11.04035587481109992 ) ) ;
#12669 = ORIENTED_EDGE ( 'NONE', *, *, #42970, .F. ) ;
#12670 = CARTESIAN_POINT ( 'NONE',  ( -8.353750934443111120, -44.79785993618280315, -5.771191893815999840 ) ) ;
#12671 = CARTESIAN_POINT ( 'NONE',  ( 47.37241341519619908, 23.44179538337159840, -54.81883836474389682 ) ) ;
#12672 = CARTESIAN_POINT ( 'NONE',  ( 17.90525427422480576, -22.20704256537504406, -48.86948804866545260 ) ) ;
#12673 = CARTESIAN_POINT ( 'NONE',  ( 63.10820510261260097, 1.196343736543249880, -62.56767596405429543 ) ) ;
#12674 = CARTESIAN_POINT ( 'NONE',  ( 57.26283650403279779, -50.61205995118769607, -53.75815461969219911 ) ) ;
#12675 = CARTESIAN_POINT ( 'NONE',  ( 11.65058176314570204, 34.15932221946850689, -17.77752836889980159 ) ) ;
#12676 = DIRECTION ( 'NONE',  ( 1.000000000000000000, 0.000000000000000000, 0.000000000000000000 ) ) ;
#12677 = CARTESIAN_POINT ( 'NONE',  ( 8.428856623959452676, -13.54543936269719140, -60.87566458307732375 ) ) ;
#12678 = DIRECTION ( 'NONE',  ( 1.000000000000000000, 0.000000000000000000, 0.000000000000000000 ) ) ;
#12679 = CARTESIAN_POINT ( 'NONE',  ( 57.78559058653489444, -47.16042636242490005, -48.07973249810120109 ) ) ;
#12680 = CARTESIAN_POINT ( 'NONE',  ( 22.20417850065088672, -53.99262654159362285, -34.79644414665607144 ) ) ;
#12681 = CARTESIAN_POINT ( 'NONE',  ( 9.761022321705594251, -12.73102580472821188, -79.98287061730054859 ) ) ;
#12682 = CARTESIAN_POINT ( 'NONE',  ( 56.35963046933279941, 19.47216735375640084, -53.17943760849389889 ) ) ;
#12683 = EDGE_CURVE ( 'NONE', #13016, #29610, #7911, .T. ) ;
#12684 = CARTESIAN_POINT ( 'NONE',  ( 9.221450368820928389, -11.63199578712598914, -76.95899765199676779 ) ) ;
#12685 = CARTESIAN_POINT ( 'NONE',  ( 17.01977459420146843, -8.849194511386347273, -47.99448796539336826 ) ) ;
#12686 = VERTEX_POINT ( 'NONE', #36769 ) ;
#12687 = CARTESIAN_POINT ( 'NONE',  ( 20.08792735693718257, 24.05142850327904114, -19.47857086969157336 ) ) ;
#12688 = CARTESIAN_POINT ( 'NONE',  ( 9.276689947635228251, 31.90394069607099681, -46.53283565787430831 ) ) ;
#12689 = CARTESIAN_POINT ( 'NONE',  ( 37.13393739769620083, -49.11618894467930829, -35.14999999999999858 ) ) ;
#12690 = LINE ( 'NONE', #25227, #37670 ) ;
#12691 = VERTEX_POINT ( 'NONE', #5086 ) ;
#12692 = CARTESIAN_POINT ( 'NONE',  ( 18.76339275528779993, 20.38750180725810068, -74.54610039094001195 ) ) ;
#12693 = ORIENTED_EDGE ( 'NONE', *, *, #32094, .F. ) ;
#12694 = VERTEX_POINT ( 'NONE', #25226 ) ;
#12695 = ORIENTED_EDGE ( 'NONE', *, *, #41068, .F. ) ;
#12696 = CARTESIAN_POINT ( 'NONE',  ( 11.48931359425379917, -64.94058050441130092, -46.32476902050240142 ) ) ;
#12697 = CARTESIAN_POINT ( 'NONE',  ( 13.19564766795559940, 10.36739510386719942, -74.14999999999999147 ) ) ;
#12698 = CARTESIAN_POINT ( 'NONE',  ( 22.56752014421309838, -18.82624589827599948, -81.23899999999999011 ) ) ;
#12699 = TOROIDAL_SURFACE ( 'NONE', #23546, 16.49999999812870044, 0.4999999999096970127 ) ;
#12700 = CARTESIAN_POINT ( 'NONE',  ( 61.44121449269439950, 14.11490161821189915, -47.30183376429939557 ) ) ;
#12701 = VERTEX_POINT ( 'NONE', #21039 ) ;
#12702 = VECTOR ( 'NONE', #12592, 1000.000000000000000 ) ;
#12703 = EDGE_CURVE ( 'NONE', #45483, #36729, #33476, .T. ) ;
#12704 = ORIENTED_EDGE ( 'NONE', *, *, #45777, .T. ) ;
#12705 = AXIS2_PLACEMENT_3D ( 'NONE', #40790, #36861, #44467 ) ;
#12706 = CARTESIAN_POINT ( 'NONE',  ( 8.835310940912428634, -63.39783216298952340, -46.67672963611274639 ) ) ;
#12707 = ORIENTED_EDGE ( 'NONE', *, *, #39393, .T. ) ;
#12708 = CARTESIAN_POINT ( 'NONE',  ( 16.13393739769620083, -15.61618894467929941, -23.15000000000000213 ) ) ;
#12709 = DIRECTION ( 'NONE',  ( -0.5765530599821041546, 0.1342272854595170650, 0.8059588108975803689 ) ) ;
#12710 = CARTESIAN_POINT ( 'NONE',  ( 22.20417850065061671, 22.76024865223504889, -34.79644414665609986 ) ) ;
#12711 = VERTEX_POINT ( 'NONE', #41232 ) ;
#12712 = ORIENTED_EDGE ( 'NONE', *, *, #2055, .T. ) ;
#12713 = CARTESIAN_POINT ( 'NONE',  ( 0.2589946642438165636, -10.52437269067010028, -34.65038329361674840 ) ) ;
#12714 = CARTESIAN_POINT ( 'NONE',  ( 15.19952276919313405, -14.93729697828149305, 36.77166666666649775 ) ) ;
#12715 = CARTESIAN_POINT ( 'NONE',  ( 66.37097619575690999, 13.88381105527300008, -12.87819276387750200 ) ) ;
#12716 = CARTESIAN_POINT ( 'NONE',  ( 48.60513791338269840, 13.96979094684940037, -10.18381246284539898 ) ) ;
#12717 = DIRECTION ( 'NONE',  ( 0.5685928097855371677, 0.5944782866685501821, -0.5685928097855381669 ) ) ;
#12718 = CARTESIAN_POINT ( 'NONE',  ( -4.835991491254990393, 16.08822738447750211, -4.623964749956109621 ) ) ;
#12719 = DIRECTION ( 'NONE',  ( 0.000000000000000000, 0.000000000000000000, 1.000000000000000000 ) ) ;
#12720 = CARTESIAN_POINT ( 'NONE',  ( 61.22342406473160281, 14.00737724369909998, -27.78055241644990048 ) ) ;
#12721 = ADVANCED_FACE ( 'NONE', ( #8750 ), #16600, .T. ) ;
#12722 = CARTESIAN_POINT ( 'NONE',  ( 8.640695177360781187, -17.94815575631400151, -62.19146876365159216 ) ) ;
#12723 = ORIENTED_EDGE ( 'NONE', *, *, #32815, .T. ) ;
#12724 = FACE_OUTER_BOUND ( 'NONE', #34192, .T. ) ;
#12725 = DIRECTION ( 'NONE',  ( 0.6911981449639432729, -0.7226652920947591596, -1.665334536937735304E-16 ) ) ;
#12726 = CARTESIAN_POINT ( 'NONE',  ( 11.43204200631220147, 33.34744811485270333, -44.55415195516030025 ) ) ;
#12727 = CARTESIAN_POINT ( 'NONE',  ( 72.35673087767170841, 1.454949836291170140, -69.56035747320190410 ) ) ;
#12728 = CARTESIAN_POINT ( 'NONE',  ( 44.03040329333745717, -39.95715391141960282, -66.51246656095132437 ) ) ;
#12729 = AXIS2_PLACEMENT_3D ( 'NONE', #421, #171, #4606 ) ;
#12730 = DIRECTION ( 'NONE',  ( 0.000000000000000000, -1.000000000000000000, 0.000000000000000000 ) ) ;
#12731 = CARTESIAN_POINT ( 'NONE',  ( 12.32752973435950139, 18.90079518381709889, -21.15176878868719967 ) ) ;
#12732 = CARTESIAN_POINT ( 'NONE',  ( 46.91750385626450282, 22.97282184422540396, -75.61476978748720512 ) ) ;
#12733 = CARTESIAN_POINT ( 'NONE',  ( 49.30791778510940304, -53.55500811875160139, -54.21103610182979793 ) ) ;
#12734 = CARTESIAN_POINT ( 'NONE',  ( -6.464119761774720807, 15.22590418212459973, -5.599264135990670077 ) ) ;
#12735 = CARTESIAN_POINT ( 'NONE',  ( 8.220189996527228260, -15.80974140266152084, -34.49988352258923641 ) ) ;
#12736 = CARTESIAN_POINT ( 'NONE',  ( 65.36111454919441144, -32.61132143204090283, -18.37584003036852565 ) ) ;
#12738 = EDGE_CURVE ( 'NONE', #26641, #7703, #12585, .T. ) ;
#12737 = CARTESIAN_POINT ( 'NONE',  ( 8.428864736639086530, -17.68696802423094994, -54.70899843708602361 ) ) ;
#12739 = VERTEX_POINT ( 'NONE', #4813 ) ;
#12740 = CARTESIAN_POINT ( 'NONE',  ( 14.17109353987640041, -22.80325638057830417, -45.65220606189499364 ) ) ;
#12741 = CARTESIAN_POINT ( 'NONE',  ( 64.20123866503199395, 1.456055805561079941, -61.44407688768469455 ) ) ;
#12742 = ORIENTED_EDGE ( 'NONE', *, *, #35492, .F. ) ;
#12743 = FACE_OUTER_BOUND ( 'NONE', #3542, .T. ) ;
#12744 = CARTESIAN_POINT ( 'NONE',  ( 61.28745719582129681, -45.57643085924389936, -47.65111777937660520 ) ) ;
#12745 = CARTESIAN_POINT ( 'NONE',  ( 55.91596999402320023, 14.67228162054319895, -25.32543311652580087 ) ) ;
#12746 = CARTESIAN_POINT ( 'NONE',  ( 72.30699981945301147, -43.38479194641627856, -12.49561599343400076 ) ) ;
#12748 = CARTESIAN_POINT ( 'NONE',  ( 23.83903410062788808, -17.68688213715710589, -77.87566196558225329 ) ) ;
#12747 = CARTESIAN_POINT ( 'NONE',  ( 42.92581320805854972, 8.626641518850258095, -71.85816444028515093 ) ) ;
#12749 = CARTESIAN_POINT ( 'NONE',  ( 11.79459217608838806, -41.85765695298068323, -34.70142521051216988 ) ) ;
#12750 = DIRECTION ( 'NONE',  ( -0.4096086573010331855, 0.9122613374817791776, 0.000000000000000000 ) ) ;
#12751 = ORIENTED_EDGE ( 'NONE', *, *, #46268, .F. ) ;
#12752 = CARTESIAN_POINT ( 'NONE',  ( 83.74313374146190370, -44.96662509718390055, -47.44649717229009411 ) ) ;
#12753 = EDGE_LOOP ( 'NONE', ( #13575, #29230, #25023, #46231, #19392 ) ) ;
#12754 = ORIENTED_EDGE ( 'NONE', *, *, #46237, .F. ) ;
#12755 = ORIENTED_EDGE ( 'NONE', *, *, #24143, .T. ) ;
#12756 = CARTESIAN_POINT ( 'NONE',  ( 61.68987997863069950, -45.11739586860179685, -46.50241001583690093 ) ) ;
#12757 = CARTESIAN_POINT ( 'NONE',  ( 53.11711213144224075, -50.37382258259036405, -77.21690155561020674 ) ) ;
#12758 = CARTESIAN_POINT ( 'NONE',  ( 76.45005458917839292, -6.303208319860135411, -13.01219602681204890 ) ) ;
#12759 = CARTESIAN_POINT ( 'NONE',  ( 52.54597304093680776, -52.44574054386669815, -54.34384594454520112 ) ) ;
#12760 = EDGE_LOOP ( 'NONE', ( #19770, #33450, #34068, #30674 ) ) ;
#12761 = ADVANCED_FACE ( 'NONE', ( #44908 ), #24957, .T. ) ;
#12762 = ORIENTED_EDGE ( 'NONE', *, *, #4835, .F. ) ;
#12763 = CARTESIAN_POINT ( 'NONE',  ( -0.02605860948296716273, 14.44407830860123454, -34.78912696276449878 ) ) ;
#12764 = DIRECTION ( 'NONE',  ( 1.000000000000000000, 0.000000000000000000, 0.000000000000000000 ) ) ;
#12765 = ADVANCED_FACE ( 'NONE', ( #25741 ), #9789, .F. ) ;
#12766 = CARTESIAN_POINT ( 'NONE',  ( 16.13393739769620083, -15.61618894467929941, -35.14999999999999858 ) ) ;
#12767 = DIRECTION ( 'NONE',  ( -0.7226652920947586045, 0.6911981449639438280, 0.000000000000000000 ) ) ;
#12768 = LINE ( 'NONE', #32125, #45966 ) ;
#12769 = CARTESIAN_POINT ( 'NONE',  ( 52.25096642469739550, -49.77129145263110388, -77.19024991109920109 ) ) ;
#12770 = EDGE_CURVE ( 'NONE', #31099, #10836, #24253, .T. ) ;
#12771 = VECTOR ( 'NONE', #12636, 1000.000000000000000 ) ;
#12772 = ORIENTED_EDGE ( 'NONE', *, *, #40810, .F. ) ;
#12773 = FACE_OUTER_BOUND ( 'NONE', #1724, .T. ) ;
#12775 = CARTESIAN_POINT ( 'NONE',  ( 52.87559987180819832, -50.28015522989610275, -77.15855498308799554 ) ) ;
#12774 = CIRCLE ( 'NONE', #47084, 2.000000000000000000 ) ;
#12776 = CARTESIAN_POINT ( 'NONE',  ( 64.77932207159149414, 0.8936201581567910779, -70.62461353540290077 ) ) ;
#12777 = CARTESIAN_POINT ( 'NONE',  ( 60.61199691158600444, 14.35120867319030147, -47.15909868881769995 ) ) ;
#12778 = CARTESIAN_POINT ( 'NONE',  ( 19.97010344705880414, -8.769979947482401172, -67.67506889758131194 ) ) ;
#12779 = CARTESIAN_POINT ( 'NONE',  ( -0.03447620312153085176, -4.141051901845263394, -34.79644660940673617 ) ) ;
#12780 = CARTESIAN_POINT ( 'NONE',  ( 54.26302937888129918, 19.38381105532069881, -76.97756791992739522 ) ) ;
#12781 = CARTESIAN_POINT ( 'NONE',  ( 43.52841460840770083, -43.39558596462239848, -4.940445812193139830 ) ) ;
#12782 = DIRECTION ( 'NONE',  ( 0.000000000000000000, 0.000000000000000000, -1.000000000000000000 ) ) ;
#12783 = CARTESIAN_POINT ( 'NONE',  ( 61.28293951100584991, -45.60372950919332879, -47.68063998090632083 ) ) ;
#12784 = CARTESIAN_POINT ( 'NONE',  ( 61.44929317945270242, -45.39846556447219683, -47.39907545912859632 ) ) ;
#12785 = EDGE_CURVE ( 'NONE', #34913, #3068, #18413, .T. ) ;
#12786 = CARTESIAN_POINT ( 'NONE',  ( 64.03000686827549259, 1.054783673856589887, -70.02747328088919687 ) ) ;
#12787 = FACE_OUTER_BOUND ( 'NONE', #51540, .T. ) ;
#12788 = CARTESIAN_POINT ( 'NONE',  ( 65.13923175699828505, 0.9544840682940559651, -17.74408481280750038 ) ) ;
#12789 = B_SPLINE_SURFACE_WITH_KNOTS ( 'NONE', 3, 3, ( 
 ( #26199, #50068, #37495, #13909, #22526, #29866 ),
 ( #50333, #49817, #14163, #26457, #42210, #34320 ),
 ( #45886, #42472, #22266, #2635, #1595, #46153 ),
 ( #9973, #1855, #17583, #49571, #34059, #6561 ),
 ( #38538, #13656, #42734, #25935, #14421, #50588 ),
 ( #41950, #30131, #33553, #10240, #30390, #18090 ),
 ( #41681, #29617, #14678, #22007, #30648, #37759 ),
 ( #18606, #45620, #26716, #46671, #34584, #2111 ),
 ( #10757, #6308, #17833, #9720, #25679, #5789 ),
 ( #38274, #21749, #33806, #2365, #18343, #46413 ) ),
 .UNSPECIFIED., .F., .F., .F.,
 ( 4, 2, 2, 2, 4 ),
 ( 4, 1, 1, 4 ),
 ( 1.507842000000000029E-11, 0.03085333683225299772, 0.08021867573973200105, 0.1592032179916990087, 0.2468266945524750233 ),
 ( 0.000000000000000000, 0.3333333333333329818, 0.6666666666666670737, 1.000000000000000000 ),
 .UNSPECIFIED. ) ;
#12790 = ADVANCED_FACE ( 'NONE', ( #46479 ), #42539, .T. ) ;
#12791 = EDGE_LOOP ( 'NONE', ( #13477, #39959, #51409, #50871 ) ) ;
#12792 = CARTESIAN_POINT ( 'NONE',  ( 13.93677001678689997, -51.54257389745239948, -75.18091805976820297 ) ) ;
#12793 = CARTESIAN_POINT ( 'NONE',  ( 47.29837881414660217, -54.72153260654879858, -54.69571569007759848 ) ) ;
#12794 = CARTESIAN_POINT ( 'NONE',  ( 20.99561754527899282, -9.290025391674188171, -37.21600393032817777 ) ) ;
#12795 = DIRECTION ( 'NONE',  ( 0.000000000000000000, 0.000000000000000000, 1.000000000000000000 ) ) ;
#12796 = CARTESIAN_POINT ( 'NONE',  ( 60.84935194822133298, -45.45999311571661394, -47.05836674529819419 ) ) ;
#12797 = CARTESIAN_POINT ( 'NONE',  ( 23.42912986796590147, -16.70365468919549912, -32.14999999999999858 ) ) ;
#12798 = DIRECTION ( 'NONE',  ( 0.000000000000000000, 0.000000000000000000, -1.000000000000000000 ) ) ;
#12799 = CARTESIAN_POINT ( 'NONE',  ( 47.72549663628029748, -54.49022007495739928, -54.99080477840750092 ) ) ;
#12800 = B_SPLINE_CURVE_WITH_KNOTS ( 'NONE', 3,
 ( #24772, #4883, #41816, #49441, #26075, #5923, #17970, #21887, #1212, #37625 ),
 .UNSPECIFIED., .F., .F.,
 ( 4, 2, 2, 2, 4 ),
 ( 0.000000000000000000, 0.2500000000000000000, 0.5000000000000000000, 0.7500000000000000000, 1.000000000000000000 ),
 .UNSPECIFIED. ) ;
#12802 = CARTESIAN_POINT ( 'NONE',  ( -8.353750934443111120, -44.79785993618280315, -5.771191893815999840 ) ) ;
#12801 = CARTESIAN_POINT ( 'NONE',  ( 47.41053031099697535, 23.00881197028234126, -75.29848679969852299 ) ) ;
#12803 = CARTESIAN_POINT ( 'NONE',  ( 35.44295439207109411, -15.61618894467929941, 17.35000000000000142 ) ) ;
#12804 = CARTESIAN_POINT ( 'NONE',  ( 48.89501045483829955, 22.56229972626200109, -54.41963477494619639 ) ) ;
#12805 = ORIENTED_EDGE ( 'NONE', *, *, #39065, .F. ) ;
#12806 = CIRCLE ( 'NONE', #3751, 9.000000000000007105 ) ;
#12807 = VECTOR ( 'NONE', #2351, 1000.000000000000000 ) ;
#12808 = CARTESIAN_POINT ( 'NONE',  ( 22.93259508256310042, -13.73980602574960130, -64.76146233876720260 ) ) ;
#12809 = ORIENTED_EDGE ( 'NONE', *, *, #24705, .F. ) ;
#12810 = CARTESIAN_POINT ( 'NONE',  ( 18.86789271228509790, -51.78678246903520233, -74.14999999999999147 ) ) ;
#12811 = DIRECTION ( 'NONE',  ( 0.5322052227529140422, -0.8460333946355099721, -0.03138623959693901538 ) ) ;
#12812 = CARTESIAN_POINT ( 'NONE',  ( 16.13393739769620083, -15.61618894467929941, -44.64999999999999858 ) ) ;
#12814 = CARTESIAN_POINT ( 'NONE',  ( 52.66238559674269482, 18.53796498309249685, -28.15003238672679942 ) ) ;
#12813 = CARTESIAN_POINT ( 'NONE',  ( 83.93027249483741059, 13.00900601712620031, -46.75947739037570017 ) ) ;
#12815 = CARTESIAN_POINT ( 'NONE',  ( 12.14570635151480005, -21.43311010788070092, -61.14412876928479790 ) ) ;
#12816 = CARTESIAN_POINT ( 'NONE',  ( 12.16231664502931054, 33.44509448364060233, -15.91745067705889838 ) ) ;
#12817 = CARTESIAN_POINT ( 'NONE',  ( 55.34563173526050406, -45.32107452727160535, -15.30572482678790003 ) ) ;
#12818 = CARTESIAN_POINT ( 'NONE',  ( 14.06335524534715908, -23.32131407103912579, -80.37566581158391443 ) ) ;
#12819 = ORIENTED_EDGE ( 'NONE', *, *, #7344, .F. ) ;
#12820 = VERTEX_POINT ( 'NONE', #41748 ) ;
#12821 = CARTESIAN_POINT ( 'NONE',  ( 11.74706319441139968, -64.93826315237700442, -16.38446683801559800 ) ) ;
#12822 = CARTESIAN_POINT ( 'NONE',  ( 11.17936320866890121, 33.58498632846880128, -46.45233409225559740 ) ) ;
#12823 = FACE_OUTER_BOUND ( 'NONE', #2860, .T. ) ;
#12824 = CARTESIAN_POINT ( 'NONE',  ( 52.81610072646800091, -49.60570963100419561, -48.45273747379939522 ) ) ;
#12825 = DIRECTION ( 'NONE',  ( 0.000000000000000000, -0.7071067811865492381, -0.7071067811865457964 ) ) ;
#12826 = ORIENTED_EDGE ( 'NONE', *, *, #8933, .F. ) ;
#12827 = CARTESIAN_POINT ( 'NONE',  ( 23.83903255575460278, -13.54548804232147852, -75.42431961480706093 ) ) ;
#12828 = CARTESIAN_POINT ( 'NONE',  ( 57.08024762781600003, 14.64810207517410134, -26.24981380567940192 ) ) ;
#12829 = EDGE_CURVE ( 'NONE', #19377, #29939, #47154, .T. ) ;
#12830 = VECTOR ( 'NONE', #44809, 1000.000000000000000 ) ;
#12831 = CARTESIAN_POINT ( 'NONE',  ( 52.20232727811570328, 19.58445708673409769, -50.88848071883410284 ) ) ;
#12832 = CARTESIAN_POINT ( 'NONE',  ( 72.49788296046230585, 1.442158793902679870, -69.35604527063249236 ) ) ;
#12833 = CARTESIAN_POINT ( 'NONE',  ( 50.35727174400659578, -49.18175002857950062, -76.16289466383710760 ) ) ;
#12834 = ADVANCED_FACE ( 'NONE', ( #26267 ), #38117, .T. ) ;
#12835 = CARTESIAN_POINT ( 'NONE',  ( 22.20417850065088672, -53.99262654159362285, -34.79644414665607144 ) ) ;
#12836 = EDGE_LOOP ( 'NONE', ( #27882, #40415, #15459, #48863, #20740, #42988, #50911 ) ) ;
#12837 = CARTESIAN_POINT ( 'NONE',  ( 55.48119509741179911, -46.46935189257190757, -25.44855095864909700 ) ) ;
#12838 = DIRECTION ( 'NONE',  ( 1.000000000000000000, 0.000000000000000000, 0.000000000000000000 ) ) ;
#12839 = ORIENTED_EDGE ( 'NONE', *, *, #51250, .F. ) ;
#12840 = LINE ( 'NONE', #504, #38559 ) ;
#12841 = CARTESIAN_POINT ( 'NONE',  ( 54.67502978642529854, 16.95168370974520400, -47.75230923849440501 ) ) ;
#12842 = CARTESIAN_POINT ( 'NONE',  ( 22.71421499214610051, -11.33989447733160105, -35.82905861000619296 ) ) ;
#12843 = CARTESIAN_POINT ( 'NONE',  ( 14.29753605308300024, -51.11618894450129602, -22.54695281101919946 ) ) ;
#12844 = CARTESIAN_POINT ( 'NONE',  ( 56.50762836072709661, 19.50983102606420161, -74.45401218589749703 ) ) ;
#12845 = CARTESIAN_POINT ( 'NONE',  ( 47.42184924485919595, -54.61356341195660491, -74.50157339271500234 ) ) ;
#12846 = ORIENTED_EDGE ( 'NONE', *, *, #48977, .F. ) ;
#12847 = DIRECTION ( 'NONE',  ( -0.8340645993220398013, -0.5516667872527448724, 0.000000000000000000 ) ) ;
#12848 = CIRCLE ( 'NONE', #10298, 9.768249999999998323 ) ;
#12849 = CARTESIAN_POINT ( 'NONE',  ( 19.81752810327339631, -22.09213314756820168, -64.56803669556019543 ) ) ;
#12850 = AXIS2_PLACEMENT_3D ( 'NONE', #37694, #49759, #29809 ) ;
#12851 = CARTESIAN_POINT ( 'NONE',  ( 52.74518595131819865, -49.73996312209429504, -48.86818382069139943 ) ) ;
#12852 = DIRECTION ( 'NONE',  ( 0.000000000000000000, -1.000000000000000000, 0.000000000000000000 ) ) ;
#12853 = DIRECTION ( 'NONE',  ( 0.000000000000000000, 0.000000000000000000, -1.000000000000000000 ) ) ;
#12854 = EDGE_CURVE ( 'NONE', #36393, #425, #26653, .T. ) ;
#12855 = CARTESIAN_POINT ( 'NONE',  ( 47.06884450802159847, 22.81823520743029832, -75.65261601872900599 ) ) ;
#12856 = EDGE_CURVE ( 'NONE', #45896, #37692, #50789, .T. ) ;
#12857 = CARTESIAN_POINT ( 'NONE',  ( 71.17905174416029013, 1.387412027389909985, -61.00994802092580471 ) ) ;
#12858 = CARTESIAN_POINT ( 'NONE',  ( -0.007164427059776000244, -8.408015226406421405, -34.77269723891829756 ) ) ;
#12859 = CYLINDRICAL_SURFACE ( 'NONE', #44484, 0.4999999999999994449 ) ;
#12860 = CARTESIAN_POINT ( 'NONE',  ( 14.11670613118836748, -49.61617733564492738, -83.15271738028131665 ) ) ;
#12861 = CIRCLE ( 'NONE', #32917, 1.000000000000000888 ) ;
#12862 = CARTESIAN_POINT ( 'NONE',  ( 16.13393739769620083, -15.61618894467929941, 9.349999999999999645 ) ) ;
#12864 = DIRECTION ( 'NONE',  ( 0.1960104533864299448, 0.03282462862515294483, 0.9800522669321607427 ) ) ;
#12863 = FILL_AREA_STYLE_COLOUR ( '', #44981 ) ;
#12865 = CARTESIAN_POINT ( 'NONE',  ( 63.16073670604789925, 0.9971903505820729485, -68.99379187066199393 ) ) ;
#12866 = CARTESIAN_POINT ( 'NONE',  ( 61.05616912171839772, 14.11849417979069976, -46.88539273277700659 ) ) ;
#12867 = CARTESIAN_POINT ( 'NONE',  ( -18.27909364759860011, -51.95925980240359365, -53.14840429075749739 ) ) ;
#12868 = VERTEX_POINT ( 'NONE', #31354 ) ;
#12869 = CARTESIAN_POINT ( 'NONE',  ( 52.72694793081979725, -49.72266251536069603, -48.50422612237640152 ) ) ;
#12870 = CARTESIAN_POINT ( 'NONE',  ( 57.65728964160980041, -45.29188684180090263, -25.94504736113060162 ) ) ;
#12871 = CARTESIAN_POINT ( 'NONE',  ( 47.64143405402000297, -54.53488714544439375, -55.14905519569939685 ) ) ;
#12872 = CARTESIAN_POINT ( 'NONE',  ( 57.20820941486360312, 14.23063652483599917, -26.05769543974410141 ) ) ;
#12873 = CARTESIAN_POINT ( 'NONE',  ( 10.34784237018260100, -19.64900680999069849, -33.25906503489069621 ) ) ;
#12874 = CARTESIAN_POINT ( 'NONE',  ( 51.47089496436409917, 18.97848234860349947, -76.34335219576519194 ) ) ;
#12875 = CARTESIAN_POINT ( 'NONE',  ( 53.10972315773789632, 18.29799478634210175, -48.97251032828970096 ) ) ;
#12876 = CARTESIAN_POINT ( 'NONE',  ( 71.13601697155240799, 1.385888765344509999, -70.30422512560809878 ) ) ;
#12877 = CARTESIAN_POINT ( 'NONE',  ( 41.36297991754139503, -44.03288059546800781, -3.553637027260359904 ) ) ;
#12878 = CARTESIAN_POINT ( 'NONE',  ( 72.02934741333440627, -44.96049524349189852, -13.48211756204479883 ) ) ;
#12879 = VERTEX_POINT ( 'NONE', #19063 ) ;
#12880 = CARTESIAN_POINT ( 'NONE',  ( 10.22095430177014208, -19.02405797898098427, -41.28611931081641728 ) ) ;
#12881 = CARTESIAN_POINT ( 'NONE',  ( 22.94884485421729892, -18.62679199014949560, -67.19975531119949608 ) ) ;
#12882 = B_SPLINE_CURVE_WITH_KNOTS ( 'NONE', 3,
 ( #40351, #12317, #19405, #28278, #35383, #44278, #35901, #7876, #23822, #32448 ),
 .UNSPECIFIED., .F., .F.,
 ( 4, 1, 1, 1, 1, 1, 1, 4 ),
 ( 0.000000000000000000, 0.06914192772689449484, 0.1483608587905285991, 0.2275797898541468967, 0.3067987209177651664, 0.3860176519813834362, 0.4652365830450022610, 0.5000014761122578699 ),
 .UNSPECIFIED. ) ;
#12884 = CARTESIAN_POINT ( 'NONE',  ( 73.01702207920239118, 1.186614556332910020, -68.98303591127670131 ) ) ;
#12883 = AXIS2_PLACEMENT_3D ( 'NONE', #35553, #43679, #27417 ) ;
#12885 = CARTESIAN_POINT ( 'NONE',  ( 47.46911263023690708, -54.60293551959159686, -54.68220836887759617 ) ) ;
#12886 = FACE_BOUND ( 'NONE', #15022, .T. ) ;
#12887 = CARTESIAN_POINT ( 'NONE',  ( 73.24770736846269870, 0.9209567800143640959, -62.51152384389749272 ) ) ;
#12888 = CARTESIAN_POINT ( 'NONE',  ( 59.79179082184240457, -29.88504740574800067, -15.96111194127940180 ) ) ;
#12889 = CARTESIAN_POINT ( 'NONE',  ( 71.38053669821270830, 1.187415670095769871, -60.71585052632950408 ) ) ;
#12890 = DIRECTION ( 'NONE',  ( -0.7071067811865457964, 0.7071067811865492381, 0.000000000000000000 ) ) ;
#12891 = CIRCLE ( 'NONE', #31252, 1.000000000000000888 ) ;
#12892 = CARTESIAN_POINT ( 'NONE',  ( 71.69261393255278847, 0.9208623934718309645, -60.81910352240609541 ) ) ;
#12893 = CARTESIAN_POINT ( 'NONE',  ( 24.04489399257771254, -15.64449612002278833, -71.50881132904470405 ) ) ;
#12894 = CARTESIAN_POINT ( 'NONE',  ( 65.01767019485730259, 1.328674444234379859, -70.47425850519080370 ) ) ;
#12895 = ORIENTED_EDGE ( 'NONE', *, *, #36257, .T. ) ;
#12896 = ORIENTED_EDGE ( 'NONE', *, *, #20724, .F. ) ;
#12897 = CARTESIAN_POINT ( 'NONE',  ( 9.299128317299539148, -63.29430534918720497, -46.53057822423220102 ) ) ;
#12898 = EDGE_CURVE ( 'NONE', #25812, #30115, #2124, .T. ) ;
#12899 = DIRECTION ( 'NONE',  ( 0.000000000000000000, 0.000000000000000000, -1.000000000000000000 ) ) ;
#12900 = ORIENTED_EDGE ( 'NONE', *, *, #36077, .F. ) ;
#12901 = CARTESIAN_POINT ( 'NONE',  ( 11.55362782463430094, -64.75226748267719756, -44.82234361046789672 ) ) ;
#12902 = CARTESIAN_POINT ( 'NONE',  ( 51.13393739769659874, -56.11618894467899565, 11.34999999999999964 ) ) ;
#12903 = CARTESIAN_POINT ( 'NONE',  ( 56.46551567295650642, 19.54378694285259854, -74.14999999999999147 ) ) ;
#12904 = CARTESIAN_POINT ( 'NONE',  ( 52.36416843628920503, 19.71812798544510059, -76.17671310447180133 ) ) ;
#12905 = VERTEX_POINT ( 'NONE', #15657 ) ;
#12906 = CYLINDRICAL_SURFACE ( 'NONE', #49367, 2.999999999999999112 ) ;
#12907 = CARTESIAN_POINT ( 'NONE',  ( 22.03478274538166204, -12.18589228887625886, -72.28500474705791135 ) ) ;
#12908 = DIRECTION ( 'NONE',  ( 0.000000000000000000, 0.000000000000000000, 1.000000000000000000 ) ) ;
#12909 = CARTESIAN_POINT ( 'NONE',  ( 19.14684319004119928, -7.941221925702031115, -39.41140439840899745 ) ) ;
#12910 = AXIS2_PLACEMENT_3D ( 'NONE', #21584, #37333, #24730 ) ;
#12911 = CARTESIAN_POINT ( 'NONE',  ( 22.89878139006187396, -15.43167601270388900, -56.44414743042131022 ) ) ;
#12912 = CARTESIAN_POINT ( 'NONE',  ( 43.32204027125330015, -37.82422349032574971, -73.70942140953911803 ) ) ;
#12913 = SHAPE_REPRESENTATION_RELATIONSHIP ( 'NONE' , 'NONE' ,  #4683, #12306 ) ;
#12914 = ORIENTED_EDGE ( 'NONE', *, *, #22640, .F. ) ;
#12915 = CARTESIAN_POINT ( 'NONE',  ( 12.73541647155440160, -65.46958205238559003, -23.66121539185130018 ) ) ;
#12916 = CARTESIAN_POINT ( 'NONE',  ( 10.58908913721369949, -20.59226687547690204, -36.99984868542069449 ) ) ;
#12917 = CARTESIAN_POINT ( 'NONE',  ( 12.04075003782359943, -10.20414989105540116, -32.14999999999999858 ) ) ;
#12918 = EDGE_CURVE ( 'NONE', #15737, #14356, #36807, .T. ) ;
#12919 = VECTOR ( 'NONE', #1657, 1000.000000000000114 ) ;
#12920 = EDGE_CURVE ( 'NONE', #28142, #31343, #19232, .T. ) ;
#12921 = CARTESIAN_POINT ( 'NONE',  ( 24.04511355972104170, -15.61618909363076924, -51.79233356384455078 ) ) ;
#12922 = CARTESIAN_POINT ( 'NONE',  ( 84.41931940662119871, -43.28155674284490573, -47.35294421590279512 ) ) ;
#12923 = CARTESIAN_POINT ( 'NONE',  ( 19.06829150976720300, -7.910847508120689930, -55.12349000844960045 ) ) ;
#12924 = VERTEX_POINT ( 'NONE', #31611 ) ;
#12925 = CARTESIAN_POINT ( 'NONE',  ( 52.87930525205649701, -49.56712260999589859, -27.60362057165029981 ) ) ;
#12926 = CARTESIAN_POINT ( 'NONE',  ( 15.80909573684840019, -51.11619220056719826, -21.61146777487360282 ) ) ;
#12927 = DIRECTION ( 'NONE',  ( 0.000000000000000000, 0.000000000000000000, -1.000000000000000000 ) ) ;
#12928 = DIRECTION ( 'NONE',  ( 0.000000000000000000, 0.000000000000000000, 1.000000000000000000 ) ) ;
#12929 = DIRECTION ( 'NONE',  ( 0.000000000000000000, 0.000000000000000000, 1.000000000000000000 ) ) ;
#12930 = ORIENTED_EDGE ( 'NONE', *, *, #31503, .F. ) ;
#12931 = CARTESIAN_POINT ( 'NONE',  ( -8.073667307587539810, -44.97251519369510220, -5.525879325573529677 ) ) ;
#12932 = CARTESIAN_POINT ( 'NONE',  ( 47.45724465533079695, 23.37779319940769795, -54.67644539602360254 ) ) ;
#12933 = CARTESIAN_POINT ( 'NONE',  ( 16.13393739769620083, -27.61618894467930119, -22.14999999999999858 ) ) ;
#12934 = CARTESIAN_POINT ( 'NONE',  ( 63.51391054266390768, 1.390208944942419755, -62.54542373973200142 ) ) ;
#12935 = LINE ( 'NONE', #24684, #18121 ) ;
#12936 = CARTESIAN_POINT ( 'NONE',  ( 11.64437502030500049, 34.15964300405810405, -17.80448360229059901 ) ) ;
#12937 = SPHERICAL_SURFACE ( 'NONE', #34453, 3.000000000000000000 ) ;
#12938 = CARTESIAN_POINT ( 'NONE',  ( 22.04686311925793873, -19.02415382287680501, -64.61948873146855021 ) ) ;
#12939 = CARTESIAN_POINT ( 'NONE',  ( 6.383937397696199945, -15.61618894467929941, -18.10000000000000142 ) ) ;
#12940 = CARTESIAN_POINT ( 'NONE',  ( 57.19193614679419824, -47.47137610322729984, -48.20267525396420183 ) ) ;
#12941 = CARTESIAN_POINT ( 'NONE',  ( 9.366764248923921343, -15.61602670952840199, -67.45282021618999124 ) ) ;
#12942 = VECTOR ( 'NONE', #41702, 1000.000000000000114 ) ;
#12943 = CARTESIAN_POINT ( 'NONE',  ( 64.93393739769589956, 1.396834109478120034, -61.06337307536559678 ) ) ;
#12944 = CARTESIAN_POINT ( 'NONE',  ( 17.78432835213279972, -52.62916658892859800, -76.03098605356829864 ) ) ;
#12945 = CARTESIAN_POINT ( 'NONE',  ( 17.01970822797235172, -22.38319285542060655, -60.91117069208365820 ) ) ;
#12946 = CARTESIAN_POINT ( 'NONE',  ( 11.21742354769409999, -20.67291226489259870, -61.59270509622239587 ) ) ;
#12947 = B_SPLINE_CURVE_WITH_KNOTS ( 'NONE', 3,
 ( #13668, #49583, #17846, #49322, #45380, #25434, #33818, #1607, #17595, #29631, #13924 ),
 .UNSPECIFIED., .F., .F.,
 ( 4, 1, 1, 1, 1, 1, 1, 1, 4 ),
 ( 0.4999960598860723193, 0.5157214477071244696, 0.5949403787707443492, 0.6741593098343618973, 0.7533782408979794454, 0.8325971719615969935, 0.9118161030252167620, 0.9910350340888344212, 1.000000000000000000 ),
 .UNSPECIFIED. ) ;
#12948 = ORIENTED_EDGE ( 'NONE', *, *, #11486, .T. ) ;
#12949 = CARTESIAN_POINT ( 'NONE',  ( -0.1946058609260517269, -10.66917667990032292, -34.93568796252242237 ) ) ;
#12950 = CARTESIAN_POINT ( 'NONE',  ( 10.13445450645900081, 31.88305279702909800, -45.99826666626069738 ) ) ;
#12951 = FACE_OUTER_BOUND ( 'NONE', #49580, .T. ) ;
#12952 = VECTOR ( 'NONE', #41079, 1000.000000000000000 ) ;
#12953 = CYLINDRICAL_SURFACE ( 'NONE', #23, 2.000000000000000444 ) ;
#12954 = VERTEX_POINT ( 'NONE', #11216 ) ;
#12955 = CARTESIAN_POINT ( 'NONE',  ( 18.20176657162249967, 20.17488022308399920, -75.08736963500949457 ) ) ;
#12956 = ORIENTED_EDGE ( 'NONE', *, *, #34703, .T. ) ;
#12957 = VERTEX_POINT ( 'NONE', #30841 ) ;
#12958 = EDGE_CURVE ( 'NONE', #39697, #15276, #40269, .T. ) ;
#12959 = AXIS2_PLACEMENT_3D ( 'NONE', #27150, #43157, #23456 ) ;
#12960 = ORIENTED_EDGE ( 'NONE', *, *, #24191, .F. ) ;
#12961 = CARTESIAN_POINT ( 'NONE',  ( 13.00893739769619906, -65.51843714052719747, -47.75434321273180416 ) ) ;
#12962 = CARTESIAN_POINT ( 'NONE',  ( -30.36606260230379917, -53.11618894467940066, 17.35000000000000142 ) ) ;
#12963 = CARTESIAN_POINT ( 'NONE',  ( 22.97220002312930376, -18.05331211082319953, -81.23899999999999011 ) ) ;
#12964 = EDGE_CURVE ( 'NONE', #8804, #24630, #6719, .T. ) ;
#12965 = CARTESIAN_POINT ( 'NONE',  ( 61.54660442415410415, 14.01734467809300000, -47.08946784971580257 ) ) ;
#12966 = EDGE_CURVE ( 'NONE', #48439, #28134, #35254, .T. ) ;
#12967 = CARTESIAN_POINT ( 'NONE',  ( 16.13393739769620083, -15.61618894467929941, -32.14999999999999858 ) ) ;
#12968 = EDGE_LOOP ( 'NONE', ( #36527, #15597, #18724, #22904, #688 ) ) ;
#12969 = ORIENTED_EDGE ( 'NONE', *, *, #29963, .T. ) ;
#12970 = DIRECTION ( 'NONE',  ( 0.000000000000000000, -1.000000000000000000, 0.000000000000000000 ) ) ;
#12971 = VERTEX_POINT ( 'NONE', #43693 ) ;
#12972 = CARTESIAN_POINT ( 'NONE',  ( 49.62157902422839584, -46.18329155571620248, -12.18456390873380002 ) ) ;
#12973 = LINE ( 'NONE', #19332, #5378 ) ;
#12974 = CARTESIAN_POINT ( 'NONE',  ( 9.125046732747128075, -54.99886678830583264, -46.59642014776720487 ) ) ;
#12975 = ORIENTED_EDGE ( 'NONE', *, *, #30582, .F. ) ;
#12977 = EDGE_LOOP ( 'NONE', ( #35774, #9091, #18734, #50473, #50631 ) ) ;
#12976 =( BOUNDED_CURVE ( )  B_SPLINE_CURVE ( 3, ( #23853, #6886, #27295, #39619 ),
 .UNSPECIFIED., .F., .T. ) 
 B_SPLINE_CURVE_WITH_KNOTS ( ( 4, 4 ),
 ( 2.356194490192338620, 3.141592653589793116 ),
 .UNSPECIFIED. ) 
 CURVE ( )  GEOMETRIC_REPRESENTATION_ITEM ( )  RATIONAL_B_SPLINE_CURVE ( ( 1.000000000000000000, 0.9492530216741903448, 0.9492530216741903448, 1.000000000000000000 ) ) 
 REPRESENTATION_ITEM ( '' )  );
#12978 = CARTESIAN_POINT ( 'NONE',  ( 9.205734167420699166, -27.61618894467930119, -24.14999999999999858 ) ) ;
#12979 = CARTESIAN_POINT ( 'NONE',  ( 3.901957390959666760, -24.50324262128464170, -6.721843382729280059 ) ) ;
#12980 = CARTESIAN_POINT ( 'NONE',  ( 75.48397637297750862, 12.14069267741320068, -13.40632821845509959 ) ) ;
#12981 = CARTESIAN_POINT ( 'NONE',  ( 47.44609020368039864, 14.70937406344200049, -10.50457812665930035 ) ) ;
#12982 = CIRCLE ( 'NONE', #41430, 2.999999999999999112 ) ;
#12983 = EDGE_CURVE ( 'NONE', #19647, #16412, #33385, .T. ) ;
#12984 = FACE_OUTER_BOUND ( 'NONE', #38341, .T. ) ;
#12985 = CARTESIAN_POINT ( 'NONE',  ( -3.223188684962630113, 17.15855307271669616, -4.799566724645049298 ) ) ;
#12986 = CARTESIAN_POINT ( 'NONE',  ( 3.310925894260581703, -55.48813533678121246, -8.795375239069176843 ) ) ;
#12987 = CARTESIAN_POINT ( 'NONE',  ( -18.86606260230360022, -50.61618894467959962, 10.84999999999999964 ) ) ;
#12988 = CARTESIAN_POINT ( 'NONE',  ( 15.14076279674840109, -7.831566128176559616, -70.74711331852249430 ) ) ;
#12989 = ORIENTED_EDGE ( 'NONE', *, *, #38834, .T. ) ;
#12990 = CARTESIAN_POINT ( 'NONE',  ( 53.48663704682059716, 18.10898805450199944, -49.00013169075800334 ) ) ;
#12991 = VECTOR ( 'NONE', #10668, 1000.000000000000227 ) ;
#12992 = CARTESIAN_POINT ( 'NONE',  ( -8.936454256227198911, -44.38145435695279417, -6.564742439952559572 ) ) ;
#12993 = CARTESIAN_POINT ( 'NONE',  ( 12.43322004349129983, 34.16501222894959966, -46.71928908691679538 ) ) ;
#12994 = CARTESIAN_POINT ( 'NONE',  ( 72.24311954201340313, 1.458407608744489936, -69.69055806410209186 ) ) ;
#12996 = EDGE_CURVE ( 'NONE', #41755, #24512, #41009, .T. ) ;
#12995 = CARTESIAN_POINT ( 'NONE',  ( 14.28038400710302724, 10.53025766472732450, -34.79644660940672907 ) ) ;
#12997 = CARTESIAN_POINT ( 'NONE',  ( 72.05113849075890187, 0.9952277120684990264, -70.19587804460290670 ) ) ;
#12998 = CARTESIAN_POINT ( 'NONE',  ( 47.03254114365169869, 23.23399901970210379, -75.29848703692678669 ) ) ;
#12999 = CARTESIAN_POINT ( 'NONE',  ( 49.58793114173199967, -53.63459837187430423, -54.62161527680289907 ) ) ;
#13000 = CARTESIAN_POINT ( 'NONE',  ( 8.223201290577328848, -15.61599831009169925, -56.79233150823699816 ) ) ;
#13001 = CARTESIAN_POINT ( 'NONE',  ( 22.64777119364662994, -20.19351164595759585, -33.70249042454723565 ) ) ;
#13002 = CARTESIAN_POINT ( 'NONE',  ( 16.13393739769620083, -15.61618894467929941, -54.64999999999999858 ) ) ;
#13003 = CARTESIAN_POINT ( 'NONE',  ( 20.99564007730179327, -21.94233451394929091, -54.08400040345370741 ) ) ;
#13004 = ORIENTED_EDGE ( 'NONE', *, *, #6521, .T. ) ;
#13005 = CARTESIAN_POINT ( 'NONE',  ( 8.816398121954771128, -14.21607706117750070, -46.12751964827680240 ) ) ;
#13006 = CARTESIAN_POINT ( 'NONE',  ( 64.36679430080839381, 1.446932438105809737, -61.32315308161489753 ) ) ;
#13007 = EDGE_LOOP ( 'NONE', ( #29236, #13474, #18783, #16897, #32028 ) ) ;
#13008 = CARTESIAN_POINT ( 'NONE',  ( 84.37071824919731000, -43.44691537143197024, -47.23470636383878229 ) ) ;
#13009 = CARTESIAN_POINT ( 'NONE',  ( 60.98979597045209999, -45.65772911195310257, -47.70964152097329958 ) ) ;
#13010 = CARTESIAN_POINT ( 'NONE',  ( 8.761423512428116567, -12.64911493208424531, -80.91422037451174276 ) ) ;
#13011 = CARTESIAN_POINT ( 'NONE',  ( 44.97169576857614715, -43.53794996313975219, -5.328605099819570867 ) ) ;
#13013 = CARTESIAN_POINT ( 'NONE',  ( 11.27221920674516120, -21.94232376229728132, -78.50066392648321312 ) ) ;
#13012 = CARTESIAN_POINT ( 'NONE',  ( 44.07620675114476683, 8.728620045891982926, -66.29034569140392819 ) ) ;
#13014 = CARTESIAN_POINT ( 'NONE',  ( 50.97251369907100838, -50.96426704539258168, -76.14992187625421138 ) ) ;
#13015 = DIRECTION ( 'NONE',  ( 0.000000000000000000, 0.000000000000000000, -1.000000000000000000 ) ) ;
#13016 = VERTEX_POINT ( 'NONE', #16679 ) ;
#13017 = CARTESIAN_POINT ( 'NONE',  ( 84.02703262422839714, -44.63621804162450246, -47.45290575524859378 ) ) ;
#13018 = AXIS2_PLACEMENT_3D ( 'NONE', #28807, #16768, #44808 ) ;
#13019 = VERTEX_POINT ( 'NONE', #24000 ) ;
#13020 = VERTEX_POINT ( 'NONE', #28202 ) ;
#13021 = EDGE_CURVE ( 'NONE', #29987, #45454, #48663, .T. ) ;
#13022 = VERTEX_POINT ( 'NONE', #44722 ) ;
#13023 = CARTESIAN_POINT ( 'NONE',  ( 61.57010480345100234, -45.13191874552030214, -46.48558154903869166 ) ) ;
#13024 = CARTESIAN_POINT ( 'NONE',  ( 52.75990471363306256, -50.16877946593007209, -77.25922079919111241 ) ) ;
#13025 = EDGE_CURVE ( 'NONE', #621, #1956, #31781, .T. ) ;
#13026 = CARTESIAN_POINT ( 'NONE',  ( 76.40893147262282525, -10.52065843673467604, -12.83499039722492086 ) ) ;
#13027 = DIRECTION ( 'NONE',  ( 0.000000000000000000, 1.000000000000000000, 0.000000000000000000 ) ) ;
#13028 = EDGE_CURVE ( 'NONE', #42929, #28327, #38508, .T. ) ;
#13029 = VERTEX_POINT ( 'NONE', #50147 ) ;
#13030 = ORIENTED_EDGE ( 'NONE', *, *, #9593, .T. ) ;
#13031 = ADVANCED_FACE ( 'NONE', ( #34400 ), #26785, .F. ) ;
#13032 = FACE_BOUND ( 'NONE', #44140, .T. ) ;
#13033 = CARTESIAN_POINT ( 'NONE',  ( 56.83258906378680564, 19.07284248766010393, -52.72698304056530105 ) ) ;
#13034 = CARTESIAN_POINT ( 'NONE',  ( -15.76845656909109117, 6.818550277744307664, -48.78419541140080185 ) ) ;
#13035 = DIRECTION ( 'NONE',  ( -1.000000000000000000, 0.000000000000000000, 0.000000000000000000 ) ) ;
#13036 = CARTESIAN_POINT ( 'NONE',  ( 22.04686165056448743, -12.20822131928401788, -36.28615126516305622 ) ) ;
#13037 = DIRECTION ( 'NONE',  ( -1.000000000000000000, 0.000000000000000000, 0.000000000000000000 ) ) ;
#13038 = CARTESIAN_POINT ( 'NONE',  ( 12.72592096703445996, -9.703291609758796454, -53.78615459825274314 ) ) ;
#13039 = ORIENTED_EDGE ( 'NONE', *, *, #31387, .T. ) ;
#13040 = CARTESIAN_POINT ( 'NONE',  ( 8.784728771177240603, -63.11543068614769680, -46.67204636144870022 ) ) ;
#13041 = CARTESIAN_POINT ( 'NONE',  ( 53.23471707971139466, -50.42895756372370641, -77.19501644749119862 ) ) ;
#13042 = CARTESIAN_POINT ( 'NONE',  ( 12.89372882336123638, -8.399748356796177262, -81.15800232914327239 ) ) ;
#13043 = B_SPLINE_CURVE_WITH_KNOTS ( 'NONE', 3,
 ( #28723, #25814, #25560, #5680, #5931, #45511, #46030, #5420, #45768, #6193, #41566, #9358, #46293, #33432, #37632, #25305 ),
 .UNSPECIFIED., .F., .F.,
 ( 4, 2, 2, 2, 2, 2, 2, 4 ),
 ( 0.000000000000000000, 1.325233610615540014, 2.839786308461869968, 3.786381744615829881, 4.259679462692810503, 5.016955811615980032, 6.228597969893040265, 7.438175257738109281 ),
 .UNSPECIFIED. ) ;
#13044 = CARTESIAN_POINT ( 'NONE',  ( 14.15073023633489946, -32.59356659976219817, -35.02127583263639821 ) ) ;
#13045 = CIRCLE ( 'NONE', #17220, 25.00000000000000000 ) ;
#13046 = CARTESIAN_POINT ( 'NONE',  ( 9.144406050478650627, -19.18454979216170386, -60.86224082610989683 ) ) ;
#13047 = DIRECTION ( 'NONE',  ( 0.000000000000000000, 0.000000000000000000, 1.000000000000000000 ) ) ;
#13048 = ADVANCED_FACE ( 'NONE', ( #42290 ), #29237, .T. ) ;
#13049 = CARTESIAN_POINT ( 'NONE',  ( 42.99451563336680238, -43.12780611646349627, -4.474847206139059175 ) ) ;
#13050 = DIRECTION ( 'NONE',  ( 0.000000000000000000, 0.000000000000000000, 1.000000000000000000 ) ) ;
#13051 = CARTESIAN_POINT ( 'NONE',  ( 68.13393739769847457, -50.70395984887981200, -74.34354914830335304 ) ) ;
#13052 = CARTESIAN_POINT ( 'NONE',  ( 53.43679795862831128, 18.11049644000932446, -48.83615822496557257 ) ) ;
#13053 = CARTESIAN_POINT ( 'NONE',  ( 63.83188146504109284, 1.061276598305570085, -69.83322846870700573 ) ) ;
#13054 = TOROIDAL_SURFACE ( 'NONE', #20532, 12.50000000000000000, 1.000000000000000000 ) ;
#13055 = CYLINDRICAL_SURFACE ( 'NONE', #42730, 6.766999999999998572 ) ;
#13056 = CARTESIAN_POINT ( 'NONE',  ( 65.33368228454421001, 0.7990771883881800930, -17.55777972051419766 ) ) ;
#13057 = VERTEX_POINT ( 'NONE', #45247 ) ;
#13058 = CIRCLE ( 'NONE', #16392, 1.500000000000001332 ) ;
#13059 = CARTESIAN_POINT ( 'NONE',  ( 13.89821648398999798, -52.00201191962840142, -75.51495726157199329 ) ) ;
#13060 = CARTESIAN_POINT ( 'NONE',  ( 47.28596910495269867, -54.73079917377950210, -54.72607146539549916 ) ) ;
#13061 = CYLINDRICAL_SURFACE ( 'NONE', #3833, 3.000000000000000444 ) ;
#13062 = CARTESIAN_POINT ( 'NONE',  ( 8.222431652840050731, -15.61631456792169992, -70.50766849176299900 ) ) ;
#13063 = DIRECTION ( 'NONE',  ( 1.000000000000000000, 0.000000000000000000, 0.000000000000000000 ) ) ;
#13065 = ADVANCED_FACE ( 'NONE', ( #28984 ), #862, .T. ) ;
#13064 = CARTESIAN_POINT ( 'NONE',  ( 23.38426144667019813, -17.11500491999589713, -32.14999999999999858 ) ) ;
#13066 = CARTESIAN_POINT ( 'NONE',  ( 57.49550338311457409, 13.88380786636074404, -25.40179352645802169 ) ) ;
#13068 = ADVANCED_FACE ( 'NONE', ( #41052 ), #30216, .F. ) ;
#13067 = CARTESIAN_POINT ( 'NONE',  ( 47.73402016065340092, -54.47968219234450515, -54.93079182720929765 ) ) ;
#13070 = CARTESIAN_POINT ( 'NONE',  ( 13.58165717576775755, -51.39134915169243811, -22.62650423440272718 ) ) ;
#13069 = CARTESIAN_POINT ( 'NONE',  ( 14.16379049197029971, 19.89932140060919963, -22.70798727815419937 ) ) ;
#13071 = CIRCLE ( 'NONE', #42350, 2.576499999999998902 ) ;
#13072 = DIRECTION ( 'NONE',  ( 0.000000000000000000, 0.000000000000000000, 1.000000000000000000 ) ) ;
#13073 = CARTESIAN_POINT ( 'NONE',  ( 48.47402464779260356, 22.93984571062519962, -55.13672603318829601 ) ) ;
#13074 = VERTEX_POINT ( 'NONE', #26539 ) ;
#13075 = CARTESIAN_POINT ( 'NONE',  ( 21.77263034913930184, -11.37971624043620089, -60.64207792345899151 ) ) ;
#13076 = ORIENTED_EDGE ( 'NONE', *, *, #23253, .T. ) ;
#13077 = AXIS2_PLACEMENT_3D ( 'NONE', #47620, #35027, #46859 ) ;
#13078 = CARTESIAN_POINT ( 'NONE',  ( -20.36606260370279742, -15.61618894417470571, 10.84999999934590242 ) ) ;
#13079 = CARTESIAN_POINT ( 'NONE',  ( 61.31807987960689843, -45.64188066342459393, -47.72348187499480332 ) ) ;
#13080 = CARTESIAN_POINT ( 'NONE',  ( 0.4047412638265869833, -22.38804348994680282, -35.14999999999999858 ) ) ;
#13082 = CARTESIAN_POINT ( 'NONE',  ( 56.15977899178509603, 14.78509994814519857, -26.01523765823269940 ) ) ;
#13081 = CARTESIAN_POINT ( 'NONE',  ( 83.71081252132779582, 13.23966547877859945, -46.63777445865510174 ) ) ;
#13083 = CARTESIAN_POINT ( 'NONE',  ( 13.63580056716289945, -9.020594121423519240, -63.83757242544779587 ) ) ;
#13084 = CARTESIAN_POINT ( 'NONE',  ( -0.1295185695944119919, -31.87964491196989414, 4.943674098299959851 ) ) ;
#13085 = CARTESIAN_POINT ( 'NONE',  ( 56.79492093344569525, -45.11618894467940066, -15.79526079812830197 ) ) ;
#13086 = CARTESIAN_POINT ( 'NONE',  ( 17.21347160910339724, 21.88381105532300097, -76.14999999999999147 ) ) ;
#13087 = B_SPLINE_CURVE_WITH_KNOTS ( 'NONE', 3,
 ( #8381, #31684, #24072, #48735, #40092, #28797, #8636, #8128, #24331, #36655, #36397, #24588, #16493, #20161, #760, #48472 ),
 .UNSPECIFIED., .F., .F.,
 ( 4, 2, 2, 2, 2, 2, 2, 4 ),
 ( -1.480557251969420118, -1.467872963798670050, -1.112024972574749970, -0.8896199780598010864, -0.7784174808023259784, -0.6004934851903659387, -0.3158150922112299419, 0.000000000000000000 ),
 .UNSPECIFIED. ) ;
#13088 = VECTOR ( 'NONE', #24096, 1000.000000000000000 ) ;
#13089 = ORIENTED_EDGE ( 'NONE', *, *, #17482, .F. ) ;
#13090 = EDGE_LOOP ( 'NONE', ( #6032, #32709 ) ) ;
#13091 = CARTESIAN_POINT ( 'NONE',  ( 12.07292176418390106, -65.23870394393370020, -16.81897063589060082 ) ) ;
#13092 = CARTESIAN_POINT ( 'NONE',  ( 10.99330672749469962, 32.73200627569549681, -45.08259804521770064 ) ) ;
#13093 = CARTESIAN_POINT ( 'NONE',  ( 50.62425669123998517, 19.75411576426495586, 16.21999999999999886 ) ) ;
#13094 = ADVANCED_FACE ( 'NONE', ( #9354 ), #46756, .T. ) ;
#13095 = CARTESIAN_POINT ( 'NONE',  ( 49.41922605943800306, -52.95060041720219601, -52.58244047610669725 ) ) ;
#13096 = CARTESIAN_POINT ( 'NONE',  ( 24.04521450903870061, -15.61618868716203501, -63.50766715510244609 ) ) ;
#13097 = AXIS2_PLACEMENT_3D ( 'NONE', #36950, #16514, #24353 ) ;
#13098 = ORIENTED_EDGE ( 'NONE', *, *, #17177, .F. ) ;
#13099 = ADVANCED_FACE ( 'NONE', ( #6910, #34660, #18427, #42814, #13032, #6130 ), #17208, .T. ) ;
#13100 = CARTESIAN_POINT ( 'NONE',  ( 65.03603135455020379, -32.24781572988710110, -17.83403478221860183 ) ) ;
#13101 = LINE ( 'NONE', #1280, #44625 ) ;
#13102 = CARTESIAN_POINT ( 'NONE',  ( 68.13393739771649393, -29.16618894460431477, -82.15000000015528769 ) ) ;
#13103 = CARTESIAN_POINT ( 'NONE',  ( 14.13393739769640156, 6.292713355527309815, -54.64999999999999858 ) ) ;
#13104 = CARTESIAN_POINT ( 'NONE',  ( 50.29495137051839748, -49.91812883465070172, -76.14999999999999147 ) ) ;
#13105 = CARTESIAN_POINT ( 'NONE',  ( 8.222787824498201559, -15.61638397318239946, -64.79233150823698395 ) ) ;
#13106 = VERTEX_POINT ( 'NONE', #25300 ) ;
#13107 = CARTESIAN_POINT ( 'NONE',  ( 26.13393739769619728, -15.61618894467929941, -18.35000000000000142 ) ) ;
#13108 = DIRECTION ( 'NONE',  ( 0.000000000000000000, 0.000000000000000000, -1.000000000000000000 ) ) ;
#13109 = ORIENTED_EDGE ( 'NONE', *, *, #34427, .T. ) ;
#13110 = CARTESIAN_POINT ( 'NONE',  ( 63.63393739769619373, 21.88381105532059934, 16.35000000000000142 ) ) ;
#13111 = CARTESIAN_POINT ( 'NONE',  ( 28.63393739769620083, -15.61618894467929941, -1.149999999999999911 ) ) ;
#13112 = CARTESIAN_POINT ( 'NONE',  ( 9.924177576303440773, -10.19202054563570137, -79.02086993021879380 ) ) ;
#13113 = CARTESIAN_POINT ( 'NONE',  ( 26.13393739769619728, -28.89524513604070322, -84.65000000000000568 ) ) ;
#13114 = FACE_OUTER_BOUND ( 'NONE', #22685, .T. ) ;
#13115 = CARTESIAN_POINT ( 'NONE',  ( 47.24300521349800164, -54.11747037892259726, -75.51940560377390455 ) ) ;
#13116 = VERTEX_POINT ( 'NONE', #46493 ) ;
#13117 = CARTESIAN_POINT ( 'NONE',  ( 56.08436785131110014, 14.47011228136549832, -17.93020320136680112 ) ) ;
#13118 = CARTESIAN_POINT ( 'NONE',  ( 57.24718409717750234, -50.61618894895349996, -53.91456318682789828 ) ) ;
#13119 = CARTESIAN_POINT ( 'NONE',  ( 11.95218966202809874, -21.29558555530719843, -33.54920349970119986 ) ) ;
#13120 = DIRECTION ( 'NONE',  ( 1.000000000000000000, 0.000000000000000000, 0.000000000000000000 ) ) ;
#13121 = VECTOR ( 'NONE', #38266, 1000.000000000000000 ) ;
#13122 = ORIENTED_EDGE ( 'NONE', *, *, #41817, .T. ) ;
#13123 = CARTESIAN_POINT ( 'NONE',  ( 47.50285655629340198, 23.36688955440150295, -74.19742682671839873 ) ) ;
#13124 = CYLINDRICAL_SURFACE ( 'NONE', #44011, 7.910999999999997812 ) ;
#13125 = CARTESIAN_POINT ( 'NONE',  ( 28.74617114340210122, -4.636586115271110309, -34.66275921114419134 ) ) ;
#13126 = VECTOR ( 'NONE', #26835, 1000.000000000000000 ) ;
#13127 = EDGE_CURVE ( 'NONE', #26692, #13682, #26821, .T. ) ;
#13128 = DIRECTION ( 'NONE',  ( 0.000000000000000000, 0.000000000000000000, -1.000000000000000000 ) ) ;
#13130 = EDGE_CURVE ( 'NONE', #44442, #51033, #46076, .T. ) ;
#13129 = CARTESIAN_POINT ( 'NONE',  ( 68.13393739806078031, -1.166188945131049870, -65.65000000072619457 ) ) ;
#13131 = CARTESIAN_POINT ( 'NONE',  ( 73.10258273731270151, 1.278021359705819870, -68.66984894295178776 ) ) ;
#13132 = CARTESIAN_POINT ( 'NONE',  ( 30.61153946640385826, -35.65524129201374848, -84.61437977358458795 ) ) ;
#13133 = CARTESIAN_POINT ( 'NONE',  ( 16.13393739769620083, -15.61618894467929941, -34.64999999999999858 ) ) ;
#13134 = CARTESIAN_POINT ( 'NONE',  ( -12.01951210174429896, -55.39328561125270056, -51.29522465964590339 ) ) ;
#13135 = EDGE_CURVE ( 'NONE', #35688, #14446, #42553, .T. ) ;
#13136 = ORIENTED_EDGE ( 'NONE', *, *, #35368, .T. ) ;
#13137 = CARTESIAN_POINT ( 'NONE',  ( 53.43246109065159999, -49.34667644580379431, -48.81566079192110408 ) ) ;
#13138 = CARTESIAN_POINT ( 'NONE',  ( 61.66984040017980107, -45.11833727456389198, -28.15134406664559563 ) ) ;
#13139 = CARTESIAN_POINT ( 'NONE',  ( 47.67211062985429493, -54.52182009381669303, -55.16489596303849652 ) ) ;
#13140 = CARTESIAN_POINT ( 'NONE',  ( 13.58375825965479855, 19.57881046872019937, -21.57335430205159810 ) ) ;
#13141 = CARTESIAN_POINT ( 'NONE',  ( 56.14448110115399970, 14.68078269655329926, -25.90882037036080021 ) ) ;
#13142 = CARTESIAN_POINT ( 'NONE',  ( 22.47358672090329890, -12.52528092440720009, -32.30843786212719948 ) ) ;
#13143 = CARTESIAN_POINT ( 'NONE',  ( 51.40462280232849679, 19.31602561253640005, -76.23573550552218592 ) ) ;
#13144 = CARTESIAN_POINT ( 'NONE',  ( 52.76130411716530233, 18.47365434860499889, -48.70176833931630256 ) ) ;
#13145 = CARTESIAN_POINT ( 'NONE',  ( 71.18923915728029783, 1.331842543267529821, -70.50106597067950531 ) ) ;
#13146 = CARTESIAN_POINT ( 'NONE',  ( 16.13393739769620083, -15.61618894467929941, -23.74958330439410048 ) ) ;
#13147 = CYLINDRICAL_SURFACE ( 'NONE', #3900, 6.766999999999998572 ) ;
#13148 = ORIENTED_EDGE ( 'NONE', *, *, #45775, .F. ) ;
#13149 = CARTESIAN_POINT ( 'NONE',  ( 23.51172799066640096, -14.57941495549949984, -77.02290276308829675 ) ) ;
#13150 = EDGE_LOOP ( 'NONE', ( #17622, #49241, #11478, #40554, #11468 ) ) ;
#13151 = CARTESIAN_POINT ( 'NONE',  ( 72.79634974714259954, 1.384378348444520013, -68.73316704115080711 ) ) ;
#13152 = CARTESIAN_POINT ( 'NONE',  ( 47.46188864440789956, -54.61821625934059909, -54.80977015378280015 ) ) ;
#13153 = CARTESIAN_POINT ( 'NONE',  ( 24.04166718631601896, -15.38336571792064866, -49.78296408212683133 ) ) ;
#13154 = CARTESIAN_POINT ( 'NONE',  ( 73.22759735627531086, 0.9947083095259759977, -62.49453424214399888 ) ) ;
#13155 = DIRECTION ( 'NONE',  ( -0.8660254037844387076, 0.4999999999999998890, 1.942890293094024439E-16 ) ) ;
#13156 = CARTESIAN_POINT ( 'NONE',  ( 53.02240706027900075, 18.32760744209570092, -48.78672998508179859 ) ) ;
#13157 = CARTESIAN_POINT ( 'NONE',  ( 51.50424210664085223, -50.10650823822277289, 16.21999999999999886 ) ) ;
#13158 = CARTESIAN_POINT ( 'NONE',  ( 71.77241571698009182, 1.241979851175089911, -60.99005311882309854 ) ) ;
#13159 = AXIS2_PLACEMENT_3D ( 'NONE', #18578, #9944, #30619 ) ;
#13160 = CARTESIAN_POINT ( 'NONE',  ( 12.14969441541569672, -22.52864909168088658, -72.17427940389318053 ) ) ;
#13161 = B_SPLINE_CURVE_WITH_KNOTS ( 'NONE', 3,
 ( #23010, #6801, #47158, #51843, #15686, #3124, #22753, #34813, #27726, #19093 ),
 .UNSPECIFIED., .F., .F.,
 ( 4, 2, 2, 2, 4 ),
 ( -0.1799215976186380184, -0.1795414484423739909, -0.1664059944893910015, -0.1383522341550179890, -0.1329710036334196266 ),
 .UNSPECIFIED. ) ;
#13162 = EDGE_CURVE ( 'NONE', #3494, #12469, #23990, .T. ) ;
#13163 = CARTESIAN_POINT ( 'NONE',  ( 65.09331375576360301, 1.276058558775509999, -70.60879112794539481 ) ) ;
#13164 = ORIENTED_EDGE ( 'NONE', *, *, #39535, .T. ) ;
#13165 = ORIENTED_EDGE ( 'NONE', *, *, #15560, .F. ) ;
#13166 = CARTESIAN_POINT ( 'NONE',  ( 8.956863767676178867, -63.15483629195879445, -46.63369080061400496 ) ) ;
#13167 = CARTESIAN_POINT ( 'NONE',  ( -4.849986043992698725, -15.61618894467930119, 6.789625226207629538 ) ) ;
#13168 = ORIENTED_EDGE ( 'NONE', *, *, #12229, .T. ) ;
#13169 = CARTESIAN_POINT ( 'NONE',  ( 22.90150794149753111, -15.57801490272766110, -72.84538554144812394 ) ) ;
#13170 = CARTESIAN_POINT ( 'NONE',  ( 16.13393739769620083, -15.61618894467929941, -34.64999999999999858 ) ) ;
#13171 = CARTESIAN_POINT ( 'NONE',  ( 56.13223116304230587, 19.60886586524600261, -74.69896703041874275 ) ) ;
#13172 = CARTESIAN_POINT ( 'NONE',  ( 52.30043100026959735, 19.46767200232369888, -76.35983844399039810 ) ) ;
#13173 = ORIENTED_EDGE ( 'NONE', *, *, #3672, .F. ) ;
#13174 = FACE_OUTER_BOUND ( 'NONE', #8826, .T. ) ;
#13175 = CARTESIAN_POINT ( 'NONE',  ( 63.88393739769619373, 11.88381105532070059, -61.44999999999999574 ) ) ;
#13176 = CIRCLE ( 'NONE', #8135, 18.00000000000000000 ) ;
#13177 = CARTESIAN_POINT ( 'NONE',  ( 18.20456276067269386, -7.911073408245188787, -43.37570542978183852 ) ) ;
#13178 = CARTESIAN_POINT ( 'NONE',  ( 14.28670337130830070, -23.65176275789830029, -56.36425564602360083 ) ) ;
#13179 = B_SPLINE_CURVE_WITH_KNOTS ( 'NONE', 3,
 ( #47777, #11883, #27073, #27841, #43841, #38632, #10850, #19212, #22872, #34674, #27328, #50933, #50674, #14772, #11365, #30741 ),
 .UNSPECIFIED., .F., .F.,
 ( 4, 2, 2, 2, 2, 2, 2, 4 ),
 ( -8.523275000000000432E-16, 0.07216186899280999101, 0.1546325764131659952, 0.2061767685508879844, 0.2319488646197490067, 0.2731842183299269533, 0.3391607842662109906, 0.4123535371017769680 ),
 .UNSPECIFIED. ) ;
#13180 = CARTESIAN_POINT ( 'NONE',  ( 22.90088944531260395, -15.58987521438611346, -56.45158775362976655 ) ) ;
#13181 = CARTESIAN_POINT ( 'NONE',  ( 53.65235395033388244, 20.09310193608997963, -75.57543365061850693 ) ) ;
#13182 = ORIENTED_EDGE ( 'NONE', *, *, #27452, .T. ) ;
#13183 = LINE ( 'NONE', #48545, #6644 ) ;
#13184 = CARTESIAN_POINT ( 'NONE',  ( 23.25907355585459868, -17.79314290212749938, -40.32704379009269502 ) ) ;
#13185 = LINE ( 'NONE', #20745, #28741 ) ;
#13186 = CARTESIAN_POINT ( 'NONE',  ( 14.77000656121960098, 21.15196775986840194, -76.02269426304029309 ) ) ;
#13187 = CARTESIAN_POINT ( 'NONE',  ( 51.80594958079759493, 17.96077681129019865, -77.05312856993060677 ) ) ;
#13188 = CARTESIAN_POINT ( 'NONE',  ( 84.12790934798559306, -43.97578464600089632, -46.91176635807759254 ) ) ;
#13189 = CARTESIAN_POINT ( 'NONE',  ( 22.03008559642460185, -9.852669435941031395, -49.26128910974178865 ) ) ;
#13190 = VERTEX_POINT ( 'NONE', #31236 ) ;
#13191 = CARTESIAN_POINT ( 'NONE',  ( 52.93948662983430609, -49.53590707237739821, -27.64880802112100255 ) ) ;
#13192 = EDGE_CURVE ( 'NONE', #25606, #27172, #49446, .T. ) ;
#13193 = CARTESIAN_POINT ( 'NONE',  ( 16.33938386690050137, -51.09625719537829980, -20.40297663956910057 ) ) ;
#13194 = DIRECTION ( 'NONE',  ( 0.000000000000000000, 0.000000000000000000, -1.000000000000000000 ) ) ;
#13195 = CARTESIAN_POINT ( 'NONE',  ( 21.51824785155721997, -11.06077896193409060, -70.62366323747509966 ) ) ;
#13196 = CARTESIAN_POINT ( 'NONE',  ( 16.13393739769620083, -15.61618894467929941, 14.34999999999999964 ) ) ;
#13197 = ORIENTED_EDGE ( 'NONE', *, *, #46823, .F. ) ;
#13198 = CARTESIAN_POINT ( 'NONE',  ( -4.005781160639729777, -47.98584768802999889, -5.016607454399269805 ) ) ;
#13199 = CARTESIAN_POINT ( 'NONE',  ( 47.21267495741800246, 23.55157179986399996, -54.62953672193049925 ) ) ;
#13200 = CIRCLE ( 'NONE', #28232, 36.55167969755429880 ) ;
#13201 = CARTESIAN_POINT ( 'NONE',  ( 20.63393739769599833, 10.38381105532070059, -54.64999999999999858 ) ) ;
#13202 = CARTESIAN_POINT ( 'NONE',  ( 63.41989057163110743, 1.369544300367010026, -62.51645495968789845 ) ) ;
#13203 = CARTESIAN_POINT ( 'NONE',  ( 11.88601302014030026, 34.20290939426369903, -17.88642737458170018 ) ) ;
#13204 = DIRECTION ( 'NONE',  ( 0.000000000000000000, 0.000000000000000000, -1.000000000000000000 ) ) ;
#13205 = CARTESIAN_POINT ( 'NONE',  ( 53.11114665040049942, 18.28111428451730092, -48.80212166739749335 ) ) ;
#13206 = CARTESIAN_POINT ( 'NONE',  ( 0.4047412638265869833, -22.38804348994680282, -35.14999999999999858 ) ) ;
#13207 = CARTESIAN_POINT ( 'NONE',  ( 60.26929283095270051, -45.78778679473020219, -47.49574889169500125 ) ) ;
#13208 = CARTESIAN_POINT ( 'NONE',  ( 21.43677159062993809, -19.88198936106610759, -66.66855547569113583 ) ) ;
#13209 = CARTESIAN_POINT ( 'NONE',  ( 52.69990148663700325, 21.03144630651199876, -53.73602009713189886 ) ) ;
#13210 = CARTESIAN_POINT ( 'NONE',  ( 17.90516118349662023, -22.20706887017997033, -60.86950335209443352 ) ) ;
#13211 = FACE_OUTER_BOUND ( 'NONE', #9605, .T. ) ;
#13212 = ORIENTED_EDGE ( 'NONE', *, *, #5628, .F. ) ;
#13213 = DIRECTION ( 'NONE',  ( 1.000000000000000000, 0.000000000000000000, 0.000000000000000000 ) ) ;
#13214 = CARTESIAN_POINT ( 'NONE',  ( 8.962435484615378201, 31.95416093520460521, -46.63293154189879886 ) ) ;
#13215 = CARTESIAN_POINT ( 'NONE',  ( 41.99202299628319679, 13.65299255882769991, -5.712667844576049703 ) ) ;
#13216 = CARTESIAN_POINT ( 'NONE',  ( 67.93181682611671590, -30.30591887840110132, -17.84857444314360109 ) ) ;
#13217 = ORIENTED_EDGE ( 'NONE', *, *, #33459, .T. ) ;
#13218 = EDGE_CURVE ( 'NONE', #37955, #42552, #35912, .T. ) ;
#13219 = CARTESIAN_POINT ( 'NONE',  ( 18.30878848283549942, 19.99149262732870014, -74.56034069004439857 ) ) ;
#13220 = ORIENTED_EDGE ( 'NONE', *, *, #1639, .F. ) ;
#13221 = ORIENTED_EDGE ( 'NONE', *, *, #7219, .T. ) ;
#13222 = DIRECTION ( 'NONE',  ( 0.000000000000000000, 0.000000000000000000, 1.000000000000000000 ) ) ;
#13223 = EDGE_CURVE ( 'NONE', #28134, #30405, #11594, .T. ) ;
#13224 = ORIENTED_EDGE ( 'NONE', *, *, #24673, .T. ) ;
#13225 = CARTESIAN_POINT ( 'NONE',  ( 11.93682371713649992, -65.18248445933780033, -46.46134574452209876 ) ) ;
#13226 = CARTESIAN_POINT ( 'NONE',  ( 57.44440056792399929, -45.44038579893220486, -26.07919784721820022 ) ) ;
#13227 = CARTESIAN_POINT ( 'NONE',  ( 23.30658763286460200, -17.14219254102309975, -81.23899999999999011 ) ) ;
#13228 = CARTESIAN_POINT ( 'NONE',  ( 61.68987241420879997, 13.88502446954749914, -46.37201345370000638 ) ) ;
#13229 = CARTESIAN_POINT ( 'NONE',  ( 72.48038400710301232, 1.530257664727401545, -65.65000000000000568 ) ) ;
#13230 = ORIENTED_EDGE ( 'NONE', *, *, #27836, .F. ) ;
#13231 = DIRECTION ( 'NONE',  ( 0.000000000000000000, 0.000000000000000000, -1.000000000000000000 ) ) ;
#13232 = ORIENTED_EDGE ( 'NONE', *, *, #37514, .T. ) ;
#13233 = CARTESIAN_POINT ( 'NONE',  ( 49.49077763376009642, -45.96749055206419854, -11.95218223477760056 ) ) ;
#13234 = CARTESIAN_POINT ( 'NONE',  ( 23.93272017389292827, -16.99025993377153654, -33.84783788291247220 ) ) ;
#13235 = CARTESIAN_POINT ( 'NONE',  ( 16.13393739769620083, -15.61618894467929941, -7.349999999999999645 ) ) ;
#13236 = EDGE_LOOP ( 'NONE', ( #48602, #16676, #26795, #25747 ) ) ;
#13237 = CARTESIAN_POINT ( 'NONE',  ( 72.74776047649520194, 1.391252479931859964, -62.52735703481241103 ) ) ;
#13238 = CARTESIAN_POINT ( 'NONE',  ( 46.35275103504449845, -52.90993241930539881, -76.14999999999999147 ) ) ;
#13239 = CARTESIAN_POINT ( 'NONE',  ( 60.65419404070010501, 14.53878550406569836, -47.75595165931559904 ) ) ;
#13240 = STYLED_ITEM ( 'NONE', ( #462 ), #44299 ) ;
#13241 = CARTESIAN_POINT ( 'NONE',  ( 51.83641662704179964, 14.98333576533859990, -13.79431318377310056 ) ) ;
#13242 = AXIS2_PLACEMENT_3D ( 'NONE', #29162, #28380, #45160 ) ;
#13243 = CARTESIAN_POINT ( 'NONE',  ( 24.04513930477782679, -15.61618913701998146, -67.79233342760500136 ) ) ;
#13244 = CARTESIAN_POINT ( 'NONE',  ( -7.993718939281059477, 13.74763319926180039, -5.173449967684150330 ) ) ;
#13245 = CARTESIAN_POINT ( 'NONE',  ( 22.18801361179549758, -19.23429899943539922, -63.01864585536749530 ) ) ;
#13246 = CARTESIAN_POINT ( 'NONE',  ( 59.69861616638479518, 13.89146436216049807, -26.11287264892089865 ) ) ;
#13247 = CARTESIAN_POINT ( 'NONE',  ( 20.29176081427040046, -8.960420572825411156, -72.96524338830390377 ) ) ;
#13248 = EDGE_LOOP ( 'NONE', ( #24357, #3991, #12065, #8107, #41363, #5232 ) ) ;
#13249 = CARTESIAN_POINT ( 'NONE',  ( 54.37486050126969417, 17.76197798406979800, -48.98148910212459839 ) ) ;
#13250 = EDGE_CURVE ( 'NONE', #35178, #7027, #41050, .T. ) ;
#13251 = CARTESIAN_POINT ( 'NONE',  ( 73.01385068780759013, 0.9098571636355720083, -62.15909090909049439 ) ) ;
#13252 = CARTESIAN_POINT ( 'NONE',  ( 28.13393739769619373, -22.54439217495488279, -35.01561944896765510 ) ) ;
#13253 = CYLINDRICAL_SURFACE ( 'NONE', #23764, 0.4999999999999983347 ) ;
#13254 = CARTESIAN_POINT ( 'NONE',  ( 82.45639937995038338, -45.09267748618990623, -46.38982090304390482 ) ) ;
#13255 = CARTESIAN_POINT ( 'NONE',  ( 20.11802031537004609, -8.703636685625692593, -59.45903915183253474 ) ) ;
#13256 = CARTESIAN_POINT ( 'NONE',  ( 49.22434610110619246, -53.62684526786699735, -54.29818755095050165 ) ) ;
#13257 = CARTESIAN_POINT ( 'NONE',  ( 51.35265160182996880, -31.92979185925464591, -17.41534043387646236 ) ) ;
#13258 = CARTESIAN_POINT ( 'NONE',  ( 9.459753751615320283, -19.88776835366272877, -34.32646034695605408 ) ) ;
#13259 = CARTESIAN_POINT ( 'NONE',  ( 18.66237950319839811, -51.43164378700720363, -74.36773579015570590 ) ) ;
#13260 = CARTESIAN_POINT ( 'NONE',  ( 55.89576372857870012, -50.73744799429999830, -52.91533302817010309 ) ) ;
#13261 = VERTEX_POINT ( 'NONE', #28078 ) ;
#13262 = CARTESIAN_POINT ( 'NONE',  ( 14.66312945716499883, -8.312531070681380641, -48.50408758018539146 ) ) ;
#13263 = CARTESIAN_POINT ( 'NONE',  ( 64.15658392863279857, 1.099201050715910011, -61.16377310064390116 ) ) ;
#13264 = VERTEX_POINT ( 'NONE', #43068 ) ;
#13265 = CARTESIAN_POINT ( 'NONE',  ( 60.70915627887830368, -45.63243799255800326, -47.54512464986149922 ) ) ;
#13266 = CARTESIAN_POINT ( 'NONE',  ( 23.32430482491550094, 18.10127401595489971, -34.64999999999999858 ) ) ;
#13267 = CIRCLE ( 'NONE', #671, 6.000000000000005329 ) ;
#13268 = CARTESIAN_POINT ( 'NONE',  ( 13.04450223504579931, 18.79195994071550047, -21.04428001324339803 ) ) ;
#13270 = CARTESIAN_POINT ( 'NONE',  ( 68.13393739769618662, -2.032350560841069687, -29.09832030244572820 ) ) ;
#13269 = CARTESIAN_POINT ( 'NONE',  ( 43.99065823752038540, 8.721581408738890318, -66.70470347308750547 ) ) ;
#13271 = CARTESIAN_POINT ( 'NONE',  ( 51.55044215929650164, -51.25128868776180013, -76.08578283986020097 ) ) ;
#13272 = CYLINDRICAL_SURFACE ( 'NONE', #32782, 20.00000000000000355 ) ;
#13273 = ORIENTED_EDGE ( 'NONE', *, *, #27106, .T. ) ;
#13274 = ORIENTED_EDGE ( 'NONE', *, *, #38270, .F. ) ;
#13275 = ORIENTED_EDGE ( 'NONE', *, *, #29680, .T. ) ;
#13276 = EDGE_CURVE ( 'NONE', #43378, #27228, #10944, .T. ) ;
#13277 = VERTEX_POINT ( 'NONE', #19459 ) ;
#13278 = CARTESIAN_POINT ( 'NONE',  ( 61.68987299561999293, -45.11740230825230213, -46.37193444313120239 ) ) ;
#13279 = DIRECTION ( 'NONE',  ( 0.000000000000000000, 0.000000000000000000, 1.000000000000000000 ) ) ;
#13280 =( BOUNDED_CURVE ( )  B_SPLINE_CURVE ( 3, ( #6615, #42005, #6103, #14734 ),
 .UNSPECIFIED., .F., .T. ) 
 B_SPLINE_CURVE_WITH_KNOTS ( ( 4, 4 ),
 ( 0.5363495246926816007, 0.7853981633974366217 ),
 .UNSPECIFIED. ) 
 CURVE ( )  GEOMETRIC_REPRESENTATION_ITEM ( )  RATIONAL_B_SPLINE_CURVE ( ( 1.000000000000000000, 0.9948379068877994946, 0.9948379068877994946, 1.000000000000000000 ) ) 
 REPRESENTATION_ITEM ( '' )  );
#13281 = DIRECTION ( 'NONE',  ( 1.000000000000000000, 0.000000000000000000, 0.000000000000000000 ) ) ;
#13282 = ORIENTED_EDGE ( 'NONE', *, *, #2966, .T. ) ;
#13283 = VERTEX_POINT ( 'NONE', #35444 ) ;
#13284 = CARTESIAN_POINT ( 'NONE',  ( 11.47911758231620993, 34.07625331222116927, -22.67538628410606805 ) ) ;
#13285 = ORIENTED_EDGE ( 'NONE', *, *, #2844, .F. ) ;
#13286 = CARTESIAN_POINT ( 'NONE',  ( 8.222281512103441159, -15.61614627842319969, -76.50766849176299900 ) ) ;
#13287 = DIRECTION ( 'NONE',  ( 0.000000000000000000, 0.000000000000000000, 1.000000000000000000 ) ) ;
#13288 = CARTESIAN_POINT ( 'NONE',  ( 10.20031836580031914, -11.80374558652071393, -66.02896523580054122 ) ) ;
#13289 = EDGE_LOOP ( 'NONE', ( #35948, #10586, #48191, #32108, #35436 ) ) ;
#13290 = DIRECTION ( 'NONE',  ( 1.562192859871379910E-09, -1.089021445294679944E-09, 1.000000000000000000 ) ) ;
#13291 = CARTESIAN_POINT ( 'NONE',  ( 52.90771576829140344, -50.68587721302630200, -76.48668075183719850 ) ) ;
#13292 = CARTESIAN_POINT ( 'NONE',  ( 9.367442997458502063, -15.61610373232760018, -47.45282021618999835 ) ) ;
#13293 = CARTESIAN_POINT ( 'NONE',  ( 60.39237854593780241, 14.46627288824030089, -47.20777951346740053 ) ) ;
#13294 = CARTESIAN_POINT ( 'NONE',  ( 14.27330375828070075, -7.992227372671099950, -59.43630006696489687 ) ) ;
#13295 = CARTESIAN_POINT ( 'NONE',  ( 57.24929578595760660, -52.61618894467940066, -74.14999999999999147 ) ) ;
#13296 = CARTESIAN_POINT ( 'NONE',  ( 41.21726848154669653, 13.59251350426850102, -5.423354614126240314 ) ) ;
#13297 = CARTESIAN_POINT ( 'NONE',  ( 42.05805429857900180, -44.46257822744319554, -5.167112339002620125 ) ) ;
#13298 = CARTESIAN_POINT ( 'NONE',  ( 0.8851803632885527628, -42.94237738927703418, -20.85710678118654471 ) ) ;
#13299 = DIRECTION ( 'NONE',  ( -1.000000000000000000, 0.000000000000000000, 0.000000000000000000 ) ) ;
#13300 = AXIS2_PLACEMENT_3D ( 'NONE', #6139, #29701, #2456 ) ;
#13301 = CARTESIAN_POINT ( 'NONE',  ( 64.36988470191930389, 1.396287116999079814, -70.06934168479099867 ) ) ;
#13302 = CARTESIAN_POINT ( 'NONE',  ( 68.13393739769618662, -0.1661889446793529956, -65.65000000000000568 ) ) ;
#13303 = VECTOR ( 'NONE', #13348, 1000.000000000000000 ) ;
#13304 = CARTESIAN_POINT ( 'NONE',  ( 66.36401773903131129, -0.6008215590598360301, -16.96146227724700495 ) ) ;
#13305 = ORIENTED_EDGE ( 'NONE', *, *, #43080, .T. ) ;
#13306 = CARTESIAN_POINT ( 'NONE',  ( 14.00960937400600059, -52.10962414010410271, -75.64877291256318870 ) ) ;
#13307 = EDGE_CURVE ( 'NONE', #26370, #45497, #6479, .T. ) ;
#13308 = CARTESIAN_POINT ( 'NONE',  ( 47.18324198357289845, -54.80726809202429450, -54.61058319554170026 ) ) ;
#13309 = CARTESIAN_POINT ( 'NONE',  ( 8.839329447558961661, 32.18893842047796738, -46.67772192970179645 ) ) ;
#13310 = CYLINDRICAL_SURFACE ( 'NONE', #22116, 2.999999999999999112 ) ;
#13311 = EDGE_CURVE ( 'NONE', #36774, #14211, #3748, .T. ) ;
#13312 = CARTESIAN_POINT ( 'NONE',  ( 61.25373297964098640, -45.57865225153049948, -47.65126977280955600 ) ) ;
#13313 = CARTESIAN_POINT ( 'NONE',  ( 22.45778058535230315, -19.86412798156090176, -32.14999999999999858 ) ) ;
#13314 = CARTESIAN_POINT ( 'NONE',  ( 55.91595717589669334, -45.90465048314089103, -17.93019253464870033 ) ) ;
#13315 = EDGE_CURVE ( 'NONE', #50462, #26977, #6640, .T. ) ;
#13316 = CARTESIAN_POINT ( 'NONE',  ( 10.78192289013670013, 33.70626262526499772, -17.70651626560779945 ) ) ;
#13318 = DIRECTION ( 'NONE',  ( 0.000000000000000000, 1.000000000000000000, 0.000000000000000000 ) ) ;
#13317 = DIRECTION ( 'NONE',  ( 0.000000000000000000, 0.000000000000000000, -1.000000000000000000 ) ) ;
#13319 = DIRECTION ( 'NONE',  ( 0.000000000000000000, 1.000000000000000000, 0.000000000000000000 ) ) ;
#13320 = CARTESIAN_POINT ( 'NONE',  ( 48.61563435628440288, 22.86626419475689787, -55.02610085215599867 ) ) ;
#13321 = ORIENTED_EDGE ( 'NONE', *, *, #23278, .F. ) ;
#13322 = CARTESIAN_POINT ( 'NONE',  ( 11.01510582436389818, -10.76437253241610037, -68.08865744343920312 ) ) ;
#13323 = ORIENTED_EDGE ( 'NONE', *, *, #27679, .F. ) ;
#13324 = CARTESIAN_POINT ( 'NONE',  ( 29.52882095054619782, 21.88381105532300097, -74.14999999999999147 ) ) ;
#13325 = CARTESIAN_POINT ( 'NONE',  ( 19.13393739769623991, -49.61618894467932250, -35.01561944896766221 ) ) ;
#13327 = EDGE_CURVE ( 'NONE', #38150, #32888, #24655, .T. ) ;
#13326 = DIRECTION ( 'NONE',  ( -0.6643794812577346054, -0.7473954140103507005, 3.025357742103549206E-15 ) ) ;
#13329 = CARTESIAN_POINT ( 'NONE',  ( 52.66238325897660388, 18.53796739974139740, -28.07429613766819898 ) ) ;
#13328 = CARTESIAN_POINT ( 'NONE',  ( 83.20652121431659509, 13.83669318944459903, -47.10047235024320145 ) ) ;
#13330 = CARTESIAN_POINT ( 'NONE',  ( 22.51615883520530303, -12.61455468660830093, -64.31288601182949094 ) ) ;
#13331 = CARTESIAN_POINT ( 'NONE',  ( 8.222496981792570381, -15.61604333543320067, -34.50766849176299900 ) ) ;
#13332 = CARTESIAN_POINT ( 'NONE',  ( 57.41961282341689810, -45.11618894467940066, -17.93020390954330168 ) ) ;
#13333 = FACE_OUTER_BOUND ( 'NONE', #35645, .T. ) ;
#13334 = EDGE_LOOP ( 'NONE', ( #1514, #12072, #6822, #6290 ) ) ;
#13335 = EDGE_CURVE ( 'NONE', #34463, #48131, #2550, .T. ) ;
#13336 = ORIENTED_EDGE ( 'NONE', *, *, #43304, .F. ) ;
#13337 = CARTESIAN_POINT ( 'NONE',  ( 11.78008937360669961, -65.13730895740229698, -16.70885295319099839 ) ) ;
#13338 = CARTESIAN_POINT ( 'NONE',  ( 11.52264128144989996, 33.52070032263379318, -45.36557337499360187 ) ) ;
#13339 = CARTESIAN_POINT ( 'NONE',  ( 0.08375394646315241498, 19.63944928676770019, -34.70982966457259522 ) ) ;
#13340 = AXIS2_PLACEMENT_3D ( 'NONE', #27317, #7418, #24129 ) ;
#13341 = CARTESIAN_POINT ( 'NONE',  ( 47.83911115347329712, -54.64680175183159605, -55.43863697538600377 ) ) ;
#13342 = CARTESIAN_POINT ( 'NONE',  ( 0.3209249304026170480, -26.47788675693900018, -34.64999999999999858 ) ) ;
#13343 = AXIS2_PLACEMENT_3D ( 'NONE', #32076, #28153, #44157 ) ;
#13344 = ORIENTED_EDGE ( 'NONE', *, *, #25757, .F. ) ;
#13345 = CARTESIAN_POINT ( 'NONE',  ( -19.05274139337909745, -33.00040335413840609, -51.45066150993559262 ) ) ;
#13346 = DIRECTION ( 'NONE',  ( 0.000000000000000000, 0.000000000000000000, 1.000000000000000000 ) ) ;
#13347 = CARTESIAN_POINT ( 'NONE',  ( 14.06323637774060842, -23.32128329111424492, -60.09102755594223311 ) ) ;
#13348 = DIRECTION ( 'NONE',  ( 0.6803061734058448717, 0.000000000000000000, -0.7329280390501489162 ) ) ;
#13349 = FACE_OUTER_BOUND ( 'NONE', #8763, .T. ) ;
#13350 = CARTESIAN_POINT ( 'NONE',  ( 1.027904703268279984, -42.68661147989060112, -20.15000000000000213 ) ) ;
#13351 = ORIENTED_EDGE ( 'NONE', *, *, #48674, .F. ) ;
#13352 = CYLINDRICAL_SURFACE ( 'NONE', #20750, 3.500000000000003109 ) ;
#13353 = CARTESIAN_POINT ( 'NONE',  ( 16.13393739769620083, -15.61618894467929941, -28.45282021618999835 ) ) ;
#13354 = ORIENTED_EDGE ( 'NONE', *, *, #37747, .T. ) ;
#13355 = LINE ( 'NONE', #17535, #27682 ) ;
#13356 = CARTESIAN_POINT ( 'NONE',  ( 50.20834198929310332, -46.19201399287660337, -12.60657503851190064 ) ) ;
#13357 = ADVANCED_FACE ( 'NONE', ( #41188 ), #42625, .F. ) ;
#13358 = CARTESIAN_POINT ( 'NONE',  ( 9.695727428901339096, -20.10352073914850379, -32.81873922958869372 ) ) ;
#13359 = CARTESIAN_POINT ( 'NONE',  ( 13.77296168685579936, -51.29346510576050377, -23.09857317148069811 ) ) ;
#13360 = CARTESIAN_POINT ( 'NONE',  ( 55.60062637994129631, 19.57032068857209950, -75.31308341371119752 ) ) ;
#13361 = CARTESIAN_POINT ( 'NONE',  ( 46.35275103504449845, -52.90993241930539881, -76.14999999999999147 ) ) ;
#13362 = VERTEX_POINT ( 'NONE', #40666 ) ;
#13363 = CARTESIAN_POINT ( 'NONE',  ( 54.70309273011209683, 14.87826559838519991, -15.84802628241609845 ) ) ;
#13364 = CARTESIAN_POINT ( 'NONE',  ( 57.19888501910689627, -50.26827476893720359, -52.76365438030089194 ) ) ;
#13365 = CARTESIAN_POINT ( 'NONE',  ( 12.67868222463649808, -21.76466606210399846, -37.51015005288219584 ) ) ;
#13366 = CARTESIAN_POINT ( 'NONE',  ( 46.27983543144653567, 22.91052256907554607, 10.84999999999999964 ) ) ;
#13367 = ORIENTED_EDGE ( 'NONE', *, *, #22674, .F. ) ;
#13368 = CARTESIAN_POINT ( 'NONE',  ( 47.11288066194880031, 22.79292711817570094, -75.65359354181590845 ) ) ;
#13369 = CARTESIAN_POINT ( 'NONE',  ( 65.03067915409710054, 1.194703186106690129, -60.63553603340079690 ) ) ;
#13370 = CONICAL_SURFACE ( 'NONE', #42664, 36.50000000000000711, 0.1651486774146265213 ) ;
#13371 = CARTESIAN_POINT ( 'NONE',  ( 60.79255070202935940, -45.73115554882355838, -47.75226182717861434 ) ) ;
#13372 = AXIS2_PLACEMENT_3D ( 'NONE', #28535, #33242, #40597 ) ;
#13373 = CARTESIAN_POINT ( 'NONE',  ( 20.53650276133985031, -41.76263555408612405, -34.79644660940672907 ) ) ;
#13374 = CIRCLE ( 'NONE', #15045, 1.000000000000000888 ) ;
#13375 = AXIS2_PLACEMENT_3D ( 'NONE', #46002, #3004, #34956 ) ;
#13377 = AXIS2_PLACEMENT_3D ( 'NONE', #21808, #25994, #22061 ) ;
#13376 = CARTESIAN_POINT ( 'NONE',  ( 14.61931855295529914, -7.511323792149719125, -80.94886153518950778 ) ) ;
#13378 = ADVANCED_FACE ( 'NONE', ( #37258 ), #4117, .F. ) ;
#13379 = CYLINDRICAL_SURFACE ( 'NONE', #33656, 6.766999999999998572 ) ;
#13381 = CARTESIAN_POINT ( 'NONE',  ( 46.92684765627410570, -40.29994455800911624, -51.82181065190314229 ) ) ;
#13380 = CARTESIAN_POINT ( 'NONE',  ( 64.64302830678670375, 0.9098571636355720083, -60.77008670988870165 ) ) ;
#13382 = CIRCLE ( 'NONE', #28391, 39.00000000000001421 ) ;
#13383 = CARTESIAN_POINT ( 'NONE',  ( 61.11046412718479814, 14.09004753107949881, -46.82997413804069708 ) ) ;
#13384 = CARTESIAN_POINT ( 'NONE',  ( 24.04519454997480210, -15.61618869140488997, -79.50766696426083513 ) ) ;
#13385 = CARTESIAN_POINT ( 'NONE',  ( -28.69324816627959862, -35.41536148188630051, -54.99967661823389875 ) ) ;
#13386 = VERTEX_POINT ( 'NONE', #33042 ) ;
#13387 = CARTESIAN_POINT ( 'NONE',  ( 53.00693771576430180, -49.57086939845230233, -48.85763912010190069 ) ) ;
#13388 = CARTESIAN_POINT ( 'NONE',  ( 57.43557945885349625, -45.19660671630600035, -25.73777145330879890 ) ) ;
#13389 = CARTESIAN_POINT ( 'NONE',  ( 47.82090655655320433, -54.45843870253389696, -55.22757576880370323 ) ) ;
#13390 = CARTESIAN_POINT ( 'NONE',  ( 13.95210466151760187, 19.57561797166449935, -21.48689998016190117 ) ) ;
#13391 = CARTESIAN_POINT ( 'NONE',  ( 57.51732571122479243, 13.88248103308219861, -25.33327368259680057 ) ) ;
#13392 = CARTESIAN_POINT ( 'NONE',  ( 22.04771027143680229, -11.77303280754949810, -36.26938441530820256 ) ) ;
#13393 = CARTESIAN_POINT ( 'NONE',  ( 50.12047694090430383, 18.16987201063400192, -76.14999999999999147 ) ) ;
#13394 = CARTESIAN_POINT ( 'NONE',  ( 53.30565515969109924, 18.20461000561270026, -49.00291067189689898 ) ) ;
#13395 = CARTESIAN_POINT ( 'NONE',  ( 71.33702656696020483, 1.265664290790580182, -70.52755531239479581 ) ) ;
#13396 = CARTESIAN_POINT ( 'NONE',  ( -0.1437508118502997256, -8.468281633606618897, -34.89146800830131667 ) ) ;
#13397 = CARTESIAN_POINT ( 'NONE',  ( 47.26412996261229438, 22.82317408360536604, -75.56727799573911852 ) ) ;
#13398 = ORIENTED_EDGE ( 'NONE', *, *, #51700, .T. ) ;
#13399 = CARTESIAN_POINT ( 'NONE',  ( 21.82166399653609901, -10.80407293660230117, -70.84382614012608315 ) ) ;
#13400 = CARTESIAN_POINT ( 'NONE',  ( 73.10855093309899644, 0.8936201581567889685, -69.00461532610479765 ) ) ;
#13401 = CARTESIAN_POINT ( 'NONE',  ( 47.42532149332459568, -54.64264661477289309, -54.89680082169689967 ) ) ;
#13402 = CARTESIAN_POINT ( 'NONE',  ( 24.04355859723787248, -15.45599216157355293, -49.78588638766495933 ) ) ;
#13403 = DIRECTION ( 'NONE',  ( 0.000000000000000000, 0.000000000000000000, -1.000000000000000000 ) ) ;
#13404 = CARTESIAN_POINT ( 'NONE',  ( 56.78254780598179963, 19.37920438373040355, -53.13068928018909531 ) ) ;
#13405 = CARTESIAN_POINT ( 'NONE',  ( 52.83236039598949674, 18.42717821426129987, -48.53480049868920077 ) ) ;
#13406 = CARTESIAN_POINT ( 'NONE',  ( 46.77956775759329133, 7.928029628855391309, -34.67032516424389854 ) ) ;
#13407 = CARTESIAN_POINT ( 'NONE',  ( 71.89814544471239799, 1.396295651964280182, -61.23077165321539184 ) ) ;
#13408 = CARTESIAN_POINT ( 'NONE',  ( 8.428791191321906240, -17.68670080509079057, -72.42431558369844424 ) ) ;
#13409 = ORIENTED_EDGE ( 'NONE', *, *, #18378, .T. ) ;
#13410 = CARTESIAN_POINT ( 'NONE',  ( 64.76518258084509228, 1.097545367735389910, -70.56928864606319962 ) ) ;
#13411 = EDGE_LOOP ( 'NONE', ( #20931, #46941, #39694, #32370 ) ) ;
#13412 = CARTESIAN_POINT ( 'NONE',  ( 8.793990757808609615, -63.16307462209709911, -46.67050766270720175 ) ) ;
#13413 = AXIS2_PLACEMENT_3D ( 'NONE', #37658, #46577, #50240 ) ;
#13414 = CARTESIAN_POINT ( 'NONE',  ( 15.75369840593345394, -50.90400523626287566, -15.65824089793746055 ) ) ;
#13415 = VERTEX_POINT ( 'NONE', #1355 ) ;
#13416 = CARTESIAN_POINT ( 'NONE',  ( 11.93218571260559990, -65.12547012744420272, -45.62050932637900047 ) ) ;
#13417 = CARTESIAN_POINT ( 'NONE',  ( 22.72480950581076087, -13.84493606381021280, -70.36948975704638087 ) ) ;
#13418 = CARTESIAN_POINT ( 'NONE',  ( 9.221466634667571327, -19.60040990916195369, -70.34100234386488637 ) ) ;
#13419 = VECTOR ( 'NONE', #8574, 1000.000000000000000 ) ;
#13420 = CARTESIAN_POINT ( 'NONE',  ( 51.18087450704700103, 19.51486598760920188, -76.16568686306109726 ) ) ;
#13421 = CIRCLE ( 'NONE', #15043, 5.251829701412240148 ) ;
#13422 = ORIENTED_EDGE ( 'NONE', *, *, #45476, .T. ) ;
#13423 = DIRECTION ( 'NONE',  ( 0.000000000000000000, 0.000000000000000000, 1.000000000000000000 ) ) ;
#13424 = AXIS2_PLACEMENT_3D ( 'NONE', #2699, #30203, #10307 ) ;
#13425 = CARTESIAN_POINT ( 'NONE',  ( 22.90092669556440086, -15.60227691359268754, -72.45217148944418284 ) ) ;
#13426 = CARTESIAN_POINT ( 'NONE',  ( 8.222922666418535087, -16.30600728892422069, -66.47990195030855887 ) ) ;
#13427 = ADVANCED_FACE ( 'NONE', ( #49066 ), #36854, .F. ) ;
#13428 = B_SPLINE_SURFACE_WITH_KNOTS ( 'NONE', 3, 3, ( 
 ( #49730, #21656, #45018, #29778, #49481, #13067, #49221, #5702, #1509, #45797, #9885 ),
 ( #13569, #36616, #16711, #48698, #12799, #28756, #44755, #8861, #40821, #990, #16989 ),
 ( #32937, #21149, #1252, #25067, #17240, #41085, #33203, #29273, #21918, #26361, #46580 ),
 ( #42380, #10670, #5959, #42642, #38970, #26626, #22433, #6740, #15112, #42116, #14851 ),
 ( #26107, #38442, #22697, #38713, #2805, #18776, #51014, #3061, #33966, #10150, #18523 ),
 ( #30037, #34749, #30302, #50500, #34496, #37926, #38185, #31071, #50758, #11188, #22950 ),
 ( #42902, #2542, #30814, #46842, #6218, #14590, #22174, #10928, #26896, #2024, #6998 ),
 ( #19034, #35009, #47100, #27151, #2279, #18002, #18255, #34224, #49983, #14076, #46060 ),
 ( #50243, #14333, #40245, #19295, #47352, #3835, #23457, #15373, #47860, #15630, #35797 ),
 ( #43158, #39483, #39221, #7252, #3318, #24221, #23718, #43920, #20303, #3581, #20054 ),
 ( #28168, #51782, #19549, #35542, #39991, #39731, #32348, #48110, #19809, #44173, #51532 ),
 ( #405, #12464, #36294, #8271, #15885, #16391, #31328, #4338, #48365, #31838, #36045 ),
 ( #23967, #27918, #51275, #23201, #35278, #8014, #4081, #155, #31581, #11961, #16131 ),
 ( #11449, #7769, #32090, #27407, #47603, #12209, #43409, #7511, #11702, #27665, #43667 ),
 ( #659, #13515, #25531, #29471, #36822, #45474, #5386, #4859, #5131, #33402, #33135 ),
 ( #49419, #25272, #9325, #29210, #9575, #8540, #1186, #37349, #41533, #5650, #40497 ),
 ( #41276, #24747, #17690, #21597, #21088, #37596, #40757, #28432, #1707, #16646, #926 ),
 ( #17181, #33660, #32605, #49675, #44432, #25003, #21342, #48899, #1447, #13256, #36557 ),
 ( #24483, #45217, #17432, #4588, #16924, #49160, #9054, #20562, #48632, #44953, #12733 ),
 ( #20826, #28687, #44689, #8793, #32865, #12999, #28950, #37090, #41018, #50697, #10873 ) ),
 .UNSPECIFIED., .F., .F., .F.,
 ( 4, 2, 2, 2, 2, 2, 2, 2, 2, 4 ),
 ( 4, 1, 1, 1, 1, 1, 1, 1, 4 ),
 ( 0.000000000000000000, 0.05535613038339300129, 0.2869944836127450438, 0.5186328368420959345, 0.8630971313986249838, 1.150796175198169902, 1.294645697097940085, 1.524804932137569846, 1.893059708200979907, 2.301592350396330033 ),
 ( 0.000000000000000000, 0.1250000000000000000, 0.2500000000000000000, 0.3750000000000000000, 0.5000000000000000000, 0.6250000000000000000, 0.7500000000000000000, 0.8750000000000000000, 1.000000000000000000 ),
 .UNSPECIFIED. ) ;
#13429 = CARTESIAN_POINT ( 'NONE',  ( 8.740794891635950137, -11.96596101467000040, -54.93831488687840192 ) ) ;
#13430 = ADVANCED_FACE ( 'NONE', ( #33312 ), #316, .T. ) ;
#13431 = CARTESIAN_POINT ( 'NONE',  ( 9.366925336875675967, -14.68809727733580495, -55.49649026802917007 ) ) ;
#13432 = CARTESIAN_POINT ( 'NONE',  ( 42.79704101284554696, -37.74735858493779972, -76.33443527249174565 ) ) ;
#13433 = EDGE_CURVE ( 'NONE', #36317, #9892, #9230, .T. ) ;
#13434 = ORIENTED_EDGE ( 'NONE', *, *, #29611, .F. ) ;
#13435 = DIRECTION ( 'NONE',  ( -0.2389682100435167045, 0.9710273912658683448, 0.000000000000000000 ) ) ;
#13436 = CARTESIAN_POINT ( 'NONE',  ( 23.43389303623280284, -14.12711491007119946, -40.16860592796539464 ) ) ;
#13437 = CARTESIAN_POINT ( 'NONE',  ( 40.69061996557520189, 14.09050113835410123, -5.669818638807839761 ) ) ;
#13438 = CARTESIAN_POINT ( 'NONE',  ( 14.48181959901199889, 20.27135023148479576, -75.33782839756391070 ) ) ;
#13439 = CIRCLE ( 'NONE', #38, 5.999999999999998224 ) ;
#13440 = FACE_OUTER_BOUND ( 'NONE', #16943, .T. ) ;
#13441 = CARTESIAN_POINT ( 'NONE',  ( -1.839728563314089849, -28.30269090235150031, -54.64999999999999858 ) ) ;
#13442 = CARTESIAN_POINT ( 'NONE',  ( 23.47067812491659922, -19.37849624346840116, -57.65849580248539752 ) ) ;
#13443 = ADVANCED_FACE ( 'NONE', ( #13174 ), #12906, .F. ) ;
#13444 = ORIENTED_EDGE ( 'NONE', *, *, #22029, .F. ) ;
#13445 = CARTESIAN_POINT ( 'NONE',  ( 52.82291935875819888, -49.60365082802910308, -27.55752660507549834 ) ) ;
#13446 = CARTESIAN_POINT ( 'NONE',  ( 55.07813547831889878, -51.04730606513820135, -75.19531985927159212 ) ) ;
#13447 = CARTESIAN_POINT ( 'NONE',  ( 6.305142788495140316, 28.78716984886350261, -12.89664123648359961 ) ) ;
#13448 = CARTESIAN_POINT ( 'NONE',  ( 11.13393739769619906, 32.28996932333459569, -43.76018303787720498 ) ) ;
#13449 = CARTESIAN_POINT ( 'NONE',  ( 50.71554959566909559, 14.96708580405049993, -12.97453803614309997 ) ) ;
#13450 = ORIENTED_EDGE ( 'NONE', *, *, #49040, .F. ) ;
#13451 = AXIS2_PLACEMENT_3D ( 'NONE', #19128, #39314, #19388 ) ;
#13452 = CARTESIAN_POINT ( 'NONE',  ( -5.145198839953950554, -47.14946543292239767, -4.849579887423169033 ) ) ;
#13453 = AXIS2_PLACEMENT_3D ( 'NONE', #37246, #25425, #28585 ) ;
#13454 = CARTESIAN_POINT ( 'NONE',  ( 47.42191991419499431, 23.41235274918789955, -54.90470402679689954 ) ) ;
#13455 = CARTESIAN_POINT ( 'NONE',  ( -24.36606260230359666, -50.61618894467959962, 16.85000000000000142 ) ) ;
#13456 = CARTESIAN_POINT ( 'NONE',  ( 63.22228946811710415, 1.003508719580009867, -62.21555175845400498 ) ) ;
#13457 = DIRECTION ( 'NONE',  ( 0.000000000000000000, 0.000000000000000000, -1.000000000000000000 ) ) ;
#13458 = VECTOR ( 'NONE', #22286, 1000.000000000000000 ) ;
#13459 = CARTESIAN_POINT ( 'NONE',  ( 11.96242378326880029, 34.20360896090840441, -17.67418126880570028 ) ) ;
#13460 = DIRECTION ( 'NONE',  ( 6.938893903907222067E-15, 0.000000000000000000, -1.000000000000000000 ) ) ;
#13461 = CARTESIAN_POINT ( 'NONE',  ( 53.06963667952170027, 18.30286252129070235, -48.79723990062230143 ) ) ;
#13462 = FACE_OUTER_BOUND ( 'NONE', #51689, .T. ) ;
#13463 = CARTESIAN_POINT ( 'NONE',  ( 59.45724307632730188, -46.21313155759460045, -47.61455192236069678 ) ) ;
#13464 = CARTESIAN_POINT ( 'NONE',  ( 53.82324154614039458, 17.55874562463440114, -27.07948292951889968 ) ) ;
#13465 = CARTESIAN_POINT ( 'NONE',  ( 53.65245010158729855, 20.72074997219770154, -53.90489108192829804 ) ) ;
#13466 = CARTESIAN_POINT ( 'NONE',  ( 63.54731047306190561, 1.396834109478129804, -68.84999999999999432 ) ) ;
#13467 = CARTESIAN_POINT ( 'NONE',  ( 22.90083016047308462, -15.61618874168370752, -60.84718745454353694 ) ) ;
#13468 = ORIENTED_EDGE ( 'NONE', *, *, #45781, .T. ) ;
#13469 = CARTESIAN_POINT ( 'NONE',  ( 64.93393739769619799, 1.396834109478129804, -70.23662692463440749 ) ) ;
#13470 = CARTESIAN_POINT ( 'NONE',  ( 9.746758075853771075, 32.08108121953329572, -46.29788637164419640 ) ) ;
#13471 = CARTESIAN_POINT ( 'NONE',  ( 42.44160469162459748, 13.71702471974399984, -5.942261413879579734 ) ) ;
#13472 = CARTESIAN_POINT ( 'NONE',  ( 67.08845630739949684, -31.07791224506899752, -17.50640734377579832 ) ) ;
#13473 = CARTESIAN_POINT ( 'NONE',  ( 18.51915660836230160, 20.76921105827980085, -75.35480091913980516 ) ) ;
#13474 = ORIENTED_EDGE ( 'NONE', *, *, #49288, .T. ) ;
#13475 = ORIENTED_EDGE ( 'NONE', *, *, #18962, .F. ) ;
#13476 = CARTESIAN_POINT ( 'NONE',  ( 20.11812534144297970, -22.52867827160516256, -79.84100308582628713 ) ) ;
#13477 = ORIENTED_EDGE ( 'NONE', *, *, #15359, .T. ) ;
#13478 = CARTESIAN_POINT ( 'NONE',  ( 12.01043929807459953, -65.26379547360380684, -46.82866647765490598 ) ) ;
#13479 = CARTESIAN_POINT ( 'NONE',  ( 57.34482800150080095, -45.61704748136379806, -26.19284480059729958 ) ) ;
#13480 = CARTESIAN_POINT ( 'NONE',  ( 9.366931649850915420, -16.50194508580061381, -45.41115730554007968 ) ) ;
#13481 = CYLINDRICAL_SURFACE ( 'NONE', #45737, 7.910999999999997812 ) ;
#13482 = CARTESIAN_POINT ( 'NONE',  ( 61.67253348274019942, 13.94162801194639911, -46.85000153395669997 ) ) ;
#13483 = CARTESIAN_POINT ( 'NONE',  ( 63.86577392472210590, 1.451792515613489876, -61.80022504404329453 ) ) ;
#13484 = ORIENTED_EDGE ( 'NONE', *, *, #23382, .F. ) ;
#13485 = CARTESIAN_POINT ( 'NONE',  ( 75.04878402891587541, -10.96810985108981207, -11.30472392811527271 ) ) ;
#13486 = ORIENTED_EDGE ( 'NONE', *, *, #3625, .F. ) ;
#13487 = CARTESIAN_POINT ( 'NONE',  ( 53.99846808212529936, -46.02098823835780195, -15.26947028995409994 ) ) ;
#13488 = EDGE_CURVE ( 'NONE', #33336, #45208, #8968, .T. ) ;
#13489 = CARTESIAN_POINT ( 'NONE',  ( 24.04486687715447601, -15.65228672134179710, -33.79378184229195625 ) ) ;
#13490 = DIRECTION ( 'NONE',  ( -0.5720614028176865817, -0.4156269377774495233, 0.7071067811865480168 ) ) ;
#13491 = ADVANCED_FACE ( 'NONE', ( #24912 ), #23361, .T. ) ;
#13492 = PRODUCT_DEFINITION_FORMATION_WITH_SPECIFIED_SOURCE ( 'ANY', '', #16002, .NOT_KNOWN. ) ;
#13493 = VERTEX_POINT ( 'NONE', #24393 ) ;
#13494 = CARTESIAN_POINT ( 'NONE',  ( 16.13393739769620083, -15.61618894467929941, -17.93019253464870033 ) ) ;
#13495 = CARTESIAN_POINT ( 'NONE',  ( 46.45656088628239644, -53.12694234138209737, -76.13971323818920212 ) ) ;
#13496 = AXIS2_PLACEMENT_3D ( 'NONE', #42087, #14305, #34194 ) ;
#13497 = CARTESIAN_POINT ( 'NONE',  ( 60.40232013370989961, 14.60517343624429998, -47.72046811377730080 ) ) ;
#13498 = AXIS2_PLACEMENT_3D ( 'NONE', #18293, #23243, #31365 ) ;
#13499 = CARTESIAN_POINT ( 'NONE',  ( 45.07857608053570431, 14.88012197229889999, -9.026857927713109575 ) ) ;
#13500 = DIRECTION ( 'NONE',  ( 0.000000000000000000, 1.000000000000000000, 0.000000000000000000 ) ) ;
#13501 = DIRECTION ( 'NONE',  ( 0.3281607301299678814, 0.6263469766835031427, 0.7071067811865485719 ) ) ;
#13502 = CARTESIAN_POINT ( 'NONE',  ( 16.13393739769620083, -15.61618894467929941, -32.14999999999999858 ) ) ;
#13503 = CARTESIAN_POINT ( 'NONE',  ( 60.40002696937390425, 13.91362826609339898, -26.58785703793860122 ) ) ;
#13504 = CARTESIAN_POINT ( 'NONE',  ( 19.68480220708229922, -22.61462500487489891, -69.63804828363188903 ) ) ;
#13505 = ADVANCED_FACE ( 'NONE', ( #5555 ), #36995, .T. ) ;
#13506 = ORIENTED_EDGE ( 'NONE', *, *, #9715, .F. ) ;
#13507 = CARTESIAN_POINT ( 'NONE',  ( 53.57228486832382686, 18.19337119796120561, -49.24858181519383749 ) ) ;
#13508 = CARTESIAN_POINT ( 'NONE',  ( -10.49744324907189963, -41.58055173219970158, -4.376973931108589788 ) ) ;
#13509 = CARTESIAN_POINT ( 'NONE',  ( 15.21636614235080032, -50.60415920577569437, -15.64999998222989852 ) ) ;
#13510 = EDGE_CURVE ( 'NONE', #24819, #31554, #10834, .T. ) ;
#13511 = CARTESIAN_POINT ( 'NONE',  ( 72.56482987857130240, 1.421976796945970012, -69.29343522641019604 ) ) ;
#13512 = DIRECTION ( 'NONE',  ( 0.000000000000000000, 0.000000000000000000, -1.000000000000000000 ) ) ;
#13513 = CARTESIAN_POINT ( 'NONE',  ( 10.13393739769589885, 22.91950879131600161, -35.14999999999999858 ) ) ;
#13514 = CARTESIAN_POINT ( 'NONE',  ( 47.51793462813986935, -54.37766851147189584, -75.00961803996818844 ) ) ;
#13515 = CARTESIAN_POINT ( 'NONE',  ( 48.94958679002760249, -53.97766395890939606, -55.24468684015499775 ) ) ;
#13516 = CARTESIAN_POINT ( 'NONE',  ( 24.04493741807383600, -16.65174055729265135, -55.83400547657857516 ) ) ;
#13517 = CARTESIAN_POINT ( 'NONE',  ( 76.82615602979319647, -43.14551972207646457, -14.66829194415775461 ) ) ;
#13518 = DIRECTION ( 'NONE',  ( 0.000000000000000000, 0.000000000000000000, -1.000000000000000000 ) ) ;
#13519 = ORIENTED_EDGE ( 'NONE', *, *, #37335, .T. ) ;
#13520 = AXIS2_PLACEMENT_3D ( 'NONE', #25850, #50512, #46592 ) ;
#13521 = CARTESIAN_POINT ( 'NONE',  ( 10.06561770371539843, -19.93847889677480012, -47.87033613167638890 ) ) ;
#13522 = CARTESIAN_POINT ( 'NONE',  ( 64.64547391238390617, 1.377110276564549984, -61.07324425200700091 ) ) ;
#13523 = VERTEX_POINT ( 'NONE', #25182 ) ;
#13524 = CARTESIAN_POINT ( 'NONE',  ( -0.007164426707907000161, -50.71887597443840434, -34.77269723932290191 ) ) ;
#13525 = AXIS2_PLACEMENT_3D ( 'NONE', #13170, #37773, #13667 ) ;
#13526 = CARTESIAN_POINT ( 'NONE',  ( 60.98388430596229881, -45.56993733780140587, -47.58050232604119856 ) ) ;
#13527 = CARTESIAN_POINT ( 'NONE',  ( 22.77438730286804258, -17.50876119793745289, -74.93619413684334063 ) ) ;
#13528 = CARTESIAN_POINT ( 'NONE',  ( 56.84932596551129791, 19.42421318737730118, -53.85230338955989993 ) ) ;
#13530 = CARTESIAN_POINT ( 'NONE',  ( 18.86789271228450104, 20.55440457967890211, -74.14999999999999147 ) ) ;
#13529 = CARTESIAN_POINT ( 'NONE',  ( 43.73535983031142393, 8.700407067847576670, -67.94015393090442956 ) ) ;
#13531 = AXIS2_PLACEMENT_3D ( 'NONE', #51180, #11347, #39637 ) ;
#13532 = CARTESIAN_POINT ( 'NONE',  ( 11.73137203405252826, -41.76263555408610273, -34.79644660940672196 ) ) ;
#13533 = CARTESIAN_POINT ( 'NONE',  ( 8.133937397696209715, -59.02534396924340143, -43.74348518090240390 ) ) ;
#13534 = ORIENTED_EDGE ( 'NONE', *, *, #38152, .T. ) ;
#13535 = VERTEX_POINT ( 'NONE', #44338 ) ;
#13536 = ORIENTED_EDGE ( 'NONE', *, *, #13130, .T. ) ;
#13537 = CARTESIAN_POINT ( 'NONE',  ( 61.44594299458270115, -45.22213083583160653, -46.96386565649149958 ) ) ;
#13538 = DIRECTION ( 'NONE',  ( 1.000000000000000000, 0.000000000000000000, 0.000000000000000000 ) ) ;
#13539 = CARTESIAN_POINT ( 'NONE',  ( 56.51581731585299906, -50.73333708345260362, -53.50072361911870189 ) ) ;
#13540 = ORIENTED_EDGE ( 'NONE', *, *, #35259, .T. ) ;
#13541 = ORIENTED_EDGE ( 'NONE', *, *, #25820, .F. ) ;
#13542 = ORIENTED_EDGE ( 'NONE', *, *, #2409, .F. ) ;
#13543 = CARTESIAN_POINT ( 'NONE',  ( 14.36260000156801553, -22.20703888855211616, -73.03610280558059742 ) ) ;
#13544 = CARTESIAN_POINT ( 'NONE',  ( -9.005807778154689913, 14.20118441705474410, -42.97877832676560672 ) ) ;
#13545 = ADVANCED_FACE ( 'NONE', ( #16553 ), #6672, .F. ) ;
#13546 = CARTESIAN_POINT ( 'NONE',  ( 17.90520375179345436, -22.20705683982200185, -52.86948537568310513 ) ) ;
#13547 = ORIENTED_EDGE ( 'NONE', *, *, #47447, .T. ) ;
#13548 = CARTESIAN_POINT ( 'NONE',  ( 52.16338473820870547, -49.90420398983260242, -76.93802979155799449 ) ) ;
#13549 = CARTESIAN_POINT ( 'NONE',  ( 60.63032377830810304, 14.34160671423079947, -47.11936141799559152 ) ) ;
#13550 = CARTESIAN_POINT ( 'NONE',  ( 11.69621752664579972, -22.08869927203039651, -60.70380296398279540 ) ) ;
#13551 = CARTESIAN_POINT ( 'NONE',  ( 68.13393739769620083, 0.8838110553206759423, -65.65000000000000568 ) ) ;
#13552 = CARTESIAN_POINT ( 'NONE',  ( 44.70619667840409761, 13.88245460051030022, -7.106835951036900134 ) ) ;
#13553 = CARTESIAN_POINT ( 'NONE',  ( 42.28714451724680146, -44.27662781396410452, -5.063832641217489439 ) ) ;
#13554 = CARTESIAN_POINT ( 'NONE',  ( 70.03247032090770574, -49.95860450173900347, -75.14853292321149070 ) ) ;
#13555 = CARTESIAN_POINT ( 'NONE',  ( -10.87564126230760131, 11.12160698687080185, -6.291562883898949465 ) ) ;
#13556 = AXIS2_PLACEMENT_3D ( 'NONE', #44884, #8988, #40946 ) ;
#13557 = CIRCLE ( 'NONE', #45350, 13.00000000000000178 ) ;
#13558 = CARTESIAN_POINT ( 'NONE',  ( 63.83871783002559397, 1.346166815163519992, -69.67924993017680890 ) ) ;
#13559 = DIRECTION ( 'NONE',  ( -1.000000000000000000, 0.000000000000000000, 0.000000000000000000 ) ) ;
#13560 = CARTESIAN_POINT ( 'NONE',  ( 67.09948597405160342, 1.833213267668650115, -20.09058995088950184 ) ) ;
#13561 = ORIENTED_EDGE ( 'NONE', *, *, #10700, .F. ) ;
#13562 = CARTESIAN_POINT ( 'NONE',  ( 14.42532105552479926, -51.34461045803089974, -75.09854824053580558 ) ) ;
#13563 = CARTESIAN_POINT ( 'NONE',  ( 47.21205592235610737, -54.78444012246939820, -54.63239976220819472 ) ) ;
#13564 = EDGE_CURVE ( 'NONE', #39558, #48021, #2653, .T. ) ;
#13565 = DIRECTION ( 'NONE',  ( 1.000000000000000000, 0.000000000000000000, 0.000000000000000000 ) ) ;
#13566 = LINE ( 'NONE', #26358, #49400 ) ;
#13567 = CARTESIAN_POINT ( 'NONE',  ( 22.47052291036699856, -19.84169571818189937, -32.14999999999999858 ) ) ;
#13568 = LINE ( 'NONE', #29531, #5533 ) ;
#13569 = CARTESIAN_POINT ( 'NONE',  ( 47.65668213871590098, -54.52839204276340013, -55.15716614278580465 ) ) ;
#13570 = DIRECTION ( 'NONE',  ( 0.000000000000000000, 0.000000000000000000, -1.000000000000000000 ) ) ;
#13571 = CARTESIAN_POINT ( 'NONE',  ( 56.47574016726019863, 19.53693441320439916, -53.73400676226840034 ) ) ;
#13572 = CARTESIAN_POINT ( 'NONE',  ( 48.01070916242489517, 23.12336947638609885, -54.98721641925899206 ) ) ;
#13573 = VERTEX_POINT ( 'NONE', #9735 ) ;
#13574 = CARTESIAN_POINT ( 'NONE',  ( 9.081352278131740619, -15.55616973317930096, -59.84988861282279515 ) ) ;
#13575 = ORIENTED_EDGE ( 'NONE', *, *, #9172, .F. ) ;
#13576 = DIRECTION ( 'NONE',  ( -1.000000000000000000, 0.000000000000000000, 0.000000000000000000 ) ) ;
#13577 = CARTESIAN_POINT ( 'NONE',  ( 65.23632417210509971, 1.383928098097870096, -60.96256459357869772 ) ) ;
#13578 = FACE_OUTER_BOUND ( 'NONE', #29507, .T. ) ;
#13580 = CARTESIAN_POINT ( 'NONE',  ( 55.05148602120549839, 15.77693620304509992, -25.60753014925489879 ) ) ;
#13579 = CARTESIAN_POINT ( 'NONE',  ( 84.24389573796460695, 12.93914432394539915, -47.41156961578170126 ) ) ;
#13581 = CARTESIAN_POINT ( 'NONE',  ( 10.05028766160000053, -12.04802911289969991, -77.62166643051759252 ) ) ;
#13582 = DIRECTION ( 'NONE',  ( 1.000000000000000000, 0.000000000000000000, 0.000000000000000000 ) ) ;
#13583 = CARTESIAN_POINT ( 'NONE',  ( 72.77636315587029969, 1.387131204727280132, -68.68796153961081075 ) ) ;
#13584 = CARTESIAN_POINT ( 'NONE',  ( 9.221491714471486745, -19.60045278370350985, -80.62566522957574477 ) ) ;
#13585 = VERTEX_POINT ( 'NONE', #22025 ) ;
#13586 = VERTEX_POINT ( 'NONE', #30664 ) ;
#13587 = B_SPLINE_CURVE_WITH_KNOTS ( 'NONE', 3,
 ( #38096, #5358, #17402, #17914 ),
 .UNSPECIFIED., .F., .F.,
 ( 4, 4 ),
 ( 0.000000000000000000, 1.000000000000000000 ),
 .UNSPECIFIED. ) ;
#13588 = CARTESIAN_POINT ( 'NONE',  ( 11.99500145081920088, -65.25785463067840908, -16.88883237368289869 ) ) ;
#13589 = CARTESIAN_POINT ( 'NONE',  ( 11.49485748460980084, 33.59317259934719146, -45.88007095197389873 ) ) ;
#13590 = CARTESIAN_POINT ( 'NONE',  ( 9.387003650334634131, -11.44024311550892037, -38.68416691240651772 ) ) ;
#13591 = CIRCLE ( 'NONE', #34478, 2.576499999999998902 ) ;
#13592 = CARTESIAN_POINT ( 'NONE',  ( 12.39013027377469989, 34.14800971684240238, -46.54379730670240178 ) ) ;
#13593 = CARTESIAN_POINT ( 'NONE',  ( 10.73552252728440060, -65.02568017880969364, -47.16673514230450337 ) ) ;
#13594 = TOROIDAL_SURFACE ( 'NONE', #30290, 24.89999999999999858, 4.000000000000059508 ) ;
#13595 = VERTEX_POINT ( 'NONE', #18357 ) ;
#13596 = CARTESIAN_POINT ( 'NONE',  ( -21.83178109590970095, -6.979653015830420415, -53.75064070593009546 ) ) ;
#13597 = FACE_OUTER_BOUND ( 'NONE', #10373, .T. ) ;
#13598 = ADVANCED_FACE ( 'NONE', ( #2131, #34601, #46689, #22543, #29884, #14438 ), #34336, .T. ) ;
#13599 = CARTESIAN_POINT ( 'NONE',  ( 52.96770052557779707, 18.26589706774769795, -48.58772269060800397 ) ) ;
#13600 = CARTESIAN_POINT ( 'NONE',  ( 61.63186543861399969, -2.018559880675780072, -16.00684823669729795 ) ) ;
#13601 = CARTESIAN_POINT ( 'NONE',  ( 51.24580075538570156, -49.39897230491230573, -76.45613186134289663 ) ) ;
#13602 = EDGE_CURVE ( 'NONE', #14356, #15737, #26743, .T. ) ;
#13603 = CARTESIAN_POINT ( 'NONE',  ( 35.69765375167399668, -15.61618894467929941, 6.850000000000000533 ) ) ;
#13604 = VERTEX_POINT ( 'NONE', #46430 ) ;
#13605 = ADVANCED_FACE ( 'NONE', ( #5805 ), #9990, .T. ) ;
#13606 = DIRECTION ( 'NONE',  ( 0.000000000000000000, 0.000000000000000000, -1.000000000000000000 ) ) ;
#13607 = CARTESIAN_POINT ( 'NONE',  ( 70.83745409581388230, 17.98087126524299606, -74.20351669811765305 ) ) ;
#13608 = ORIENTED_EDGE ( 'NONE', *, *, #37719, .T. ) ;
#13609 = CARTESIAN_POINT ( 'NONE',  ( 37.88393739769619373, -41.76263555408612405, -34.79644660940672907 ) ) ;
#13610 = DIRECTION ( 'NONE',  ( 0.000000000000000000, 0.000000000000000000, -1.000000000000000000 ) ) ;
#13611 = EDGE_CURVE ( 'NONE', #4756, #44974, #30408, .T. ) ;
#13612 = CARTESIAN_POINT ( 'NONE',  ( 14.92914649562269958, -23.37087955876669909, -34.56155571298829443 ) ) ;
#13613 = CARTESIAN_POINT ( 'NONE',  ( 21.40734412482820304, -20.29953610935300290, -65.07833806302818402 ) ) ;
#13614 = CARTESIAN_POINT ( 'NONE',  ( 56.79288268143969987, 19.43545220660120165, -74.14914690165589661 ) ) ;
#13615 = CARTESIAN_POINT ( 'NONE',  ( 47.50498297817869542, -54.47480520914279367, -74.80901628187270092 ) ) ;
#13616 = ORIENTED_EDGE ( 'NONE', *, *, #45449, .F. ) ;
#13617 = CARTESIAN_POINT ( 'NONE',  ( 56.24180394757939894, 14.16774694249440003, -16.78461393623150144 ) ) ;
#13618 = CARTESIAN_POINT ( 'NONE',  ( 21.54529218309743044, -11.45756400702632760, -78.24448439904941210 ) ) ;
#13619 = CARTESIAN_POINT ( 'NONE',  ( 57.13721805172019685, -50.61838845098209561, -53.74365126625890099 ) ) ;
#13620 = EDGE_CURVE ( 'NONE', #44905, #6898, #30059, .T. ) ;
#13621 = CARTESIAN_POINT ( 'NONE',  ( 11.92983776680200059, -9.953318164945169855, -38.14390150139109892 ) ) ;
#13622 = CARTESIAN_POINT ( 'NONE',  ( 12.30558705848279999, -9.692820574005770240, -44.16454026222620399 ) ) ;
#13623 = ORIENTED_EDGE ( 'NONE', *, *, #38533, .F. ) ;
#13624 = CARTESIAN_POINT ( 'NONE',  ( 47.19371938996339821, 22.91183880830930164, -75.51723258725729693 ) ) ;
#13625 = CARTESIAN_POINT ( 'NONE',  ( 20.13393739083949896, -55.41568640430479320, -20.65000000000000213 ) ) ;
#13626 = EDGE_CURVE ( 'NONE', #29074, #49316, #18303, .T. ) ;
#13627 = CARTESIAN_POINT ( 'NONE',  ( 75.25323313020308547, -34.43977339652462888, -12.29989660903943438 ) ) ;
#13628 = VECTOR ( 'NONE', #23748, 1000.000000000000000 ) ;
#13629 = CARTESIAN_POINT ( 'NONE',  ( 64.22355794744891000, 1.454950765200730078, -69.87277598216670071 ) ) ;
#13630 = AXIS2_PLACEMENT_3D ( 'NONE', #5807, #1872, #1095 ) ;
#13631 = CARTESIAN_POINT ( 'NONE',  ( 29.10094820555050177, -4.504588236828580783, -34.97139175453740023 ) ) ;
#13632 = CARTESIAN_POINT ( 'NONE',  ( 18.89608595021987725, -49.61618894467940777, -83.05213603404914124 ) ) ;
#13633 = CARTESIAN_POINT ( 'NONE',  ( 62.03393739769618520, -0.5161889446793590519, -65.65000000000000568 ) ) ;
#13635 = CARTESIAN_POINT ( 'NONE',  ( 45.45010799891814202, -40.18496802584400740, -59.12881032271813808 ) ) ;
#13634 = CARTESIAN_POINT ( 'NONE',  ( 64.68608103367580497, 0.9036513197889539661, -60.73950228677190211 ) ) ;
#13636 = CARTESIAN_POINT ( 'NONE',  ( 61.30391762588470073, 13.98869191317340110, -46.37202200358919413 ) ) ;
#13637 = CARTESIAN_POINT ( 'NONE',  ( -18.27909364759700139, 20.72688191304690264, -53.14840429075709949 ) ) ;
#13638 = ORIENTED_EDGE ( 'NONE', *, *, #11889, .F. ) ;
#13639 = CARTESIAN_POINT ( 'NONE',  ( 53.21742324705429894, -49.46290330832970028, -48.89816740597070321 ) ) ;
#13640 = VERTEX_POINT ( 'NONE', #37778 ) ;
#13641 = EDGE_CURVE ( 'NONE', #42293, #41355, #6066, .T. ) ;
#13642 = CARTESIAN_POINT ( 'NONE',  ( 58.74123455927210102, -45.12673593262880445, -25.78612740298530071 ) ) ;
#13643 = CYLINDRICAL_SURFACE ( 'NONE', #10978, 1.999999999999970246 ) ;
#13644 = CARTESIAN_POINT ( 'NONE',  ( 56.14548367315779842, 14.43159843830459899, -25.51430258618709956 ) ) ;
#13645 = CARTESIAN_POINT ( 'NONE',  ( 17.63133417498849909, -22.50823955302369939, -46.88472117783319959 ) ) ;
#13646 = CARTESIAN_POINT ( 'NONE',  ( 29.07912664786299928, -26.71971901182079989, -34.92075920103129505 ) ) ;
#13647 = CARTESIAN_POINT ( 'NONE',  ( 52.87767298794570081, 18.41793525666839670, -48.88837531658360547 ) ) ;
#13648 = CARTESIAN_POINT ( 'NONE',  ( 60.23130391296999875, -45.78304229081430066, -47.24246919202539630 ) ) ;
#13649 = CARTESIAN_POINT ( 'NONE',  ( 73.82352657437539278, -44.30885758721080236, -13.22070786789489993 ) ) ;
#13650 = VERTEX_POINT ( 'NONE', #1611 ) ;
#13651 = CARTESIAN_POINT ( 'NONE',  ( 8.754676953983009824, -14.58992891808219916, -72.11132903714390352 ) ) ;
#13652 = CARTESIAN_POINT ( 'NONE',  ( 73.11690592692660573, 0.8925687589132640376, -68.99219224778180148 ) ) ;
#13653 = CARTESIAN_POINT ( 'NONE',  ( 47.45628758025669924, -54.61120735724659880, -54.67911033738580073 ) ) ;
#13654 = DIRECTION ( 'NONE',  ( 0.000000000000000000, 0.000000000000000000, -1.000000000000000000 ) ) ;
#13655 = CARTESIAN_POINT ( 'NONE',  ( 72.95819590288698464, 1.328674444234379859, -62.53373279716100086 ) ) ;
#13656 = CARTESIAN_POINT ( 'NONE',  ( 11.74201408114130096, -65.42316349444709545, -18.09919823657899940 ) ) ;
#13657 = CARTESIAN_POINT ( 'NONE',  ( 71.29447239804829906, 1.393731187554809958, -61.04935521477050031 ) ) ;
#13658 = CARTESIAN_POINT ( 'NONE',  ( 17.14513548805572540, -23.53033894168608953, -76.25158136700031264 ) ) ;
#13659 = CARTESIAN_POINT ( 'NONE',  ( 17.67054341374410242, -9.002906339670014191, -62.02556814933810614 ) ) ;
#13660 = CARTESIAN_POINT ( 'NONE',  ( 13.02825699543591220, -22.94029734278106858, -46.13525268572119131 ) ) ;
#13661 = CARTESIAN_POINT ( 'NONE',  ( 64.82191989009379540, 0.9958340104639651358, -70.64420736479868879 ) ) ;
#13662 = ORIENTED_EDGE ( 'NONE', *, *, #48761, .T. ) ;
#13663 = CARTESIAN_POINT ( 'NONE',  ( 8.977345137891989069, -63.27590191225959870, -46.63353902393470207 ) ) ;
#13664 = LINE ( 'NONE', #45629, #17673 ) ;
#13665 = ORIENTED_EDGE ( 'NONE', *, *, #46377, .F. ) ;
#13666 = LINE ( 'NONE', #29629, #6600 ) ;
#13667 = DIRECTION ( 'NONE',  ( 0.5112408204145773016, 0.8594375041513080404, 0.000000000000000000 ) ) ;
#13668 = CARTESIAN_POINT ( 'NONE',  ( 22.90099491887654182, -15.61618908163285546, -52.84717737022585027 ) ) ;
#13669 = EDGE_CURVE ( 'NONE', #32498, #46482, #1870, .T. ) ;
#13670 = CARTESIAN_POINT ( 'NONE',  ( 51.93758447892039953, 19.58744159688830067, -76.23465794037869614 ) ) ;
#13671 = VECTOR ( 'NONE', #36626, 1000.000000000000000 ) ;
#13672 = EDGE_LOOP ( 'NONE', ( #7850, #33830, #46873, #11631, #32435, #32827, #36971, #1057, #12132, #29310, #2049, #45967, #40424, #21271, #31409, #22463, #18685, #49002, #5499, #32399, #21766, #21425, #9979, #25032, #12321, #4358, #45374, #8094, #38300, #42717, #1501, #40567, #11472, #19512, #44588, #49470, #48929, #45318, #5171, #46620, #1993, #27444, #34855, #28398, #41341, #13484, #2968, #34523, #22536, #18042, #10920, #17008, #22954, #51242, #41782, #32281, #50465, #1983, #8959, #24049, #13979, #43735, #13890, #133, #28957, #50218, #20843, #4929, #23619, #49751, #23826, #32118, #12772, #4628, #3662, #33564, #39802, #18540, #40354, #4364, #37576, #50204, #15715, #23975, #42595, #32054, #15272, #14814, #46742, #27888, #36262, #13776, #45161, #24706, #31200, #935, #31516, #9604, #43089, #92, #7776, #9045, #51494 ) ) ;
#13673 = EDGE_CURVE ( 'NONE', #46679, #13415, #4149, .T. ) ;
#13674 = CIRCLE ( 'NONE', #15310, 16.60961179679784649 ) ;
#13675 = DIRECTION ( 'NONE',  ( 1.000000000000000000, 0.000000000000000000, 0.000000000000000000 ) ) ;
#13676 = CARTESIAN_POINT ( 'NONE',  ( -24.36606260230359666, -50.61618894467959962, 14.21249999999999858 ) ) ;
#13677 = CARTESIAN_POINT ( 'NONE',  ( 12.14971260091438765, -8.703718504070650397, -43.12570318788042556 ) ) ;
#13678 = EDGE_CURVE ( 'NONE', #12521, #38625, #27336, .T. ) ;
#13679 = CARTESIAN_POINT ( 'NONE',  ( 23.35206755134019829, -11.63105191554319973, -57.63175854304149937 ) ) ;
#13680 = CARTESIAN_POINT ( 'NONE',  ( -0.007164427059776000244, -20.74946784552680157, -34.77269723891829756 ) ) ;
#13681 = CARTESIAN_POINT ( 'NONE',  ( 45.14904957753085313, -38.06017041830072145, -64.57443011523157850 ) ) ;
#13682 = VERTEX_POINT ( 'NONE', #22284 ) ;
#13683 = CARTESIAN_POINT ( 'NONE',  ( 56.82260617504960010, -46.00315474979750263, -26.24626356014529804 ) ) ;
#13684 = CARTESIAN_POINT ( 'NONE',  ( 22.13578182761139956, -11.20205740560600027, -46.03080682667329881 ) ) ;
#13685 = CARTESIAN_POINT ( 'NONE',  ( 52.56949981068910205, -49.85724369911659437, -48.49331493222930334 ) ) ;
#13686 = CARTESIAN_POINT ( 'NONE',  ( 8.823988302720360721, -15.97264899720290288, -32.14999999999999858 ) ) ;
#13687 = CARTESIAN_POINT ( 'NONE',  ( 14.13832751391059972, 19.89797661840560039, -74.34810712130391153 ) ) ;
#13688 = ADVANCED_FACE ( 'NONE', ( #17852 ), #49835, .F. ) ;
#13689 = CARTESIAN_POINT ( 'NONE',  ( 17.52127312675804305, -52.24942673177908148, -75.96019247807906538 ) ) ;
#13690 = CARTESIAN_POINT ( 'NONE',  ( 45.65337825043140185, -45.22678660988140109, -8.155634320957650729 ) ) ;
#13691 = CARTESIAN_POINT ( 'NONE',  ( 23.99659259676478484, -14.72524117505133390, -61.47176532453648434 ) ) ;
#13692 = CARTESIAN_POINT ( 'NONE',  ( 23.28245223885990356, -11.50748400581630015, -57.34162007823099572 ) ) ;
#13693 = ORIENTED_EDGE ( 'NONE', *, *, #10454, .T. ) ;
#13694 = CARTESIAN_POINT ( 'NONE',  ( 55.13720784205819569, -47.03157555599469930, -26.02069266286289917 ) ) ;
#13695 = CARTESIAN_POINT ( 'NONE',  ( 15.46269294851370013, -51.02814174995680219, -21.20027565687029991 ) ) ;
#13697 = CARTESIAN_POINT ( 'NONE',  ( 41.64058680028773551, -39.72527599113804087, -78.06475774647746846 ) ) ;
#13696 = CARTESIAN_POINT ( 'NONE',  ( 1.943467852530839979, 24.47558943821050192, -10.50290134495580041 ) ) ;
#13698 = VECTOR ( 'NONE', #6492, 1000.000000000000114 ) ;
#13699 = CARTESIAN_POINT ( 'NONE',  ( 18.68994930968701240, -9.042806080414303338, -70.46522537534779929 ) ) ;
#13700 = DIRECTION ( 'NONE',  ( -1.000000000000000000, 0.000000000000000000, 0.000000000000000000 ) ) ;
#13701 = VECTOR ( 'NONE', #44445, 1000.000000000000000 ) ;
#13702 = ORIENTED_EDGE ( 'NONE', *, *, #39986, .T. ) ;
#13703 = CARTESIAN_POINT ( 'NONE',  ( -8.354434865538138411, -44.72889599991650300, -5.578549619731169251 ) ) ;
#13704 = VECTOR ( 'NONE', #32764, 1000.000000000000000 ) ;
#13706 = CARTESIAN_POINT ( 'NONE',  ( 47.51579407122170551, 23.33782210192210016, -54.66949387222739887 ) ) ;
#13705 = VECTOR ( 'NONE', #10989, 999.9999999999998863 ) ;
#13707 = EDGE_CURVE ( 'NONE', #5521, #13106, #10517, .T. ) ;
#13708 = CARTESIAN_POINT ( 'NONE',  ( 22.15575932996800290, 22.87009133999809762, -34.93361312117490058 ) ) ;
#13709 = CARTESIAN_POINT ( 'NONE',  ( 63.40532295848070987, 1.369664981662529923, -62.55358821066108987 ) ) ;
#13710 = CARTESIAN_POINT ( 'NONE',  ( 61.08978246524510070, 14.10367963069579922, -46.92961180776249819 ) ) ;
#13711 = CARTESIAN_POINT ( 'NONE',  ( 41.34908647067909726, 13.52015569396220052, -5.352709625395239534 ) ) ;
#13712 = CARTESIAN_POINT ( 'NONE',  ( 51.90728853546290367, 18.14319514060320060, -77.08409337567729835 ) ) ;
#13713 = CARTESIAN_POINT ( 'NONE',  ( 52.84731125486479897, 18.41934504040209930, -48.60966020774090168 ) ) ;
#13714 = CARTESIAN_POINT ( 'NONE',  ( 68.13393739769620083, -43.11618894467930119, -73.25000000000000000 ) ) ;
#13715 = B_SPLINE_CURVE_WITH_KNOTS ( 'NONE', 3,
 ( #44811, #521, #16507, #32457, #48484, #773, #8650, #24603, #4715, #16772, #8919, #24865, #37725, #30354, #5507, #5249, #45855, #46383, #17299, #6016, #34282, #2336, #14129, #13625 ),
 .UNSPECIFIED., .F., .F.,
 ( 4, 2, 1, 1, 2, 2, 1, 1, 2, 2, 1, 1, 2, 2, 4 ),
 ( 0.000000000000000000, 0.2499999999999947820, 0.3749999999999936162, 0.4374999999999935052, 0.4687499999999939493, 0.4999999999999943379, 0.5624999999999930056, 0.5937499999999930056, 0.6093749999999936717, 0.6249999999999942268, 0.6874999999999985567, 0.7187500000000000000, 0.7343750000000007772, 0.7500000000000015543, 1.000000000000000000 ),
 .UNSPECIFIED. ) ;
#13716 = CARTESIAN_POINT ( 'NONE',  ( 22.90065123677362635, -15.61618748955864433, -66.45281999012681240 ) ) ;
#13717 = EDGE_CURVE ( 'NONE', #10836, #31172, #7491, .T. ) ;
#13718 = CARTESIAN_POINT ( 'NONE',  ( 54.86690915992559781, 20.20342982344670091, -53.70992542625590005 ) ) ;
#13719 = CARTESIAN_POINT ( 'NONE',  ( 63.58464056502309347, 1.025917269765419970, -69.56324595238550046 ) ) ;
#13720 = PLANE ( 'NONE',  #50870 ) ;
#13721 = ORIENTED_EDGE ( 'NONE', *, *, #39582, .F. ) ;
#13722 = DIRECTION ( 'NONE',  ( 0.8660254037844384856, -0.5000000000000003331, -2.775557561562892337E-16 ) ) ;
#13723 = CARTESIAN_POINT ( 'NONE',  ( 10.49050030533310007, 32.01494398242250128, -45.62565322571249737 ) ) ;
#13724 = CARTESIAN_POINT ( 'NONE',  ( 41.40756759976829926, 13.53921337778190015, -5.393983492778530398 ) ) ;
#13725 = CARTESIAN_POINT ( 'NONE',  ( 9.367407790820902136, -15.61608574124520032, -61.84717978381009829 ) ) ;
#13726 = DIRECTION ( 'NONE',  ( 0.3863301728269248891, 0.9223605572461988089, -3.330669073875469621E-16 ) ) ;
#13727 = ORIENTED_EDGE ( 'NONE', *, *, #25757, .T. ) ;
#13728 = ORIENTED_EDGE ( 'NONE', *, *, #26820, .F. ) ;
#13729 = VECTOR ( 'NONE', #51313, 1000.000000000000000 ) ;
#13730 = CARTESIAN_POINT ( 'NONE',  ( 8.222963689089544559, -16.65192889645067353, -80.46600190389186480 ) ) ;
#13731 = ORIENTED_EDGE ( 'NONE', *, *, #6270, .T. ) ;
#13732 = CARTESIAN_POINT ( 'NONE',  ( 10.70946016660839994, -64.33455432219130898, -46.11556548067969885 ) ) ;
#13733 = CARTESIAN_POINT ( 'NONE',  ( 56.80041699543109956, -45.59906731679899394, -26.04381423261900252 ) ) ;
#13734 = DIRECTION ( 'NONE',  ( 0.000000000000000000, 0.000000000000000000, 1.000000000000000000 ) ) ;
#13735 = EDGE_CURVE ( 'NONE', #16294, #44712, #37590, .T. ) ;
#13736 =( BOUNDED_CURVE ( )  B_SPLINE_CURVE ( 3, ( #33644, #38113, #33899, #42305 ),
 .UNSPECIFIED., .F., .T. ) 
 B_SPLINE_CURVE_WITH_KNOTS ( ( 4, 4 ),
 ( 2.356194490192482505, 3.141592653589790451 ),
 .UNSPECIFIED. ) 
 CURVE ( )  GEOMETRIC_REPRESENTATION_ITEM ( )  RATIONAL_B_SPLINE_CURVE ( ( 1.000000000000000000, 0.9492530216742089966, 0.9492530216742089966, 1.000000000000000000 ) ) 
 REPRESENTATION_ITEM ( '' )  );
#13737 = CARTESIAN_POINT ( 'NONE',  ( 63.93393739769619089, 1.883811055320669947, -68.84999999999999432 ) ) ;
#13738 = ORIENTED_EDGE ( 'NONE', *, *, #6459, .T. ) ;
#13739 = CARTESIAN_POINT ( 'NONE',  ( 45.45535151068285984, 6.862517011477148543, -63.04287378213577142 ) ) ;
#13740 = EDGE_CURVE ( 'NONE', #30578, #42328, #1618, .T. ) ;
#13741 = VERTEX_POINT ( 'NONE', #38820 ) ;
#13742 = CARTESIAN_POINT ( 'NONE',  ( 55.10456398469269601, -45.21089673982120161, -14.92011640338920131 ) ) ;
#13743 = DIRECTION ( 'NONE',  ( -1.000000000000000000, 0.000000000000000000, 0.000000000000000000 ) ) ;
#13744 = CARTESIAN_POINT ( 'NONE',  ( 16.19673815769250069, 19.83680681410009683, -20.37207796061779774 ) ) ;
#13745 = DIRECTION ( 'NONE',  ( -0.8090169943749474513, -0.5877852522924732481, 0.000000000000000000 ) ) ;
#13746 = ORIENTED_EDGE ( 'NONE', *, *, #1153, .F. ) ;
#13747 = DIRECTION ( 'NONE',  ( 0.000000000000000000, 1.000000000000000000, 0.000000000000000000 ) ) ;
#13748 = CARTESIAN_POINT ( 'NONE',  ( 46.85564613059059980, -54.06445821833459320, -75.74423906255060501 ) ) ;
#13749 = CARTESIAN_POINT ( 'NONE',  ( 60.96148484106869603, 14.45202308121209889, -47.73691995860960446 ) ) ;
#13750 = CARTESIAN_POINT ( 'NONE',  ( 55.00116481104370081, 13.88381105532070059, -13.90662477428320187 ) ) ;
#13751 = DIRECTION ( 'NONE',  ( 1.000000000000000000, 0.000000000000000000, 0.000000000000000000 ) ) ;
#13752 = CARTESIAN_POINT ( 'NONE',  ( 51.90125962217079802, 20.02812747325270237, -76.04050507973269646 ) ) ;
#13753 = CARTESIAN_POINT ( 'NONE',  ( 61.58485588298179891, 13.89573119013970093, -28.02799758715149991 ) ) ;
#13754 = CARTESIAN_POINT ( 'NONE',  ( 8.361024636538020971, -14.53518228854489891, -72.33149193979490121 ) ) ;
#13755 = EDGE_LOOP ( 'NONE', ( #49197, #33990, #31994, #47761, #7585, #1244, #20124, #36635 ) ) ;
#13756 = CARTESIAN_POINT ( 'NONE',  ( 68.13393739769620083, -48.11618894467930119, -73.25000000000000000 ) ) ;
#13757 = VECTOR ( 'NONE', #19207, 1000.000000000000114 ) ;
#13758 = CARTESIAN_POINT ( 'NONE',  ( 73.20393974370449541, 0.8850831926798620186, -62.44126551166660022 ) ) ;
#13759 = CARTESIAN_POINT ( 'NONE',  ( 47.13393739769619373, -35.30990563848522612, -54.64999999999994884 ) ) ;
#13760 = CARTESIAN_POINT ( 'NONE',  ( 72.83631794868971099, 1.056975075118959939, -69.36644202706580131 ) ) ;
#13761 = CARTESIAN_POINT ( 'NONE',  ( 23.83903582647615593, -17.68687351299132970, -35.87566232877769323 ) ) ;
#13762 = CARTESIAN_POINT ( 'NONE',  ( 9.221354005738056969, -11.63216052016282909, -42.67431283448043189 ) ) ;
#13763 = CARTESIAN_POINT ( 'NONE',  ( 11.27215929994608246, -9.290099381825209335, -59.08403816176677736 ) ) ;
#13764 = CARTESIAN_POINT ( 'NONE',  ( 20.30127474080349970, -42.11618894467939356, -34.64999999999999858 ) ) ;
#13765 = CARTESIAN_POINT ( 'NONE',  ( 23.83903208326023559, -17.68689219033248960, -55.87567441642309518 ) ) ;
#13766 = ADVANCED_FACE ( 'NONE', ( #23817 ), #10864, .T. ) ;
#13767 = VECTOR ( 'NONE', #14679, 999.9999999999998863 ) ;
#13768 = CARTESIAN_POINT ( 'NONE',  ( 22.90092414013790645, -15.63002369583071172, -62.45347908067368081 ) ) ;
#13769 = CARTESIAN_POINT ( 'NONE',  ( 17.98015038839400148, -51.14708712906670485, -74.55381114263370534 ) ) ;
#13770 = CARTESIAN_POINT ( 'NONE',  ( 16.13393739769620083, -1.480959244941480124, -34.70142521051216988 ) ) ;
#13771 = ADVANCED_FACE ( 'NONE', ( #7106 ), #6848, .T. ) ;
#13772 = ORIENTED_EDGE ( 'NONE', *, *, #44316, .F. ) ;
#13773 = CIRCLE ( 'NONE', #43079, 0.5000000000000000000 ) ;
#13774 = CARTESIAN_POINT ( 'NONE',  ( 17.91338361966710124, -8.381531697687238491, -58.64411075632859394 ) ) ;
#13775 = CARTESIAN_POINT ( 'NONE',  ( 64.55375726973680628, 0.9618757110842720559, -60.83484875704370154 ) ) ;
#13776 = ORIENTED_EDGE ( 'NONE', *, *, #28121, .F. ) ;
#13777 = CARTESIAN_POINT ( 'NONE',  ( 22.83850260844683433, -14.06168006131323622, -34.77405416936607452 ) ) ;
#13778 = CARTESIAN_POINT ( 'NONE',  ( 60.67537254770959976, -45.75026917865599785, -47.73567082154549723 ) ) ;
#13779 = DIRECTION ( 'NONE',  ( 0.6888026391158372785, -0.7071067811865469066, 0.1598465650148877537 ) ) ;
#13780 = DIRECTION ( 'NONE',  ( 1.000000000000000000, 3.191443934968493537E-12, -1.224645901081695283E-16 ) ) ;
#13782 = CARTESIAN_POINT ( 'NONE',  ( 8.222960110812529422, -14.58047518749336291, -34.83399806068581483 ) ) ;
#13781 = CARTESIAN_POINT ( 'NONE',  ( 43.27650499216790081, 8.659509414535037308, -70.16183350288429210 ) ) ;
#13783 = CYLINDRICAL_SURFACE ( 'NONE', #41006, 0.5000000000000000000 ) ;
#13784 = DIRECTION ( 'NONE',  ( -1.000000000000000000, 4.735514272306495889E-33, 9.834501533011742432E-16 ) ) ;
#13785 = VERTEX_POINT ( 'NONE', #35897 ) ;
#13786 = ORIENTED_EDGE ( 'NONE', *, *, #9053, .F. ) ;
#13787 = ORIENTED_EDGE ( 'NONE', *, *, #8710, .F. ) ;
#13788 = CARTESIAN_POINT ( 'NONE',  ( -22.83979347564535800, -16.55049450429037350, -54.74432729527064367 ) ) ;
#13789 = FACE_OUTER_BOUND ( 'NONE', #34468, .T. ) ;
#13790 = CARTESIAN_POINT ( 'NONE',  ( 24.58073416742070094, -18.76089852590099838, -35.14999999999999858 ) ) ;
#13791 = ORIENTED_EDGE ( 'NONE', *, *, #18376, .T. ) ;
#13792 = EDGE_CURVE ( 'NONE', #32428, #10642, #15219, .T. ) ;
#13793 = ORIENTED_EDGE ( 'NONE', *, *, #24609, .F. ) ;
#13794 = FACE_OUTER_BOUND ( 'NONE', #36721, .T. ) ;
#13795 = CIRCLE ( 'NONE', #34723, 19.30901699437490038 ) ;
#13796 = DIRECTION ( 'NONE',  ( 0.000000000000000000, 0.000000000000000000, -1.000000000000000000 ) ) ;
#13797 = ORIENTED_EDGE ( 'NONE', *, *, #32015, .T. ) ;
#13798 = CARTESIAN_POINT ( 'NONE',  ( 56.63393739769620083, 19.38381105532069881, 11.34999999999999964 ) ) ;
#13799 = CARTESIAN_POINT ( 'NONE',  ( 52.15433690512320197, -49.89707748732470804, -76.93549829881520452 ) ) ;
#13800 = CARTESIAN_POINT ( 'NONE',  ( 47.81335647231890107, -54.39749252969859583, -54.71582838609030119 ) ) ;
#13801 = CARTESIAN_POINT ( 'NONE',  ( 22.80008605052550053, -19.75734937745210118, -64.18943593078199683 ) ) ;
#13802 = LINE ( 'NONE', #38421, #49826 ) ;
#13803 = CARTESIAN_POINT ( 'NONE',  ( 41.99202299628319679, 13.65299255882769991, -5.712667844576049703 ) ) ;
#13804 = VECTOR ( 'NONE', #31830, 1000.000000000000000 ) ;
#13805 = CARTESIAN_POINT ( 'NONE',  ( 41.41708184556559758, -44.31838638563439758, -4.679819512558520245 ) ) ;
#13806 = CARTESIAN_POINT ( 'NONE',  ( 68.13393739769840352, -50.61618894467879670, -73.25000000000220268 ) ) ;
#13807 = CARTESIAN_POINT ( 'NONE',  ( 68.13393739769620083, 19.38381105532069881, -83.65000000000000568 ) ) ;
#13808 = CARTESIAN_POINT ( 'NONE',  ( 64.12887023277500020, 1.457834087086459895, -69.79194131696009151 ) ) ;
#13809 = CARTESIAN_POINT ( 'NONE',  ( -11.80944000494479873, 2.826328597561450273, -45.03554556751399929 ) ) ;
#13810 = CARTESIAN_POINT ( 'NONE',  ( 65.88232188379309662, 0.1705518047408740023, -17.13915755217489689 ) ) ;
#13811 = ORIENTED_EDGE ( 'NONE', *, *, #23622, .F. ) ;
#13812 = CARTESIAN_POINT ( 'NONE',  ( 14.91526764967280094, -52.98224883304730071, -76.14999999999999147 ) ) ;
#13813 = CARTESIAN_POINT ( 'NONE',  ( 47.18324198357289845, -54.80726809202429450, -54.61058319554170026 ) ) ;
#13814 = DIRECTION ( 'NONE',  ( 5.878706999999999976E-17, 3.795112000000000086E-17, 1.000000000000000000 ) ) ;
#13815 = CARTESIAN_POINT ( 'NONE',  ( 11.61427276589894575, 33.59338474805557695, -44.95328842582802764 ) ) ;
#13816 = LINE ( 'NONE', #2802, #12991 ) ;
#13817 = CARTESIAN_POINT ( 'NONE',  ( 63.47556362806851382, 1.384708701328909886, -68.74455794701600553 ) ) ;
#13818 = CARTESIAN_POINT ( 'NONE',  ( 10.88578148295150072, 33.80155039833079655, -17.73314437547309907 ) ) ;
#13819 = AXIS2_PLACEMENT_3D ( 'NONE', #35780, #39463, #7235 ) ;
#13820 = CARTESIAN_POINT ( 'NONE',  ( 22.77360043544521417, -11.26806673883854337, -45.32308785462522849 ) ) ;
#13821 = EDGE_CURVE ( 'NONE', #3407, #13650, #11, .T. ) ;
#13822 = CARTESIAN_POINT ( 'NONE',  ( 18.38906992954201058, -55.55385106823292318, -76.14999999999999147 ) ) ;
#13823 = CARTESIAN_POINT ( 'NONE',  ( 48.26315220932669803, 23.03099554315049957, -55.14606850299719554 ) ) ;
#13824 = VERTEX_POINT ( 'NONE', #11033 ) ;
#13825 = AXIS2_PLACEMENT_3D ( 'NONE', #11556, #3173, #39842 ) ;
#13826 = CARTESIAN_POINT ( 'NONE',  ( 23.14736512976970317, -16.36076306552550008, -68.88084675407539237 ) ) ;
#13827 = ORIENTED_EDGE ( 'NONE', *, *, #9804, .F. ) ;
#13828 = CARTESIAN_POINT ( 'NONE',  ( 55.91595717589669334, -45.90465048314089103, -17.93019253464870033 ) ) ;
#13829 = FACE_OUTER_BOUND ( 'NONE', #20734, .T. ) ;
#13830 = LINE ( 'NONE', #21417, #12003 ) ;
#13832 = CARTESIAN_POINT ( 'NONE',  ( 55.89862311850580312, 14.72947118455319959, -25.58674067759540094 ) ) ;
#13831 = CARTESIAN_POINT ( 'NONE',  ( 84.30744353797240365, 12.70315578777099930, -47.37637942009979497 ) ) ;
#13833 = CARTESIAN_POINT ( 'NONE',  ( 18.79898847303969944, -22.14612473781209800, -76.82947711988119011 ) ) ;
#13834 = CARTESIAN_POINT ( 'NONE',  ( 12.26282170032090590, 33.38295891277739713, -15.83707920940340053 ) ) ;
#13835 = DIRECTION ( 'NONE',  ( 0.000000000000000000, 0.000000000000000000, 1.000000000000000000 ) ) ;
#13836 = FACE_OUTER_BOUND ( 'NONE', #33049, .T. ) ;
#13837 = B_SPLINE_SURFACE_WITH_KNOTS ( 'NONE', 3, 3, ( 
 ( #24746, #28167, #27917, #48898, #40755, #36293, #4587, #40496, #41017, #4858, #1185, #12998, #11960, #32864, #404, #12732, #20560, #32089, #16390, #48109, #32346, #658, #8013, #28686, #9052, #20825 ),
 ( #48364, #36821, #925, #24220, #23966, #5130, #16923, #21087, #37089, #17180, #154, #39990, #4080, #20053, #36044, #16130, #12463, #44172, #8270, #40244, #20302, #4337, #28431, #8539, #24482, #39850 ),
 ( #23576, #8396, #31186, #27269, #40358, #3444, #32207, #40103, #43531, #47217, #4199, #7631, #20173, #15742, #16000, #15490, #43781, #36411, #36161, #31442, #47721, #8138, #11305, #7370, #19667, #3699 ),
 ( #39594, #7884, #39342, #269, #12326, #16251, #35661, #48228, #44036, #51648, #23830, #28286, #19916, #27523, #31695, #28032, #44286, #31954, #24345, #43280, #3956, #24083, #4455, #20423, #23316, #51393 ),
 ( #35908, #15234, #12079, #19414, #35395, #47471, #11565, #11825, #47976, #27, #27783, #4977, #772, #36943, #41136, #520, #37208, #33521, #21201, #1044, #1309, #9684, #36670, #9439, #20682, #16771 ),
 ( #32722, #8649, #45590, #20948, #25646, #48748, #5248, #5506, #32456, #5754, #21463, #24602, #37461, #49533, #1560, #8918, #12855, #41649, #21711, #40616, #17038, #45069, #28810, #4714, #16506, #32992 ),
 ( #28549, #44810, #13123, #24864, #40876, #17298, #49019, #9174, #29076, #48483, #25132, #12587, #44548, #33258, #13624, #49276, #13368, #29585, #29334, #45334, #25388, #17548, #41389, #50036, #30094, #34550 ),
 ( #42699, #14389, #22748, #14128, #37724, #10986, #9940, #10205, #1819, #6796, #14903, #46121, #26166, #30868, #17800, #49783, #26949, #25899, #2861, #10722, #42176, #33773, #26677, #6276, #38768, #38241 ),
 ( #18308, #42955, #50812, #2334, #38497, #34809, #22233, #46638, #18826, #21973, #41915, #26422, #34280, #30353, #6015, #46895, #7054, #13875, #50304, #29834, #14646, #46382, #10467, #45853, #42440, #6529 ),
 ( #22491, #37985, #2080, #2601, #50554, #30614, #18059, #34027, #18574, #15937, #11503, #31636, #15682, #16185, #19857, #28226, #40044, #23004, #8075, #27460, #23773, #47655, #7305, #43463, #23257, #7564 ) ),
 .UNSPECIFIED., .F., .F., .F.,
 ( 4, 1, 1, 1, 1, 1, 1, 4 ),
 ( 4, 2, 2, 2, 2, 2, 2, 2, 2, 2, 2, 2, 4 ),
 ( -8.374790374999999340E-06, 0.1428571428571430157, 0.2857142857142860315, 0.4285714285714289917, 0.5714285714285709528, 0.7142857142857139685, 0.8571428571428569843, 1.000000000000000000 ),
 ( -6.275064945719149634, -6.131805065669529320, -5.288548408819579549, -4.761512998288360166, -4.381730680025620828, -4.001948361762890372, -3.527220463934470196, -3.134672448649570065, -2.742124433364669933, -2.114047608908829812, -1.109124689779479978, -0.2434889638270290035, 0.005711673629634999964 ),
 .UNSPECIFIED. ) ;
#13838 = DIRECTION ( 'NONE',  ( 0.7071067811865475727, 0.7071067811865475727, 0.000000000000000000 ) ) ;
#13839 = ORIENTED_EDGE ( 'NONE', *, *, #3957, .F. ) ;
#13840 = AXIS2_PLACEMENT_3D ( 'NONE', #13756, #21853, #37860 ) ;
#13841 = EDGE_LOOP ( 'NONE', ( #9952, #51096, #35026, #14203 ) ) ;
#13842 = CARTESIAN_POINT ( 'NONE',  ( 12.20485434016359960, -64.96606476350561366, -16.27613458665190294 ) ) ;
#13844 = EDGE_CURVE ( 'NONE', #10985, #28850, #35800, .T. ) ;
#13843 = CARTESIAN_POINT ( 'NONE',  ( 11.68619745379040076, 33.77259971275340433, -46.13864009073310513 ) ) ;
#13845 = CARTESIAN_POINT ( 'NONE',  ( 8.302058585374817667, -14.33516931341604561, -38.55923738394448463 ) ) ;
#13846 = CARTESIAN_POINT ( 'NONE',  ( 10.72263499592188118, -19.77488192770410080, -55.24448753831254066 ) ) ;
#13847 = LINE ( 'NONE', #1789, #712 ) ;
#13848 = EDGE_LOOP ( 'NONE', ( #31560, #14426, #43016, #47104 ) ) ;
#13849 = EDGE_CURVE ( 'NONE', #13888, #16348, #35144, .T. ) ;
#13850 = CARTESIAN_POINT ( 'NONE',  ( -22.72850738805879800, -18.52594519380850002, -54.52996344323300093 ) ) ;
#13851 = CARTESIAN_POINT ( 'NONE',  ( 53.40279069281933033, 17.93096837380682729, -27.32834194345275591 ) ) ;
#13852 = CARTESIAN_POINT ( 'NONE',  ( 53.08510103305950167, 18.23200443139790039, -48.78473343235920368 ) ) ;
#13853 = ADVANCED_FACE ( 'NONE', ( #30918 ), #51379, .T. ) ;
#13854 = CARTESIAN_POINT ( 'NONE',  ( -21.36606260230379917, 30.88381105532059934, 11.84999999999999964 ) ) ;
#13855 = CARTESIAN_POINT ( 'NONE',  ( 51.43588982009890742, -49.74596692343669702, -76.47300594495250436 ) ) ;
#13856 = CARTESIAN_POINT ( 'NONE',  ( 59.02019150423489435, -47.64116135995680423, -49.73071094584800278 ) ) ;
#13857 = ORIENTED_EDGE ( 'NONE', *, *, #16254, .T. ) ;
#13858 = DIRECTION ( 'NONE',  ( 1.000000000000000000, 2.460964292799963328E-14, 0.000000000000000000 ) ) ;
#13859 = CARTESIAN_POINT ( 'NONE',  ( 66.23540447448930024, 18.72622661238430553, -73.39853292320987066 ) ) ;
#13860 = VERTEX_POINT ( 'NONE', #31427 ) ;
#13861 = CARTESIAN_POINT ( 'NONE',  ( 12.73487495346794240, -55.47150669537813883, -75.56421462368682285 ) ) ;
#13862 = DIRECTION ( 'NONE',  ( 0.000000000000000000, 0.000000000000000000, -1.000000000000000000 ) ) ;
#13863 = AXIS2_PLACEMENT_3D ( 'NONE', #45071, #12081, #522 ) ;
#13864 = CARTESIAN_POINT ( 'NONE',  ( 10.45564697911039964, -10.19920034271800091, -37.25499936915139187 ) ) ;
#13865 = CIRCLE ( 'NONE', #31418, 0.9999999999999940048 ) ;
#13866 = DIRECTION ( 'NONE',  ( -0.2846079131720438693, 0.9586440088791325920, 0.000000000000000000 ) ) ;
#13867 = CARTESIAN_POINT ( 'NONE',  ( 55.67187328886809894, 19.41528913861149874, -75.85395822069619953 ) ) ;
#13868 = CARTESIAN_POINT ( 'NONE',  ( 47.56586919366919375, -54.47692839446759905, -74.72677413543641478 ) ) ;
#13869 = VERTEX_POINT ( 'NONE', #27001 ) ;
#13870 = CARTESIAN_POINT ( 'NONE',  ( 55.25371901226309745, 14.61435477241920111, -16.15016637665110011 ) ) ;
#13871 = CARTESIAN_POINT ( 'NONE',  ( 17.01976985042453805, -8.849193832279162564, -77.99448518340960845 ) ) ;
#13872 = CARTESIAN_POINT ( 'NONE',  ( 56.89024916085300276, -50.49705092091460301, -53.06448611164700679 ) ) ;
#13873 = CARTESIAN_POINT ( 'NONE',  ( 68.13393739769840352, -50.61618894467879670, -73.25000000000220268 ) ) ;
#13874 = FACE_OUTER_BOUND ( 'NONE', #21537, .T. ) ;
#13875 = CARTESIAN_POINT ( 'NONE',  ( 47.10376384439059905, 22.64445950907689564, -75.76537844053849824 ) ) ;
#13876 = CARTESIAN_POINT ( 'NONE',  ( 65.21688447373020381, 1.383136297697689976, -60.93121850368469694 ) ) ;
#13877 = CARTESIAN_POINT ( 'NONE',  ( 60.49059093688927646, -45.82073196953276550, -47.74858579941451353 ) ) ;
#13878 = CARTESIAN_POINT ( 'NONE',  ( 31.58225770014188427, -28.80002732851970393, -65.65000000000000568 ) ) ;
#13879 = CARTESIAN_POINT ( 'NONE',  ( 68.13393739769618662, -1.166188944679350081, -65.65000000000000568 ) ) ;
#13880 = CARTESIAN_POINT ( 'NONE',  ( 15.61576201279904552, -15.99266539877262971, -12.13039854958090125 ) ) ;
#13881 = DIRECTION ( 'NONE',  ( -2.565320000000000120E-13, 1.000000000000000000, -8.628712999999999808E-13 ) ) ;
#13882 = CARTESIAN_POINT ( 'NONE',  ( -5.122171525981340068, 17.49197490117069620, -39.56459775772290044 ) ) ;
#13884 = CARTESIAN_POINT ( 'NONE',  ( 44.62438891534000618, -39.14235344977141295, -67.35856431845091663 ) ) ;
#13883 = DIRECTION ( 'NONE',  ( -0.5685928097855452723, 0.5944782866685394129, 0.5685928097855412755 ) ) ;
#13885 = ADVANCED_FACE ( 'NONE', ( #47456 ), #43513, .T. ) ;
#13886 = CARTESIAN_POINT ( 'NONE',  ( 61.18510815024300342, 14.05093947119190112, -46.73529673433709775 ) ) ;
#13887 = CARTESIAN_POINT ( 'NONE',  ( -0.4147641054028919916, 31.50987371720300700, -49.23002488738170257 ) ) ;
#13888 = VERTEX_POINT ( 'NONE', #27511 ) ;
#13889 = CARTESIAN_POINT ( 'NONE',  ( 53.21185470119179683, -49.46165491835810002, -48.84882516131230545 ) ) ;
#13890 = ORIENTED_EDGE ( 'NONE', *, *, #46340, .F. ) ;
#13891 = CARTESIAN_POINT ( 'NONE',  ( 47.23631910128078459, 8.041419318995805199, -54.68400724043278416 ) ) ;
#13892 = AXIS2_PLACEMENT_3D ( 'NONE', #20120, #32409, #36113 ) ;
#13893 = CARTESIAN_POINT ( 'NONE',  ( 18.13393739769599833, 14.38381105532070059, -49.33749999999999858 ) ) ;
#13894 = CARTESIAN_POINT ( 'NONE',  ( 13.31268657292839919, 19.90328963381880101, -21.89251117597479990 ) ) ;
#13895 = CARTESIAN_POINT ( 'NONE',  ( 57.66356598520189891, 13.88992849527940088, -25.34725557404829743 ) ) ;
#13896 = CARTESIAN_POINT ( 'NONE',  ( 9.119179062043329509, -16.34812076460110220, -49.41972697186909613 ) ) ;
#13897 = CARTESIAN_POINT ( 'NONE',  ( 28.93686911782380022, -26.66694171151199910, -34.75221567031800163 ) ) ;
#13898 = CARTESIAN_POINT ( 'NONE',  ( 52.93745296751840357, 18.38235333221300039, -48.89566025814650629 ) ) ;
#13899 = CARTESIAN_POINT ( 'NONE',  ( 64.66447934098378880, 0.9065823421260970072, -60.75474143511929981 ) ) ;
#13900 = CARTESIAN_POINT ( 'NONE',  ( 16.13393739769620083, -15.61618894467929941, 17.35000000000000142 ) ) ;
#13901 = CARTESIAN_POINT ( 'NONE',  ( 52.56521993351449851, 18.62941884369810097, -28.15000000000000213 ) ) ;
#13902 = AXIS2_PLACEMENT_3D ( 'NONE', #31552, #10638, #26593 ) ;
#13903 = EDGE_LOOP ( 'NONE', ( #1712, #3435, #16362, #4551 ) ) ;
#13904 = CARTESIAN_POINT ( 'NONE',  ( 15.92376862201360233, -23.06350546971500037, -69.57632324310819172 ) ) ;
#13905 = CARTESIAN_POINT ( 'NONE',  ( 73.10923647485390120, 1.096036836948800053, -68.93088433361418765 ) ) ;
#13906 = CARTESIAN_POINT ( 'NONE',  ( 47.40907417377749766, -54.65069181535059784, -54.79938858936409929 ) ) ;
#13907 = DIRECTION ( 'NONE',  ( 0.000000000000000000, 0.000000000000000000, 1.000000000000000000 ) ) ;
#13908 = CARTESIAN_POINT ( 'NONE',  ( 72.83058059882510804, 1.382840740411490188, -62.66598281567230089 ) ) ;
#13909 = CARTESIAN_POINT ( 'NONE',  ( 10.97864148254310024, -65.14694562472800499, -18.17421237900940412 ) ) ;
#13910 = DIRECTION ( 'NONE',  ( 0.000000000000000000, 0.000000000000000000, 1.000000000000000000 ) ) ;
#13911 = CYLINDRICAL_SURFACE ( 'NONE', #31672, 2.999999999999942712 ) ;
#13912 = CARTESIAN_POINT ( 'NONE',  ( 71.27262092911099955, 0.8838110553206740549, -60.53635606803790381 ) ) ;
#13913 = EDGE_CURVE ( 'NONE', #14500, #45267, #7617, .T. ) ;
#13914 = CARTESIAN_POINT ( 'NONE',  ( 12.72604310356256185, -9.703222519325121809, -57.78615345517096102 ) ) ;
#13915 = ORIENTED_EDGE ( 'NONE', *, *, #8913, .T. ) ;
#13916 = CARTESIAN_POINT ( 'NONE',  ( 64.92362553771700107, 1.265401080857980087, -70.52378931128959039 ) ) ;
#13917 = ORIENTED_EDGE ( 'NONE', *, *, #29950, .T. ) ;
#13918 = CARTESIAN_POINT ( 'NONE',  ( 13.92806294471009920, -51.20625127023169654, -22.96889534167359770 ) ) ;
#13919 = CARTESIAN_POINT ( 'NONE',  ( 22.19035827901491587, -12.49215051982365132, -32.30141085084914465 ) ) ;
#13920 = ORIENTED_EDGE ( 'NONE', *, *, #20225, .F. ) ;
#13921 = ADVANCED_FACE ( 'NONE', ( #4697 ), #31742, .T. ) ;
#13922 = PLANE ( 'NONE',  #40938 ) ;
#13923 = DIRECTION ( 'NONE',  ( 0.8320502943378438321, 0.000000000000000000, -0.5547001962252288143 ) ) ;
#13924 = CARTESIAN_POINT ( 'NONE',  ( 9.366543050370410128, -15.61630854221780140, -53.84717978381009829 ) ) ;
#13925 = CARTESIAN_POINT ( 'NONE',  ( 53.23404575114440718, 19.38950307978380039, -76.66833037291560515 ) ) ;
#13926 = ORIENTED_EDGE ( 'NONE', *, *, #50630, .T. ) ;
#13927 = CARTESIAN_POINT ( 'NONE',  ( -22.84941414684771388, -15.61618224896967355, -54.74986855478772441 ) ) ;
#13928 = DIRECTION ( 'NONE',  ( 1.000000000000000000, 0.000000000000000000, 0.000000000000000000 ) ) ;
#13930 = DIRECTION ( 'NONE',  ( 0.000000000000000000, 0.000000000000000000, 1.000000000000000000 ) ) ;
#13929 = AXIS2_PLACEMENT_3D ( 'NONE', #5717, #21673, #13838 ) ;
#13931 = DIRECTION ( 'NONE',  ( 0.000000000000000000, 1.000000000000000000, 0.000000000000000000 ) ) ;
#13932 = CARTESIAN_POINT ( 'NONE',  ( 18.69804252995849936, -7.779857856303769914, -49.39298971242509850 ) ) ;
#13933 = CIRCLE ( 'NONE', #43222, 0.9999999999999940048 ) ;
#13934 = CARTESIAN_POINT ( 'NONE',  ( 23.06214062797170072, -3.616188944679339823, -32.14999999999999858 ) ) ;
#13935 = CARTESIAN_POINT ( 'NONE',  ( 45.74427000726045378, -38.12636687890177001, -61.59833689282645253 ) ) ;
#13936 = ORIENTED_EDGE ( 'NONE', *, *, #9652, .T. ) ;
#13937 = DIRECTION ( 'NONE',  ( 0.000000000000000000, -1.000000000000000000, 0.000000000000000000 ) ) ;
#13938 = CARTESIAN_POINT ( 'NONE',  ( 16.81282819544960105, -23.03547469802990122, -42.70361172200119881 ) ) ;
#13939 = CARTESIAN_POINT ( 'NONE',  ( 8.818632591069450299, -16.16764275473400048, -32.14999999999999858 ) ) ;
#13940 = AXIS2_PLACEMENT_3D ( 'NONE', #39234, #19309, #38725 ) ;
#13941 = CARTESIAN_POINT ( 'NONE',  ( 13.95908631254890153, 19.99149262732870014, -74.56034069004439857 ) ) ;
#13942 = CARTESIAN_POINT ( 'NONE',  ( 20.99565841940248490, -9.290058012837690171, -51.50066301143422720 ) ) ;
#13943 = CARTESIAN_POINT ( 'NONE',  ( 41.02378997853850251, -45.15608259841430083, -5.717059075756449893 ) ) ;
#13944 = CARTESIAN_POINT ( 'NONE',  ( 23.92517191223645057, -14.20005315669235202, -61.45044126124142991 ) ) ;
#13945 = CARTESIAN_POINT ( 'NONE',  ( 24.19548247469570157, -13.88580988780200087, -55.44036573270409463 ) ) ;
#13946 = EDGE_LOOP ( 'NONE', ( #26527, #8627, #493, #46811, #19256, #17953 ) ) ;
#13947 = CARTESIAN_POINT ( 'NONE',  ( 53.68844523372570166, -48.62671425848849793, -26.42115278879650120 ) ) ;
#13948 = CARTESIAN_POINT ( 'NONE',  ( 14.38278649113050101, -51.04890725439349808, -21.89951529875390079 ) ) ;
#13950 = CARTESIAN_POINT ( 'NONE',  ( 42.13477582370718721, -39.77883744432604374, -75.68159061675045507 ) ) ;
#13949 = CARTESIAN_POINT ( 'NONE',  ( 7.712457590364880211, 30.55593849442650267, -15.52623999900530016 ) ) ;
#13951 = ADVANCED_FACE ( 'NONE', ( #49258 ), #24330, .F. ) ;
#13952 = CARTESIAN_POINT ( 'NONE',  ( 12.13393739769649926, 24.18330853958550364, -74.14999999999999147 ) ) ;
#13953 = CARTESIAN_POINT ( 'NONE',  ( -3.429778956281600344, -15.61618894467929763, 6.850000000000000533 ) ) ;
#13954 = ADVANCED_FACE ( 'NONE', ( #41122 ), #17024, .T. ) ;
#13955 = ORIENTED_EDGE ( 'NONE', *, *, #38640, .F. ) ;
#13956 = CARTESIAN_POINT ( 'NONE',  ( -7.612837316484470485, -45.36256704244740234, -5.450487342267620328 ) ) ;
#13957 = EDGE_CURVE ( 'NONE', #2565, #15778, #14555, .T. ) ;
#13958 = CARTESIAN_POINT ( 'NONE',  ( 47.39219260321910099, 23.42968706821420355, -54.83958130849970303 ) ) ;
#13959 = AXIS2_PLACEMENT_3D ( 'NONE', #7709, #98, #32280 ) ;
#13960 = CARTESIAN_POINT ( 'NONE',  ( 56.61928470354429521, -45.32411298099489727, -25.29356197036729981 ) ) ;
#13961 = CARTESIAN_POINT ( 'NONE',  ( 63.49151163952229382, 1.387131204727290124, -62.61203846038919352 ) ) ;
#13962 = DIRECTION ( 'NONE',  ( 0.000000000000000000, 0.000000000000000000, 1.000000000000000000 ) ) ;
#13963 = CARTESIAN_POINT ( 'NONE',  ( 11.55844479304150063, 33.94000257695360290, -16.94284747318280182 ) ) ;
#13964 = EDGE_CURVE ( 'NONE', #15968, #21893, #14189, .T. ) ;
#13965 = CARTESIAN_POINT ( 'NONE',  ( 9.367054778780087076, -16.02018512892366786, -57.82818532426606595 ) ) ;
#13966 = CARTESIAN_POINT ( 'NONE',  ( 71.33393739769628894, 1.883811055320669947, -70.34999999999999432 ) ) ;
#13967 = DIRECTION ( 'NONE',  ( 0.000000000000000000, -1.000000000000000000, 0.000000000000000000 ) ) ;
#13968 = CARTESIAN_POINT ( 'NONE',  ( -0.4123484725610440105, -45.29119327467250145, -35.12503119152799513 ) ) ;
#13969 = CARTESIAN_POINT ( 'NONE',  ( 22.89996919748105952, -15.73990749768590369, -66.45863867653210377 ) ) ;
#13970 = CARTESIAN_POINT ( 'NONE',  ( 51.63654749813390055, 21.60074325994370170, -54.53423779907880231 ) ) ;
#13971 = CARTESIAN_POINT ( 'NONE',  ( 63.54316066981328959, 1.321110558595150142, -69.27633817897910262 ) ) ;
#13972 = CARTESIAN_POINT ( 'NONE',  ( 8.133937397696209715, -63.11543068638779630, -43.74348518090240390 ) ) ;
#13973 = ORIENTED_EDGE ( 'NONE', *, *, #31858, .F. ) ;
#13974 = CARTESIAN_POINT ( 'NONE',  ( 19.97121697892356096, 23.71689785217428437, -18.51157020816790677 ) ) ;
#13975 = CARTESIAN_POINT ( 'NONE',  ( 11.10541747795749856, 31.97147113388010098, -44.25032562221770149 ) ) ;
#13976 = CARTESIAN_POINT ( 'NONE',  ( 72.86184465953650147, 1.051325075269279985, -61.96652996135610181 ) ) ;
#13977 = CIRCLE ( 'NONE', #40746, 2.000000000000000888 ) ;
#13978 = CARTESIAN_POINT ( 'NONE',  ( 65.33367464557400695, -32.03144653440359946, -17.55776891374469884 ) ) ;
#13979 = ORIENTED_EDGE ( 'NONE', *, *, #1467, .F. ) ;
#13980 = CARTESIAN_POINT ( 'NONE',  ( 18.32671892753329956, 19.96087044110830178, -74.35527526576579760 ) ) ;
#13981 = VERTEX_POINT ( 'NONE', #503 ) ;
#13982 = VERTEX_POINT ( 'NONE', #17281 ) ;
#13983 = DIRECTION ( 'NONE',  ( 0.6934629132905124616, 0.5038302981000506442, 0.5150380749100490485 ) ) ;
#13984 = DIRECTION ( 'NONE',  ( 1.681650659181820092E-11, -1.000000000000000000, -2.220771714818679968E-11 ) ) ;
#13985 = ORIENTED_EDGE ( 'NONE', *, *, #14940, .T. ) ;
#13986 = ADVANCED_FACE ( 'NONE', ( #5234 ), #45994, .F. ) ;
#13987 = CARTESIAN_POINT ( 'NONE',  ( 11.09709421595390033, -63.47517990175989411, -44.33319825685619975 ) ) ;
#13988 = CARTESIAN_POINT ( 'NONE',  ( 56.33219501251220152, -46.17132564709319809, -26.19903194913430156 ) ) ;
#13989 = CARTESIAN_POINT ( 'NONE',  ( 62.09157612670949788, -15.61618894467929941, -65.34607522167520699 ) ) ;
#13990 = CARTESIAN_POINT ( 'NONE',  ( 4.133937397696209715, -22.54439217495480108, -35.14999999999999858 ) ) ;
#13991 = ORIENTED_EDGE ( 'NONE', *, *, #21143, .F. ) ;
#13992 = CARTESIAN_POINT ( 'NONE',  ( 45.49907709881001949, 6.867305819722518301, -62.82425208550701257 ) ) ;
#13993 = ORIENTED_EDGE ( 'NONE', *, *, #41328, .T. ) ;
#13994 = CARTESIAN_POINT ( 'NONE',  ( 49.66558981609640000, -45.58299324948399800, -11.70455807815109850 ) ) ;
#13995 = CARTESIAN_POINT ( 'NONE',  ( 22.32569053158739081, -20.61273240502229243, -34.00854356534225786 ) ) ;
#13996 = CARTESIAN_POINT ( 'NONE',  ( 16.06830620277569821, 19.82972613027099840, -20.66285861647660127 ) ) ;
#13997 = DIRECTION ( 'NONE',  ( 0.000000000000000000, 0.000000000000000000, -1.000000000000000000 ) ) ;
#13998 = DIRECTION ( 'NONE',  ( 0.000000000000000000, 0.000000000000000000, 1.000000000000000000 ) ) ;
#13999 = CARTESIAN_POINT ( 'NONE',  ( 47.03253577542010078, -54.46635581206609800, -75.29851419728690587 ) ) ;
#14000 = CARTESIAN_POINT ( 'NONE',  ( 41.36014877832850800, 13.74763066256429944, -5.614912196991499904 ) ) ;
#14001 = EDGE_CURVE ( 'NONE', #32635, #31811, #25867, .T. ) ;
#14002 = CARTESIAN_POINT ( 'NONE',  ( 54.00440282445959639, 13.97710996490090096, -14.09294272437499984 ) ) ;
#14003 = DIRECTION ( 'NONE',  ( 0.000000000000000000, -1.000000000000000000, 0.000000000000000000 ) ) ;
#14004 = B_SPLINE_SURFACE_WITH_KNOTS ( 'NONE', 3, 3, ( 
 ( #51739, #15835, #44579, #25161, #8683, #24893, #17329, #49308, #33292, #20713 ),
 ( #49048, #29361, #9209, #24635, #36977, #41168, #45367, #3540, #12887, #19510 ),
 ( #20977, #4746, #48780, #1074, #36704, #40906, #5016, #13154, #29104, #38537 ),
 ( #41421, #2364, #42471, #49816, #37756, #50587, #10755, #29616, #6048, #17832 ),
 ( #6307, #13908, #42209, #45885, #22265, #9972, #38015, #21748, #21494, #25934 ),
 ( #46412, #33805, #37494, #13655, #45619, #41948, #34583, #49569, #30647, #38273 ),
 ( #30130, #6560, #29865, #22525, #18342, #2633, #14162, #41680, #18605, #14677 ),
 ( #46670, #50332, #22006, #14420, #2110, #5539, #30388, #1594, #10500, #17582 ),
 ( #18089, #34057, #1854, #50067, #46151, #33552, #10239, #34319, #9719, #25678 ),
 ( #26456, #26198, #5788, #39817, #19887, #23803, #43251, #3927, #3669, #35878 ),
 ( #15199, #7601, #31667, #7853, #11794, #35363, #43751, #31158, #43499, #47186 ),
 ( #39309, #35099, #23545, #7338, #33548, #15971, #46929, #31925, #39563, #51362 ),
 ( #23037, #47947, #26714, #14935, #23286, #3152, #27754, #19639, #51100, #27492 ),
 ( #35631, #11273, #3412, #7087, #6828, #27233, #42733, #47690, #19120, #22780 ),
 ( #50844, #19380, #38800, #34844, #2894, #18859, #11013, #51617, #15710, #30900 ),
 ( #26984, #42991, #15462, #39059, #31412, #47440, #11535, #20654, #33226, #24056 ) ),
 .UNSPECIFIED., .F., .F., .F.,
 ( 4, 2, 2, 2, 2, 2, 2, 4 ),
 ( 4, 1, 1, 1, 1, 1, 1, 4 ),
 ( 6.613222000000000237E-15, 0.07216186899281500089, 0.1546325764131659952, 0.2061767685508859860, 0.2319488646197460091, 0.2731842183299219573, 0.3391607842662039962, 0.4123535371017659767 ),
 ( 0.000000000000000000, 0.1428571428571430157, 0.2857142857142860315, 0.4285714285714289917, 0.5714285714285709528, 0.7142857142857139685, 0.8571428571428569843, 1.000000000000000000 ),
 .UNSPECIFIED. ) ;
#14005 = CARTESIAN_POINT ( 'NONE',  ( 51.49462702931260338, 19.89667258983029896, -76.11693519487849358 ) ) ;
#14006 = VECTOR ( 'NONE', #12332, 1000.000000000000000 ) ;
#14007 = CARTESIAN_POINT ( 'NONE',  ( 61.42876130599449880, 13.93441044190779898, -28.04346750121399978 ) ) ;
#14008 = CARTESIAN_POINT ( 'NONE',  ( 22.44091603520600131, -10.94620300795959977, -77.08462780361209354 ) ) ;
#14009 = ORIENTED_EDGE ( 'NONE', *, *, #15240, .F. ) ;
#14010 = CARTESIAN_POINT ( 'NONE',  ( 57.50723796702470025, -47.11618894467930119, -31.98003398042899903 ) ) ;
#14011 = CARTESIAN_POINT ( 'NONE',  ( -11.09336481576520228, -42.12635149981709759, -6.270041010354289845 ) ) ;
#14012 = CARTESIAN_POINT ( 'NONE',  ( 22.90075166721855737, -15.61618922411645727, -44.45281379938008115 ) ) ;
#14013 = CARTESIAN_POINT ( 'NONE',  ( 72.82314924247010879, 1.153605328057900170, -69.33289095355348763 ) ) ;
#14014 = EDGE_CURVE ( 'NONE', #39800, #43431, #9997, .T. ) ;
#14015 = FACE_OUTER_BOUND ( 'NONE', #1984, .T. ) ;
#14016 = LINE ( 'NONE', #9323, #1689 ) ;
#14017 = CARTESIAN_POINT ( 'NONE',  ( 41.13550739303550330, 13.07993219133260077, -4.257233324915049799 ) ) ;
#14018 = ADVANCED_FACE ( 'NONE', ( #37192 ), #32708, .T. ) ;
#14019 = CARTESIAN_POINT ( 'NONE',  ( 65.01129443250870565, 1.391252479931859964, -70.26382307879910627 ) ) ;
#14020 = CARTESIAN_POINT ( 'NONE',  ( 20.13393739768839552, 24.18330853958629945, -74.14999999999999147 ) ) ;
#14021 = CARTESIAN_POINT ( 'NONE',  ( 16.13393739769620083, -15.61618894467929941, -12.65000000000000036 ) ) ;
#14022 = DIRECTION ( 'NONE',  ( 0.3445670372598625963, -0.6174735272333260472, -0.7071067811865442421 ) ) ;
#14023 = CARTESIAN_POINT ( 'NONE',  ( 18.82012537086889736, -51.74366499200339575, -74.55381114263370534 ) ) ;
#14024 = CARTESIAN_POINT ( 'NONE',  ( 11.48393739769620048, -15.61618894467929941, -18.35000000000000142 ) ) ;
#14025 = VERTEX_POINT ( 'NONE', #40857 ) ;
#14026 = CARTESIAN_POINT ( 'NONE',  ( 13.78034597000720041, -8.547433627804178258, -52.46503413336629507 ) ) ;
#14027 =( BOUNDED_CURVE ( )  B_SPLINE_CURVE ( 3, ( #39524, #27708, #19848, #35838 ),
 .UNSPECIFIED., .F., .T. ) 
 B_SPLINE_CURVE_WITH_KNOTS ( ( 4, 4 ),
 ( 1.570796326794897890, 2.356194490192353719 ),
 .UNSPECIFIED. ) 
 CURVE ( )  GEOMETRIC_REPRESENTATION_ITEM ( )  RATIONAL_B_SPLINE_CURVE ( ( 1.000000000000000000, 0.9492530216741901228, 0.9492530216741901228, 1.000000000000000000 ) ) 
 REPRESENTATION_ITEM ( '' )  );
#14028 = CARTESIAN_POINT ( 'NONE',  ( 63.89396393056810552, 1.440335647928530083, -61.72174419063350115 ) ) ;
#14029 = ORIENTED_EDGE ( 'NONE', *, *, #38233, .T. ) ;
#14030 = CARTESIAN_POINT ( 'NONE',  ( 10.28183423898790139, 33.24228732221659754, -17.86145330243139995 ) ) ;
#14031 = CARTESIAN_POINT ( 'NONE',  ( 46.63393739769619373, -36.11618894467930119, -35.14999999999999858 ) ) ;
#14032 = CYLINDRICAL_SURFACE ( 'NONE', #35463, 1.999999999999999556 ) ;
#14033 = CARTESIAN_POINT ( 'NONE',  ( 21.80601387979700689, -21.13100886278292379, -61.75318708358965836 ) ) ;
#14035 = CARTESIAN_POINT ( 'NONE',  ( 17.16956447778131079, -7.705200310418222287, -35.33399669007164334 ) ) ;
#14034 = CARTESIAN_POINT ( 'NONE',  ( 43.36638863507317865, 8.667721898220143828, -69.72695248505642951 ) ) ;
#14036 = CARTESIAN_POINT ( 'NONE',  ( 9.469768305572209499, -17.67289628306980021, -81.23899999999999011 ) ) ;
#14037 = CARTESIAN_POINT ( 'NONE',  ( 43.92196079148860122, -45.97878081364699909, -8.176196025614100193 ) ) ;
#14038 = ORIENTED_EDGE ( 'NONE', *, *, #44073, .F. ) ;
#14039 = VERTEX_POINT ( 'NONE', #20930 ) ;
#14040 = VERTEX_POINT ( 'NONE', #1031 ) ;
#14041 = CARTESIAN_POINT ( 'NONE',  ( 61.27231440712809984, -45.23762772617749306, -46.51050628912130236 ) ) ;
#14042 = CARTESIAN_POINT ( 'NONE',  ( 17.76831794872871839, 10.74943050428838021, -34.64999999999999858 ) ) ;
#14043 = CARTESIAN_POINT ( 'NONE',  ( 54.62261979470829942, -51.56116820793610600, -54.09401641884280565 ) ) ;
#14044 = AXIS2_PLACEMENT_3D ( 'NONE', #40467, #1155, #12434 ) ;
#14045 = ORIENTED_EDGE ( 'NONE', *, *, #4701, .F. ) ;
#14046 = ORIENTED_EDGE ( 'NONE', *, *, #25335, .F. ) ;
#14047 = CARTESIAN_POINT ( 'NONE',  ( 56.46551611171859975, 19.54378718077660082, -53.85224439323700096 ) ) ;
#14049 = CARTESIAN_POINT ( 'NONE',  ( 22.04685344253070056, -19.02417191927269613, -52.61948472975157642 ) ) ;
#14048 = AXIS2_PLACEMENT_3D ( 'NONE', #35219, #51477, #47803 ) ;
#14050 = CARTESIAN_POINT ( 'NONE',  ( 10.64863409883700029, -63.44323389162830296, -23.66469670114080159 ) ) ;
#14051 = ORIENTED_EDGE ( 'NONE', *, *, #11312, .T. ) ;
#14052 = CARTESIAN_POINT ( 'NONE',  ( 71.83393739769618946, 11.38381105532070059, -68.84999999999999432 ) ) ;
#14053 = CARTESIAN_POINT ( 'NONE',  ( 53.39545525563219996, -50.89097375543660462, -76.18303027081991274 ) ) ;
#14054 = CARTESIAN_POINT ( 'NONE',  ( 60.45267362128890198, 14.46205442568079924, -47.42411346985809928 ) ) ;
#14055 = ADVANCED_FACE ( 'NONE', ( #32976, #49001 ), #12313, .T. ) ;
#14056 = CARTESIAN_POINT ( 'NONE',  ( 8.741653217529419706, -18.25074435142980178, -72.90351834778009277 ) ) ;
#14057 = EDGE_CURVE ( 'NONE', #20265, #49113, #42690, .T. ) ;
#14058 = FACE_OUTER_BOUND ( 'NONE', #29949, .T. ) ;
#14059 = CARTESIAN_POINT ( 'NONE',  ( 45.65337825293430285, 13.99440872041340000, -8.155634322266280378 ) ) ;
#14060 = CARTESIAN_POINT ( 'NONE',  ( 41.02005783313650511, -44.34833457011540503, -4.033361466744690205 ) ) ;
#14061 = EDGE_CURVE ( 'NONE', #13869, #49655, #254, .T. ) ;
#14062 = DIRECTION ( 'NONE',  ( 0.000000000000000000, 0.000000000000000000, -1.000000000000000000 ) ) ;
#14063 = CARTESIAN_POINT ( 'NONE',  ( -3.979110003385970540, 17.20385159207049952, -5.632303519440180040 ) ) ;
#14064 = CARTESIAN_POINT ( 'NONE',  ( 64.62682451405710538, 1.027624964385369877, -70.50782134747939267 ) ) ;
#14065 = CARTESIAN_POINT ( 'NONE',  ( -19.86606260230379917, -15.61618894467929408, 6.349999999999999645 ) ) ;
#14066 = CARTESIAN_POINT ( 'NONE',  ( 11.73137203405248385, 10.53025766472752522, -34.79644660940672907 ) ) ;
#14067 = ORIENTED_EDGE ( 'NONE', *, *, #1535, .F. ) ;
#14068 = CARTESIAN_POINT ( 'NONE',  ( 15.05440318628160057, -53.11618894467930119, -76.14999999999999147 ) ) ;
#14069 = CARTESIAN_POINT ( 'NONE',  ( 57.32295481445549967, 19.23251083971900144, -53.14992580837979119 ) ) ;
#14070 = CARTESIAN_POINT ( 'NONE',  ( 10.13410506222094298, 33.50987130397768254, -47.01082059560806670 ) ) ;
#14071 = DIRECTION ( 'NONE',  ( -0.7071067811865475727, 0.000000000000000000, 0.7071067811865475727 ) ) ;
#14072 = CIRCLE ( 'NONE', #51749, 21.19999999999999929 ) ;
#14073 = CARTESIAN_POINT ( 'NONE',  ( 47.07821196700830058, -54.56982298144170329, -75.12266286288350159 ) ) ;
#14074 = ADVANCED_FACE ( 'NONE', ( #14110 ), #45410, .F. ) ;
#14075 = CARTESIAN_POINT ( 'NONE',  ( 63.32591849070559675, 1.327322800621349996, -68.80227784490020326 ) ) ;
#14076 = CARTESIAN_POINT ( 'NONE',  ( 48.21690961261940345, -54.18825503271109767, -54.70306002727500072 ) ) ;
#14077 = CARTESIAN_POINT ( 'NONE',  ( 8.222937779697582883, -14.90190862121987792, -44.53641600745626761 ) ) ;
#14078 = CARTESIAN_POINT ( 'NONE',  ( 56.35191062136929929, 19.31104562819170312, -52.86474270505669892 ) ) ;
#14079 = CARTESIAN_POINT ( 'NONE',  ( 48.19376166029200448, 23.04067999044779924, -54.98857909375249875 ) ) ;
#14080 = ORIENTED_EDGE ( 'NONE', *, *, #27106, .F. ) ;
#14081 = CARTESIAN_POINT ( 'NONE',  ( 14.18091115246270029, -22.39322721071389921, -77.43649130894630161 ) ) ;
#14082 = ORIENTED_EDGE ( 'NONE', *, *, #14800, .F. ) ;
#14083 = DIRECTION ( 'NONE',  ( 0.000000000000000000, 0.000000000000000000, -1.000000000000000000 ) ) ;
#14084 = DIRECTION ( 'NONE',  ( -0.4640893551880615475, -0.8857883891771946017, 0.000000000000000000 ) ) ;
#14085 = CARTESIAN_POINT ( 'NONE',  ( 23.04646839281239679, -11.63207206855464015, -77.62566222703568997 ) ) ;
#14087 = CARTESIAN_POINT ( 'NONE',  ( 53.88904214046930008, 17.16505862634210189, -26.27980819959719838 ) ) ;
#14086 = CARTESIAN_POINT ( 'NONE',  ( 84.08245047910018855, 13.26582018360060111, -47.41523600659849791 ) ) ;
#14088 = CARTESIAN_POINT ( 'NONE',  ( 12.48870797616079997, -21.65397505889350072, -71.12571408330069289 ) ) ;
#14089 = CARTESIAN_POINT ( 'NONE',  ( 22.90145954991004729, -15.72428510330016849, -78.85226058911112546 ) ) ;
#14090 = DIRECTION ( 'NONE',  ( 0.8660254037844383745, -0.5000000000000003331, 0.000000000000000000 ) ) ;
#14091 = CARTESIAN_POINT ( 'NONE',  ( 26.13393739769619728, -15.61618894467929941, -5.966499999999999915 ) ) ;
#14092 = ORIENTED_EDGE ( 'NONE', *, *, #46861, .F. ) ;
#14093 = DIRECTION ( 'NONE',  ( -0.3502816565540492477, 0.000000000000000000, 0.9366444154970182678 ) ) ;
#14094 = ORIENTED_EDGE ( 'NONE', *, *, #38375, .F. ) ;
#14095 = CARTESIAN_POINT ( 'NONE',  ( 12.30205595647329986, -64.73832649162540065, -15.96528926833489948 ) ) ;
#14096 = FACE_OUTER_BOUND ( 'NONE', #19662, .T. ) ;
#14097 = CARTESIAN_POINT ( 'NONE',  ( -33.86606260230181675, -10.73525358442780941, -57.75434594776561426 ) ) ;
#14098 = FACE_OUTER_BOUND ( 'NONE', #22166, .T. ) ;
#14099 = ORIENTED_EDGE ( 'NONE', *, *, #1639, .T. ) ;
#14100 = ORIENTED_EDGE ( 'NONE', *, *, #828, .F. ) ;
#14101 = CARTESIAN_POINT ( 'NONE',  ( -20.79634969123249988, -28.70049512919520041, -52.86954696638409246 ) ) ;
#14102 = DIRECTION ( 'NONE',  ( 0.000000000000000000, 0.000000000000000000, -1.000000000000000000 ) ) ;
#14103 = CARTESIAN_POINT ( 'NONE',  ( 53.56302256516740101, -49.38660883080410713, -49.17075139047770449 ) ) ;
#14104 = CARTESIAN_POINT ( 'NONE',  ( 52.05055437614630165, 19.18114209767879785, -49.15813440252989608 ) ) ;
#14105 = CARTESIAN_POINT ( 'NONE',  ( 60.35865778877810328, -2.352205281898970490, -15.82496069747729983 ) ) ;
#14106 = CARTESIAN_POINT ( 'NONE',  ( 50.57709999312749716, -48.61618543841219520, -76.21964823130220168 ) ) ;
#14107 = CARTESIAN_POINT ( 'NONE',  ( 58.05620727321760199, -49.44730473131560444, -51.87485358542139835 ) ) ;
#14108 = VERTEX_POINT ( 'NONE', #37445 ) ;
#14109 = CARTESIAN_POINT ( 'NONE',  ( 21.35490516321459609, -9.654190832205486572, -33.52126662197601092 ) ) ;
#14110 = FACE_OUTER_BOUND ( 'NONE', #16952, .T. ) ;
#14111 = ORIENTED_EDGE ( 'NONE', *, *, #43268, .T. ) ;
#14112 = CARTESIAN_POINT ( 'NONE',  ( 15.09836090117696017, -7.705192450957612849, -53.25066628357330956 ) ) ;
#14113 = VECTOR ( 'NONE', #17161, 1000.000000000000000 ) ;
#14114 = CYLINDRICAL_SURFACE ( 'NONE', #25310, 0.4999999999999364397 ) ;
#14115 = VECTOR ( 'NONE', #41683, 1000.000000000000000 ) ;
#14116 = CARTESIAN_POINT ( 'NONE',  ( 18.29348190141509889, -23.16092983672059802, -40.42375661169609913 ) ) ;
#14117 = EDGE_CURVE ( 'NONE', #48021, #12701, #40964, .T. ) ;
#14118 = CARTESIAN_POINT ( 'NONE',  ( 13.64640607913560011, -50.80567383909779977, -21.56020319207080149 ) ) ;
#14119 = CARTESIAN_POINT ( 'NONE',  ( 53.99861951552289696, 19.51405001656310034, -76.30342085868839774 ) ) ;
#14120 = CARTESIAN_POINT ( 'NONE',  ( 47.60133233420110344, -54.52312452709470136, -74.50414561666529778 ) ) ;
#14121 = VERTEX_POINT ( 'NONE', #9921 ) ;
#14122 = EDGE_CURVE ( 'NONE', #50075, #18993, #17533, .T. ) ;
#14123 = CARTESIAN_POINT ( 'NONE',  ( 55.69613912887059826, 14.53694977389559995, -16.67869178985480261 ) ) ;
#14124 = CARTESIAN_POINT ( 'NONE',  ( 47.71697316577869685, 23.26510924299340033, -55.03111162414960233 ) ) ;
#14125 = CARTESIAN_POINT ( 'NONE',  ( 57.32828653034319899, -50.41406207962300812, -53.00038473087199975 ) ) ;
#14126 = CARTESIAN_POINT ( 'NONE',  ( 10.66652299674349891, -20.07151597450609870, -41.62953446819029324 ) ) ;
#14127 = CARTESIAN_POINT ( 'NONE',  ( 3.633937397696210159, -19.08029055981709732, -35.14999999999999858 ) ) ;
#14128 = CARTESIAN_POINT ( 'NONE',  ( 47.56773526946430763, 23.32812596456290066, -74.36162932837530093 ) ) ;
#14129 = CARTESIAN_POINT ( 'NONE',  ( 20.13393738107516029, -55.41568638132210367, -20.08918511024506159 ) ) ;
#14130 = CARTESIAN_POINT ( 'NONE',  ( 41.14609131925150365, -45.53782844434120136, -6.107216659010040516 ) ) ;
#14131 = CARTESIAN_POINT ( 'NONE',  ( 12.79282753983206611, -65.49328885638416864, -23.41071104114353574 ) ) ;
#14132 = B_SPLINE_CURVE_WITH_KNOTS ( 'NONE', 3,
 ( #34423, #30491, #42313, #5890, #14523, #1698, #33391, #41783, #10604, #1440 ),
 .UNSPECIFIED., .F., .F.,
 ( 4, 1, 1, 1, 1, 1, 1, 4 ),
 ( 0.000000000000000000, 0.05993458473492679905, 0.1391535157985444027, 0.2183724468621642545, 0.2975913779257818859, 0.3768103089894005997, 0.4560292400530182033, 0.4999984997257186370 ),
 .UNSPECIFIED. ) ;
#14133 = DIRECTION ( 'NONE',  ( 0.000000000000000000, -1.000000000000000000, 0.000000000000000000 ) ) ;
#14134 = DIRECTION ( 'NONE',  ( 0.000000000000000000, 0.000000000000000000, 1.000000000000000000 ) ) ;
#14135 = EDGE_CURVE ( 'NONE', #20725, #20296, #29568, .T. ) ;
#14136 = CARTESIAN_POINT ( 'NONE',  ( 82.55595867320781167, 14.40020173682131954, -47.71333528890980347 ) ) ;
#14137 = CARTESIAN_POINT ( 'NONE',  ( -0.2761815207641740155, 19.58270920947809657, -35.04694460471009876 ) ) ;
#14139 = CARTESIAN_POINT ( 'NONE',  ( 43.70467631200691727, -39.04050123248909188, -71.92343701204615058 ) ) ;
#14138 = CARTESIAN_POINT ( 'NONE',  ( 65.01767771978660448, 0.8838110553206759423, -60.52272727272730179 ) ) ;
#14140 = EDGE_CURVE ( 'NONE', #20583, #48341, #50205, .T. ) ;
#14141 = CARTESIAN_POINT ( 'NONE',  ( 64.93393739769619799, 11.38381105532070059, -61.94999999999999574 ) ) ;
#14142 = CARTESIAN_POINT ( 'NONE',  ( -26.85818705357539926, 10.53358274763490066, -55.57881993978430302 ) ) ;
#14143 = ORIENTED_EDGE ( 'NONE', *, *, #47982, .F. ) ;
#14144 = CARTESIAN_POINT ( 'NONE',  ( 53.29389463559500228, -49.43182142001269597, -48.95065373416729670 ) ) ;
#14145 = ORIENTED_EDGE ( 'NONE', *, *, #30165, .T. ) ;
#14146 = AXIS2_PLACEMENT_3D ( 'NONE', #41976, #13937, #2139 ) ;
#14147 = CARTESIAN_POINT ( 'NONE',  ( 17.21347160910339724, 21.88381105532300097, -76.14999999999999147 ) ) ;
#14148 = CARTESIAN_POINT ( 'NONE',  ( 53.67901547079682700, -51.32026565108220240, -75.56983433779308257 ) ) ;
#14149 = CARTESIAN_POINT ( 'NONE',  ( 13.47926327417509995, 19.82353983917930051, -21.90689185999260147 ) ) ;
#14150 = CARTESIAN_POINT ( 'NONE',  ( 57.62061476366090318, 13.90145536118990144, -25.55370966833229929 ) ) ;
#14151 = CARTESIAN_POINT ( 'NONE',  ( 14.86072368984219949, -8.679223790466799926, -49.89504055825069884 ) ) ;
#14153 = CARTESIAN_POINT ( 'NONE',  ( 50.98562399990609606, 19.60288930407019947, -76.14999999999999147 ) ) ;
#14152 = CIRCLE ( 'NONE', #24142, 2.999999999999999112 ) ;
#14154 = CARTESIAN_POINT ( 'NONE',  ( 53.50489543215090293, 18.19328726694199716, -49.20411598972469847 ) ) ;
#14155 = CARTESIAN_POINT ( 'NONE',  ( 64.76223432283440218, 1.187296498006439993, -60.79044767480839795 ) ) ;
#14156 = DIRECTION ( 'NONE',  ( -1.000000000000000000, 0.000000000000000000, 0.000000000000000000 ) ) ;
#14157 = VERTEX_POINT ( 'NONE', #19843 ) ;
#14158 = B_SPLINE_CURVE_WITH_KNOTS ( 'NONE', 3,
 ( #44931, #10329, #45972, #2203, #42037, #49139, #25760, #25505, #29448, #17409 ),
 .UNSPECIFIED., .F., .F.,
 ( 4, 1, 1, 1, 1, 1, 1, 4 ),
 ( 0.4999984997257186370, 0.5352481711166380274, 0.6144671021802581290, 0.6936860332438941068, 0.7729049643075164289, 0.8521238953711365305, 0.9313428264347566321, 1.000000000000000000 ),
 .UNSPECIFIED. ) ;
#14159 = CARTESIAN_POINT ( 'NONE',  ( 11.48089076940169839, -21.93567517873050221, -33.98952930500309577 ) ) ;
#14160 = CARTESIAN_POINT ( 'NONE',  ( 49.40539548398250247, -53.49785366680099941, -54.15746054658189479 ) ) ;
#14161 = CARTESIAN_POINT ( 'NONE',  ( 24.04493594278903146, -15.61063966555162708, -49.79210729519485312 ) ) ;
#14162 = CARTESIAN_POINT ( 'NONE',  ( 73.12314370215899828, 1.096110717717209804, -62.39142878032480155 ) ) ;
#14163 = CARTESIAN_POINT ( 'NONE',  ( 11.41950678098469929, -65.35719241412380143, -18.15863199444450160 ) ) ;
#14164 = CARTESIAN_POINT ( 'NONE',  ( 71.44880243016270072, 1.326666718054979821, -60.91913985162000245 ) ) ;
#14165 = LINE ( 'NONE', #1857, #48540 ) ;
#14166 = CARTESIAN_POINT ( 'NONE',  ( 71.36799767121769378, 0.8859637708054480809, -60.59611492242089525 ) ) ;
#14167 = CARTESIAN_POINT ( 'NONE',  ( 8.223454620794861114, -15.61605491354059971, -46.50766849176290663 ) ) ;
#14168 = VERTEX_POINT ( 'NONE', #7038 ) ;
#14169 = CARTESIAN_POINT ( 'NONE',  ( 64.84946247134770658, 1.186701509386330011, -70.56202332290359891 ) ) ;
#14170 = ORIENTED_EDGE ( 'NONE', *, *, #20069, .F. ) ;
#14171 = CARTESIAN_POINT ( 'NONE',  ( 10.49392349455719931, -63.33912771724479995, -45.62648268597099843 ) ) ;
#14172 = CARTESIAN_POINT ( 'NONE',  ( 14.06330661571832863, -7.911076412684214354, -47.20899900762205448 ) ) ;
#14173 = VERTEX_POINT ( 'NONE', #15152 ) ;
#14174 = CARTESIAN_POINT ( 'NONE',  ( 3.633937397696210159, -8.399310579809009525, -34.64999999999999858 ) ) ;
#14175 = CARTESIAN_POINT ( 'NONE',  ( 56.94152841858620206, 19.37848640203839778, -53.44912207968510387 ) ) ;
#14176 = PLANE ( 'NONE',  #34519 ) ;
#14177 = CARTESIAN_POINT ( 'NONE',  ( 52.10718133714609479, 18.87579468230029889, -76.73077508321010498 ) ) ;
#14178 = ORIENTED_EDGE ( 'NONE', *, *, #704, .T. ) ;
#14179 = CARTESIAN_POINT ( 'NONE',  ( 11.55867067850401853, -65.29213368257272521, -47.38009360245612811 ) ) ;
#14180 = DIRECTION ( 'NONE',  ( 0.1564344650402237358, -0.9876883405951387696, 0.000000000000000000 ) ) ;
#14181 = CARTESIAN_POINT ( 'NONE',  ( 53.63393739769619373, 31.88381105532059934, 11.84999999999999964 ) ) ;
#14182 = CARTESIAN_POINT ( 'NONE',  ( 20.99558350725401112, -9.289997995219156479, -43.50069810257394920 ) ) ;
#14183 = CARTESIAN_POINT ( 'NONE',  ( 7.895084482184580921, -15.93871443592090031, -54.77987702475120102 ) ) ;
#14184 = ADVANCED_FACE ( 'NONE', ( #11747 ), #35834, .T. ) ;
#14185 = CARTESIAN_POINT ( 'NONE',  ( 12.14992655622318551, -22.52878033032515148, -48.17433562066877784 ) ) ;
#14186 = CARTESIAN_POINT ( 'NONE',  ( 45.01043142363850791, -38.04361682771764208, -65.26752630117056242 ) ) ;
#14187 = ORIENTED_EDGE ( 'NONE', *, *, #12656, .T. ) ;
#14188 = AXIS2_PLACEMENT_3D ( 'NONE', #24295, #35608, #51597 ) ;
#14189 = CIRCLE ( 'NONE', #12502, 1.999999999999998224 ) ;
#14190 = CARTESIAN_POINT ( 'NONE',  ( 56.56121202467220144, -46.20600250404840637, -26.26606259789259923 ) ) ;
#14191 = CARTESIAN_POINT ( 'NONE',  ( 9.151664503347209489, -18.21514239443270355, -41.11923310072890558 ) ) ;
#14192 = AXIS2_PLACEMENT_3D ( 'NONE', #4456, #20683, #24085 ) ;
#14193 = AXIS2_PLACEMENT_3D ( 'NONE', #32746, #24886, #5531 ) ;
#14194 = CARTESIAN_POINT ( 'NONE',  ( 8.880059303195860565, -15.24727849168679938, -32.14999999999999858 ) ) ;
#14195 = VECTOR ( 'NONE', #9401, 999.9999999999998863 ) ;
#14196 = B_SPLINE_CURVE_WITH_KNOTS ( 'NONE', 3,
 ( #18524, #50501, #14852, #30561, #46581, #30815, #47101 ),
 .UNSPECIFIED., .F., .F.,
 ( 4, 1, 1, 1, 4 ),
 ( 0.6416644417609895790, 0.6584949831503380535, 0.7723299887668140240, 0.8861649943832899945, 1.000000000000000000 ),
 .UNSPECIFIED. ) ;
#14197 = CARTESIAN_POINT ( 'NONE',  ( 13.94115586785109961, 19.96087044110830178, -74.35527526576591129 ) ) ;
#14198 = DIRECTION ( 'NONE',  ( 1.000000000000000000, 0.000000000000000000, 0.000000000000000000 ) ) ;
#14199 = B_SPLINE_CURVE_WITH_KNOTS ( 'NONE', 3,
 ( #18215, #5910, #29733, #45749, #25795, #6173, #30258, #22132, #41804, #46540 ),
 .UNSPECIFIED., .F., .F.,
 ( 4, 1, 1, 1, 1, 1, 1, 4 ),
 ( 0.000000000000000000, 0.05183927916845956774, 0.1310582102320191900, 0.2102771412957371577, 0.2894960723593013596, 0.3687150034230238238, 0.4479339344865834738, 0.4999968673859223056 ),
 .UNSPECIFIED. ) ;
#14200 = CARTESIAN_POINT ( 'NONE',  ( 45.76559021992609644, -45.11804673858839720, -7.588959103897489733 ) ) ;
#14201 = CARTESIAN_POINT ( 'NONE',  ( 9.855508381251125272, -10.73142913993969394, -60.71829047705996629 ) ) ;
#14202 = CARTESIAN_POINT ( 'NONE',  ( 22.29884365131979962, -21.09128269666270228, -65.73882677097451221 ) ) ;
#14203 = ORIENTED_EDGE ( 'NONE', *, *, #43013, .T. ) ;
#14204 = CARTESIAN_POINT ( 'NONE',  ( 54.80419448789260173, -47.33494133938750537, -25.92210209326049863 ) ) ;
#14205 = CARTESIAN_POINT ( 'NONE',  ( 55.66118929916900271, -50.90930937580999682, -75.01110568612280360 ) ) ;
#14207 = CARTESIAN_POINT ( 'NONE',  ( 46.63604585716099393, -39.11158712134929516, -34.65000333419789769 ) ) ;
#14206 = CARTESIAN_POINT ( 'NONE',  ( 3.156509474638800050, 24.30419543549970030, -8.938496486758239712 ) ) ;
#14209 = EDGE_CURVE ( 'NONE', #42105, #13573, #44336, .T. ) ;
#14208 = CARTESIAN_POINT ( 'NONE',  ( 53.63393739769619373, 30.88381105532059934, 10.84999999999999964 ) ) ;
#14210 = CARTESIAN_POINT ( 'NONE',  ( 3.205734167420700498, -15.61618894467930652, -23.15000000000000213 ) ) ;
#14211 = VERTEX_POINT ( 'NONE', #47138 ) ;
#14212 = CARTESIAN_POINT ( 'NONE',  ( 23.62413055734840128, 17.52287609088140030, -35.14999999999999858 ) ) ;
#14213 = CARTESIAN_POINT ( 'NONE',  ( 47.47773078780689815, 23.37030520192059768, -54.73382622973240075 ) ) ;
#14214 = CARTESIAN_POINT ( 'NONE',  ( 11.12952202957884573, -9.453362623693060129, -65.07532067451190017 ) ) ;
#14215 = CARTESIAN_POINT ( 'NONE',  ( 63.28685848367280897, 1.187931651339009909, -62.25809267083580778 ) ) ;
#14216 = DIRECTION ( 'NONE',  ( 0.000000000000000000, -1.000000000000000000, 0.000000000000000000 ) ) ;
#14217 = CARTESIAN_POINT ( 'NONE',  ( 11.78008937361119912, 33.90493106804039769, -16.70885295318199937 ) ) ;
#14218 = DIRECTION ( 'NONE',  ( 0.000000000000000000, -1.000000000000000000, 0.000000000000000000 ) ) ;
#14219 = DIRECTION ( 'NONE',  ( 1.062456999999999985E-16, -7.719205000000000365E-17, 1.000000000000000000 ) ) ;
#14220 = CARTESIAN_POINT ( 'NONE',  ( 14.28038030992529528, -32.47778390180254604, -34.79644291222909658 ) ) ;
#14221 = CARTESIAN_POINT ( 'NONE',  ( 55.85157221570699448, 15.39592295138489852, -26.24938425740990056 ) ) ;
#14222 = AXIS2_PLACEMENT_3D ( 'NONE', #2276, #5954, #18251 ) ;
#14223 = CARTESIAN_POINT ( 'NONE',  ( 53.46638755025719547, 20.54076140048909949, -53.27253650584940203 ) ) ;
#14224 = VECTOR ( 'NONE', #45181, 1000.000000000000000 ) ;
#14225 = CARTESIAN_POINT ( 'NONE',  ( 63.46161254120319484, 1.063296977482639960, -69.40459734810629300 ) ) ;
#14226 = CARTESIAN_POINT ( 'NONE',  ( 12.21895752911560074, -64.97095625756598736, -16.28177273609240316 ) ) ;
#14227 = CARTESIAN_POINT ( 'NONE',  ( 18.13393739769620083, -32.62399965035220362, -35.14999999999999858 ) ) ;
#14228 = CARTESIAN_POINT ( 'NONE',  ( 20.07088694243709881, -21.46793974735500043, -73.15866903151078304 ) ) ;
#14229 = CARTESIAN_POINT ( 'NONE',  ( 11.10530294771320037, 31.88305279702909800, -44.25053028539870326 ) ) ;
#14230 = CARTESIAN_POINT ( 'NONE',  ( 72.80915813965889072, 1.367045641526529964, -62.38166218803879559 ) ) ;
#14231 = AXIS2_PLACEMENT_3D ( 'NONE', #3851, #43935, #16147 ) ;
#14232 = AXIS2_PLACEMENT_3D ( 'NONE', #42597, #6955, #29989 ) ;
#14233 = CARTESIAN_POINT ( 'NONE',  ( 66.32946235891380127, -32.37525661809159772, -18.17791974922089793 ) ) ;
#14234 = CARTESIAN_POINT ( 'NONE',  ( 10.40721251143282977, -10.10600624985592333, -80.75144566232624754 ) ) ;
#14235 = ORIENTED_EDGE ( 'NONE', *, *, #25631, .F. ) ;
#14236 = ORIENTED_EDGE ( 'NONE', *, *, #4320, .F. ) ;
#14237 = CARTESIAN_POINT ( 'NONE',  ( 48.85702442728309336, 22.78471410673780184, -55.29194429107999298 ) ) ;
#14238 = VECTOR ( 'NONE', #37691, 1000.000000000000000 ) ;
#14239 = CARTESIAN_POINT ( 'NONE',  ( 49.84506783314736822, -1.611968319188557208, -15.88097192665358470 ) ) ;
#14240 = VERTEX_POINT ( 'NONE', #3619 ) ;
#14241 = CARTESIAN_POINT ( 'NONE',  ( 13.00893739769619906, -65.51843714052719747, -47.75434321273180416 ) ) ;
#14242 = CARTESIAN_POINT ( 'NONE',  ( 56.09983961787049367, -45.96733836777529802, -25.91450243792759878 ) ) ;
#14243 = CARTESIAN_POINT ( 'NONE',  ( 51.13393739769659874, -50.61618894467899565, 11.34999999999999964 ) ) ;
#14244 = CARTESIAN_POINT ( 'NONE',  ( 63.49388541862201407, 1.387412027389909985, -68.69511434646409498 ) ) ;
#14245 = ORIENTED_EDGE ( 'NONE', *, *, #42591, .F. ) ;
#14246 = DIRECTION ( 'NONE',  ( 0.000000000000000000, 0.000000000000000000, -1.000000000000000000 ) ) ;
#14247 = CARTESIAN_POINT ( 'NONE',  ( 46.80774876147005159, 7.000071986378179290, -56.28089294811472598 ) ) ;
#14248 = ORIENTED_EDGE ( 'NONE', *, *, #32660, .T. ) ;
#14249 = CARTESIAN_POINT ( 'NONE',  ( 45.07857577476659827, -46.11250025407090192, -9.026857998747990663 ) ) ;
#14250 = EDGE_CURVE ( 'NONE', #1196, #23424, #27704, .T. ) ;
#14251 = CARTESIAN_POINT ( 'NONE',  ( 51.92091365860093788, 1.594025306073798331, -18.96882430330588321 ) ) ;
#14252 = CARTESIAN_POINT ( 'NONE',  ( 16.60577464339750264, 19.88381273883279832, -20.14978695510530216 ) ) ;
#14253 = CARTESIAN_POINT ( 'NONE',  ( 68.13393739806289773, -1.666188944679350081, -42.14999999999999858 ) ) ;
#14254 = EDGE_CURVE ( 'NONE', #29295, #7519, #46033, .T. ) ;
#14255 = CARTESIAN_POINT ( 'NONE',  ( 20.02379755832415498, -21.17856784602826181, -46.75851876412026087 ) ) ;
#14256 = EDGE_CURVE ( 'NONE', #4764, #10139, #26412, .T. ) ;
#14257 = DIRECTION ( 'NONE',  ( 0.000000000000000000, 0.000000000000000000, 1.000000000000000000 ) ) ;
#14258 = CARTESIAN_POINT ( 'NONE',  ( 47.18324198357279897, -54.80726809202429450, -74.17417149933299925 ) ) ;
#14259 = CARTESIAN_POINT ( 'NONE',  ( 64.44913706933721187, 13.88381324743080114, -12.01620149882199939 ) ) ;
#14260 = ADVANCED_FACE ( 'NONE', ( #3361 ), #10968, .T. ) ;
#14261 = DIRECTION ( 'NONE',  ( 0.9441882088883087887, -0.3294064756441308917, 0.000000000000000000 ) ) ;
#14262 = VECTOR ( 'NONE', #18581, 1000.000000000000000 ) ;
#14263 = CIRCLE ( 'NONE', #2553, 29.70020322226740106 ) ;
#14264 = CARTESIAN_POINT ( 'NONE',  ( 51.76047950956219523, 20.08324044957950250, -76.04144537520539870 ) ) ;
#14265 = CARTESIAN_POINT ( 'NONE',  ( 59.34853940138299322, 13.89250407454670011, -25.97953579402879853 ) ) ;
#14266 = CLOSED_SHELL ( 'NONE', ( #17675, #15781, #44001, #35360, #2161, #9858, #982, #50169, #10343, #37698, #34167, #46997, #2376, #16988, #12790, #14414, #8155, #20634, #49600, #1754, #40445, #6587, #37421, #19029, #38299, #12649, #10004, #11374, #21912, #38529, #50927, #11465, #4539, #33054, #36760, #7874, #49075, #38937, #51775, #27125, #41711, #20141, #12257, #1494, #3765, #13766, #15228, #38573, #31509, #49712, #15664, #50820, #4426, #37325, #34272, #1239, #16859, #25800, #19908, #13545, #17158, #24445, #21723, #11361, #579, #50235, #28839, #3033, #28331, #37979, #27912, #7500, #39704, #738, #21461, #11821, #49179, #6105, #7296, #3064, #11908, #49538, #25219, #44161, #46443, #35727, #49593, #12414, #14596, #34268, #40680, #10220, #49774, #19617, #18220, #3823, #51002, #39760, #50365, #43034, #32601, #32899, #13443, #38404, #13605, #36026, #18247, #31720, #34638, #40615, #46703, #24769, #43178, #9497, #27380, #49853, #46148, #23441, #40870, #16922, #3102, #8152, #22865, #10122, #6312, #45190, #33883, #17113, #20609, #40217, #48756, #6336, #24251, #6598, #44480, #22755, #22871, #5326, #12588, #25192, #29967, #33819, #20403, #10402, #25964, #34937, #44351, #3693, #1429, #44687, #45037, #5495, #13065, #1574, #48141, #21081, #48892, #46087, #34299, #40414, #23380, #34604, #8408, #12721, #38082, #49399, #24803, #1508, #5261, #34580, #18996, #47647, #45424, #41957, #43615, #45270, #7957, #49947, #32490, #51408, #7966, #19281, #48208, #16714, #19922, #10959, #32596, #7223, #29903, #14909, #26181, #7376, #19807, #29333, #3980, #34417, #40032, #49109, #33161, #24525, #4431, #51225, #4366, #15554, #15299, #491, #1850, #18572, #21625, #35298, #5932, #38020, #49810, #28175, #24346, #49138, #30009, #43592, #43248 ) ) ;
#14267 = CARTESIAN_POINT ( 'NONE',  ( 23.20097397146510332, -12.20389611180989853, -79.14432001126608895 ) ) ;
#14268 = B_SPLINE_SURFACE_WITH_KNOTS ( 'NONE', 3, 3, ( 
 ( #50807, #10977, #31886, #31375, #51578, #43965 ),
 ( #27712, #15422, #47906, #7559, #11235, #43209 ),
 ( #27455, #4129, #3886, #43457, #12007, #27196 ),
 ( #8070, #20105, #14895, #26944, #23503, #39528 ),
 ( #43712, #42950, #7046, #22998, #39019, #39267 ),
 ( #3628, #35056, #3369, #51062, #35590, #15676 ),
 ( #31630, #31121, #7815, #23768, #39780, #47146 ),
 ( #7299, #23250, #19342, #20613, #36876, #20881 ),
 ( #974, #29260, #33188, #12260, #40295, #48682 ),
 ( #8323, #40804, #8589, #28743, #12784, #36095 ),
 ( #32138, #201, #48155, #17227, #16700, #16976 ) ),
 .UNSPECIFIED., .F., .F., .F.,
 ( 4, 1, 1, 1, 1, 1, 1, 1, 4 ),
 ( 4, 2, 4 ),
 ( 0.000000000000000000, 0.1250000000000000000, 0.2500000000000000000, 0.3750000000000000000, 0.5000000000000000000, 0.6250000000000000000, 0.7500000000000000000, 0.8750000000000000000, 1.000001225116700088 ),
 ( -0.8336663705528200019, -0.6216045683949800171, -0.5133023023850340483 ),
 .UNSPECIFIED. ) ;
#14269 = ORIENTED_EDGE ( 'NONE', *, *, #40321, .T. ) ;
#14270 = CARTESIAN_POINT ( 'NONE',  ( 68.13393739769620083, 11.38381105532070059, -65.65000000000000568 ) ) ;
#14271 = CARTESIAN_POINT ( 'NONE',  ( -5.339937516195930378, -47.24367322247450574, -5.307116475879639417 ) ) ;
#14272 = DIRECTION ( 'NONE',  ( 0.000000000000000000, 0.000000000000000000, -1.000000000000000000 ) ) ;
#14274 = EDGE_CURVE ( 'NONE', #29692, #46452, #13421, .T. ) ;
#14273 = CARTESIAN_POINT ( 'NONE',  ( 72.72056432233058842, 1.396834109478129804, -68.84999999999999432 ) ) ;
#14275 = CARTESIAN_POINT ( 'NONE',  ( 61.21108842818934903, -45.54439463435623026, -47.60783370497615863 ) ) ;
#14276 = DIRECTION ( 'NONE',  ( 1.000000000000000000, 0.000000000000000000, 0.000000000000000000 ) ) ;
#14277 = CARTESIAN_POINT ( 'NONE',  ( 72.33393739770313857, 10.88381105532029380, -69.85000000000677289 ) ) ;
#14278 = CARTESIAN_POINT ( 'NONE',  ( 1.027904703268279984, -42.68661147989060112, -15.65000000000000036 ) ) ;
#14279 = CARTESIAN_POINT ( 'NONE',  ( 41.67695037001420388, 12.61921981549519955, -4.028589964710610261 ) ) ;
#14280 = CARTESIAN_POINT ( 'NONE',  ( 68.13393739769630031, 16.88381105532302939, -68.79999999999976978 ) ) ;
#14281 = CARTESIAN_POINT ( 'NONE',  ( 9.937051593248220627, -53.70417188095279926, -34.65604926186119172 ) ) ;
#14282 = CARTESIAN_POINT ( 'NONE',  ( 56.46551611171859975, 19.54378718077660082, -53.85224439323700096 ) ) ;
#14283 = CARTESIAN_POINT ( 'NONE',  ( 76.64341730006429998, -43.20802362345402514, -14.27775341716986368 ) ) ;
#14284 = ORIENTED_EDGE ( 'NONE', *, *, #32329, .T. ) ;
#14285 = CARTESIAN_POINT ( 'NONE',  ( 11.67472944696460146, -21.58461912274730210, -49.77159047720329710 ) ) ;
#14286 = CARTESIAN_POINT ( 'NONE',  ( 63.47399051652649860, 1.241979851175949889, -62.01152168070590420 ) ) ;
#14287 = ORIENTED_EDGE ( 'NONE', *, *, #13844, .F. ) ;
#14288 = CARTESIAN_POINT ( 'NONE',  ( 22.90093737722143885, -16.50198483417289097, -68.49448457974217774 ) ) ;
#14289 = DIRECTION ( 'NONE',  ( 0.000000000000000000, 0.000000000000000000, 1.000000000000000000 ) ) ;
#14290 = PLANE ( 'NONE',  #42170 ) ;
#14291 = CARTESIAN_POINT ( 'NONE',  ( 23.60684277050431845, -18.32442953224958515, -61.61821266173036804 ) ) ;
#14292 = CARTESIAN_POINT ( 'NONE',  ( 45.76294970761291836, 8.847485351248307595, -58.11021846651873091 ) ) ;
#14293 = EDGE_CURVE ( 'NONE', #18008, #3359, #15753, .T. ) ;
#14294 = CARTESIAN_POINT ( 'NONE',  ( 9.283276003734380666, -17.14284064744749969, -81.23899999999999011 ) ) ;
#14295 = CARTESIAN_POINT ( 'NONE',  ( 44.98351759279099582, -46.11098047250180088, -8.963088896874140232 ) ) ;
#14296 = ORIENTED_EDGE ( 'NONE', *, *, #32922, .T. ) ;
#14297 = VERTEX_POINT ( 'NONE', #14886 ) ;
#14298 = ORIENTED_EDGE ( 'NONE', *, *, #37139, .T. ) ;
#14299 = CARTESIAN_POINT ( 'NONE',  ( 61.43669518452560396, -45.19312879481820033, -46.80308561288980229 ) ) ;
#14300 = CARTESIAN_POINT ( 'NONE',  ( -21.28852503460515067, -26.72198803963431857, -53.52383174611850336 ) ) ;
#14301 = AXIS2_PLACEMENT_3D ( 'NONE', #13133, #1317, #33784 ) ;
#14302 = VERTEX_POINT ( 'NONE', #46881 ) ;
#14303 = AXIS2_PLACEMENT_3D ( 'NONE', #24852, #16239, #28275 ) ;
#14304 = ORIENTED_EDGE ( 'NONE', *, *, #34879, .T. ) ;
#14305 = DIRECTION ( 'NONE',  ( -1.129617809262089999E-08, -1.032305616123179888E-08, 1.000000000000000000 ) ) ;
#14306 = CARTESIAN_POINT ( 'NONE',  ( 11.97532584595513683, -21.02755421326961383, -53.16115279593655885 ) ) ;
#14307 = FACE_OUTER_BOUND ( 'NONE', #8694, .T. ) ;
#14308 = VERTEX_POINT ( 'NONE', #26935 ) ;
#14309 = CARTESIAN_POINT ( 'NONE',  ( 21.35165372367944059, -21.64041393852045658, -49.78022346639211548 ) ) ;
#14310 = CARTESIAN_POINT ( 'NONE',  ( 53.83039865239790345, -50.85522019609880573, -76.11625649690100204 ) ) ;
#14311 = CARTESIAN_POINT ( 'NONE',  ( 60.73605156023749885, 14.28962119872829994, -47.17434044904690182 ) ) ;
#14312 = EDGE_CURVE ( 'NONE', #29849, #37903, #19335, .T. ) ;
#14313 = CARTESIAN_POINT ( 'NONE',  ( 10.89649166119029999, -21.46049469889319994, -72.74508048565289187 ) ) ;
#14314 = DIRECTION ( 'NONE',  ( -0.2260571801428140071, 0.000000000000000000, 0.9741140340359949468 ) ) ;
#14315 = CARTESIAN_POINT ( 'NONE',  ( 43.41584083283380124, 13.83172669772440067, -6.498305962786799839 ) ) ;
#14316 = CARTESIAN_POINT ( 'NONE',  ( 42.00588769014139956, -43.70649907349879726, -4.238533582109900166 ) ) ;
#14317 = LINE ( 'NONE', #26092, #28673 ) ;
#14318 = CYLINDRICAL_SURFACE ( 'NONE', #41587, 2.000000000000006217 ) ;
#14319 = CARTESIAN_POINT ( 'NONE',  ( 64.79641848607099064, 1.369332017692449943, -70.29624551492651108 ) ) ;
#14320 = CARTESIAN_POINT ( 'NONE',  ( 38.67452568954060155, -36.11618894467930119, -81.65000000000000568 ) ) ;
#14321 = CARTESIAN_POINT ( 'NONE',  ( 28.28038400710292422, -12.15208732954159920, -34.79644660940672907 ) ) ;
#14322 = ORIENTED_EDGE ( 'NONE', *, *, #12022, .T. ) ;
#14323 = CARTESIAN_POINT ( 'NONE',  ( 14.51946302495829855, -52.60116553372549930, -76.03823174343609992 ) ) ;
#14324 = CARTESIAN_POINT ( 'NONE',  ( 47.20824439995679711, -54.78745981783090713, -54.64190477282399883 ) ) ;
#14325 = ADVANCED_FACE ( 'NONE', ( #31364 ), #51566, .T. ) ;
#14326 = CARTESIAN_POINT ( 'NONE',  ( 46.15610874489437521, -40.10233669974212489, -56.20102867703486282 ) ) ;
#14327 = CARTESIAN_POINT ( 'NONE',  ( 11.13393739769619906, 32.28996932333459569, -43.76018303787720498 ) ) ;
#14328 = TOROIDAL_SURFACE ( 'NONE', #29398, 19.56371635397779940, 1.000000000000000000 ) ;
#14329 =( BOUNDED_CURVE ( )  B_SPLINE_CURVE ( 2, ( #30780, #46805, #10894 ),
 .UNSPECIFIED., .F., .T. ) 
 B_SPLINE_CURVE_WITH_KNOTS ( ( 3, 3 ),
 ( 0.1896353341141479854, 2.672615408357010391 ),
 .UNSPECIFIED. ) 
 CURVE ( )  GEOMETRIC_REPRESENTATION_ITEM ( )  RATIONAL_B_SPLINE_CURVE ( ( 1.004410800606350129, 1.032237589135669875, 1.032581180562780032 ) ) 
 REPRESENTATION_ITEM ( '' )  );
#14330 = VECTOR ( 'NONE', #10636, 1000.000000000000114 ) ;
#14331 = CARTESIAN_POINT ( 'NONE',  ( 47.06489453142850010, -54.53966941020699721, -75.17791912558919876 ) ) ;
#14332 = CARTESIAN_POINT ( 'NONE',  ( 63.23977555071250123, 1.186515949276290227, -68.96459770949519452 ) ) ;
#14333 = CARTESIAN_POINT ( 'NONE',  ( 48.31166452737429751, -54.24939451924300471, -55.28583570618040710 ) ) ;
#14334 = CARTESIAN_POINT ( 'NONE',  ( 61.75019796695539753, -46.11618894467930119, -28.15000000000000213 ) ) ;
#14335 = LINE ( 'NONE', #30304, #4981 ) ;
#14336 = CARTESIAN_POINT ( 'NONE',  ( 18.20458473725057758, -23.32129814441765703, -46.20904756636038968 ) ) ;
#14337 = CARTESIAN_POINT ( 'NONE',  ( 48.08520103749209795, 23.02686870344080106, -54.72849252353350380 ) ) ;
#14338 = VERTEX_POINT ( 'NONE', #44473 ) ;
#14339 = CARTESIAN_POINT ( 'NONE',  ( 22.88559359100839785, -17.65523230413990063, -70.94053896172950147 ) ) ;
#14340 = VERTEX_POINT ( 'NONE', #9094 ) ;
#14341 = CARTESIAN_POINT ( 'NONE',  ( 71.44807725908989937, 0.8904513541338849869, -70.65165619965239330 ) ) ;
#14342 = DIRECTION ( 'NONE',  ( -0.9117581046690675928, 0.4107275965530798323, 0.000000000000000000 ) ) ;
#14343 = CARTESIAN_POINT ( 'NONE',  ( 74.17629866868290378, -33.11618894467940066, -65.34607522167520699 ) ) ;
#14345 = CARTESIAN_POINT ( 'NONE',  ( 52.69501071984650054, 18.49099401042879975, -27.56727973799209863 ) ) ;
#14344 = CARTESIAN_POINT ( 'NONE',  ( 83.66059785054299880, 13.61222787120309974, -47.23564833931240514 ) ) ;
#14346 = EDGE_CURVE ( 'NONE', #51329, #39, #34287, .T. ) ;
#14347 = CARTESIAN_POINT ( 'NONE',  ( 20.34823716830939944, -9.960904602951780262, -80.15667222455330432 ) ) ;
#14348 = CARTESIAN_POINT ( 'NONE',  ( -33.86606260230380627, -15.61618894467929941, -56.14999999999999858 ) ) ;
#14349 = CARTESIAN_POINT ( 'NONE',  ( 11.27233786307961516, -21.94241352851297933, -42.21600145475415644 ) ) ;
#14350 = DIRECTION ( 'NONE',  ( 0.000000000000000000, 0.000000000000000000, 1.000000000000000000 ) ) ;
#14351 = ORIENTED_EDGE ( 'NONE', *, *, #10520, .T. ) ;
#14352 = CARTESIAN_POINT ( 'NONE',  ( 8.711199217769845404, -48.88697541251521983, -34.82978046822304918 ) ) ;
#14353 = EDGE_CURVE ( 'NONE', #50419, #21662, #33287, .T. ) ;
#14354 = EDGE_LOOP ( 'NONE', ( #252, #47506, #20460, #15301, #27167, #38481, #41720 ) ) ;
#14355 = B_SPLINE_CURVE_WITH_KNOTS ( 'NONE', 3,
 ( #44831, #8936, #49032, #29089, #45086, #9195, #25147, #22252, #42978, #10487, #26443, #35084, #42459, #6814, #18326, #6294, #41934, #14406 ),
 .UNSPECIFIED., .F., .F.,
 ( 4, 2, 2, 2, 2, 2, 2, 2, 4 ),
 ( 0.000000000000000000, 0.06249999926200177497, 0.1249999985240035499, 0.1874999977860053180, 0.2499999970480070999, 0.3124999963100088540, 0.3749999955720106359, 0.4374999948340124178, 0.4999999940960141998 ),
 .UNSPECIFIED. ) ;
#14356 = VERTEX_POINT ( 'NONE', #4898 ) ;
#14357 = ADVANCED_FACE ( 'NONE', ( #11998 ), #10079, .T. ) ;
#14358 = CARTESIAN_POINT ( 'NONE',  ( 12.16231664501490073, -64.67747237300790175, -15.91745067707079819 ) ) ;
#14359 = CARTESIAN_POINT ( 'NONE',  ( 21.24080222438520948, -9.496642911058136960, -39.22927993103733257 ) ) ;
#14360 = CARTESIAN_POINT ( 'NONE',  ( 37.88393739769619373, -42.11618894467939356, -35.14999999999999858 ) ) ;
#14361 = LINE ( 'NONE', #1533, #40080 ) ;
#14362 = ORIENTED_EDGE ( 'NONE', *, *, #31660, .T. ) ;
#14363 = ORIENTED_EDGE ( 'NONE', *, *, #11357, .T. ) ;
#14364 = CARTESIAN_POINT ( 'NONE',  ( -22.65260339427180014, -11.81924193806499979, -54.48195099813599995 ) ) ;
#14365 = CARTESIAN_POINT ( 'NONE',  ( 56.83355978135429609, 14.76424485735420156, -26.24603836142980029 ) ) ;
#14366 = CARTESIAN_POINT ( 'NONE',  ( 9.627976488470578076, -13.67980814752628227, -45.54496871415931736 ) ) ;
#14367 = CARTESIAN_POINT ( 'NONE',  ( 59.28498198370309780, -3.120077556817410169, -15.67198597102109936 ) ) ;
#14368 = CARTESIAN_POINT ( 'NONE',  ( 51.08268012532420244, -48.61618608430239874, -76.44192738162151102 ) ) ;
#14369 = CARTESIAN_POINT ( 'NONE',  ( 60.62314435019690251, -45.49594437324660134, -47.31712978262719815 ) ) ;
#14370 = EDGE_CURVE ( 'NONE', #30581, #26391, #21, .T. ) ;
#14371 = ORIENTED_EDGE ( 'NONE', *, *, #28294, .T. ) ;
#14372 = CARTESIAN_POINT ( 'NONE',  ( 52.57246135266279907, -49.85409740178759819, -27.98331546413460202 ) ) ;
#14374 = CARTESIAN_POINT ( 'NONE',  ( 70.83393739769690001, 16.88381105531749782, -71.50000000000000000 ) ) ;
#14373 = CIRCLE ( 'NONE', #11018, 0.5000000000000000000 ) ;
#14375 = ORIENTED_EDGE ( 'NONE', *, *, #28323, .T. ) ;
#14376 = DIRECTION ( 'NONE',  ( 1.000000000000000000, 0.000000000000000000, 0.000000000000000000 ) ) ;
#14377 = CARTESIAN_POINT ( 'NONE',  ( 53.28808755212359216, -45.11618894467940066, -12.64220374978839878 ) ) ;
#14378 = EDGE_CURVE ( 'NONE', #25374, #10844, #36536, .T. ) ;
#14379 = CARTESIAN_POINT ( 'NONE',  ( 17.14114147996649962, -7.833368920533811064, -47.55346040742190183 ) ) ;
#14380 = CARTESIAN_POINT ( 'NONE',  ( 12.80406157968080016, -50.65217205733890182, -21.33287590401240053 ) ) ;
#14381 = CARTESIAN_POINT ( 'NONE',  ( 56.68161733921530043, 19.46491649270590329, -74.14923232710660272 ) ) ;
#14382 = CARTESIAN_POINT ( 'NONE',  ( 47.61773728487339952, -54.54450626489860099, -74.19830160072660874 ) ) ;
#14383 = CARTESIAN_POINT ( 'NONE',  ( 57.12074889286160584, 13.88381105532070059, -16.42681869645199910 ) ) ;
#14384 = CARTESIAN_POINT ( 'NONE',  ( 47.78812228777269411, 23.20823330413379892, -54.85175909439769981 ) ) ;
#14385 = CARTESIAN_POINT ( 'NONE',  ( 56.72395159914599816, -50.68578410791079847, -53.71484871590959642 ) ) ;
#14386 = CARTESIAN_POINT ( 'NONE',  ( 18.59784447790319817, -9.007730646819130271, -38.46077722564549362 ) ) ;
#14387 = CARTESIAN_POINT ( 'NONE',  ( 22.90080846266944548, -15.61618871746016879, -44.84718732428002852 ) ) ;
#14388 = ORIENTED_EDGE ( 'NONE', *, *, #31026, .T. ) ;
#14389 = CARTESIAN_POINT ( 'NONE',  ( 47.57154853779519499, 23.33333473833040017, -74.17376148238459166 ) ) ;
#14390 = CARTESIAN_POINT ( 'NONE',  ( 64.92606658240281092, 0.9214125008369580261, -60.57945272938810177 ) ) ;
#14391 = DIRECTION ( 'NONE',  ( 0.000000000000000000, 0.000000000000000000, -1.000000000000000000 ) ) ;
#14392 = CARTESIAN_POINT ( 'NONE',  ( 68.13393739769598767, -2.032350560840590070, -29.09832030244560741 ) ) ;
#14393 = CARTESIAN_POINT ( 'NONE',  ( 48.42521416700790127, -56.37491125791819968, -64.38029159777090626 ) ) ;
#14394 = DIRECTION ( 'NONE',  ( 0.6415444970810870728, -0.4854844151940968522, 0.5939070136550171908 ) ) ;
#14395 = CARTESIAN_POINT ( 'NONE',  ( 82.34852001369439733, 14.40950277491920062, -47.72348187592570667 ) ) ;
#14396 = CARTESIAN_POINT ( 'NONE',  ( -9.348292170159599124, 13.97290946334260120, -42.89544360152859781 ) ) ;
#14398 = CARTESIAN_POINT ( 'NONE',  ( 46.13944883215520321, -40.23853505593529434, -55.73485720529632204 ) ) ;
#14397 = DIRECTION ( 'NONE',  ( 0.000000000000000000, 1.000000000000000000, 0.000000000000000000 ) ) ;
#14399 = CARTESIAN_POINT ( 'NONE',  ( 22.76950726391698154, -11.20136067151295833, -71.32103239729558197 ) ) ;
#14400 = CARTESIAN_POINT ( 'NONE',  ( -32.74859963536999885, -5.990261158790339380, -56.32353328738960130 ) ) ;
#14401 = VERTEX_POINT ( 'NONE', #24200 ) ;
#14402 = CARTESIAN_POINT ( 'NONE',  ( 52.85417444733669612, -49.65285076575479906, -48.78849744257649945 ) ) ;
#14403 = AXIS2_PLACEMENT_3D ( 'NONE', #25603, #14350, #22712 ) ;
#14404 = VERTEX_POINT ( 'NONE', #44671 ) ;
#14405 = CARTESIAN_POINT ( 'NONE',  ( 43.81109536264059301, 8.794139443671282308, -67.21774360442289264 ) ) ;
#14406 = CARTESIAN_POINT ( 'NONE',  ( 24.04527493495583457, -15.61618894149694192, -73.79233149842438877 ) ) ;
#14407 = CARTESIAN_POINT ( 'NONE',  ( 13.86461347845260050, 19.85757936412190006, -22.12913923296040153 ) ) ;
#14408 = CARTESIAN_POINT ( 'NONE',  ( 56.44408186407410000, 14.18700613804810118, -25.29404973353000230 ) ) ;
#14409 = CARTESIAN_POINT ( 'NONE',  ( 12.93140221574939908, -21.90000363839990172, -49.10285124761459485 ) ) ;
#14410 = CARTESIAN_POINT ( 'NONE',  ( 28.74617114340210122, -26.59579177408749828, -34.66275921114419134 ) ) ;
#14411 = CARTESIAN_POINT ( 'NONE',  ( 53.40032980815939823, 18.21520279426259847, -49.16199818797040422 ) ) ;
#14412 = CARTESIAN_POINT ( 'NONE',  ( 55.49709987488149210, -45.80398698926880030, -16.40980232892859902 ) ) ;
#14413 = CARTESIAN_POINT ( 'NONE',  ( 15.10238578887313388, -43.89919387818888907, -61.51477253168710035 ) ) ;
#14414 = ADVANCED_FACE ( 'NONE', ( #48090 ), #385, .T. ) ;
#14415 = ORIENTED_EDGE ( 'NONE', *, *, #27076, .F. ) ;
#14416 = CARTESIAN_POINT ( 'NONE',  ( 20.98937642605960008, -9.450845481008398608, -36.99984868542069449 ) ) ;
#14417 = EDGE_CURVE ( 'NONE', #9032, #16350, #48531, .T. ) ;
#14418 = CARTESIAN_POINT ( 'NONE',  ( 11.78395113718259957, -65.42271807190199695, -17.88069380536639841 ) ) ;
#14419 = CARTESIAN_POINT ( 'NONE',  ( 11.89098172404790077, 34.12547406030940778, -47.42262565194260304 ) ) ;
#14420 = CARTESIAN_POINT ( 'NONE',  ( 72.94195630468689728, 1.327322800621349996, -62.49772215509980100 ) ) ;
#14421 = CARTESIAN_POINT ( 'NONE',  ( 10.77197593517290031, -64.97501271978380544, -18.02693217527109937 ) ) ;
#14422 = CARTESIAN_POINT ( 'NONE',  ( 53.02879952360030558, -49.61047114518112267, -49.09530619433566301 ) ) ;
#14423 = CARTESIAN_POINT ( 'NONE',  ( 17.25281598583982401, -22.57971318746314893, -67.29646813281843265 ) ) ;
#14424 = CARTESIAN_POINT ( 'NONE',  ( 9.807798170205042965, -10.75447755698773200, -45.00063938649487483 ) ) ;
#14425 = CARTESIAN_POINT ( 'NONE',  ( 19.92014648307743130, -22.58664708275372135, -45.84940091502108572 ) ) ;
#14426 = ORIENTED_EDGE ( 'NONE', *, *, #3205, .T. ) ;
#14427 = CARTESIAN_POINT ( 'NONE',  ( 64.77932207159149414, 0.8936201581567889685, -70.62461353540280129 ) ) ;
#14428 = EDGE_LOOP ( 'NONE', ( #39074, #9508, #18747, #22921, #32571 ) ) ;
#14429 = CARTESIAN_POINT ( 'NONE',  ( 10.76935505275949900, -63.13244369400850076, -45.20656299583839655 ) ) ;
#14430 = FACE_OUTER_BOUND ( 'NONE', #6913, .T. ) ;
#14431 = ORIENTED_EDGE ( 'NONE', *, *, #29492, .T. ) ;
#14432 = LINE ( 'NONE', #33816, #27530 ) ;
#14433 = CARTESIAN_POINT ( 'NONE',  ( 57.16059586828990291, 19.35048569732870050, -53.44447636780819977 ) ) ;
#14434 = CARTESIAN_POINT ( 'NONE',  ( 52.22858155672869884, 18.58352814647409801, -77.10495058268929824 ) ) ;
#14435 = EDGE_LOOP ( 'NONE', ( #8851, #9348, #2375, #12440 ) ) ;
#14436 = FACE_OUTER_BOUND ( 'NONE', #28824, .T. ) ;
#14437 = PRODUCT_DEFINITION_SHAPE ( 'NONE', 'NONE',  #46257 ) ;
#14438 = FACE_OUTER_BOUND ( 'NONE', #23807, .T. ) ;
#14439 = CARTESIAN_POINT ( 'NONE',  ( 0.03808610503982497175, -26.96777797282045697, -34.73334895013598356 ) ) ;
#14440 = CARTESIAN_POINT ( 'NONE',  ( 46.25525774125583922, -33.99486860111965569, -44.64999999999999858 ) ) ;
#14441 = EDGE_CURVE ( 'NONE', #34841, #19315, #2513, .T. ) ;
#14442 = CARTESIAN_POINT ( 'NONE',  ( 15.28400219184669950, -23.81742849744160040, -60.32520219920449733 ) ) ;
#14443 = CARTESIAN_POINT ( 'NONE',  ( 16.13393739769620083, -38.61618894467930119, 4.943674098299959851 ) ) ;
#14444 = CARTESIAN_POINT ( 'NONE',  ( 44.79480296850380228, -38.01802765133241735, -66.34561246062233408 ) ) ;
#14445 = EDGE_CURVE ( 'NONE', #41111, #28142, #18407, .T. ) ;
#14446 = VERTEX_POINT ( 'NONE', #640 ) ;
#14447 = CARTESIAN_POINT ( 'NONE',  ( 57.31659485773750617, -45.81640764159139678, -26.26798733862809954 ) ) ;
#14448 = CARTESIAN_POINT ( 'NONE',  ( 16.66132627741290051, -8.184597272991679162, -57.75520862408900058 ) ) ;
#14449 = CIRCLE ( 'NONE', #34522, 3.569999999999939444 ) ;
#14450 = CARTESIAN_POINT ( 'NONE',  ( 9.442544990296008578, -13.22597753588140002, -32.14999999999999858 ) ) ;
#14451 = CARTESIAN_POINT ( 'NONE',  ( 16.13393739769620083, -15.61618894467929941, -6.649999999999999467 ) ) ;
#14452 = CARTESIAN_POINT ( 'NONE',  ( 14.02313605303129762, 20.10118929730710136, -74.92517623884199907 ) ) ;
#14453 = DIRECTION ( 'NONE',  ( 0.000000000000000000, 0.000000000000000000, -1.000000000000000000 ) ) ;
#14454 = B_SPLINE_CURVE_WITH_KNOTS ( 'NONE', 3,
 ( #31299, #15346, #51253, #47328, #23692, #27638, #6709, #34722, #43132, #10901, #2773, #15605, #42874, #35772, #7744, #26598, #26867, #42615 ),
 .UNSPECIFIED., .F., .F.,
 ( 4, 2, 2, 2, 2, 2, 2, 2, 4 ),
 ( 0.4999988908354166539, 0.5624990294809895097, 0.6249991681265623100, 0.6874993067721352213, 0.7499994454177081327, 0.8124995840632810440, 0.8749997227088539553, 0.9374998613544269777, 1.000000000000000000 ),
 .UNSPECIFIED. ) ;
#14455 = CARTESIAN_POINT ( 'NONE',  ( 45.45696629059829519, -45.23491596358309863, -8.052740744783449145 ) ) ;
#14456 = CARTESIAN_POINT ( 'NONE',  ( 24.04493568462940090, -15.61079658766591649, -61.50745927652321399 ) ) ;
#14457 = CARTESIAN_POINT ( 'NONE',  ( 17.10857306732300032, -7.428832471405029558, -63.04538311481149293 ) ) ;
#14458 = ORIENTED_EDGE ( 'NONE', *, *, #22986, .T. ) ;
#14459 = CARTESIAN_POINT ( 'NONE',  ( 53.02464382135099896, -49.36657896306630278, -27.03748697953070135 ) ) ;
#14460 = CARTESIAN_POINT ( 'NONE',  ( 55.34407407925619538, -50.75763021394610064, -75.61144563105409588 ) ) ;
#14462 = DIRECTION ( 'NONE',  ( 0.000000000000000000, 0.000000000000000000, 1.000000000000000000 ) ) ;
#14461 = FACE_OUTER_BOUND ( 'NONE', #3907, .T. ) ;
#14463 = CARTESIAN_POINT ( 'NONE',  ( 12.06284766121009966, -63.44323389162830296, -22.25048313876769868 ) ) ;
#14464 = CARTESIAN_POINT ( 'NONE',  ( 22.90071877914020249, -15.61618922162072565, -76.45281474520940890 ) ) ;
#14465 = EDGE_LOOP ( 'NONE', ( #39452, #21036 ) ) ;
#14466 = CARTESIAN_POINT ( 'NONE',  ( -6.547582927393579943, -46.10825334578329660, -4.746448008273789654 ) ) ;
#14467 = CARTESIAN_POINT ( 'NONE',  ( 47.46890301732349826, 23.37795228188129926, -54.75658226910749704 ) ) ;
#14468 = CARTESIAN_POINT ( 'NONE',  ( 61.13393739769620083, -15.61618894467929941, -84.38499399519520239 ) ) ;
#14469 = CARTESIAN_POINT ( 'NONE',  ( 83.95017614158776098, -44.74867211454660776, -47.46180894508327697 ) ) ;
#14470 = CARTESIAN_POINT ( 'NONE',  ( 71.33393739769670105, 0.9098571636355720083, -61.17674615073129729 ) ) ;
#14471 = CARTESIAN_POINT ( 'NONE',  ( 11.57186432615969984, 33.71257428197279182, -16.50172565923969970 ) ) ;
#14472 = CARTESIAN_POINT ( 'NONE',  ( 51.65858043804030331, 17.70229134975009799, -76.94737799408660806 ) ) ;
#14473 = CARTESIAN_POINT ( 'NONE',  ( 52.97622283594260040, 18.35180465121920079, -48.78091467802120462 ) ) ;
#14474 = DIRECTION ( 'NONE',  ( 0.7071067811865475727, -0.7071067811865475727, 0.000000000000000000 ) ) ;
#14475 = DIRECTION ( 'NONE',  ( 0.000000000000000000, 1.000000000000000000, 0.000000000000000000 ) ) ;
#14476 = CARTESIAN_POINT ( 'NONE',  ( 54.85732554741899492, 16.42837036004689821, -26.50322149960979701 ) ) ;
#14477 = EDGE_CURVE ( 'NONE', #19842, #34653, #20748, .T. ) ;
#14478 = CARTESIAN_POINT ( 'NONE',  ( 50.03007040746459921, 5.621799825072190337, -76.14999999999999147 ) ) ;
#14479 = CIRCLE ( 'NONE', #50476, 16.50000000000000000 ) ;
#14480 = CARTESIAN_POINT ( 'NONE',  ( 63.40501886558961075, 1.309113972621119837, -69.02948859405739768 ) ) ;
#14481 = FACE_OUTER_BOUND ( 'NONE', #8702, .T. ) ;
#14482 = CARTESIAN_POINT ( 'NONE',  ( 8.222290034161709116, -15.61613760572089937, -44.79233150823699816 ) ) ;
#14483 = CARTESIAN_POINT ( 'NONE',  ( 71.17456103962899761, 1.276058558775509999, -60.69120887205459525 ) ) ;
#14484 = CARTESIAN_POINT ( 'NONE',  ( 10.97897909118739967, 32.05266905124919674, -44.74264738324500001 ) ) ;
#14485 = AXIS2_PLACEMENT_3D ( 'NONE', #29172, #45173, #9286 ) ;
#14486 = CARTESIAN_POINT ( 'NONE',  ( 72.85590616764901029, 0.9486745332815790244, -61.94714277540219882 ) ) ;
#14487 = DIRECTION ( 'NONE',  ( 0.6676418852213139576, 0.2329255526947012489, -0.7071067811865460184 ) ) ;
#14488 = ORIENTED_EDGE ( 'NONE', *, *, #32904, .T. ) ;
#14489 = CARTESIAN_POINT ( 'NONE',  ( 18.32671526147660046, 19.96087670211870346, -74.14993703734479880 ) ) ;
#14490 = VERTEX_POINT ( 'NONE', #32844 ) ;
#14491 = ORIENTED_EDGE ( 'NONE', *, *, #36357, .F. ) ;
#14492 = CARTESIAN_POINT ( 'NONE',  ( 19.41271919554131031, -21.86055833610470955, -37.19327432862769456 ) ) ;
#14493 = CARTESIAN_POINT ( 'NONE',  ( 76.49475457737827355, -3.230541735902681122, -13.20481492880512242 ) ) ;
#14494 = ORIENTED_EDGE ( 'NONE', *, *, #10406, .T. ) ;
#14495 = CARTESIAN_POINT ( 'NONE',  ( 11.56725258447900018, -64.80210873993979703, -45.44585228502439378 ) ) ;
#14496 = CARTESIAN_POINT ( 'NONE',  ( 56.47614208328440100, -45.49446754575470209, -25.70510218961669935 ) ) ;
#14497 = LINE ( 'NONE', #10318, #10222 ) ;
#14498 = EDGE_CURVE ( 'NONE', #6837, #7993, #17598, .T. ) ;
#14499 = CARTESIAN_POINT ( 'NONE',  ( 11.87263725465938258, 24.15631867182189652, -22.13626404611502707 ) ) ;
#14500 = VERTEX_POINT ( 'NONE', #4839 ) ;
#14501 = CARTESIAN_POINT ( 'NONE',  ( 71.71126032029680175, 15.88381105532069704, -46.37203261889099792 ) ) ;
#14502 = LINE ( 'NONE', #26283, #44376 ) ;
#14503 = CARTESIAN_POINT ( 'NONE',  ( 11.89322115925799928, 34.20364973214489623, -22.25048088549079850 ) ) ;
#14504 = ORIENTED_EDGE ( 'NONE', *, *, #48086, .F. ) ;
#14505 = ADVANCED_FACE ( 'NONE', ( #48875 ), #28149, .T. ) ;
#14506 = CARTESIAN_POINT ( 'NONE',  ( 46.47787128639799903, -45.11618894461340545, -8.157179474024399468 ) ) ;
#14507 = CIRCLE ( 'NONE', #43788, 18.86180339887500068 ) ;
#14508 = DIRECTION ( 'NONE',  ( 3.191443934968489902E-12, -1.000000000000000000, -2.813979115193090113E-11 ) ) ;
#14509 = CARTESIAN_POINT ( 'NONE',  ( 14.13974949994110020, 19.81019562857040128, -21.96874462324929667 ) ) ;
#14510 = EDGE_CURVE ( 'NONE', #12905, #26981, #30100, .T. ) ;
#14511 = CARTESIAN_POINT ( 'NONE',  ( 13.13393739769600010, 18.38381105532060289, -35.14999999999999858 ) ) ;
#14512 = CARTESIAN_POINT ( 'NONE',  ( 17.43063470081056821, -22.26741796077540059, -46.89152911514357669 ) ) ;
#14513 = CARTESIAN_POINT ( 'NONE',  ( 73.20393974370439594, 0.8850831926798620186, -68.85873448833349642 ) ) ;
#14514 = CARTESIAN_POINT ( 'NONE',  ( 47.32873553055200233, -54.60302095746399687, -74.72285389774751252 ) ) ;
#14515 = CARTESIAN_POINT ( 'NONE',  ( 49.34439353803710304, 13.88381105527630055, -8.366262819176959908 ) ) ;
#14516 = TOROIDAL_SURFACE ( 'NONE', #21311, 5.500000000000000000, 0.5000000000000000000 ) ;
#14517 = DIRECTION ( 'NONE',  ( 0.000000000000000000, 0.000000000000000000, -1.000000000000000000 ) ) ;
#14518 = AXIS2_PLACEMENT_3D ( 'NONE', #1220, #48664, #12764 ) ;
#14519 = CARTESIAN_POINT ( 'NONE',  ( 52.61549993852860041, 20.12575500109499771, -75.86880970507380084 ) ) ;
#14520 = CARTESIAN_POINT ( 'NONE',  ( 11.88236613208781023, 34.20274921340377006, -17.91369326123606598 ) ) ;
#14521 = CARTESIAN_POINT ( 'NONE',  ( 13.50542271583660003, -23.43115095844289897, -36.11094655318100166 ) ) ;
#14522 = VERTEX_POINT ( 'NONE', #12979 ) ;
#14523 = CARTESIAN_POINT ( 'NONE',  ( 14.74159083669217729, -8.702150310962082358, -48.28392467753529615 ) ) ;
#14524 = CARTESIAN_POINT ( 'NONE',  ( 5.283814748811780149, -58.95969427206990332, -12.16686142996949904 ) ) ;
#14525 = CARTESIAN_POINT ( 'NONE',  ( 76.59602575693580206, 4.418458492249149216, -13.63971784130609777 ) ) ;
#14526 = CARTESIAN_POINT ( 'NONE',  ( 16.13393739769620083, -15.61618894467929941, 16.85000000000000142 ) ) ;
#14527 = CARTESIAN_POINT ( 'NONE',  ( 19.64923255343473585, -55.46140024220354547, -75.44170189639848445 ) ) ;
#14528 = DIRECTION ( 'NONE',  ( 0.4640893551880597712, -0.8857883891771956009, 0.000000000000000000 ) ) ;
#14529 = CARTESIAN_POINT ( 'NONE',  ( 8.231257142393115345, -9.874555653973354552, -18.08174999999999955 ) ) ;
#14530 = CARTESIAN_POINT ( 'NONE',  ( 57.36123081079020380, 18.90300135422739913, -52.61896059691729732 ) ) ;
#14531 = DIRECTION ( 'NONE',  ( -0.7071067811865475727, 0.000000000000000000, -0.7071067811865475727 ) ) ;
#14532 = CARTESIAN_POINT ( 'NONE',  ( 40.53658511620930227, 13.51357186806880151, -4.211756100499810529 ) ) ;
#14533 = CARTESIAN_POINT ( 'NONE',  ( 16.13393739769620083, -15.61618894467929941, -54.64999999999999858 ) ) ;
#14534 = DIRECTION ( 'NONE',  ( -0.8059588108975778153, 0.1342272854594989684, -0.5765530599821118152 ) ) ;
#14535 = CARTESIAN_POINT ( 'NONE',  ( 68.13393739769790614, -49.95860450174040324, -75.14853292321149070 ) ) ;
#14536 = AXIS2_PLACEMENT_3D ( 'NONE', #40710, #48841, #26262 ) ;
#14537 = ADVANCED_FACE ( 'NONE', ( #12189 ), #5849, .T. ) ;
#14538 = FACE_OUTER_BOUND ( 'NONE', #7787, .T. ) ;
#14539 = CARTESIAN_POINT ( 'NONE',  ( 17.89921485063580064, -51.35369855969700126, -75.11575902015950135 ) ) ;
#14540 = CARTESIAN_POINT ( 'NONE',  ( 53.33161320831360541, -44.97067256191790108, -8.409648214525970999 ) ) ;
#14541 = ORIENTED_EDGE ( 'NONE', *, *, #27373, .T. ) ;
#14542 = EDGE_CURVE ( 'NONE', #885, #5705, #12442, .T. ) ;
#14543 = CARTESIAN_POINT ( 'NONE',  ( 22.76337341064190056, -19.01578781639930327, -57.21816999718349450 ) ) ;
#14544 = CARTESIAN_POINT ( 'NONE',  ( 63.55130486076479457, 0.9860880133283479454, -61.77606584740419748 ) ) ;
#14545 = VERTEX_POINT ( 'NONE', #28667 ) ;
#14546 = DIRECTION ( 'NONE',  ( 1.000000000000000000, 0.000000000000000000, 0.000000000000000000 ) ) ;
#14547 = CARTESIAN_POINT ( 'NONE',  ( 9.366937397696199596, -15.61618894467949836, -28.45282021618999835 ) ) ;
#14548 = DIRECTION ( 'NONE',  ( -0.2260571801428130634, -5.828670879282072626E-15, 0.9741140340359951688 ) ) ;
#14549 = CARTESIAN_POINT ( 'NONE',  ( 7.571123728786868234, -60.97650226374818772, -20.43741446242723114 ) ) ;
#14550 = CARTESIAN_POINT ( 'NONE',  ( 9.140883284797808983, -16.59444103326700315, -81.23899999999999011 ) ) ;
#14551 = CARTESIAN_POINT ( 'NONE',  ( 10.80839229981719818, 21.91123435898759908, -23.15000000000000213 ) ) ;
#14552 = VERTEX_POINT ( 'NONE', #23697 ) ;
#14553 = VERTEX_POINT ( 'NONE', #51760 ) ;
#14554 = AXIS2_PLACEMENT_3D ( 'NONE', #4544, #20516, #36510 ) ;
#14555 = B_SPLINE_CURVE_WITH_KNOTS ( 'NONE', 3,
 ( #8635, #1289, #24587, #24850, #36396, #40346, #8126, #32443 ),
 .UNSPECIFIED., .F., .F.,
 ( 4, 2, 2, 4 ),
 ( 0.04513248637254871354, 0.05146834906984269764, 0.06948743965982991100, 0.08616863070281119419 ),
 .UNSPECIFIED. ) ;
#14556 = ORIENTED_EDGE ( 'NONE', *, *, #49523, .F. ) ;
#14557 = CARTESIAN_POINT ( 'NONE',  ( 56.44264214053480089, -45.11618894467940066, -15.14376385419100046 ) ) ;
#14558 = CARTESIAN_POINT ( 'NONE',  ( 61.49690240543349518, -45.15381908667030331, -46.58186461253090016 ) ) ;
#14559 = VECTOR ( 'NONE', #2421, 1000.000000000000000 ) ;
#14560 = ADVANCED_FACE ( 'NONE', ( #31819 ), #831, .T. ) ;
#14561 = DIRECTION ( 'NONE',  ( 1.000000000000000000, 0.000000000000000000, 0.000000000000000000 ) ) ;
#14562 = AXIS2_PLACEMENT_3D ( 'NONE', #26953, #31899, #23777 ) ;
#14563 = ORIENTED_EDGE ( 'NONE', *, *, #16258, .T. ) ;
#14564 = ORIENTED_EDGE ( 'NONE', *, *, #42900, .T. ) ;
#14565 = CARTESIAN_POINT ( 'NONE',  ( -18.86606260230360022, -50.61618894467959962, 14.21249999999999858 ) ) ;
#14566 = EDGE_CURVE ( 'NONE', #19834, #23063, #31776, .T. ) ;
#14567 = DIRECTION ( 'NONE',  ( 0.000000000000000000, 0.000000000000000000, -1.000000000000000000 ) ) ;
#14568 = EDGE_LOOP ( 'NONE', ( #27951, #15921, #51686, #25493 ) ) ;
#14569 = DIRECTION ( 'NONE',  ( 0.000000000000000000, -1.000000000000000000, 0.000000000000000000 ) ) ;
#14570 = CARTESIAN_POINT ( 'NONE',  ( 51.74354729887659943, -51.02687482177999811, -76.13548131957189469 ) ) ;
#14571 = CARTESIAN_POINT ( 'NONE',  ( 60.47761782512560558, 14.47093190675899876, -47.49433626963359956 ) ) ;
#14572 = DIRECTION ( 'NONE',  ( 1.000000000000000000, 0.000000000000000000, 0.000000000000000000 ) ) ;
#14573 = VECTOR ( 'NONE', #48998, 1000.000000000000000 ) ;
#14574 = CARTESIAN_POINT ( 'NONE',  ( 41.84726576968089518, -43.59559707646589999, -3.460729485120859650 ) ) ;
#14575 = CARTESIAN_POINT ( 'NONE',  ( 22.46012682185303078, -20.47783369061121661, -79.71600332221316876 ) ) ;
#14576 = CARTESIAN_POINT ( 'NONE',  ( 55.94825483526997800, 14.62989463075238916, -25.32139416924175634 ) ) ;
#14577 = CARTESIAN_POINT ( 'NONE',  ( 64.49518718159480102, 1.242005038313980014, -70.30973843397600831 ) ) ;
#14578 = CARTESIAN_POINT ( 'NONE',  ( 22.90097160515300345, -15.96958584066058151, -42.86379408845288452 ) ) ;
#14579 = CARTESIAN_POINT ( 'NONE',  ( 22.90091122653545241, -15.61618862529044804, -78.45282272177526295 ) ) ;
#14580 = CARTESIAN_POINT ( 'NONE',  ( 22.89829579906880141, -19.59490778382370024, -47.45674758581829877 ) ) ;
#14581 = ORIENTED_EDGE ( 'NONE', *, *, #37668, .F. ) ;
#14582 = CARTESIAN_POINT ( 'NONE',  ( 14.91264436884699940, -52.75136490455189886, -76.12493046668770091 ) ) ;
#14583 = VECTOR ( 'NONE', #11899, 1000.000000000000000 ) ;
#14584 = CARTESIAN_POINT ( 'NONE',  ( 57.42543158765980138, 19.07922509033599567, -52.86045852939989942 ) ) ;
#14585 = CARTESIAN_POINT ( 'NONE',  ( 71.52463645511689094, 1.229084191802120030, -70.46414972969260759 ) ) ;
#14586 = CARTESIAN_POINT ( 'NONE',  ( 45.77509190452501997, -40.08057006376965603, -58.05133673132166905 ) ) ;
#14587 = CARTESIAN_POINT ( 'NONE',  ( 52.68908936341578908, -49.75029824513269716, -38.31189016485959797 ) ) ;
#14588 = DIRECTION ( 'NONE',  ( 0.1686178020941689892, 0.6660492713794449182, -0.7265992051412129005 ) ) ;
#14589 = CARTESIAN_POINT ( 'NONE',  ( 63.19468704395299596, 0.8986939045430379913, -69.05651959838648679 ) ) ;
#14590 = CARTESIAN_POINT ( 'NONE',  ( 48.06703750773939987, -54.33034557285180455, -54.98976173603559658 ) ) ;
#14591 = CARTESIAN_POINT ( 'NONE',  ( 24.04493583903491682, -15.61104923254273835, -45.50746918787013584 ) ) ;
#14592 = EDGE_CURVE ( 'NONE', #44136, #45507, #19598, .T. ) ;
#14593 = CARTESIAN_POINT ( 'NONE',  ( 56.52383276625670305, 19.52002294768380253, -53.80484218896539517 ) ) ;
#14594 = CARTESIAN_POINT ( 'NONE',  ( 48.26548450438669846, 23.00817015210510164, -54.98365607671500044 ) ) ;
#14595 = ORIENTED_EDGE ( 'NONE', *, *, #21916, .F. ) ;
#14596 = ADVANCED_FACE ( 'NONE', ( #38759 ), #26942, .T. ) ;
#14597 = CARTESIAN_POINT ( 'NONE',  ( 14.62412072909330085, -22.50552946476250327, -71.41585254811130312 ) ) ;
#14598 = EDGE_CURVE ( 'NONE', #4677, #22335, #7297, .T. ) ;
#14599 = EDGE_LOOP ( 'NONE', ( #33193, #37705, #32824, #27670 ) ) ;
#14600 = CARTESIAN_POINT ( 'NONE',  ( 71.45588032111159293, 0.8910129994591549085, -70.64647704525299332 ) ) ;
#14601 = DIRECTION ( 'NONE',  ( -1.000000000000000000, 0.000000000000000000, 0.000000000000000000 ) ) ;
#14602 = DIRECTION ( 'NONE',  ( 0.000000000000000000, 0.000000000000000000, -1.000000000000000000 ) ) ;
#14604 = CARTESIAN_POINT ( 'NONE',  ( 16.13393739769620083, -15.61618894467929941, -7.101316701949489385 ) ) ;
#14603 = CARTESIAN_POINT ( 'NONE',  ( 83.47359158205310337, 13.98615420182590086, -47.48415154309289932 ) ) ;
#14605 = CARTESIAN_POINT ( 'NONE',  ( 9.831878794972480406, -12.44970571174390095, -71.60102766968249455 ) ) ;
#14607 = EDGE_CURVE ( 'NONE', #23688, #51520, #2854, .T. ) ;
#14606 = CARTESIAN_POINT ( 'NONE',  ( 52.82975622904280755, 18.42854261028849905, -28.15000000000000213 ) ) ;
#14608 = CARTESIAN_POINT ( 'NONE',  ( 0.4937122138108709923, -22.40531513632469895, -34.90839531524139971 ) ) ;
#14609 = DIRECTION ( 'NONE',  ( -2.619602780254359830E-11, 3.858400438143729530E-12, 1.000000000000000000 ) ) ;
#14610 = ORIENTED_EDGE ( 'NONE', *, *, #15848, .T. ) ;
#14611 = CARTESIAN_POINT ( 'NONE',  ( 51.13393739769659874, -50.61618894467899565, 14.21249999999999858 ) ) ;
#14612 = ORIENTED_EDGE ( 'NONE', *, *, #19023, .F. ) ;
#14613 = VERTEX_POINT ( 'NONE', #10975 ) ;
#14614 = CARTESIAN_POINT ( 'NONE',  ( 12.21104395315190061, -64.88750845341350271, -16.16308188032050097 ) ) ;
#14615 = CARTESIAN_POINT ( 'NONE',  ( 7.768034174689500304, -60.63850792724319660, -20.78409677699329805 ) ) ;
#14616 = CARTESIAN_POINT ( 'NONE',  ( 10.71149743639709939, -11.10623284283549950, -62.06801868260409094 ) ) ;
#14617 = CARTESIAN_POINT ( 'NONE',  ( 12.48503350875200013, -65.45837120426659794, -47.47731082152539983 ) ) ;
#14618 = EDGE_CURVE ( 'NONE', #13860, #48001, #51830, .T. ) ;
#14619 = ORIENTED_EDGE ( 'NONE', *, *, #17325, .T. ) ;
#14620 = ORIENTED_EDGE ( 'NONE', *, *, #29983, .T. ) ;
#14621 = CARTESIAN_POINT ( 'NONE',  ( 52.99344130519229878, 21.02275823560590240, -54.37359777462930310 ) ) ;
#14622 = CARTESIAN_POINT ( 'NONE',  ( 56.55522360613520760, 14.97957722649010037, -26.26695323647559732 ) ) ;
#14623 = CARTESIAN_POINT ( 'NONE',  ( 52.76699503163899152, 18.41354606731650279, -48.30730215388749826 ) ) ;
#14624 = B_SPLINE_CURVE_WITH_KNOTS ( 'NONE', 3,
 ( #26832, #31262, #22374, #42578, #6416, #27347, #19229, #50439, #38380, #38907, #6673, #23144 ),
 .UNSPECIFIED., .F., .F.,
 ( 4, 2, 2, 2, 2, 4 ),
 ( 0.000000000000000000, 0.2528991456833806772, 0.3793487185250741800, 0.4425735049459256776, 0.4741858981563524256, 0.5057982913667791181 ),
 .UNSPECIFIED. ) ;
#14625 = CARTESIAN_POINT ( 'NONE',  ( 75.13393739769618662, -33.11618894467940066, -84.38499399519520239 ) ) ;
#14626 = EDGE_CURVE ( 'NONE', #20497, #23063, #10905, .T. ) ;
#14627 = CARTESIAN_POINT ( 'NONE',  ( 51.25913874074879573, -49.93899559840220093, -76.33308073030519836 ) ) ;
#14628 = CARTESIAN_POINT ( 'NONE',  ( 56.39270163676989966, -50.52750478097990339, -52.86271286804240077 ) ) ;
#14629 = ORIENTED_EDGE ( 'NONE', *, *, #39039, .F. ) ;
#14630 = FACE_OUTER_BOUND ( 'NONE', #23680, .T. ) ;
#14631 = CARTESIAN_POINT ( 'NONE',  ( 22.47876248253967901, -18.58448477081164896, -50.98678728705716878 ) ) ;
#14632 = ORIENTED_EDGE ( 'NONE', *, *, #36645, .F. ) ;
#14633 = CARTESIAN_POINT ( 'NONE',  ( 52.82975622904280755, -49.66092049964720445, -28.15000000000000213 ) ) ;
#14634 = DIRECTION ( 'NONE',  ( 0.000000000000000000, 1.000000000000000000, 0.000000000000000000 ) ) ;
#14635 = CARTESIAN_POINT ( 'NONE',  ( 20.06159909528509999, -22.41032032263160190, -48.34564971805809819 ) ) ;
#14636 = CARTESIAN_POINT ( 'NONE',  ( 14.13996207071699907, -51.04257905764659853, -21.96868406873729995 ) ) ;
#14637 = CARTESIAN_POINT ( 'NONE',  ( 47.30391968620949683, -54.13632037683530029, -75.47331621149609759 ) ) ;
#14638 = CARTESIAN_POINT ( 'NONE',  ( 56.50061946469200080, 14.14892819972229887, -17.74286813043059752 ) ) ;
#14639 = CARTESIAN_POINT ( 'NONE',  ( 10.49497832658790131, 32.13626875971579722, -45.62743361653370044 ) ) ;
#14640 =( BOUNDED_CURVE ( )  B_SPLINE_CURVE ( 3, ( #8631, #24581, #36647, #752 ),
 .UNSPECIFIED., .F., .T. ) 
 B_SPLINE_CURVE_WITH_KNOTS ( ( 4, 4 ),
 ( 4.416522867113069850, 4.551367696244820849 ),
 .UNSPECIFIED. ) 
 CURVE ( )  GEOMETRIC_REPRESENTATION_ITEM ( )  RATIONAL_B_SPLINE_CURVE ( ( 1.000000000000000000, 0.9984853132547846233, 0.9984853132547846233, 1.000000000000000000 ) ) 
 REPRESENTATION_ITEM ( '' )  );
#14641 = DIRECTION ( 'NONE',  ( -0.000000000000000000, -1.000000000000000000, -0.000000000000000000 ) ) ;
#14642 = ADVANCED_FACE ( 'NONE', ( #3112 ), #43710, .T. ) ;
#14643 = CARTESIAN_POINT ( 'NONE',  ( 12.28756344725089988, -21.52786946782889999, -43.53078881371720144 ) ) ;
#14644 = ORIENTED_EDGE ( 'NONE', *, *, #17574, .F. ) ;
#14645 = AXIS2_PLACEMENT_3D ( 'NONE', #19659, #12576, #36402 ) ;
#14646 = CARTESIAN_POINT ( 'NONE',  ( 46.80224289649839875, 22.25487713458520034, -76.02816653588809004 ) ) ;
#14647 = CARTESIAN_POINT ( 'NONE',  ( 65.03752560835731344, 1.369664981662519931, -60.92138556078450051 ) ) ;
#14648 = CARTESIAN_POINT ( 'NONE',  ( 20.99565279412726682, -9.290053523812696668, -51.21599975162614982 ) ) ;
#14649 = CARTESIAN_POINT ( 'NONE',  ( 45.24652675828470194, -45.11233960980349877, -7.238436661000799965 ) ) ;
#14650 = LINE ( 'NONE', #22238, #11460 ) ;
#14651 = CARTESIAN_POINT ( 'NONE',  ( 46.35275103504449845, -52.90993241930539881, -76.14999999999999147 ) ) ;
#14652 = CONICAL_SURFACE ( 'NONE', #43949, 0.3230324999999999447, 0.7853981633974469467 ) ;
#14653 = CARTESIAN_POINT ( 'NONE',  ( 82.61194114885600470, 14.02128113440400092, -47.15273303709880537 ) ) ;
#14654 = CARTESIAN_POINT ( 'NONE',  ( -0.01911352800862239909, 19.70019394631319898, -34.82369549110249807 ) ) ;
#14656 = CARTESIAN_POINT ( 'NONE',  ( 46.44081879553109360, -38.06850544220679922, -58.10139953457039752 ) ) ;
#14655 = DIRECTION ( 'NONE',  ( 1.000000000000000000, 1.222653822078627158E-29, -4.718060457820110146E-11 ) ) ;
#14657 = CARTESIAN_POINT ( 'NONE',  ( 9.530058881327454046, -20.02245067740681961, -32.60498688510223531 ) ) ;
#14658 = CARTESIAN_POINT ( 'NONE',  ( -29.90021944857959824, 4.910539643151190958, -56.90940863684170381 ) ) ;
#14659 = ORIENTED_EDGE ( 'NONE', *, *, #10406, .F. ) ;
#14660 = EDGE_CURVE ( 'NONE', #11419, #17917, #50805, .T. ) ;
#14661 = CARTESIAN_POINT ( 'NONE',  ( 52.87767300843589879, -49.65031313576589866, -48.88837533472770502 ) ) ;
#14662 = VERTEX_POINT ( 'NONE', #43207 ) ;
#14663 = CARTESIAN_POINT ( 'NONE',  ( 42.66089338409341281, 8.656733235152263006, -72.90937615055806020 ) ) ;
#14664 = DIRECTION ( 'NONE',  ( 0.000000000000000000, 1.218758999999999977E-12, 1.000000000000000000 ) ) ;
#14665 = CARTESIAN_POINT ( 'NONE',  ( 13.58976835783069959, 19.98880259310410068, -22.27010927015149733 ) ) ;
#14666 = CARTESIAN_POINT ( 'NONE',  ( 51.84382200394469464, -49.26715888966499790, -77.06468274235049876 ) ) ;
#14667 = CARTESIAN_POINT ( 'NONE',  ( 18.71115058146540022, -9.051089486024348929, -40.07189310636189816 ) ) ;
#14668 = CARTESIAN_POINT ( 'NONE',  ( 12.72590404555789512, -21.52907670588500721, -77.11949976459347056 ) ) ;
#14670 = EDGE_CURVE ( 'NONE', #28389, #4191, #28415, .T. ) ;
#14669 = CARTESIAN_POINT ( 'NONE',  ( 53.54325352770920432, 18.17990710143569899, -49.20622422613530489 ) ) ;
#14671 = CARTESIAN_POINT ( 'NONE',  ( 22.52295300047549276, -13.38580680388945332, -80.74026669357201058 ) ) ;
#14672 = DIRECTION ( 'NONE',  ( 0.000000000000000000, 0.000000000000000000, -1.000000000000000000 ) ) ;
#14673 = ORIENTED_EDGE ( 'NONE', *, *, #25836, .T. ) ;
#14674 = CARTESIAN_POINT ( 'NONE',  ( 12.87814453327409936, -22.40556983950980197, -31.92983709734899378 ) ) ;
#14675 = CARTESIAN_POINT ( 'NONE',  ( 60.34379259250669492, 14.63564649040839960, -47.72732609510669732 ) ) ;
#14676 = CARTESIAN_POINT ( 'NONE',  ( 12.91799614346290070, 34.28036428892229992, -47.72740221857549869 ) ) ;
#14677 = CARTESIAN_POINT ( 'NONE',  ( 73.15108049798000422, 0.8888742037077609348, -62.35931220671560027 ) ) ;
#14678 = CARTESIAN_POINT ( 'NONE',  ( 11.46916641884869925, -65.36694628387890305, -17.97103954075589982 ) ) ;
#14679 = DIRECTION ( 'NONE',  ( -0.3863301728269282753, -0.9223605572461974766, 0.000000000000000000 ) ) ;
#14680 = CARTESIAN_POINT ( 'NONE',  ( 24.04487507994048201, -15.64862276394573115, -75.79363074543330470 ) ) ;
#14681 = AXIS2_PLACEMENT_3D ( 'NONE', #18061, #14391, #38243 ) ;
#14682 = CARTESIAN_POINT ( 'NONE',  ( 22.89016887680049450, -19.75659366885420098, -45.68273552378035163 ) ) ;
#14683 = EDGE_LOOP ( 'NONE', ( #51837, #14619, #40300, #22853 ) ) ;
#14684 = CARTESIAN_POINT ( 'NONE',  ( 64.74203006853210240, 1.187931651339009909, -70.49707891402360360 ) ) ;
#14685 = ORIENTED_EDGE ( 'NONE', *, *, #16367, .F. ) ;
#14686 = CIRCLE ( 'NONE', #43971, 2.999999999999999112 ) ;
#14687 = CARTESIAN_POINT ( 'NONE',  ( 10.14580672186800214, -63.28459696954880087, -45.99312667690720957 ) ) ;
#14688 = CARTESIAN_POINT ( 'NONE',  ( 23.83903686589412629, -13.54550955106036980, -47.70900000688411069 ) ) ;
#14689 = ORIENTED_EDGE ( 'NONE', *, *, #38684, .T. ) ;
#14690 = DIRECTION ( 'NONE',  ( 0.000000000000000000, 0.000000000000000000, 1.000000000000000000 ) ) ;
#14691 = CYLINDRICAL_SURFACE ( 'NONE', #42827, 1.999999999999999778 ) ;
#14692 = CARTESIAN_POINT ( 'NONE',  ( 53.05142854777299988, 19.34251570886219795, -76.69950310396559701 ) ) ;
#14693 = ORIENTED_EDGE ( 'NONE', *, *, #23312, .T. ) ;
#14694 = FACE_OUTER_BOUND ( 'NONE', #9155, .T. ) ;
#14695 = DIRECTION ( 'NONE',  ( 1.000000000000000000, 0.000000000000000000, 0.000000000000000000 ) ) ;
#14696 = CARTESIAN_POINT ( 'NONE',  ( 15.27024859253024403, -22.36980594194034566, -32.99316856505028994 ) ) ;
#14697 = DIRECTION ( 'NONE',  ( 0.000000000000000000, 0.000000000000000000, 1.000000000000000000 ) ) ;
#14698 = B_SPLINE_SURFACE_WITH_KNOTS ( 'NONE', 3, 3, ( 
 ( #37250, #33303, #45628, #45894, #40917, #49317, #25687, #8960, #5797, #5025, #1083, #13412, #17082, #29114, #21758, #33813 ),
 ( #37769, #13663, #33033, #33562, #1862, #25942, #45113, #44856, #41960, #6056, #21503, #49057, #13166, #22014, #38025, #18100 ),
 ( #12897, #37503, #29374, #1347, #25428, #34066, #9220, #24903, #49579, #1603, #28853, #29626, #2119, #20990, #45375, #25173 ),
 ( #5289, #17338, #9481, #17590, #34591, #30399, #30138, #18870, #38808, #50076, #34852, #31165, #50852, #50597, #14945, #7346 ),
 ( #7095, #18350, #34327, #14687, #30908, #46939, #2902, #11024, #43258, #47193, #26206, #2373, #10766, #46421, #22273, #35108 ),
 ( #3419, #27240, #14171, #10509, #46161, #10248, #42217, #11280, #30655, #26993, #23294, #26466, #42999, #46680, #51107, #6840 ),
 ( #42480, #50343, #23047, #39068, #6572, #15211, #3159, #22789, #19129, #39315, #19389, #6317, #26725, #38284, #14429, #42742 ),
 ( #22534, #38546, #2645, #18613, #23555, #496, #8372, #11800, #3933, #43758, #40339, #4433, #44526, #48462, #43505, #24062 ),
 ( #40589, #35639, #31675, #28007, #32185, #16229, #4690, #23808, #7859, #19893, #48202, #16482, #11541, #35886, #12305, #31419 ),
 ( #27502, #39569, #2, #3676, #51623, #28264, #20401, #24320, #44266, #36143, #19645, #4173, #36388, #32437, #15717, #15468 ),
 ( #12565, #44015, #47698, #27763, #28527, #8629, #35371, #24578, #51368, #8116, #15979, #39826, #47953, #47446, #7607, #31933 ) ),
 .UNSPECIFIED., .F., .F., .F.,
 ( 4, 1, 1, 1, 1, 1, 1, 1, 4 ),
 ( 4, 2, 2, 2, 2, 2, 2, 4 ),
 ( 0.000000000000000000, 0.1250000000000000000, 0.2500000000000000000, 0.3750000000000000000, 0.5000000000000000000, 0.6250000000000000000, 0.7500000000000000000, 0.8750000000000000000, 1.000000000000000000 ),
 ( -0.4072589812491170247, -0.3359886595305220380, -0.2545368632807000209, -0.2036294906245599834, -0.1781758042964910194, -0.1374499061715789838, -0.07228846917172100650, -3.520742999999999947E-15 ),
 .UNSPECIFIED. ) ;
#14699 = CARTESIAN_POINT ( 'NONE',  ( 22.81009815672139851, -10.77763569235409946, -61.59270509622250245 ) ) ;
#14700 = CARTESIAN_POINT ( 'NONE',  ( 68.13393739769618662, -30.49118894467929763, -65.65000000000000568 ) ) ;
#14701 = CARTESIAN_POINT ( 'NONE',  ( 45.36210379758509248, -38.08434548607991132, -63.50911186322624502 ) ) ;
#14702 = ORIENTED_EDGE ( 'NONE', *, *, #5966, .F. ) ;
#14703 = ORIENTED_EDGE ( 'NONE', *, *, #33262, .F. ) ;
#14704 = FACE_OUTER_BOUND ( 'NONE', #3921, .T. ) ;
#14705 = CARTESIAN_POINT ( 'NONE',  ( 8.874208692728860370, -17.29041501526199909, -53.16051062239899494 ) ) ;
#14706 = CARTESIAN_POINT ( 'NONE',  ( 52.56874714592159847, -49.85803425300269964, -48.49333755979899507 ) ) ;
#14707 = EDGE_CURVE ( 'NONE', #16787, #5288, #7536, .T. ) ;
#14708 = CARTESIAN_POINT ( 'NONE',  ( 9.872657506090700252, -12.41267197780759979, -32.14999999999999858 ) ) ;
#14709 = AXIS2_PLACEMENT_3D ( 'NONE', #37804, #18388, #42776 ) ;
#14710 = EDGE_CURVE ( 'NONE', #18163, #47819, #23248, .T. ) ;
#14711 = DIRECTION ( 'NONE',  ( 0.000000000000000000, 0.000000000000000000, 1.000000000000000000 ) ) ;
#14712 = DIRECTION ( 'NONE',  ( -0.5481517552764691992, -0.4595822764623992418, -0.6987945222659983635 ) ) ;
#14713 = EDGE_CURVE ( 'NONE', #12186, #43432, #47400, .T. ) ;
#14714 = CARTESIAN_POINT ( 'NONE',  ( 38.67452568954060155, 4.883811055320659733, -84.65000000000000568 ) ) ;
#14715 = CARTESIAN_POINT ( 'NONE',  ( 43.71655669661049615, -45.13538107674550304, -6.831381356293830365 ) ) ;
#14716 = CARTESIAN_POINT ( 'NONE',  ( 24.03960203508535187, -15.30246675214741181, -61.49505239560236447 ) ) ;
#14717 = AXIS2_PLACEMENT_3D ( 'NONE', #18902, #51657, #35405 ) ;
#14718 = CARTESIAN_POINT ( 'NONE',  ( 7.942461939831210849, -16.55557732664409798, -64.47132387395669184 ) ) ;
#14719 = VERTEX_POINT ( 'NONE', #19340 ) ;
#14720 = CARTESIAN_POINT ( 'NONE',  ( 52.58045726207989645, -49.84558690476340104, -28.15000000000000213 ) ) ;
#14721 = AXIS2_PLACEMENT_3D ( 'NONE', #22497, #6282, #10211 ) ;
#14722 = CARTESIAN_POINT ( 'NONE',  ( 56.40006832003150095, -50.78900847487010850, -74.42134219975289966 ) ) ;
#14724 = FACE_OUTER_BOUND ( 'NONE', #39961, .T. ) ;
#14723 = CARTESIAN_POINT ( 'NONE',  ( -9.486391603338390155, 12.57410522446340018, -6.341346566467760404 ) ) ;
#14725 = DIRECTION ( 'NONE',  ( -1.000000000000000000, 0.000000000000000000, 0.000000000000000000 ) ) ;
#14726 = FACE_OUTER_BOUND ( 'NONE', #9939, .T. ) ;
#14727 = VERTEX_POINT ( 'NONE', #31884 ) ;
#14728 = CARTESIAN_POINT ( 'NONE',  ( -8.393077763122880341, -44.64307718677159187, -5.215838194937219896 ) ) ;
#14729 = CARTESIAN_POINT ( 'NONE',  ( 47.78813954756139992, 23.17881026155490076, -54.71474246861410506 ) ) ;
#14730 = CARTESIAN_POINT ( 'NONE',  ( 41.40756764072759921, -44.77159127043780273, -5.393983506378570603 ) ) ;
#14731 = CARTESIAN_POINT ( 'NONE',  ( 63.51397770047800861, 1.389468113695440099, -62.45014271800210537 ) ) ;
#14732 = CARTESIAN_POINT ( 'NONE',  ( -21.36606260230379917, -62.82329572586585442, 11.14289321881345529 ) ) ;
#14733 = CARTESIAN_POINT ( 'NONE',  ( 12.10371154477419964, 33.94898634442529328, -16.68259577208300115 ) ) ;
#14734 = CARTESIAN_POINT ( 'NONE',  ( 7.635415421591214447, 29.62789471496180482, -20.56421356237308729 ) ) ;
#14736 = EDGE_CURVE ( 'NONE', #22390, #586, #45841, .T. ) ;
#14735 = CARTESIAN_POINT ( 'NONE',  ( 53.06503245504000432, 18.30587288450670158, -48.83676475384709903 ) ) ;
#14737 = CARTESIAN_POINT ( 'NONE',  ( 9.807815151057885927, -20.47792212130217493, -70.58399882812879866 ) ) ;
#14738 = CARTESIAN_POINT ( 'NONE',  ( 58.76944267056379800, -46.69458659170329895, -47.97775221472399920 ) ) ;
#14739 = CARTESIAN_POINT ( 'NONE',  ( 53.09178932327359490, 18.18835396469560095, -27.54443142566670133 ) ) ;
#14740 = CARTESIAN_POINT ( 'NONE',  ( 12.86517331568619937, 17.88381105532060289, -34.64999999999999858 ) ) ;
#14741 = CARTESIAN_POINT ( 'NONE',  ( 12.14978603429348958, -8.703677051011474930, -37.12566588475947071 ) ) ;
#14742 = FACE_OUTER_BOUND ( 'NONE', #5458, .T. ) ;
#14743 = CARTESIAN_POINT ( 'NONE',  ( 75.41048247916201319, -48.61618894467930119, -82.11365365517008286 ) ) ;
#14744 = CARTESIAN_POINT ( 'NONE',  ( 71.33861941035669929, 1.097085799869280009, -60.62778596399619602 ) ) ;
#14745 = CARTESIAN_POINT ( 'NONE',  ( 10.77042980482839951, 31.95257362349920172, -45.20517183706909492 ) ) ;
#14746 = CARTESIAN_POINT ( 'NONE',  ( 17.92370450342619748, 19.88381105532299742, -15.67980087199299888 ) ) ;
#14747 = DIRECTION ( 'NONE',  ( 0.000000000000000000, 0.000000000000000000, -1.000000000000000000 ) ) ;
#14748 = AXIS2_PLACEMENT_3D ( 'NONE', #30696, #46718, #18651 ) ;
#14749 = CARTESIAN_POINT ( 'NONE',  ( 17.92367119475710169, 19.88380572466640217, -74.33583724502659607 ) ) ;
#14750 = ORIENTED_EDGE ( 'NONE', *, *, #3185, .T. ) ;
#14751 = ORIENTED_EDGE ( 'NONE', *, *, #29964, .F. ) ;
#14752 = CARTESIAN_POINT ( 'NONE',  ( 9.405693712298736742, -17.02440160981913309, -37.78093115865203089 ) ) ;
#14753 = CARTESIAN_POINT ( 'NONE',  ( 76.55943877964870126, 0.2330598837798364131, -13.48354878354143516 ) ) ;
#14754 = ORIENTED_EDGE ( 'NONE', *, *, #38498, .F. ) ;
#14755 = CARTESIAN_POINT ( 'NONE',  ( 11.17710517087889954, -63.96272249765520712, -44.13856387930640324 ) ) ;
#14757 = B_SPLINE_CURVE_WITH_KNOTS ( 'NONE', 3,
 ( #28484, #32921, #32654, #25319, #41071, #44742, #21136, #48415, #16180, #9373 ),
 .UNSPECIFIED., .F., .F.,
 ( 4, 1, 1, 1, 1, 1, 1, 4 ),
 ( 0.000000000000000000, 0.1428596598124854400, 0.2857193196249708800, 0.4285789794374563200, 0.5714386392499406497, 0.7142982990624261452, 0.8571579588749115297, 1.000000000000000000 ),
 .UNSPECIFIED. ) ;
#14756 = CARTESIAN_POINT ( 'NONE',  ( 56.99474382507709436, -45.26449535605289753, -25.71127314621080018 ) ) ;
#14758 = CARTESIAN_POINT ( 'NONE',  ( 0.6320745533423631768, -8.781616017679803932, -34.77490583097452514 ) ) ;
#14759 = CARTESIAN_POINT ( 'NONE',  ( 63.54027722212589424, 1.395196698723390138, -68.83033655198650536 ) ) ;
#14760 = EDGE_LOOP ( 'NONE', ( #50611, #23484, #38874, #26071, #9729, #12014, #36376, #24453, #28209, #37954 ) ) ;
#14761 = DIRECTION ( 'NONE',  ( 0.000000000000000000, 1.000000000000000000, 0.000000000000000000 ) ) ;
#14762 = CARTESIAN_POINT ( 'NONE',  ( 43.01395769380430067, 6.547552581025015250, -75.24989832121792688 ) ) ;
#14763 = AXIS2_PLACEMENT_3D ( 'NONE', #30626, #50824, #10733 ) ;
#14764 = CARTESIAN_POINT ( 'NONE',  ( 11.36992640080890027, 32.26814655965639389, -24.38598900311270157 ) ) ;
#14765 = ORIENTED_EDGE ( 'NONE', *, *, #18160, .T. ) ;
#14766 = CARTESIAN_POINT ( 'NONE',  ( 21.14893523691819865, -22.16084452985059983, -36.08420929373698982 ) ) ;
#14767 = VECTOR ( 'NONE', #46074, 1000.000000000000000 ) ;
#14768 = DIRECTION ( 'NONE',  ( -1.000000000000000000, 0.000000000000000000, 0.000000000000000000 ) ) ;
#14769 = DIRECTION ( 'NONE',  ( 0.000000000000000000, 0.000000000000000000, 1.000000000000000000 ) ) ;
#14770 = CARTESIAN_POINT ( 'NONE',  ( 13.15886326406111451, -21.71786568543119955, -51.09713416873294278 ) ) ;
#14771 = FACE_OUTER_BOUND ( 'NONE', #32564, .T. ) ;
#14772 = CARTESIAN_POINT ( 'NONE',  ( 63.22343968446819673, 0.9036513197889520788, -62.20214363597949614 ) ) ;
#14773 = CARTESIAN_POINT ( 'NONE',  ( 47.37032927764639822, -54.67515752274410090, -74.17395249489511855 ) ) ;
#14774 = CARTESIAN_POINT ( 'NONE',  ( 52.15685074734039972, 13.73913658471580135, -8.117659720543509039 ) ) ;
#14775 = EDGE_CURVE ( 'NONE', #27489, #19246, #36803, .T. ) ;
#14776 = AXIS2_PLACEMENT_3D ( 'NONE', #4855, #28429, #4586 ) ;
#14777 = CARTESIAN_POINT ( 'NONE',  ( 49.81371308193354253, 22.09252804302983009, -54.04984813473200234 ) ) ;
#14778 = CARTESIAN_POINT ( 'NONE',  ( 65.17764417800763965, -31.69782882504341259, -17.21758621636998754 ) ) ;
#14779 = CARTESIAN_POINT ( 'NONE',  ( 18.55035336995420181, -8.149777981444650266, -80.88713649466590994 ) ) ;
#14780 = ORIENTED_EDGE ( 'NONE', *, *, #45307, .F. ) ;
#14781 = CARTESIAN_POINT ( 'NONE',  ( 53.68666193310649959, -48.91266994132399759, -27.15311340496670311 ) ) ;
#14782 = CARTESIAN_POINT ( 'NONE',  ( -3.663975856005799780, -49.36779947823060155, -6.368283874185619808 ) ) ;
#14783 = CARTESIAN_POINT ( 'NONE',  ( 75.49632929579119889, 4.576312485752930037, -12.47599735184120107 ) ) ;
#14784 = CARTESIAN_POINT ( 'NONE',  ( 75.25100069975053430, 13.51599575700000422, -14.19917115362995830 ) ) ;
#14785 = CARTESIAN_POINT ( 'NONE',  ( 38.67452568954060155, 2.762490711761019124, -83.77132034355965118 ) ) ;
#14786 = CYLINDRICAL_SURFACE ( 'NONE', #43159, 0.4999999999999986677 ) ;
#14787 = B_SPLINE_CURVE_WITH_KNOTS ( 'NONE', 3,
 ( #18773, #10146, #42640, #18253, #46578, #49981, #46317, #33714, #34745, #14073, #14331, #26624, #9883, #25839, #34221, #10409, #42377, #6474, #22948, #41851, #5956, #2022, #46058, #26105, #20051, #31835 ),
 .UNSPECIFIED., .F., .F.,
 ( 4, 2, 2, 2, 2, 2, 2, 2, 2, 2, 2, 2, 4 ),
 ( 0.000000000000000000, 0.02309096440924889374, 0.1572026337881723412, 0.2410224271499988302, 0.3014770649499997623, 0.3619317027499990846, 0.4374999999999998335, 0.5000000000000000000, 0.6250000000000004441, 0.7081425603971044369, 0.7912851207942084297, 0.8880021141917445737, 1.000000000000000000 ),
 .UNSPECIFIED. ) ;
#14788 = DIRECTION ( 'NONE',  ( 0.3535533905932738974, -0.6123724356957941373, 0.7071067811865477948 ) ) ;
#14789 = VECTOR ( 'NONE', #34434, 1000.000000000000000 ) ;
#14790 = CARTESIAN_POINT ( 'NONE',  ( 82.68209466367581228, -45.40217087331220114, -47.42729881771100509 ) ) ;
#14791 = DIRECTION ( 'NONE',  ( 0.000000000000000000, 0.000000000000000000, 1.000000000000000000 ) ) ;
#14792 = CARTESIAN_POINT ( 'NONE',  ( 41.59466759967410354, 12.80917673894839837, -4.344851877681960239 ) ) ;
#14794 = EDGE_CURVE ( 'NONE', #11039, #42293, #17552, .T. ) ;
#14793 = CARTESIAN_POINT ( 'NONE',  ( 68.38971107296249841, -30.11618894467929763, -18.15384911730639672 ) ) ;
#14795 = CARTESIAN_POINT ( 'NONE',  ( 37.13393739769620083, -49.11618894467930829, -35.14999999999999858 ) ) ;
#14796 = AXIS2_PLACEMENT_3D ( 'NONE', #29994, #49433, #10107 ) ;
#14797 = CARTESIAN_POINT ( 'NONE',  ( 68.13393739769649926, -48.11618894467630270, -70.54999999999999716 ) ) ;
#14798 = FACE_OUTER_BOUND ( 'NONE', #1334, .T. ) ;
#14799 = CARTESIAN_POINT ( 'NONE',  ( 18.20232122522270046, -51.72389970538209525, -75.45052476223459337 ) ) ;
#14800 = EDGE_CURVE ( 'NONE', #23175, #25078, #8344, .T. ) ;
#14801 = CARTESIAN_POINT ( 'NONE',  ( 53.51285457508119947, -44.36157961519030124, -7.701314136274850952 ) ) ;
#14802 = EDGE_LOOP ( 'NONE', ( #36198, #44059, #8423, #19190, #39287 ) ) ;
#14803 = CARTESIAN_POINT ( 'NONE',  ( 20.78426059192069886, -9.795433965503590912, -52.78190985762079634 ) ) ;
#14804 = CARTESIAN_POINT ( 'NONE',  ( 63.83389103303669998, 1.116860450401449878, -61.47226487784700311 ) ) ;
#14805 = ORIENTED_EDGE ( 'NONE', *, *, #29898, .T. ) ;
#14806 = CARTESIAN_POINT ( 'NONE',  ( -0.9227350764160839880, 21.52762428946969919, -9.384582815335910766 ) ) ;
#14807 = DIRECTION ( 'NONE',  ( 0.000000000000000000, 0.000000000000000000, -1.000000000000000000 ) ) ;
#14808 = CARTESIAN_POINT ( 'NONE',  ( 73.18852689059310990, 0.9219904752505979628, -68.88295677568349618 ) ) ;
#14809 = CARTESIAN_POINT ( 'NONE',  ( 45.56486364238802622, 8.835226115373638223, -59.07248904589445715 ) ) ;
#14810 = CARTESIAN_POINT ( 'NONE',  ( 19.13393739769592727, 18.38381105532069526, -35.01561944896768352 ) ) ;
#14811 = CARTESIAN_POINT ( 'NONE',  ( 45.12942576520030258, -45.58081347128780436, -8.542108704436810029 ) ) ;
#14812 = ORIENTED_EDGE ( 'NONE', *, *, #36920, .T. ) ;
#14813 = AXIS2_PLACEMENT_3D ( 'NONE', #3246, #51460, #31254 ) ;
#14814 = ORIENTED_EDGE ( 'NONE', *, *, #47918, .F. ) ;
#14815 = VECTOR ( 'NONE', #34545, 1000.000000000000000 ) ;
#14816 = ADVANCED_BREP_SHAPE_REPRESENTATION ( '', ( #10093, #20940 ), #50248 ) ;
#14817 = ORIENTED_EDGE ( 'NONE', *, *, #34412, .F. ) ;
#14818 = CARTESIAN_POINT ( 'NONE',  ( 57.05054250623780376, -45.11618894467940066, -16.05309365090189999 ) ) ;
#14819 = CARTESIAN_POINT ( 'NONE',  ( 61.07761260003830017, -45.33963634432910084, -46.86460514787039955 ) ) ;
#14820 = CARTESIAN_POINT ( 'NONE',  ( 82.64648846854103681, -45.32234436122444521, -47.29314152744393596 ) ) ;
#14821 = CIRCLE ( 'NONE', #39919, 18.50000000000000000 ) ;
#14822 = ORIENTED_EDGE ( 'NONE', *, *, #49923, .T. ) ;
#14823 = CARTESIAN_POINT ( 'NONE',  ( 20.63541822830437766, -51.88627667935604393, -69.46507341766410093 ) ) ;
#14824 = ORIENTED_EDGE ( 'NONE', *, *, #7623, .F. ) ;
#14825 = DIRECTION ( 'NONE',  ( 0.000000000000000000, 1.000000000000000000, 0.000000000000000000 ) ) ;
#14826 = CARTESIAN_POINT ( 'NONE',  ( 65.01767771978660448, 0.8838110553206759423, -60.52272727272730179 ) ) ;
#14827 = ORIENTED_EDGE ( 'NONE', *, *, #42970, .T. ) ;
#14828 = CARTESIAN_POINT ( 'NONE',  ( 29.13393739769619728, 4.555383930574470774, -84.65000000000000568 ) ) ;
#14829 = CARTESIAN_POINT ( 'NONE',  ( 50.96210775137730309, -50.95759000963079899, -76.15000017728290516 ) ) ;
#14830 = CARTESIAN_POINT ( 'NONE',  ( 60.28321421690059623, 14.52514086966039919, -47.30254520759619652 ) ) ;
#14831 = TOROIDAL_SURFACE ( 'NONE', #35738, 39.99999927950579348, 2.000000001564220309 ) ;
#14832 = FACE_OUTER_BOUND ( 'NONE', #13848, .T. ) ;
#14833 = EDGE_CURVE ( 'NONE', #3421, #34462, #16698, .T. ) ;
#14834 = CARTESIAN_POINT ( 'NONE',  ( 43.12694253603230266, -42.75409364460660555, -4.223455518406679765 ) ) ;
#14835 = FACE_OUTER_BOUND ( 'NONE', #50003, .T. ) ;
#14836 = CARTESIAN_POINT ( 'NONE',  ( -6.891925080208380017, 14.67362240842299848, -5.213017414248930059 ) ) ;
#14837 = CARTESIAN_POINT ( 'NONE',  ( 64.51140068127359939, 1.434916633744939940, -70.06045877469239258 ) ) ;
#14838 = CARTESIAN_POINT ( 'NONE',  ( 41.23393739769609567, -15.61618894467929586, 8.450000000000018829 ) ) ;
#14839 = DIRECTION ( 'NONE',  ( -1.000000000000000000, 0.000000000000000000, 0.000000000000000000 ) ) ;
#14840 = CARTESIAN_POINT ( 'NONE',  ( 18.85312695456509857, -22.97776189731640173, -49.67487765559980062 ) ) ;
#14841 = VERTEX_POINT ( 'NONE', #48949 ) ;
#14842 = CARTESIAN_POINT ( 'NONE',  ( 14.77612737573100077, -52.84830569448709525, -76.12661215459480957 ) ) ;
#14843 = B_SPLINE_CURVE_WITH_KNOTS ( 'NONE', 3,
 ( #9055, #37875, #41019, #1187, #21343, #21089, #9576, #28952, #25004, #1967, #37091, #1708, #9833, #25786, #17944, #5387 ),
 .UNSPECIFIED., .F., .F.,
 ( 4, 2, 2, 2, 2, 2, 2, 4 ),
 ( 0.000000000000000000, 0.1839239004051475279, 0.3399707309250580844, 0.4375000000000012768, 0.5000000000000000000, 0.6249999999999998890, 0.8250000000000015099, 1.000000000000000000 ),
 .UNSPECIFIED. ) ;
#14844 = CARTESIAN_POINT ( 'NONE',  ( 57.40343761314740334, 19.28400752131850027, -53.29433798474970274 ) ) ;
#14845 = CARTESIAN_POINT ( 'NONE',  ( 72.05113849075890187, 0.9952277120684979161, -70.19587804460300617 ) ) ;
#14846 = CARTESIAN_POINT ( 'NONE',  ( 45.42364261614932275, -40.05881144132143135, -59.75727053604451555 ) ) ;
#14847 = CARTESIAN_POINT ( 'NONE',  ( 15.91925957857180052, 19.75099634535679982, -20.31192411766160077 ) ) ;
#14848 = CARTESIAN_POINT ( 'NONE',  ( 21.25580764232959652, -11.01228238293339956, -32.14999999999999858 ) ) ;
#14849 = CARTESIAN_POINT ( 'NONE',  ( 20.63393739769620083, -41.61618894467930119, -35.14999999999999858 ) ) ;
#14850 = CARTESIAN_POINT ( 'NONE',  ( 61.04001029137710077, 14.12696047140060074, -46.86320535112459851 ) ) ;
#14851 = CARTESIAN_POINT ( 'NONE',  ( 47.88879426235710213, -54.35786135377490069, -54.72388424469730239 ) ) ;
#14852 = CARTESIAN_POINT ( 'NONE',  ( 22.95878781942407443, -14.77418192080419068, -80.80869067174239717 ) ) ;
#14853 = CARTESIAN_POINT ( 'NONE',  ( 56.47485682376580485, 19.50905819124500340, -53.50470829161239550 ) ) ;
#14854 = EDGE_CURVE ( 'NONE', #20584, #36469, #41827, .T. ) ;
#14855 = CARTESIAN_POINT ( 'NONE',  ( 9.807730840030560060, -10.75456395163743117, -71.00065483045410986 ) ) ;
#14856 = ORIENTED_EDGE ( 'NONE', *, *, #45978, .T. ) ;
#14857 = CARTESIAN_POINT ( 'NONE',  ( 18.09661853408499965, -22.39043738500939895, -71.25741468598400274 ) ) ;
#14858 = ORIENTED_EDGE ( 'NONE', *, *, #36462, .T. ) ;
#14859 = LINE ( 'NONE', #3074, #11689 ) ;
#14860 = CARTESIAN_POINT ( 'NONE',  ( 48.79180034249638709, -53.85388452497296896, -54.46585069627487741 ) ) ;
#14862 = DIRECTION ( 'NONE',  ( 1.000000000000000000, 0.000000000000000000, 0.000000000000000000 ) ) ;
#14861 = CARTESIAN_POINT ( 'NONE',  ( 83.74313374146190370, 13.73424720782510100, -47.44649717229000174 ) ) ;
#14863 = CARTESIAN_POINT ( 'NONE',  ( 11.78046264069759985, -10.06712384583619979, -81.74105084582579650 ) ) ;
#14864 = CARTESIAN_POINT ( 'NONE',  ( 8.773163716056640027, 17.21388800179359890, -41.74835365322499570 ) ) ;
#14865 = CARTESIAN_POINT ( 'NONE',  ( 71.34267188602959209, 0.8850831926798620186, -70.72000234600820079 ) ) ;
#14866 = CARTESIAN_POINT ( 'NONE',  ( 68.13393739769618662, -29.66618894467940137, -65.65000000000000568 ) ) ;
#14867 = ORIENTED_EDGE ( 'NONE', *, *, #11168, .F. ) ;
#14868 = DIRECTION ( 'NONE',  ( -1.000000000000000000, 0.000000000000000000, 0.000000000000000000 ) ) ;
#14869 = ORIENTED_EDGE ( 'NONE', *, *, #24321, .F. ) ;
#14870 = AXIS2_PLACEMENT_3D ( 'NONE', #18332, #2356, #34311 ) ;
#14871 = ORIENTED_EDGE ( 'NONE', *, *, #8269, .F. ) ;
#14872 = CARTESIAN_POINT ( 'NONE',  ( 12.36320305068320025, -64.54682834576858852, -15.76422791927960176 ) ) ;
#14873 = CARTESIAN_POINT ( 'NONE',  ( 23.04645209240441162, -11.63204155749060931, -39.62566383368776002 ) ) ;
#14874 = CARTESIAN_POINT ( 'NONE',  ( 76.47997422168397463, -27.07588652318575129, -13.14112417631144325 ) ) ;
#14875 = CARTESIAN_POINT ( 'NONE',  ( 12.80749145503170006, -65.50216741970210421, -47.64796710884480291 ) ) ;
#14876 = VERTEX_POINT ( 'NONE', #9101 ) ;
#14877 = ORIENTED_EDGE ( 'NONE', *, *, #42673, .T. ) ;
#14878 = CARTESIAN_POINT ( 'NONE',  ( 52.47879378027160158, 21.24197845805020179, -54.47385978244420102 ) ) ;
#14879 = FACE_OUTER_BOUND ( 'NONE', #41585, .T. ) ;
#14880 = CARTESIAN_POINT ( 'NONE',  ( 22.90093739769648806, -15.61618495405599560, -46.45282767544845370 ) ) ;
#14881 = CARTESIAN_POINT ( 'NONE',  ( 65.12608554791199822, 0.7709852564592141189, -17.50910145119379990 ) ) ;
#14882 = CARTESIAN_POINT ( 'NONE',  ( 51.50850403090069562, -48.69821067683690075, -76.79363216376179935 ) ) ;
#14883 = CARTESIAN_POINT ( 'NONE',  ( 61.09079324505120212, -45.54437747975160278, -47.59851791355200135 ) ) ;
#14884 = ORIENTED_EDGE ( 'NONE', *, *, #27178, .F. ) ;
#14885 = CARTESIAN_POINT ( 'NONE',  ( -18.86606260230360022, -50.61618894467959962, 16.85000000000000142 ) ) ;
#14886 = CARTESIAN_POINT ( 'NONE',  ( 40.76017233408010298, 14.12870932884110076, -5.740519046195230679 ) ) ;
#14887 = ORIENTED_EDGE ( 'NONE', *, *, #43137, .T. ) ;
#14888 = CARTESIAN_POINT ( 'NONE',  ( 9.366917463373315655, -14.83999494934982621, -33.48934057612472515 ) ) ;
#14889 = CARTESIAN_POINT ( 'NONE',  ( 48.77938445319979621, -45.11618894467940066, -9.436603585651489823 ) ) ;
#14890 = CARTESIAN_POINT ( 'NONE',  ( 22.82885795094379944, -19.71067137562029714, -48.18721185593089729 ) ) ;
#14891 = CARTESIAN_POINT ( 'NONE',  ( 13.71441810546650153, -51.14956980057220193, -22.21276096959649848 ) ) ;
#14892 = EDGE_CURVE ( 'NONE', #1527, #44651, #20942, .T. ) ;
#14893 = CARTESIAN_POINT ( 'NONE',  ( 18.25866816537099169, -8.891006542728039364, -64.44458661451926673 ) ) ;
#14894 = CARTESIAN_POINT ( 'NONE',  ( 56.48007840179790406, 14.15040822888880001, -17.55434835152090045 ) ) ;
#14895 = CARTESIAN_POINT ( 'NONE',  ( 60.94787312208169539, -45.42919348794200118, -47.18994051989060523 ) ) ;
#14896 = EDGE_CURVE ( 'NONE', #39662, #33083, #39371, .T. ) ;
#14897 = CARTESIAN_POINT ( 'NONE',  ( 56.84186849725410440, -50.37971971411840144, -52.83665658960050138 ) ) ;
#14898 = AXIS2_PLACEMENT_3D ( 'NONE', #28491, #51840, #11762 ) ;
#14899 = CARTESIAN_POINT ( 'NONE',  ( 22.44169310211590229, -12.46106974759469921, -46.69954605626199395 ) ) ;
#14900 = LINE ( 'NONE', #51581, #6858 ) ;
#14901 = EDGE_CURVE ( 'NONE', #1290, #4073, #8320, .T. ) ;
#14902 = ORIENTED_EDGE ( 'NONE', *, *, #25335, .T. ) ;
#14903 = CARTESIAN_POINT ( 'NONE',  ( 47.40092525023009529, 23.10040719678089971, -75.17431006860279297 ) ) ;
#14904 = CARTESIAN_POINT ( 'NONE',  ( 65.09597585808539577, 1.387131204727280132, -61.00757424182599920 ) ) ;
#14905 = B_SPLINE_CURVE_WITH_KNOTS ( 'NONE', 3,
 ( #3330, #31594, #51287, #43169, #23730, #7523, #7780, #47614, #19044, #39494 ),
 .UNSPECIFIED., .F., .F.,
 ( 4, 2, 2, 2, 4 ),
 ( 0.000000000000000000, 0.1775000000085890928, 0.3375000000163220770, 0.4375000000211544116, 0.4459052190640770963 ),
 .UNSPECIFIED. ) ;
#14906 = CARTESIAN_POINT ( 'NONE',  ( 18.20468874562406825, -7.911109138856854628, -51.09100011753265136 ) ) ;
#14907 = FACE_OUTER_BOUND ( 'NONE', #21852, .T. ) ;
#14908 = CARTESIAN_POINT ( 'NONE',  ( 23.04647201731028616, -11.63207886453984052, -47.34100298069407842 ) ) ;
#14909 = ADVANCED_FACE ( 'NONE', ( #29003 ), #28740, .T. ) ;
#14910 = DIRECTION ( 'NONE',  ( 0.000000000000000000, 0.000000000000000000, -1.000000000000000000 ) ) ;
#14911 = PLANE ( 'NONE',  #12461 ) ;
#14912 = CARTESIAN_POINT ( 'NONE',  ( -5.088235941628160397, 17.51416456853099746, -39.61904198186269355 ) ) ;
#14914 = CARTESIAN_POINT ( 'NONE',  ( 47.49152231325319207, -38.14496413414819642, -52.84339506842029266 ) ) ;
#14913 = CARTESIAN_POINT ( 'NONE',  ( 52.47677922141266293, 18.72919119518283182, -77.24546349350585217 ) ) ;
#14915 = DIRECTION ( 'NONE',  ( 1.000000000000000000, 0.000000000000000000, 0.000000000000000000 ) ) ;
#14916 = FACE_OUTER_BOUND ( 'NONE', #10749, .T. ) ;
#14917 = ADVANCED_FACE ( 'NONE', ( #25052 ), #47750, .T. ) ;
#14918 = CARTESIAN_POINT ( 'NONE',  ( 48.92624713453859897, 22.59774914665240075, -54.51889614858499300 ) ) ;
#14919 = ORIENTED_EDGE ( 'NONE', *, *, #48105, .T. ) ;
#14920 = CARTESIAN_POINT ( 'NONE',  ( 53.20331604642460377, -49.48552951222239926, -48.99213278053210274 ) ) ;
#14921 = EDGE_LOOP ( 'NONE', ( #18026, #22204, #20326, #22144 ) ) ;
#14922 = FACE_OUTER_BOUND ( 'NONE', #28639, .T. ) ;
#14923 = CARTESIAN_POINT ( 'NONE',  ( 10.40182605014470063, -11.50699697134410115, -40.04515584691789343 ) ) ;
#14924 = CARTESIAN_POINT ( 'NONE',  ( 14.03113113476580232, 19.93369484523139690, -22.86118034424179868 ) ) ;
#14925 = CARTESIAN_POINT ( 'NONE',  ( 51.13393739769659874, -56.11618894467899565, 16.85000000000000142 ) ) ;
#14926 = CARTESIAN_POINT ( 'NONE',  ( 16.17631379709270334, -8.563475783249899109, -51.95473276590480083 ) ) ;
#14927 = CARTESIAN_POINT ( 'NONE',  ( 52.90146998106999376, 18.41335516957889951, -48.94440823327429513 ) ) ;
#14928 = CARTESIAN_POINT ( 'NONE',  ( 55.59350741772299642, -45.78716744078080580, -16.53259405490819844 ) ) ;
#14929 = DIRECTION ( 'NONE',  ( 0.000000000000000000, 0.000000000000000000, -1.000000000000000000 ) ) ;
#14930 = ORIENTED_EDGE ( 'NONE', *, *, #2428, .T. ) ;
#14931 = CARTESIAN_POINT ( 'NONE',  ( 10.38431742451460060, -20.95740775194419925, -36.04922151265729724 ) ) ;
#14932 = ORIENTED_EDGE ( 'NONE', *, *, #16789, .T. ) ;
#14933 = CARTESIAN_POINT ( 'NONE',  ( 72.92278648876269642, 1.264689361399219836, -69.01667010504620237 ) ) ;
#14934 = CARTESIAN_POINT ( 'NONE',  ( 9.342451040078868729, 32.74871876812539995, -46.70581140351080052 ) ) ;
#14935 = CARTESIAN_POINT ( 'NONE',  ( 72.90248002265630589, 1.325715844996850024, -62.41274800841679848 ) ) ;
#14936 = CARTESIAN_POINT ( 'NONE',  ( 53.59019059237800064, -49.40616797538680061, -49.22498841376049938 ) ) ;
#14937 = CARTESIAN_POINT ( 'NONE',  ( 16.13393739769620083, -15.61618894467929941, -170.7999095292539948 ) ) ;
#14938 = CARTESIAN_POINT ( 'NONE',  ( 51.13393739769620083, 19.38381105532069881, 11.34999999999999964 ) ) ;
#14939 = AXIS2_PLACEMENT_3D ( 'NONE', #16963, #41060, #9093 ) ;
#14940 = EDGE_CURVE ( 'NONE', #2702, #29187, #25123, .T. ) ;
#14941 = CARTESIAN_POINT ( 'NONE',  ( 51.82317580592130213, -52.75362460619970051, -54.60923380648279846 ) ) ;
#14942 = ORIENTED_EDGE ( 'NONE', *, *, #49040, .T. ) ;
#14943 = CARTESIAN_POINT ( 'NONE',  ( 61.50409964636570237, 14.14168666559669951, -47.35437808293550432 ) ) ;
#14944 = VERTEX_POINT ( 'NONE', #48413 ) ;
#14945 = CARTESIAN_POINT ( 'NONE',  ( 9.727947716817020307, -63.12714292155349938, -46.30183543362019805 ) ) ;
#14946 = CARTESIAN_POINT ( 'NONE',  ( 12.13393739769649926, 24.18330853958550364, -23.15000000000000213 ) ) ;
#14947 = ORIENTED_EDGE ( 'NONE', *, *, #21686, .F. ) ;
#14948 = CARTESIAN_POINT ( 'NONE',  ( 66.85007717593936150, -33.11601710128963560, -20.46329705161230805 ) ) ;
#14949 = CARTESIAN_POINT ( 'NONE',  ( 56.95883372640280129, 19.02269652816849899, -52.69722348556799574 ) ) ;
#14950 = CARTESIAN_POINT ( 'NONE',  ( 53.18839696306619658, 19.26518443456370022, -76.93089028591350598 ) ) ;
#14951 =( BOUNDED_CURVE ( )  B_SPLINE_CURVE ( 3, ( #20298, #28162, #20817, #28680 ),
 .UNSPECIFIED., .F., .T. ) 
 B_SPLINE_CURVE_WITH_KNOTS ( ( 4, 4 ),
 ( 0.7853981633974057575, 1.570796326794889231 ),
 .UNSPECIFIED. ) 
 CURVE ( )  GEOMETRIC_REPRESENTATION_ITEM ( )  RATIONAL_B_SPLINE_CURVE ( ( 1.000000000000000000, 0.9492530216741866811, 0.9492530216741866811, 1.000000000000000000 ) ) 
 REPRESENTATION_ITEM ( '' )  );
#14952 = ORIENTED_EDGE ( 'NONE', *, *, #45444, .T. ) ;
#14953 = CARTESIAN_POINT ( 'NONE',  ( 9.013808796976707782, -63.78940032850923103, -46.72196777939856105 ) ) ;
#14954 = CARTESIAN_POINT ( 'NONE',  ( 53.09962126454065867, 20.18306339911599778, -75.69942531578703893 ) ) ;
#14955 = CARTESIAN_POINT ( 'NONE',  ( 9.985151944901502929, -18.54018250714871741, -33.31138893891623809 ) ) ;
#14956 = CARTESIAN_POINT ( 'NONE',  ( 24.04490452168148451, -15.61618923948461557, -69.79232899952297942 ) ) ;
#14957 = CARTESIAN_POINT ( 'NONE',  ( 10.59188935906489881, -9.511402003807539529, -59.05769930218669828 ) ) ;
#14958 = FACE_OUTER_BOUND ( 'NONE', #39064, .T. ) ;
#14959 = LINE ( 'NONE', #3949, #46819 ) ;
#14960 = VERTEX_POINT ( 'NONE', #8843 ) ;
#14961 = VERTEX_POINT ( 'NONE', #8587 ) ;
#14962 = DIRECTION ( 'NONE',  ( 0.000000000000000000, 0.000000000000000000, 1.000000000000000000 ) ) ;
#14963 = CARTESIAN_POINT ( 'NONE',  ( 16.76097247798089995, -23.04003705824129966, -58.70583579685249731 ) ) ;
#14964 = CARTESIAN_POINT ( 'NONE',  ( 52.58955037394610343, -49.83869439510250032, -48.57080679444320026 ) ) ;
#14965 = CARTESIAN_POINT ( 'NONE',  ( 52.74287992188719443, 13.88381105524769943, -12.54865867989730077 ) ) ;
#14966 = FACE_OUTER_BOUND ( 'NONE', #47107, .T. ) ;
#14967 = EDGE_CURVE ( 'NONE', #51304, #10101, #21950, .T. ) ;
#14968 = CARTESIAN_POINT ( 'NONE',  ( 16.13393739769620083, -15.61618894467929941, -32.14999999999999858 ) ) ;
#14969 = CARTESIAN_POINT ( 'NONE',  ( 16.13393739769609780, -15.61618894467929941, 8.449999999999999289 ) ) ;
#14970 = FACE_OUTER_BOUND ( 'NONE', #19652, .T. ) ;
#14971 = CARTESIAN_POINT ( 'NONE',  ( 11.79626796994640081, 33.68213603922090016, -16.32611600087430048 ) ) ;
#14972 = CIRCLE ( 'NONE', #13300, 2.000000000000002220 ) ;
#14974 = AXIS2_PLACEMENT_3D ( 'NONE', #34070, #1865, #49830 ) ;
#14973 = CARTESIAN_POINT ( 'NONE',  ( 14.04158334993860002, -7.640928745299749636, -58.92599869950329605 ) ) ;
#14975 = CARTESIAN_POINT ( 'NONE',  ( 20.92244642525459852, -21.76386151488839715, -32.14999999999999858 ) ) ;
#14976 = CARTESIAN_POINT ( 'NONE',  ( 54.19674966252080139, -50.83120162869429493, -76.02018738249189767 ) ) ;
#14978 = CARTESIAN_POINT ( 'NONE',  ( 75.13393739769618662, -15.61618894467929941, -84.38499399519520239 ) ) ;
#14977 = CARTESIAN_POINT ( 'NONE',  ( -5.639092938195660487, 16.55660679010130210, -6.778460780884890902 ) ) ;
#14979 = CIRCLE ( 'NONE', #37573, 16.00000000000000000 ) ;
#14980 = DIRECTION ( 'NONE',  ( -0.7226652920947608250, -0.6911981449639416075, 0.000000000000000000 ) ) ;
#14981 = DIRECTION ( 'NONE',  ( 1.224646799147353207E-16, 1.000000000000000000, -0.000000000000000000 ) ) ;
#14982 = ORIENTED_EDGE ( 'NONE', *, *, #51280, .F. ) ;
#14983 = CARTESIAN_POINT ( 'NONE',  ( -8.399016668626551052, -44.63805185196870440, -5.182633193463829890 ) ) ;
#14984 = CARTESIAN_POINT ( 'NONE',  ( 47.71230462437779352, 23.25609537601400234, -54.91947580701529574 ) ) ;
#14985 = CARTESIAN_POINT ( 'NONE',  ( 45.92996289863866366, -45.11618893962639021, -7.538592778498961700 ) ) ;
#14986 = CARTESIAN_POINT ( 'NONE',  ( 63.52141932237860544, 1.390806392144100068, -62.43047455269960011 ) ) ;
#14987 = CARTESIAN_POINT ( 'NONE',  ( 61.12445714337039959, 14.53949875652389956, -47.85281647892329460 ) ) ;
#14988 = CARTESIAN_POINT ( 'NONE',  ( 11.27698456966049889, 33.93186547003269737, -17.25002982802569917 ) ) ;
#14989 = CARTESIAN_POINT ( 'NONE',  ( 51.95458709081180615, 18.47553477844409997, -76.89034002170231474 ) ) ;
#14990 = CARTESIAN_POINT ( 'NONE',  ( 52.81826460758630049, 18.43456339274279898, -48.49937508744089598 ) ) ;
#14991 = CARTESIAN_POINT ( 'NONE',  ( 23.04646828283125615, -19.60030602656101451, -69.95900078780417175 ) ) ;
#14992 = CARTESIAN_POINT ( 'NONE',  ( -0.2553902877309514596, -45.40777142809078271, -34.98886107151971459 ) ) ;
#14993 = CARTESIAN_POINT ( 'NONE',  ( 54.53382703113199881, 16.91529470431860105, -26.77221820697280208 ) ) ;
#14994 = CARTESIAN_POINT ( 'NONE',  ( 50.50556472799611640, 4.843111011011147049, -76.20733270045852237 ) ) ;
#14995 = DIRECTION ( 'NONE',  ( 0.000000000000000000, -1.000000000000000000, 0.000000000000000000 ) ) ;
#14996 = CARTESIAN_POINT ( 'NONE',  ( 53.55182622754160349, 18.18654131614419711, -49.22385694762949981 ) ) ;
#14997 = CARTESIAN_POINT ( 'NONE',  ( 62.15049734348340138, -31.05978833337919554, -16.60284431732980082 ) ) ;
#14998 = CARTESIAN_POINT ( 'NONE',  ( 71.30079129029560647, 1.267233196669030004, -60.75373513970999539 ) ) ;
#14999 = CARTESIAN_POINT ( 'NONE',  ( 11.13393739769619906, 32.18560202157300409, -43.92096349992370108 ) ) ;
#15000 = CARTESIAN_POINT ( 'NONE',  ( 73.01385068780759013, 0.9098571636355720083, -62.15909090909049439 ) ) ;
#15001 = ADVANCED_FACE ( 'NONE', ( #28218 ), #44219, .T. ) ;
#15002 = CARTESIAN_POINT ( 'NONE',  ( 50.96349269431694040, -35.28592947176570505, -76.38117427622687217 ) ) ;
#15003 = CARTESIAN_POINT ( 'NONE',  ( 8.222623404330700936, -15.61601543569009820, -34.79233150823699816 ) ) ;
#15004 = ORIENTED_EDGE ( 'NONE', *, *, #9563, .F. ) ;
#15005 = ADVANCED_FACE ( 'NONE', ( #3543 ), #1696, .T. ) ;
#15006 = VERTEX_POINT ( 'NONE', #42018 ) ;
#15007 = DIRECTION ( 'NONE',  ( -0.6320511108061763750, -0.7748042566436798007, -0.01377523921801214815 ) ) ;
#15008 = CARTESIAN_POINT ( 'NONE',  ( 76.56354261845024212, 0.4299193838037037585, -13.50123283572469290 ) ) ;
#15009 = ORIENTED_EDGE ( 'NONE', *, *, #34409, .T. ) ;
#15010 = CARTESIAN_POINT ( 'NONE',  ( 11.51479647464729972, -64.70247410274960487, -44.93983864453959853 ) ) ;
#15011 = CARTESIAN_POINT ( 'NONE',  ( 57.41391223940169652, -45.19612066180349785, -25.73569688666339772 ) ) ;
#15012 = DIRECTION ( 'NONE',  ( 0.000000000000000000, -1.000000000000000000, 0.000000000000000000 ) ) ;
#15013 = EDGE_CURVE ( 'NONE', #18163, #1900, #46066, .T. ) ;
#15014 = CYLINDRICAL_SURFACE ( 'NONE', #47398, 7.910999999999997812 ) ;
#15015 = AXIS2_PLACEMENT_3D ( 'NONE', #11809, #11549, #46947 ) ;
#15016 = CARTESIAN_POINT ( 'NONE',  ( 47.90111851008803967, -55.06578241374122484, 11.34999999999999964 ) ) ;
#15017 = ORIENTED_EDGE ( 'NONE', *, *, #1763, .T. ) ;
#15018 = DIRECTION ( 'NONE',  ( 0.05355673475992404897, -0.9985648081931662867, 0.000000000000000000 ) ) ;
#15019 = AXIS2_PLACEMENT_3D ( 'NONE', #39464, #7998, #50991 ) ;
#15020 = CARTESIAN_POINT ( 'NONE',  ( 43.64772454978100313, 6.637557646638361675, -72.08106405648152304 ) ) ;
#15021 = CARTESIAN_POINT ( 'NONE',  ( 11.96620750885719886, 34.18065854861499986, -22.91770525601710062 ) ) ;
#15022 = EDGE_LOOP ( 'NONE', ( #5391, #25551 ) ) ;
#15023 = CARTESIAN_POINT ( 'NONE',  ( 17.41568895538090089, -23.76111577064400393, -36.24264715586419783 ) ) ;
#15024 = CARTESIAN_POINT ( 'NONE',  ( 51.51227227048835999, 0.9479476914507564134, -17.73309803839580212 ) ) ;
#15025 = AXIS2_PLACEMENT_3D ( 'NONE', #9585, #32877, #20835 ) ;
#15026 = CARTESIAN_POINT ( 'NONE',  ( 8.327182772215820705, -17.08089162929084637, -50.73335963105622426 ) ) ;
#15027 = CARTESIAN_POINT ( 'NONE',  ( 10.02873241999632370, -18.59298069272300680, -51.30846019940189962 ) ) ;
#15028 = CARTESIAN_POINT ( 'NONE',  ( 59.73136311602019788, -29.07177110127760145, -15.76233559764669856 ) ) ;
#15029 = CYLINDRICAL_SURFACE ( 'NONE', #30885, 0.9999999999999988898 ) ;
#15030 = CARTESIAN_POINT ( 'NONE',  ( 46.41634634279859739, -53.01112433162619908, -76.14999999999999147 ) ) ;
#15031 = CARTESIAN_POINT ( 'NONE',  ( 41.17242422168380500, 13.88381105527830073, -6.491247222890830670 ) ) ;
#15032 = EDGE_CURVE ( 'NONE', #36840, #12954, #3382, .T. ) ;
#15033 = CARTESIAN_POINT ( 'NONE',  ( 14.96048611060250089, 21.72103359751309881, -76.14999999999999147 ) ) ;
#15034 = CARTESIAN_POINT ( 'NONE',  ( 61.68315737383129971, 13.88381108669560149, -27.59559020379299810 ) ) ;
#15035 = CARTESIAN_POINT ( 'NONE',  ( 19.96701598536469646, -22.91620464669880164, -37.85376303658059527 ) ) ;
#15036 = ORIENTED_EDGE ( 'NONE', *, *, #12390, .T. ) ;
#15037 = CARTESIAN_POINT ( 'NONE',  ( 4.133937397696209715, -8.687985714403829718, -35.14999999999999858 ) ) ;
#15038 = CARTESIAN_POINT ( 'NONE',  ( 0.9985768606438358841, -53.36496704980149985, -7.599376136359519585 ) ) ;
#15039 = CARTESIAN_POINT ( 'NONE',  ( 76.34491340151899408, -12.50878940850270027, -12.55768725632909977 ) ) ;
#15040 = CARTESIAN_POINT ( 'NONE',  ( 75.40247264985536901, 12.93137384474434803, -13.67377317579595264 ) ) ;
#15041 = CARTESIAN_POINT ( 'NONE',  ( 61.06707969152498805, -45.46952364607431463, -47.42741923847710694 ) ) ;
#15042 = AXIS2_PLACEMENT_3D ( 'NONE', #17748, #28759, #49483 ) ;
#15043 = AXIS2_PLACEMENT_3D ( 'NONE', #22732, #23242, #19591 ) ;
#15044 = CARTESIAN_POINT ( 'NONE',  ( 14.14886614762370165, 1.362847559348080217, -35.02873218748179340 ) ) ;
#15045 = AXIS2_PLACEMENT_3D ( 'NONE', #45878, #28635, #21997 ) ;
#15046 = DIRECTION ( 'NONE',  ( 0.000000000000000000, -1.000000000000000000, 0.000000000000000000 ) ) ;
#15047 = CIRCLE ( 'NONE', #23367, 0.5000000000000004441 ) ;
#15048 = CARTESIAN_POINT ( 'NONE',  ( 82.75410128693920342, -45.59485774729899532, -47.67218414831240381 ) ) ;
#15049 = CARTESIAN_POINT ( 'NONE',  ( 57.30875059015219364, -50.56238778299910308, -53.44855692689219495 ) ) ;
#15050 = CARTESIAN_POINT ( 'NONE',  ( 42.13038056796350617, 12.10098310850369963, -3.383138905913079864 ) ) ;
#15051 = DIRECTION ( 'NONE',  ( 0.000000000000000000, 0.000000000000000000, -1.000000000000000000 ) ) ;
#15052 = DIRECTION ( 'NONE',  ( 0.000000000000000000, 0.000000000000000000, -1.000000000000000000 ) ) ;
#15053 = CARTESIAN_POINT ( 'NONE',  ( 56.51601257069349771, -47.72958752039729546, -47.92267345016610136 ) ) ;
#15054 = CARTESIAN_POINT ( 'NONE',  ( 56.52536539877749533, 19.51942783438209972, -53.84278118897309895 ) ) ;
#15055 = CIRCLE ( 'NONE', #4992, 0.4999999999856508115 ) ;
#15056 = CARTESIAN_POINT ( 'NONE',  ( 23.13393739769620083, -28.89524513604070322, -39.64999999999999858 ) ) ;
#15057 = CARTESIAN_POINT ( 'NONE',  ( 18.36965831139549721, -52.00201191962840142, -75.51495726157199329 ) ) ;
#15058 = CARTESIAN_POINT ( 'NONE',  ( 53.02870100497279537, -51.95943102007580450, -53.35088539576909739 ) ) ;
#15059 = CARTESIAN_POINT ( 'NONE',  ( 20.82481716059549726, -9.828068231670309629, -68.78413393247190299 ) ) ;
#15060 = CARTESIAN_POINT ( 'NONE',  ( 63.87013147868781004, 1.277124412296160028, -61.51639082798710234 ) ) ;
#15061 = VERTEX_POINT ( 'NONE', #10044 ) ;
#15062 = LINE ( 'NONE', #2756, #8360 ) ;
#15063 = LINE ( 'NONE', #27111, #32555 ) ;
#15064 = CARTESIAN_POINT ( 'NONE',  ( 73.24770736846269870, 0.9209567800143640959, -68.78847615610258970 ) ) ;
#15065 = CARTESIAN_POINT ( 'NONE',  ( 46.10619593582758569, 8.867239705439473596, -56.44334475430651565 ) ) ;
#15066 = CARTESIAN_POINT ( 'NONE',  ( 16.13393739769620083, -15.61618894467929941, -22.14999999999999858 ) ) ;
#15067 = CARTESIAN_POINT ( 'NONE',  ( 44.44811449676429760, -45.82485402717239964, -8.385894475659950942 ) ) ;
#15068 = ORIENTED_EDGE ( 'NONE', *, *, #43795, .T. ) ;
#15069 = CARTESIAN_POINT ( 'NONE',  ( 18.14078639169169804, 20.99064699730730155, -75.77237669558989808 ) ) ;
#15070 = ORIENTED_EDGE ( 'NONE', *, *, #38516, .F. ) ;
#15071 = EDGE_CURVE ( 'NONE', #41372, #10507, #19468, .T. ) ;
#15072 = ORIENTED_EDGE ( 'NONE', *, *, #46395, .F. ) ;
#15073 = ORIENTED_EDGE ( 'NONE', *, *, #33575, .T. ) ;
#15074 = CARTESIAN_POINT ( 'NONE',  ( -0.01453923778984735939, -32.60559584230732355, 4.943674098299959851 ) ) ;
#15075 = CARTESIAN_POINT ( 'NONE',  ( 22.60922503113999937, -11.32550468333229965, -81.23899999999999011 ) ) ;
#15076 = EDGE_CURVE ( 'NONE', #19, #20901, #24446, .T. ) ;
#15077 = CYLINDRICAL_SURFACE ( 'NONE', #34337, 20.79999999999999716 ) ;
#15078 = VERTEX_POINT ( 'NONE', #18161 ) ;
#15079 = CARTESIAN_POINT ( 'NONE',  ( 16.58604368022989561, -8.818121607810667228, -79.97378616020819209 ) ) ;
#15080 = ORIENTED_EDGE ( 'NONE', *, *, #31664, .F. ) ;
#15081 = PLANE ( 'NONE',  #150 ) ;
#15082 = CARTESIAN_POINT ( 'NONE',  ( 17.92370450347650035, -51.11618894467930119, -15.67980085856620143 ) ) ;
#15083 = CIRCLE ( 'NONE', #44366, 19.50000000000000000 ) ;
#15084 = CIRCLE ( 'NONE', #22622, 34.55616290057869833 ) ;
#15085 = ORIENTED_EDGE ( 'NONE', *, *, #19555, .F. ) ;
#15086 = CARTESIAN_POINT ( 'NONE',  ( 8.847469766316544693, -18.75936127001048348, -50.37806134412886649 ) ) ;
#15087 = CARTESIAN_POINT ( 'NONE',  ( 51.26685530262009394, -51.02395401094319993, -76.14349094382490080 ) ) ;
#15088 = AXIS2_PLACEMENT_3D ( 'NONE', #19448, #8175, #23105 ) ;
#15089 = CARTESIAN_POINT ( 'NONE',  ( 60.34240538927109299, 14.50246306764029924, -47.36430858416980527 ) ) ;
#15090 = AXIS2_PLACEMENT_3D ( 'NONE', #47815, #11923, #23925 ) ;
#15091 = EDGE_CURVE ( 'NONE', #27518, #51178, #38219, .T. ) ;
#15092 = DIRECTION ( 'NONE',  ( 0.6522074047277899300, 0.2731766849828906607, 0.7071067811865471286 ) ) ;
#15093 = EDGE_CURVE ( 'NONE', #13277, #26382, #1923, .T. ) ;
#15094 = CARTESIAN_POINT ( 'NONE',  ( 41.08683558286960391, -44.27600910371930354, -3.799114098081400215 ) ) ;
#15095 = CARTESIAN_POINT ( 'NONE',  ( 65.46029542295769943, -1.463538230407920082, -16.55376543218019947 ) ) ;
#15096 = CARTESIAN_POINT ( 'NONE',  ( -11.32734370190460105, 10.64934056395049922, -6.430192534648650593 ) ) ;
#15097 =( BOUNDED_CURVE ( )  B_SPLINE_CURVE ( 2, ( #12978, #28148, #44152 ),
 .UNSPECIFIED., .F., .T. ) 
 B_SPLINE_CURVE_WITH_KNOTS ( ( 3, 3 ),
 ( 1.104980434577240045, 2.168627590050199672 ),
 .UNSPECIFIED. ) 
 CURVE ( )  GEOMETRIC_REPRESENTATION_ITEM ( )  RATIONAL_B_SPLINE_CURVE ( ( 1.323085463760209857, 1.425426480542939967, 1.425426480542939967 ) ) 
 REPRESENTATION_ITEM ( '' )  );
#15098 = CARTESIAN_POINT ( 'NONE',  ( 64.47339077398659413, 0.9757097601092069583, -70.40482852006680048 ) ) ;
#15099 = CARTESIAN_POINT ( 'NONE',  ( 16.13393739769620083, -15.61618894467929941, -17.89999999999999858 ) ) ;
#15100 = CARTESIAN_POINT ( 'NONE',  ( 23.97941690387960278, -15.42857364349520033, -57.27989503770719892 ) ) ;
#15101 = ORIENTED_EDGE ( 'NONE', *, *, #46325, .F. ) ;
#15102 = DIRECTION ( 'NONE',  ( 1.000000000000000000, 2.460964292799963328E-14, 0.000000000000000000 ) ) ;
#15103 = CARTESIAN_POINT ( 'NONE',  ( 57.37957920624790376, 19.37952914044570107, -53.76443781220810791 ) ) ;
#15104 = B_SPLINE_CURVE_WITH_KNOTS ( 'NONE', 3,
 ( #14469, #10808, #18143, #34108, #30441, #50635, #27035, #50119 ),
 .UNSPECIFIED., .F., .F.,
 ( 4, 2, 2, 4 ),
 ( 0.5000013127411032654, 0.6249999999792921201, 0.8249999999903363523, 1.000000000000000000 ),
 .UNSPECIFIED. ) ;
#15105 = CARTESIAN_POINT ( 'NONE',  ( 71.92023852231459102, 1.432916438945839976, -69.99522902979279593 ) ) ;
#15106 = CIRCLE ( 'NONE', #26921, 22.00000000000000000 ) ;
#15107 = CARTESIAN_POINT ( 'NONE',  ( 45.44843781540670591, -40.06038511326323004, -59.63698597941407797 ) ) ;
#15108 = CARTESIAN_POINT ( 'NONE',  ( 15.67956920600530069, 19.63025757447420006, -20.20255632743559815 ) ) ;
#15109 = DIRECTION ( 'NONE',  ( 0.000000000000000000, 0.000000000000000000, -1.000000000000000000 ) ) ;
#15110 = CARTESIAN_POINT ( 'NONE',  ( 12.16981616251349863, 18.81688478108560147, -21.14999999999999858 ) ) ;
#15111 = CARTESIAN_POINT ( 'NONE',  ( 63.40307724931621181, 1.326666718054969829, -68.96486503246650557 ) ) ;
#15112 = CARTESIAN_POINT ( 'NONE',  ( 47.87513792687950342, -54.38076868848589385, -54.78262502738859752 ) ) ;
#15113 = DIRECTION ( 'NONE',  ( -0.7288689868556628149, -0.6846531968814575375, 0.000000000000000000 ) ) ;
#15114 = CARTESIAN_POINT ( 'NONE',  ( 56.36079227718369822, 19.32759065149559774, -52.89779386132410366 ) ) ;
#15115 = CARTESIAN_POINT ( 'NONE',  ( 17.16944539447341711, -7.705183308742559412, -71.33398442287155206 ) ) ;
#15116 = CIRCLE ( 'NONE', #7566, 2.000000000000001776 ) ;
#15117 = ORIENTED_EDGE ( 'NONE', *, *, #45984, .F. ) ;
#15118 = VECTOR ( 'NONE', #2684, 1000.000000000000114 ) ;
#15119 = CARTESIAN_POINT ( 'NONE',  ( 8.909593156947090975, -13.79532524041309927, -36.14593433426069424 ) ) ;
#15120 = ORIENTED_EDGE ( 'NONE', *, *, #30844, .F. ) ;
#15121 = CARTESIAN_POINT ( 'NONE',  ( 71.44620697304119972, 0.9254905997697669973, -70.65289529397499280 ) ) ;
#15122 = AXIS2_PLACEMENT_3D ( 'NONE', #29110, #29370, #24641 ) ;
#15123 = CARTESIAN_POINT ( 'NONE',  ( 12.14989623194125201, -22.52876317393949890, -58.17433482716594995 ) ) ;
#15124 = DIRECTION ( 'NONE',  ( 0.000000000000000000, 0.000000000000000000, 1.000000000000000000 ) ) ;
#15125 = CARTESIAN_POINT ( 'NONE',  ( 14.34417029198879945, -51.11618894467930119, -74.14999999999999147 ) ) ;
#15127 = CARTESIAN_POINT ( 'NONE',  ( 16.13393739769620083, -1.759782484128330049, -47.64999999999999858 ) ) ;
#15126 = CARTESIAN_POINT ( 'NONE',  ( 69.63393739769620083, -43.11618894467930119, -73.25000000000000000 ) ) ;
#15128 = AXIS2_PLACEMENT_3D ( 'NONE', #18279, #33993, #45301 ) ;
#15129 = DIRECTION ( 'NONE',  ( -0.2169304578186569410, 0.000000000000000000, 0.9761870601839526262 ) ) ;
#15130 = CARTESIAN_POINT ( 'NONE',  ( 20.11810741955662607, -22.52868898135160336, -41.84100097860003586 ) ) ;
#15131 = PLANE ( 'NONE',  #46232 ) ;
#15132 = B_SPLINE_SURFACE_WITH_KNOTS ( 'NONE', 3, 3, ( 
 ( #35982, #24680, #20498, #28625, #51720, #24159, #11902, #36489, #16329, #39929, #12670, #24420, #36234, #44369, #32801, #4526 ),
 ( #16579, #48303, #40432, #40181, #23904, #32533, #4027, #12400, #40693, #23654, #43608, #4274, #44624, #594, #11638, #8730 ),
 ( #20761, #4793, #19743, #343, #43858, #16853, #7955, #19987, #48564, #16072, #100, #15813, #36748, #858, #27602, #7711 ),
 ( #39669, #20244, #8474, #3777, #35736, #24939, #37022, #5584, #13956, #12931, #13703, #28887, #21800, #44889, #49352, #33337 ),
 ( #1901, #8994, #13198, #40951, #49865, #41730, #21023, #5064, #9517, #29147, #45667, #2159, #29913, #48827, #21538, #17369 ),
 ( #45932, #1120, #37535, #13452, #37284, #25463, #18139, #45148, #17117, #17630, #33069, #49096, #29661, #6097, #33599, #29410 ),
 ( #22052, #9259, #5835, #25207, #41213, #45411, #41469, #10021, #5325, #21278, #1382, #1641, #49613, #9769, #25721, #25984 ),
 ( #41998, #37806, #38064, #17879, #33849, #14466, #30182, #34103, #46201, #15249, #14728, #34890, #2936, #39104, #6609, #47231 ),
 ( #51153, #22312, #30699, #34368, #7133, #38848, #10548, #35148, #46979, #6877, #14983, #3458, #27030, #19169, #3196, #18907 ) ),
 .UNSPECIFIED., .F., .F., .F.,
 ( 4, 1, 1, 1, 1, 1, 4 ),
 ( 4, 2, 2, 2, 2, 2, 2, 4 ),
 ( 0.000000000000000000, 0.1666666666666670182, 0.3333333333333329818, 0.5000000000000000000, 0.6666666666666670737, 0.8333333333333330373, 1.000000005975759887 ),
 ( -11.87104306964520006, -9.393165086804188491, -7.415090133440680020, -5.929772490031120391, -5.187113668326339244, -3.998859553598700156, -2.097652970034459941, 0.01149808360710800025 ),
 .UNSPECIFIED. ) ;
#15133 = VERTEX_POINT ( 'NONE', #2957 ) ;
#15134 = ORIENTED_EDGE ( 'NONE', *, *, #36029, .T. ) ;
#15135 = EDGE_CURVE ( 'NONE', #17657, #46911, #48563, .T. ) ;
#15136 = EDGE_LOOP ( 'NONE', ( #6393, #20490, #1534, #1838, #2845 ) ) ;
#15137 = DIRECTION ( 'NONE',  ( 1.000000000000000000, 0.000000000000000000, 0.000000000000000000 ) ) ;
#15138 = DIRECTION ( 'NONE',  ( 0.000000000000000000, -1.000000000000000000, 0.000000000000000000 ) ) ;
#15139 = CARTESIAN_POINT ( 'NONE',  ( 16.13393739769620083, -15.61618894467929941, -35.12503119152809461 ) ) ;
#15140 = CARTESIAN_POINT ( 'NONE',  ( 11.91942152901519947, -65.30442633750028847, -47.17797789126349528 ) ) ;
#15141 = ORIENTED_EDGE ( 'NONE', *, *, #17798, .T. ) ;
#15142 = VERTEX_POINT ( 'NONE', #27819 ) ;
#15143 = CARTESIAN_POINT ( 'NONE',  ( 16.13393739769620083, -15.61618894467929941, 5.729250452415290518 ) ) ;
#15144 = FACE_OUTER_BOUND ( 'NONE', #26452, .T. ) ;
#15145 = CARTESIAN_POINT ( 'NONE',  ( 22.88146960594603385, -14.93411597101013299, -50.42079114153778363 ) ) ;
#15146 = CARTESIAN_POINT ( 'NONE',  ( 9.543100655325421400, -13.84480880723966756, -35.53615332108730485 ) ) ;
#15147 = CARTESIAN_POINT ( 'NONE',  ( 62.35336129981750020, -0.9719900955148390587, -16.24009828415930201 ) ) ;
#15148 = CARTESIAN_POINT ( 'NONE',  ( 51.68242196786739839, -49.02157941676630060, -76.95384497480380048 ) ) ;
#15149 = CARTESIAN_POINT ( 'NONE',  ( 46.98749101202549383, -39.23094825485602399, -34.79644638567071269 ) ) ;
#15150 = ORIENTED_EDGE ( 'NONE', *, *, #19116, .T. ) ;
#15151 = CARTESIAN_POINT ( 'NONE',  ( 16.13393739767329649, -15.61618894439989980, -19.08999999984770213 ) ) ;
#15152 = CARTESIAN_POINT ( 'NONE',  ( 61.13393739769620083, 1.883811055320649963, -84.38499399519520239 ) ) ;
#15153 = CARTESIAN_POINT ( 'NONE',  ( 10.72266837725936384, -11.45745312862252518, -51.66115301124705184 ) ) ;
#15154 = CARTESIAN_POINT ( 'NONE',  ( 57.08228080684060046, -47.57523781541689800, -48.30570546696120005 ) ) ;
#15155 = CARTESIAN_POINT ( 'NONE',  ( 8.397759403314990934, -16.93463410123079882, -42.95876240573199567 ) ) ;
#15156 = CARTESIAN_POINT ( 'NONE',  ( 13.75402769379000034, -50.28666754275069906, -20.97890654100260122 ) ) ;
#15157 = CARTESIAN_POINT ( 'NONE',  ( 55.44813972691670045, 19.38381105532069881, -76.34352098789580054 ) ) ;
#15158 = EDGE_CURVE ( 'NONE', #10936, #30581, #24286, .T. ) ;
#15159 = DIRECTION ( 'NONE',  ( 0.6933752452815363787, 0.7071067811865472397, -0.1386750490563077587 ) ) ;
#15160 = CARTESIAN_POINT ( 'NONE',  ( 56.55949779134230226, 13.95391148746589849, -16.30411193604290077 ) ) ;
#15161 = CARTESIAN_POINT ( 'NONE',  ( 8.744443678271633047, 17.71880458988568208, -34.77532226276706240 ) ) ;
#15162 = B_SPLINE_CURVE_WITH_KNOTS ( 'NONE', 3,
 ( #10009, #2145, #50367, #41713, #13689, #42507, #17359, #21528, #49849, #5822 ),
 .UNSPECIFIED., .F., .F.,
 ( 4, 2, 2, 2, 4 ),
 ( 0.000000000000000000, 0.1774999999982775079, 0.3374999999967193687, 0.4374999999957477348, 0.4999999271596042849 ),
 .UNSPECIFIED. ) ;
#15163 = CARTESIAN_POINT ( 'NONE',  ( 71.25658036288379549, 1.391252479931859964, -70.26382307879899258 ) ) ;
#15164 = AXIS2_PLACEMENT_3D ( 'NONE', #18484, #22401, #34459 ) ;
#15165 = CARTESIAN_POINT ( 'NONE',  ( 12.30558705848279999, -9.692820574005770240, -44.16454026222620399 ) ) ;
#15166 = CARTESIAN_POINT ( 'NONE',  ( -0.007164427059776000244, -22.82436266295209748, -34.77269723891829756 ) ) ;
#15167 = CIRCLE ( 'NONE', #19347, 33.97624844042360337 ) ;
#15168 = ORIENTED_EDGE ( 'NONE', *, *, #9913, .F. ) ;
#15169 = CARTESIAN_POINT ( 'NONE',  ( 14.13832835820899980, -51.13035289118570148, -74.36013246831049628 ) ) ;
#15170 = CARTESIAN_POINT ( 'NONE',  ( 64.90928650851489579, 1.188042061556800144, -60.70318061837799917 ) ) ;
#15171 = CARTESIAN_POINT ( 'NONE',  ( 44.98351815555930244, -46.11094773564500571, -8.963066483085869507 ) ) ;
#15172 = CARTESIAN_POINT ( 'NONE',  ( 54.86079194568145567, -47.84550249862039095, -26.65937158387647798 ) ) ;
#15173 = CARTESIAN_POINT ( 'NONE',  ( 24.04493737487536009, -14.58064688416050281, -47.46600315403375703 ) ) ;
#15174 = DIRECTION ( 'NONE',  ( 0.3294064756441309472, 0.9441882088883087887, -3.053113317719179500E-16 ) ) ;
#15175 = CARTESIAN_POINT ( 'NONE',  ( 82.46546147468319532, 13.86078240809950124, -46.44239936464539653 ) ) ;
#15176 = CARTESIAN_POINT ( 'NONE',  ( 10.61751707702059910, 33.59325229219749787, -22.25048313876769868 ) ) ;
#15178 = CARTESIAN_POINT ( 'NONE',  ( 8.223295469878840080, -15.61636541503349918, -58.79233150823709764 ) ) ;
#15177 = CARTESIAN_POINT ( 'NONE',  ( 47.48065465286614284, 23.09789386337090633, -75.12259495334244264 ) ) ;
#15179 = CARTESIAN_POINT ( 'NONE',  ( 68.13393739769618662, -29.66618894467940137, -65.65000000000000568 ) ) ;
#15180 = CARTESIAN_POINT ( 'NONE',  ( 49.54598800151349991, 22.37956328914630078, -54.50101998263440350 ) ) ;
#15181 = ORIENTED_EDGE ( 'NONE', *, *, #13792, .T. ) ;
#15182 = CARTESIAN_POINT ( 'NONE',  ( 52.67442042553170012, -49.76228255682879364, -48.55745968341410190 ) ) ;
#15183 = ORIENTED_EDGE ( 'NONE', *, *, #28118, .T. ) ;
#15184 = CARTESIAN_POINT ( 'NONE',  ( 43.06614223494208460, 7.660936950709002602, -75.35385097105195484 ) ) ;
#15185 = CARTESIAN_POINT ( 'NONE',  ( 17.90525307069644612, -9.025334985065097015, -42.03615321375040992 ) ) ;
#15186 = CARTESIAN_POINT ( 'NONE',  ( 13.51721710176069813, 20.04444091306159947, -22.28354745645999913 ) ) ;
#15187 = CARTESIAN_POINT ( 'NONE',  ( 47.12245394960979894, -39.27662683125719667, -35.02700949942419584 ) ) ;
#15188 = CARTESIAN_POINT ( 'NONE',  ( 14.02133164252290065, -8.887187858349010483, -53.85598711143169481 ) ) ;
#15189 = CARTESIAN_POINT ( 'NONE',  ( 52.78885562451659297, 18.47641143109279938, -48.87892841330330640 ) ) ;
#15190 = CARTESIAN_POINT ( 'NONE',  ( 54.72151381108420765, -45.94167981062680184, -15.73273755979830213 ) ) ;
#15191 = LINE ( 'NONE', #31152, #40705 ) ;
#15192 = ORIENTED_EDGE ( 'NONE', *, *, #32015, .F. ) ;
#15193 = ADVANCED_FACE ( 'NONE', ( #19951 ), #51684, .F. ) ;
#15194 = CARTESIAN_POINT ( 'NONE',  ( 8.350530164053800775, -16.61895995459930120, -32.24671282160349506 ) ) ;
#15195 = ORIENTED_EDGE ( 'NONE', *, *, #42419, .F. ) ;
#15196 = EDGE_CURVE ( 'NONE', #33336, #30137, #21306, .T. ) ;
#15197 = CARTESIAN_POINT ( 'NONE',  ( 11.93174564592020026, -65.43929186371940432, -17.93019396377230024 ) ) ;
#15198 = CARTESIAN_POINT ( 'NONE',  ( 9.548543281838000496, 32.54799942213450237, -46.53732641210050502 ) ) ;
#15199 = CARTESIAN_POINT ( 'NONE',  ( 72.76396860142250489, 1.388715606738730068, -62.57493595107060713 ) ) ;
#15200 = CONICAL_SURFACE ( 'NONE', #44519, 0.7349999999999987654, 0.06981317007977388966 ) ;
#15201 = CARTESIAN_POINT ( 'NONE',  ( 22.46007751831445276, -20.47790136755202184, -40.00067590845137033 ) ) ;
#15203 = EDGE_CURVE ( 'NONE', #17902, #7053, #5881, .T. ) ;
#15202 = CARTESIAN_POINT ( 'NONE',  ( 53.51280994016380532, -49.43204902681937796, -49.22146059094290393 ) ) ;
#15204 = LINE ( 'NONE', #35634, #43407 ) ;
#15205 = AXIS2_PLACEMENT_3D ( 'NONE', #32997, #776, #523 ) ;
#15206 = AXIS2_PLACEMENT_3D ( 'NONE', #21124, #20597, #24781 ) ;
#15207 = CARTESIAN_POINT ( 'NONE',  ( 53.06587257203489827, -52.00459370491639532, -53.44894298165189639 ) ) ;
#15208 = EDGE_CURVE ( 'NONE', #7609, #39844, #38890, .T. ) ;
#15209 = VERTEX_POINT ( 'NONE', #15003 ) ;
#15210 = FACE_OUTER_BOUND ( 'NONE', #30056, .T. ) ;
#15211 = CARTESIAN_POINT ( 'NONE',  ( 10.77236125395059929, -63.28329410503849317, -45.20487655624160084 ) ) ;
#15212 = CARTESIAN_POINT ( 'NONE',  ( 69.22748654599826068, 19.47158195952029303, -72.59354914830210248 ) ) ;
#15213 = ORIENTED_EDGE ( 'NONE', *, *, #32495, .T. ) ;
#15214 = CARTESIAN_POINT ( 'NONE',  ( 23.54919931531921762, -18.42977095681591138, -43.90770150007058703 ) ) ;
#15215 = DIRECTION ( 'NONE',  ( -0.2517544074889990768, 0.9677911542837447367, 0.000000000000000000 ) ) ;
#15216 = CARTESIAN_POINT ( 'NONE',  ( 22.09114981806095557, -10.39072778660224472, -49.27845259825229363 ) ) ;
#15217 = ORIENTED_EDGE ( 'NONE', *, *, #39277, .F. ) ;
#15218 = SURFACE_SIDE_STYLE ('',( #23562 ) ) ;
#15219 = LINE ( 'NONE', #23302, #40106 ) ;
#15220 = CARTESIAN_POINT ( 'NONE',  ( 82.45630311851421368, 13.86034003618500066, -46.38988467804559690 ) ) ;
#15221 = EDGE_CURVE ( 'NONE', #11609, #25171, #15777, .T. ) ;
#15222 = CARTESIAN_POINT ( 'NONE',  ( 23.04645602048810460, -11.63204889956642596, -69.62566745447085736 ) ) ;
#15223 = CARTESIAN_POINT ( 'NONE',  ( 7.927515648975639984, -16.41453857865010235, -64.76146233876730207 ) ) ;
#15224 = DIRECTION ( 'NONE',  ( 0.8090169943749464521, -0.5877852522924744694, 0.000000000000000000 ) ) ;
#15225 = DIRECTION ( 'NONE',  ( 1.000000000000000000, 0.000000000000000000, 0.000000000000000000 ) ) ;
#15226 = DIRECTION ( 'NONE',  ( 1.000000000000000000, 0.000000000000000000, 0.000000000000000000 ) ) ;
#15227 = VERTEX_POINT ( 'NONE', #31480 ) ;
#15228 = ADVANCED_FACE ( 'NONE', ( #31731 ), #19449, .T. ) ;
#15229 = ORIENTED_EDGE ( 'NONE', *, *, #46274, .T. ) ;
#15230 = CARTESIAN_POINT ( 'NONE',  ( 43.60412366894710345, -43.70472620657429985, -5.064848484333539957 ) ) ;
#15231 = CARTESIAN_POINT ( 'NONE',  ( 10.77928268962459946, -10.43599910622039850, -53.47738634665349622 ) ) ;
#15232 = CARTESIAN_POINT ( 'NONE',  ( 47.13393739769622215, 7.372368883616073454, -54.64997583104464951 ) ) ;
#15233 = CARTESIAN_POINT ( 'NONE',  ( 11.14075301740580137, -21.57559600035230218, -32.14999999999999858 ) ) ;
#15234 = CARTESIAN_POINT ( 'NONE',  ( 47.37032930261479891, 23.44277967668870133, -74.17365615959539582 ) ) ;
#15235 = CARTESIAN_POINT ( 'NONE',  ( 45.07858682377059978, -46.11248607424209922, -9.026855431852869316 ) ) ;
#15236 = DIRECTION ( 'NONE',  ( -0.6377178376951687655, 0.7702700562045746713, -4.336808689942011820E-16 ) ) ;
#15237 = VECTOR ( 'NONE', #29463, 1000.000000000000000 ) ;
#15238 = CIRCLE ( 'NONE', #35316, 3.000000000000004885 ) ;
#15239 = CARTESIAN_POINT ( 'NONE',  ( 12.14266246862359999, 33.62769506002970132, -16.13799733647190138 ) ) ;
#15240 = EDGE_CURVE ( 'NONE', #14039, #15968, #45242, .T. ) ;
#15241 = CARTESIAN_POINT ( 'NONE',  ( 8.261206528015369699, -18.06625616060409811, -62.41163166630260406 ) ) ;
#15242 = CARTESIAN_POINT ( 'NONE',  ( 52.61516928385270120, -49.80859478947380126, -27.82854103740449858 ) ) ;
#15243 = CARTESIAN_POINT ( 'NONE',  ( 56.79288265842479433, -50.66783009735559773, -74.14912528235450395 ) ) ;
#15245 = CARTESIAN_POINT ( 'NONE',  ( 15.24805746485052715, -8.849198816118178712, -59.91112637248544104 ) ) ;
#15244 = CARTESIAN_POINT ( 'NONE',  ( -4.702024263459519737, 16.16474464310789827, -5.099307284078279601 ) ) ;
#15246 = DIRECTION ( 'NONE',  ( 1.000000000000000000, 0.000000000000000000, 0.000000000000000000 ) ) ;
#15247 = CARTESIAN_POINT ( 'NONE',  ( 27.73905384484250192, -53.11618894467930119, -74.14999999999999147 ) ) ;
#15248 = ORIENTED_EDGE ( 'NONE', *, *, #27849, .F. ) ;
#15249 = CARTESIAN_POINT ( 'NONE',  ( -8.110719422787710187, -44.87935480251360332, -5.130695632534920669 ) ) ;
#15250 = CARTESIAN_POINT ( 'NONE',  ( 47.60001556901690378, 23.30894354097369714, -54.85861573280610060 ) ) ;
#15251 = CARTESIAN_POINT ( 'NONE',  ( 57.34505690168419534, -45.81270932441739774, -26.27162216713519882 ) ) ;
#15252 = DIRECTION ( 'NONE',  ( -0.9486832980505123247, 1.161801964362114161E-16, 0.3162277660168421045 ) ) ;
#15253 = CARTESIAN_POINT ( 'NONE',  ( 61.12214340571450322, 14.22653868544119860, -47.44127583901740053 ) ) ;
#15254 = CARTESIAN_POINT ( 'NONE',  ( 9.117428229974370524, -13.11113547131370005, -75.34181132021248573 ) ) ;
#15255 = CARTESIAN_POINT ( 'NONE',  ( 52.13018002042409904, 18.64453568514510096, -76.92945343287659909 ) ) ;
#15256 = CARTESIAN_POINT ( 'NONE',  ( 52.81415214587489970, 18.43716763046850105, -48.60514635218409296 ) ) ;
#15257 = CARTESIAN_POINT ( 'NONE',  ( 23.83903667619928868, -17.68686933249846405, -69.87566771576088342 ) ) ;
#15258 = CARTESIAN_POINT ( 'NONE',  ( 52.82975622904280755, -49.66092049964720445, -48.48626292588439668 ) ) ;
#15259 = CARTESIAN_POINT ( 'NONE',  ( 54.94524618045259956, 16.46847369675259642, -26.58277649024360301 ) ) ;
#15260 = CARTESIAN_POINT ( 'NONE',  ( 16.13393739769620083, -15.61618894467929941, 4.450000000000000178 ) ) ;
#15261 = CARTESIAN_POINT ( 'NONE',  ( 17.14078862016341276, -23.46602985074793679, -61.96707586313608118 ) ) ;
#15262 = CARTESIAN_POINT ( 'NONE',  ( 8.815605938724019097, -63.28267558148569094, -46.67186391142220003 ) ) ;
#15263 = CARTESIAN_POINT ( 'NONE',  ( 42.78018059643970616, 11.47668021806869909, -3.187564294433590462 ) ) ;
#15264 = CARTESIAN_POINT ( 'NONE',  ( 64.56161859372949152, -31.20701609037800139, -16.82687391434760116 ) ) ;
#15266 = ADVANCED_FACE ( 'NONE', ( #11601 ), #5041, .T. ) ;
#15265 = CARTESIAN_POINT ( 'NONE',  ( 71.14534185144368905, 1.334812829108570131, -60.78020385162600547 ) ) ;
#15267 = CARTESIAN_POINT ( 'NONE',  ( 11.13393739769619906, 32.06972070065159386, -43.74696042565229703 ) ) ;
#15268 = CARTESIAN_POINT ( 'NONE',  ( 72.47916642748789684, 1.432916438945919912, -61.86369887538009493 ) ) ;
#15269 = CARTESIAN_POINT ( 'NONE',  ( 51.40028038159698553, -34.49096119182996745, -76.69282701588583961 ) ) ;
#15270 = EDGE_CURVE ( 'NONE', #40473, #50288, #34367, .T. ) ;
#15271 = CARTESIAN_POINT ( 'NONE',  ( 61.28610861176739633, -45.23040055550220018, -28.15000000000000213 ) ) ;
#15272 = ORIENTED_EDGE ( 'NONE', *, *, #16144, .F. ) ;
#15273 = ORIENTED_EDGE ( 'NONE', *, *, #14135, .T. ) ;
#15274 = CARTESIAN_POINT ( 'NONE',  ( 56.66762828431429710, 19.14715517649329968, -52.77094437924129977 ) ) ;
#15275 = CARTESIAN_POINT ( 'NONE',  ( 49.88572956512600598, -29.68138763751254672, -15.90126589776440902 ) ) ;
#15276 = VERTEX_POINT ( 'NONE', #47445 ) ;
#15277 = CARTESIAN_POINT ( 'NONE',  ( 55.96457922517269878, -45.97039086805419572, -25.73835096114130039 ) ) ;
#15278 = CARTESIAN_POINT ( 'NONE',  ( 16.13128530227220025, -23.52718894015337980, -78.00777821068726325 ) ) ;
#15279 = AXIS2_PLACEMENT_3D ( 'NONE', #46750, #6904, #11094 ) ;
#15280 = ORIENTED_EDGE ( 'NONE', *, *, #16851, .F. ) ;
#15281 = CIRCLE ( 'NONE', #16116, 20.00000000000001421 ) ;
#15282 = CARTESIAN_POINT ( 'NONE',  ( 11.11663740960502977, 33.77554069907087353, -23.06313725433601647 ) ) ;
#15283 = CARTESIAN_POINT ( 'NONE',  ( 43.35947853168794808, 6.597306704977007108, -73.52222986434853169 ) ) ;
#15284 = CARTESIAN_POINT ( 'NONE',  ( 11.00910675228320024, 32.24153982397250218, -24.02516935458699976 ) ) ;
#15285 = ORIENTED_EDGE ( 'NONE', *, *, #46532, .F. ) ;
#15286 = CARTESIAN_POINT ( 'NONE',  ( 55.00894648611440374, -45.11618894467940066, -13.91245063309409957 ) ) ;
#15287 = CARTESIAN_POINT ( 'NONE',  ( 51.23914035111342713, 0.5199290082084727649, -17.21756640535365790 ) ) ;
#15288 = CARTESIAN_POINT ( 'NONE',  ( 10.64977475916229999, 33.62388472332079914, -18.05902683574160150 ) ) ;
#15289 = EDGE_CURVE ( 'NONE', #24229, #48161, #15084, .T. ) ;
#15290 = CARTESIAN_POINT ( 'NONE',  ( 59.85171547485399657, -28.82033292544180014, -15.75458271846640024 ) ) ;
#15291 = DIRECTION ( 'NONE',  ( 0.000000000000000000, 0.7071067811865457964, -0.7071067811865492381 ) ) ;
#15292 = CARTESIAN_POINT ( 'NONE',  ( 46.84316060478769828, -53.76087950960219786, -75.90467361879859709 ) ) ;
#15293 = CARTESIAN_POINT ( 'NONE',  ( 8.586485337726889711, -17.76623897297480070, -78.92415710861520495 ) ) ;
#15294 = CARTESIAN_POINT ( 'NONE',  ( 12.72596619939935003, -21.52911186578291236, -37.11948596911255294 ) ) ;
#15295 = CARTESIAN_POINT ( 'NONE',  ( 41.01789762497119796, 13.77558802515430081, -5.564947099249000217 ) ) ;
#15296 = DIRECTION ( 'NONE',  ( -0.4439767838697923907, -0.8960382890170686121, 0.000000000000000000 ) ) ;
#15297 = CARTESIAN_POINT ( 'NONE',  ( 84.44784216359251161, -43.11618894467930119, -47.47585302082339354 ) ) ;
#15298 = CARTESIAN_POINT ( 'NONE',  ( 11.49541412066449375, 34.11692877646753175, -17.78290583436891836 ) ) ;
#15299 = ADVANCED_FACE ( 'NONE', ( #15210 ), #10764, .T. ) ;
#15300 = CARTESIAN_POINT ( 'NONE',  ( 12.59304842796170121, -22.61967803536170152, -79.93650932190239189 ) ) ;
#15301 = ORIENTED_EDGE ( 'NONE', *, *, #45781, .F. ) ;
#15303 = EDGE_CURVE ( 'NONE', #47835, #35625, #49463, .T. ) ;
#15302 = CARTESIAN_POINT ( 'NONE',  ( 54.62083344167059806, -48.06803323320840349, -26.73900343537430047 ) ) ;
#15304 = CARTESIAN_POINT ( 'NONE',  ( 0.4116173174696240444, -53.57266544184560075, -8.235445646974270062 ) ) ;
#15305 = CARTESIAN_POINT ( 'NONE',  ( 76.15791883449350053, -14.05836797832549934, -12.10556864792070009 ) ) ;
#15306 = CARTESIAN_POINT ( 'NONE',  ( 75.39077318432113373, 12.99911917340609513, -13.71505546934280417 ) ) ;
#15307 = B_SPLINE_CURVE_WITH_KNOTS ( 'NONE', 3,
 ( #51672, #3722, #3207, #34901, #19941, #31719, #47240, #15515, #31469, #48000, #47744, #50900, #35931, #46990, #11075, #7395, #7658, #11589, #43046, #23344, #7142, #27550, #19178, #43557, #35157, #23601, #39366, #27808, #15258, #19439 ),
 .UNSPECIFIED., .F., .F.,
 ( 4, 2, 2, 2, 2, 2, 2, 2, 2, 2, 2, 2, 2, 2, 4 ),
 ( 0.000000000000000000, 0.09071737296906999537, 0.2140426870042120011, 0.2911210082761760409, 0.3773790848024499711, 0.4312903826313709832, 0.4852016804602920508, 0.5283307187234289604, 0.5714597569865670357, 0.6404662182075859800, 0.6753556120789150352, 0.7102450059502449786, 0.7544326870336059976, 0.8251329767669829396, 0.8625807652627419664 ),
 .UNSPECIFIED. ) ;
#15308 = CARTESIAN_POINT ( 'NONE',  ( 12.44378449474779913, -49.98269640123930202, -21.13285771871539964 ) ) ;
#15309 = DIRECTION ( 'NONE',  ( 0.000000000000000000, 0.000000000000000000, -1.000000000000000000 ) ) ;
#15310 = AXIS2_PLACEMENT_3D ( 'NONE', #39522, #40030, #28213 ) ;
#15311 = CARTESIAN_POINT ( 'NONE',  ( 9.366980835600751121, -15.61636285886159925, -47.84717978380999881 ) ) ;
#15312 = CARTESIAN_POINT ( 'NONE',  ( 82.36128958404080436, -45.10908765980170188, -46.45434936409679949 ) ) ;
#15313 = CARTESIAN_POINT ( 'NONE',  ( 57.39005023914570103, -50.59266058909979336, -53.60531501353280248 ) ) ;
#15314 = CARTESIAN_POINT ( 'NONE',  ( 43.27773194996530037, 11.67331461295569994, -4.515873930613719445 ) ) ;
#15315 = DIRECTION ( 'NONE',  ( -1.000000000000000000, 0.000000000000000000, 0.000000000000000000 ) ) ;
#15316 = CARTESIAN_POINT ( 'NONE',  ( 0.2019267050627020776, 14.82321529695447992, -34.66067870389102978 ) ) ;
#15317 = CARTESIAN_POINT ( 'NONE',  ( 59.42623547831379938, -46.20484020020990101, -47.44643030202959721 ) ) ;
#15318 = CARTESIAN_POINT ( 'NONE',  ( 70.83393739769719843, -48.11618894467220287, -73.25000000000000000 ) ) ;
#15319 = CARTESIAN_POINT ( 'NONE',  ( 104.6856170952509757, -28.80002732851879088, -29.09832030244561807 ) ) ;
#15320 = CARTESIAN_POINT ( 'NONE',  ( 18.43159307031459804, -52.07648608105650112, -75.48775473117470369 ) ) ;
#15321 = CARTESIAN_POINT ( 'NONE',  ( 51.07994173643560032, -52.78781467787970882, -53.74568964421160189 ) ) ;
#15322 = EDGE_CURVE ( 'NONE', #26340, #4326, #32631, .T. ) ;
#15323 = CARTESIAN_POINT ( 'NONE',  ( 15.01392763274439979, -22.98180313935129959, -65.61537668992708916 ) ) ;
#15324 = CARTESIAN_POINT ( 'NONE',  ( 17.16952488601623728, -7.705194658554545661, -77.33399647545617484 ) ) ;
#15325 = CARTESIAN_POINT ( 'NONE',  ( 63.27571426518280617, 1.027568165752089868, -62.14345989183700425 ) ) ;
#15326 = VERTEX_POINT ( 'NONE', #31417 ) ;
#15327 = DIRECTION ( 'NONE',  ( -1.000000000000000000, 0.000000000000000000, 0.000000000000000000 ) ) ;
#15328 = CARTESIAN_POINT ( 'NONE',  ( 18.88229416847884679, -21.86306642924426313, -34.82060356745882501 ) ) ;
#15329 = CARTESIAN_POINT ( 'NONE',  ( 73.08914738367541020, 1.188582381068100213, -68.85996346914730282 ) ) ;
#15330 = CARTESIAN_POINT ( 'NONE',  ( 10.22109171085586965, -12.20808510601136909, -73.61948688482468128 ) ) ;
#15331 = CARTESIAN_POINT ( 'NONE',  ( 10.69159450438010062, -10.36448435242919963, -81.23899999999999011 ) ) ;
#15332 = CARTESIAN_POINT ( 'NONE',  ( 43.08927530004059747, -45.90404663275549524, -7.588629812463259405 ) ) ;
#15333 = ADVANCED_FACE ( 'NONE', ( #39066 ), #3158, .T. ) ;
#15334 = VERTEX_POINT ( 'NONE', #11540 ) ;
#15335 = CARTESIAN_POINT ( 'NONE',  ( 17.59779143982609639, 21.21781726285519909, -76.03742712147929694 ) ) ;
#15336 = ORIENTED_EDGE ( 'NONE', *, *, #35357, .T. ) ;
#15337 = AXIS2_PLACEMENT_3D ( 'NONE', #1442, #14272, #26303 ) ;
#15338 = ORIENTED_EDGE ( 'NONE', *, *, #20418, .T. ) ;
#15339 = DIRECTION ( 'NONE',  ( 0.000000000000000000, 0.000000000000000000, 1.000000000000000000 ) ) ;
#15340 = CARTESIAN_POINT ( 'NONE',  ( 23.28014774377560059, -12.88775224658349927, -81.23899999999999011 ) ) ;
#15341 = CARTESIAN_POINT ( 'NONE',  ( 71.71126032029680175, -45.25223929932899125, -47.09707863094710945 ) ) ;
#15342 = DIRECTION ( 'NONE',  ( 1.130501000000000083E-17, -8.343543999999999066E-19, -1.000000000000000000 ) ) ;
#15343 = ORIENTED_EDGE ( 'NONE', *, *, #24047, .F. ) ;
#15344 = CARTESIAN_POINT ( 'NONE',  ( 22.46010023493453645, -10.75450771427420449, -53.29933757767130231 ) ) ;
#15345 = ORIENTED_EDGE ( 'NONE', *, *, #24450, .F. ) ;
#15346 = CARTESIAN_POINT ( 'NONE',  ( 24.04493737255387487, -14.58064479785229217, -63.75066696746915795 ) ) ;
#15347 = CARTESIAN_POINT ( 'NONE',  ( 20.13393739769620083, -2.337132753317949785, -39.64999999999999858 ) ) ;
#15348 = AXIS2_PLACEMENT_3D ( 'NONE', #46462, #3199, #18909 ) ;
#15349 = ORIENTED_EDGE ( 'NONE', *, *, #36092, .F. ) ;
#15350 = CARTESIAN_POINT ( 'NONE',  ( 72.82769086651219936, 1.383811055320669947, -62.77287342953649585 ) ) ;
#15352 = CARTESIAN_POINT ( 'NONE',  ( 52.01748110390389712, -51.11128007685600494, -76.09025191383899767 ) ) ;
#15351 = VECTOR ( 'NONE', #31355, 1000.000000000000000 ) ;
#15353 = CARTESIAN_POINT ( 'NONE',  ( 60.32372535534909730, 14.61230269747050059, -47.67141866289379948 ) ) ;
#15354 = DIRECTION ( 'NONE',  ( 0.8660254037844259400, -0.5000000000000219824, 0.000000000000000000 ) ) ;
#15355 = LINE ( 'NONE', #44939, #1621 ) ;
#15356 = CARTESIAN_POINT ( 'NONE',  ( -3.258131835852990044, 17.22944021436429907, -5.041088719362160298 ) ) ;
#15357 = CARTESIAN_POINT ( 'NONE',  ( 47.03254412713606314, 23.23399685673784631, -75.29848680170620412 ) ) ;
#15358 = CARTESIAN_POINT ( 'NONE',  ( 33.53393739769619231, -15.61618894538776559, -7.049999999999999822 ) ) ;
#15359 = EDGE_CURVE ( 'NONE', #44438, #5111, #50098, .T. ) ;
#15360 = CARTESIAN_POINT ( 'NONE',  ( 18.44579043026860177, -8.116716713984079234, -48.88268834496359716 ) ) ;
#15361 = EDGE_LOOP ( 'NONE', ( #4430, #45696, #20795, #44347, #15004 ) ) ;
#15363 = ADVANCED_FACE ( 'NONE', ( #8628 ), #49442, .F. ) ;
#15362 = CARTESIAN_POINT ( 'NONE',  ( 57.26570439199549867, 16.10442508092609870, -47.75313496841199878 ) ) ;
#15364 = AXIS2_PLACEMENT_3D ( 'NONE', #39552, #27989, #23789 ) ;
#15365 = DIRECTION ( 'NONE',  ( 0.000000000000000000, 0.000000000000000000, 1.000000000000000000 ) ) ;
#15366 = CARTESIAN_POINT ( 'NONE',  ( 71.46698656264879901, 1.308647200627810259, -70.40208447574099182 ) ) ;
#15367 = EDGE_CURVE ( 'NONE', #19986, #44502, #32964, .T. ) ;
#15368 = CARTESIAN_POINT ( 'NONE',  ( 45.59441226390927682, -40.06939850403506398, -58.92915879617162744 ) ) ;
#15369 = CARTESIAN_POINT ( 'NONE',  ( 15.00539844365889941, 19.69078932486479871, -21.20430891277120011 ) ) ;
#15370 = DIRECTION ( 'NONE',  ( 0.000000000000000000, -1.000000000000000000, 0.000000000000000000 ) ) ;
#15371 = CARTESIAN_POINT ( 'NONE',  ( 9.647229718197021242, -18.13221079759153298, -45.72885989622667324 ) ) ;
#15372 = CARTESIAN_POINT ( 'NONE',  ( 61.50409964636570237, 14.14168666559669951, -47.35437808293550432 ) ) ;
#15373 = CARTESIAN_POINT ( 'NONE',  ( 48.30764984760519809, -54.18332414096600047, -54.81566210031060393 ) ) ;
#15374 = PLANE ( 'NONE',  #33955 ) ;
#15375 = CARTESIAN_POINT ( 'NONE',  ( 64.93393739769619799, 1.883811055320669947, -69.84999999999999432 ) ) ;
#15376 = CARTESIAN_POINT ( 'NONE',  ( 47.82941845642289991, 23.15673897679920046, -54.71834399002119653 ) ) ;
#15377 = VERTEX_POINT ( 'NONE', #1021 ) ;
#15378 = AXIS2_PLACEMENT_3D ( 'NONE', #46070, #5968, #41601 ) ;
#15379 = CARTESIAN_POINT ( 'NONE',  ( 16.02785660032570192, -23.06571518483509919, -37.57187509340590026 ) ) ;
#15380 = VECTOR ( 'NONE', #27963, 1000.000000000000000 ) ;
#15381 = ORIENTED_EDGE ( 'NONE', *, *, #8251, .F. ) ;
#15382 = CARTESIAN_POINT ( 'NONE',  ( 17.82929433848870104, 21.38896804161856124, -76.01806011806066010 ) ) ;
#15383 = CARTESIAN_POINT ( 'NONE',  ( 60.37123110817940130, -45.73378107691389971, -47.43125510679269752 ) ) ;
#15384 = CARTESIAN_POINT ( 'NONE',  ( 53.41693480158270546, -49.35328119387190071, -48.75416851881869462 ) ) ;
#15385 = LINE ( 'NONE', #11715, #1835 ) ;
#15387 = PLANE ( 'NONE',  #27278 ) ;
#15386 = CARTESIAN_POINT ( 'NONE',  ( 83.34325726105171839, 14.07779472782969954, -47.50551966704799867 ) ) ;
#15388 = CARTESIAN_POINT ( 'NONE',  ( 29.35444738288253674, 4.484612253612125343, -84.62343415937573354 ) ) ;
#15389 = CARTESIAN_POINT ( 'NONE',  ( 16.13393739769620083, -15.61618894467929941, 8.349999999999999645 ) ) ;
#15390 = EDGE_CURVE ( 'NONE', #39228, #5583, #35162, .T. ) ;
#15391 = EDGE_LOOP ( 'NONE', ( #46816, #18868, #37892, #20538 ) ) ;
#15392 = DIRECTION ( 'NONE',  ( 0.2169304578186566079, 0.000000000000000000, -0.9761870601839527373 ) ) ;
#15393 = ORIENTED_EDGE ( 'NONE', *, *, #49637, .T. ) ;
#15394 = CARTESIAN_POINT ( 'NONE',  ( 21.69971205180370077, -19.94801438831689921, -59.05769930218669828 ) ) ;
#15395 = CARTESIAN_POINT ( 'NONE',  ( 17.16943041195074926, -7.705181169127810037, -39.33399222304974074 ) ) ;
#15396 = CARTESIAN_POINT ( 'NONE',  ( 12.96406378517139935, 34.28324915654220462, -47.66759396690779482 ) ) ;
#15397 = CARTESIAN_POINT ( 'NONE',  ( 10.41800581969009976, -64.65214231680860735, -46.79321165223139900 ) ) ;
#15398 = ORIENTED_EDGE ( 'NONE', *, *, #8583, .F. ) ;
#15399 = ORIENTED_EDGE ( 'NONE', *, *, #46405, .F. ) ;
#15400 = DIRECTION ( 'NONE',  ( 0.000000000000000000, 0.000000000000000000, -1.000000000000000000 ) ) ;
#15401 = CARTESIAN_POINT ( 'NONE',  ( 22.90571047178253394, -13.64498330036649421, -32.75701418906501772 ) ) ;
#15402 = CARTESIAN_POINT ( 'NONE',  ( 56.45988984176000258, -50.72305344967870155, -53.39311493514949802 ) ) ;
#15403 = CONICAL_SURFACE ( 'NONE', #44682, 0.7980000000000000426, 0.7853981633974476129 ) ;
#15404 = B_SPLINE_CURVE_WITH_KNOTS ( 'NONE', 3,
 ( #38593, #50386, #22058, #22318, #46464, #42525, #10552, #30188 ),
 .UNSPECIFIED., .F., .F.,
 ( 4, 2, 2, 4 ),
 ( 0.000000000000000000, 0.3098045115950139317, 0.9301223358193300150, 1.000000000000000000 ),
 .UNSPECIFIED. ) ;
#15405 = DIRECTION ( 'NONE',  ( 0.000000000000000000, 1.000000000000000000, 0.000000000000000000 ) ) ;
#15406 = CARTESIAN_POINT ( 'NONE',  ( 65.32687762751260152, -0.2389500108568909931, -16.78952551121680159 ) ) ;
#15407 = CARTESIAN_POINT ( 'NONE',  ( 51.67588111593500599, -48.61618684213020458, -77.01364305260700860 ) ) ;
#15408 = B_SPLINE_CURVE_WITH_KNOTS ( 'NONE', 3,
 ( #4387, #20355, #48951, #13052, #36342 ),
 .UNSPECIFIED., .F., .F.,
 ( 4, 1, 4 ),
 ( 0.000000000000000000, 0.5000000000000000000, 1.000000000000000000 ),
 .UNSPECIFIED. ) ;
#15409 = CARTESIAN_POINT ( 'NONE',  ( 14.07181180123552267, -52.32662977626135614, -75.76245441612901743 ) ) ;
#15410 =( BOUNDED_CURVE ( )  B_SPLINE_CURVE ( 2, ( #21283, #37288, #865, #40187, #37027 ),
 .UNSPECIFIED., .F., .T. ) 
 B_SPLINE_CURVE_WITH_KNOTS ( ( 3, 2, 3 ),
 ( -0.003205554299145560102, 0.8238407534178779912, 1.650887061134900025 ),
 .UNSPECIFIED. ) 
 CURVE ( )  GEOMETRIC_REPRESENTATION_ITEM ( )  RATIONAL_B_SPLINE_CURVE ( ( 1.000000000000000000, 0.9157107718028779653, 1.000000000000000000, 0.9157107718028449916, 1.000000000000000000 ) ) 
 REPRESENTATION_ITEM ( '' )  );
#15411 = ORIENTED_EDGE ( 'NONE', *, *, #1757, .T. ) ;
#15412 = CARTESIAN_POINT ( 'NONE',  ( 63.25402410758490390, 0.9098571636355720083, -69.14090909090960224 ) ) ;
#15413 = DIRECTION ( 'NONE',  ( 0.000000000000000000, 1.000000000000000000, 0.000000000000000000 ) ) ;
#15414 = CARTESIAN_POINT ( 'NONE',  ( 31.39345689194515643, -4.529499075180571488, 17.07360679774999923 ) ) ;
#15415 = DIRECTION ( 'NONE',  ( 0.000000000000000000, -1.000000000000000000, 0.000000000000000000 ) ) ;
#15416 = CARTESIAN_POINT ( 'NONE',  ( 8.372471907742799146, -14.45584372025490083, -57.05973213505629360 ) ) ;
#15417 = CARTESIAN_POINT ( 'NONE',  ( 12.27824370503449991, -50.15233315604800168, -21.14999999870460101 ) ) ;
#15418 = CARTESIAN_POINT ( 'NONE',  ( 56.85087055762509323, 19.38381105532069881, -75.22080214333730908 ) ) ;
#15419 = CIRCLE ( 'NONE', #44691, 2.000000000000000000 ) ;
#15420 = DIRECTION ( 'NONE',  ( 1.224646799147353207E-16, 1.000000000000000000, -0.000000000000000000 ) ) ;
#15421 = CARTESIAN_POINT ( 'NONE',  ( 56.50061855791859955, 14.14892826505740153, -17.93020493892149858 ) ) ;
#15422 = CARTESIAN_POINT ( 'NONE',  ( 60.77439903042079550, -45.49849954229439675, -47.09774554394410018 ) ) ;
#15423 = VECTOR ( 'NONE', #40248, 1000.000000000000000 ) ;
#15424 = CARTESIAN_POINT ( 'NONE',  ( 56.62432785517169975, -50.71560893929619596, -53.83726655417689955 ) ) ;
#15425 = AXIS2_PLACEMENT_3D ( 'NONE', #8080, #43976, #19609 ) ;
#15426 = CARTESIAN_POINT ( 'NONE',  ( 22.24871428180119892, -12.10163878398070025, -56.68113137027810211 ) ) ;
#15427 = CARTESIAN_POINT ( 'NONE',  ( 14.36260794969588162, -9.025336946788870662, -43.86945627782853308 ) ) ;
#15428 = ORIENTED_EDGE ( 'NONE', *, *, #18899, .F. ) ;
#15430 = EDGE_CURVE ( 'NONE', #17080, #47621, #10751, .T. ) ;
#15429 = CARTESIAN_POINT ( 'NONE',  ( 13.76101809997250136, -51.29511715723850074, -74.14992839339309683 ) ) ;
#15431 = CARTESIAN_POINT ( 'NONE',  ( 64.98165955279600325, 1.327322800621349996, -60.84198109300940160 ) ) ;
#15432 = CARTESIAN_POINT ( 'NONE',  ( 22.46012145614304245, -10.75453683683663719, -51.29933284102181545 ) ) ;
#15433 = CARTESIAN_POINT ( 'NONE',  ( 17.92370450339619836, 19.88381105532299742, -74.14999999999999147 ) ) ;
#15434 = CARTESIAN_POINT ( 'NONE',  ( 20.11810581040045776, -8.703687945963876516, -47.17433608290784974 ) ) ;
#15435 = CARTESIAN_POINT ( 'NONE',  ( 47.20372080753160304, -53.97904105312669287, -75.66073271794819277 ) ) ;
#15436 = CARTESIAN_POINT ( 'NONE',  ( 11.89433743672330124, 34.20374474164479750, -18.12680249707489821 ) ) ;
#15437 = AXIS2_PLACEMENT_3D ( 'NONE', #7685, #23630, #48804 ) ;
#15438 = CARTESIAN_POINT ( 'NONE',  ( 71.67217357260551580, 0.9170823515327869435, -70.49605724842390941 ) ) ;
#15440 = CARTESIAN_POINT ( 'NONE',  ( 43.22703756266240305, -37.76642993860559727, -74.18277498300450645 ) ) ;
#15439 = LINE ( 'NONE', #11512, #23926 ) ;
#15441 = CARTESIAN_POINT ( 'NONE',  ( 5.758805994657699934, -59.74572380576150010, -13.93820318808900005 ) ) ;
#15442 = CARTESIAN_POINT ( 'NONE',  ( 49.36944273108730386, 22.50304657733999747, -54.70700368065020314 ) ) ;
#15443 = VERTEX_POINT ( 'NONE', #48461 ) ;
#15444 = CARTESIAN_POINT ( 'NONE',  ( 52.78885568635549674, -49.70878928925869644, -48.87892847977669675 ) ) ;
#15445 = ORIENTED_EDGE ( 'NONE', *, *, #27139, .T. ) ;
#15446 = CARTESIAN_POINT ( 'NONE',  ( 42.37737783785518531, 7.575582158853551462, -78.76371035586005576 ) ) ;
#15447 = LINE ( 'NONE', #24824, #21840 ) ;
#15448 = CARTESIAN_POINT ( 'NONE',  ( 11.90611060580384084, 34.20474548859955632, -18.00436963405675428 ) ) ;
#15449 = CARTESIAN_POINT ( 'NONE',  ( 71.33393739769628894, 10.88381105532070059, -61.94999999999999574 ) ) ;
#15450 = CARTESIAN_POINT ( 'NONE',  ( 11.39331812359460194, -10.39420775028169963, -59.71818801013959899 ) ) ;
#15451 = FACE_OUTER_BOUND ( 'NONE', #17840, .T. ) ;
#15452 = CARTESIAN_POINT ( 'NONE',  ( 55.58072258071959482, -45.98463045567079632, -16.80393901860190198 ) ) ;
#15453 = ADVANCED_FACE ( 'NONE', ( #20659 ), #55, .T. ) ;
#15454 = CARTESIAN_POINT ( 'NONE',  ( 16.65420337844999921, -51.11618894467930119, -20.15000000000000213 ) ) ;
#15455 = ORIENTED_EDGE ( 'NONE', *, *, #33862, .F. ) ;
#15456 = AXIS2_PLACEMENT_3D ( 'NONE', #20043, #7499, #26883 ) ;
#15457 = CARTESIAN_POINT ( 'NONE',  ( 8.346677780718652073, -14.64390511730509914, -40.32704379009269502 ) ) ;
#15458 = EDGE_CURVE ( 'NONE', #17902, #19884, #5924, .T. ) ;
#15459 = ORIENTED_EDGE ( 'NONE', *, *, #39034, .T. ) ;
#15460 = CARTESIAN_POINT ( 'NONE',  ( 11.74995130100939988, -65.25618184072669692, -17.00864122140729862 ) ) ;
#15461 = CARTESIAN_POINT ( 'NONE',  ( 10.41478454943800003, 33.42186449018819872, -46.79156209876850170 ) ) ;
#15462 = CARTESIAN_POINT ( 'NONE',  ( 72.79675206836721202, 1.372372808637209785, -62.39142423721519748 ) ) ;
#15463 = CARTESIAN_POINT ( 'NONE',  ( 50.10014236208279215, -52.83395586467779736, -53.32348334894899722 ) ) ;
#15464 = DIRECTION ( 'NONE',  ( -0.4872913772396108012, -0.8732394366197184787, 0.000000000000000000 ) ) ;
#15465 = DIRECTION ( 'NONE',  ( 0.3294064756441278941, 0.9441882088883097879, 0.000000000000000000 ) ) ;
#15466 = ORIENTED_EDGE ( 'NONE', *, *, #7052, .F. ) ;
#15467 = CARTESIAN_POINT ( 'NONE',  ( 64.68925548900169531, 0.9369374701296260266, -70.56272516144500173 ) ) ;
#15468 = CARTESIAN_POINT ( 'NONE',  ( 11.13393739769619906, -63.11543068638779630, -43.91250110351749925 ) ) ;
#15469 = CARTESIAN_POINT ( 'NONE',  ( 65.43042069958036677, 17.98087126525108914, -68.79648330188406646 ) ) ;
#15470 = EDGE_LOOP ( 'NONE', ( #18261, #32977, #36908, #34018 ) ) ;
#15471 = CARTESIAN_POINT ( 'NONE',  ( 14.35970537249007428, -23.39490274268978709, -44.36388938044733266 ) ) ;
#15472 = CARTESIAN_POINT ( 'NONE',  ( 56.72051766552240082, 19.45439143119729763, -53.84018978621849527 ) ) ;
#15473 = CARTESIAN_POINT ( 'NONE',  ( 20.13393739768839552, 24.18330853958629945, -74.14999999999999147 ) ) ;
#15474 = VERTEX_POINT ( 'NONE', #48993 ) ;
#15475 = CARTESIAN_POINT ( 'NONE',  ( 24.04501723819814529, -15.61618889329698412, -35.50767088183642528 ) ) ;
#15476 = CARTESIAN_POINT ( 'NONE',  ( 19.31296351478369999, -49.88685839599860117, -82.14319696191608955 ) ) ;
#15477 = CARTESIAN_POINT ( 'NONE',  ( 14.72165982897219116, 20.94681317766939443, -75.92929758211541014 ) ) ;
#15478 = CARTESIAN_POINT ( 'NONE',  ( 83.89200044194980421, 19.38381105532069881, -53.92796738110899923 ) ) ;
#15479 = CARTESIAN_POINT ( 'NONE',  ( 21.47519512629029848, -21.89740585963049568, -62.06801868260419752 ) ) ;
#15480 = CIRCLE ( 'NONE', #28023, 1.500000000038269388 ) ;
#15481 = PLANE ( 'NONE',  #12145 ) ;
#15482 = CARTESIAN_POINT ( 'NONE',  ( 46.43957250303571982, -38.19754231318525939, -58.12182445229009886 ) ) ;
#15483 = APPLICATION_PROTOCOL_DEFINITION ( 'draft international standard', 'automotive_design', 1998, #4024 ) ;
#15484 = EDGE_LOOP ( 'NONE', ( #47358, #41822, #27362, #33724, #32561 ) ) ;
#15485 = VERTEX_POINT ( 'NONE', #13100 ) ;
#15486 = CARTESIAN_POINT ( 'NONE',  ( 43.75992007188810362, -43.62559376723620375, -5.076600545282080823 ) ) ;
#15487 = CARTESIAN_POINT ( 'NONE',  ( 9.133675843628138225, -18.16629325230719871, -57.12145717557989855 ) ) ;
#15488 = CARTESIAN_POINT ( 'NONE',  ( 46.03121500769550067, 13.88381105532070059, -7.582874790343590021 ) ) ;
#15489 = DIRECTION ( 'NONE',  ( -1.000000000000000000, 0.000000000000000000, 0.000000000000000000 ) ) ;
#15491 = EDGE_CURVE ( 'NONE', #121, #48001, #46966, .T. ) ;
#15490 = CARTESIAN_POINT ( 'NONE',  ( 46.96102914747190482, 22.94339939543869988, -75.61154402005681163 ) ) ;
#15492 = AXIS2_PLACEMENT_3D ( 'NONE', #39728, #48108, #151 ) ;
#15493 = CARTESIAN_POINT ( 'NONE',  ( 16.13393739769620083, -15.61618894467929941, 17.35000000000000142 ) ) ;
#15494 = CARTESIAN_POINT ( 'NONE',  ( 16.13393739769620083, -15.61618894467929941, -54.64999999999999858 ) ) ;
#15495 = CARTESIAN_POINT ( 'NONE',  ( 11.74347662707550022, 33.65273995683249808, -16.31133514116600125 ) ) ;
#15496 = CIRCLE ( 'NONE', #15611, 7.910999999999997812 ) ;
#15497 = CARTESIAN_POINT ( 'NONE',  ( 8.010480352932539461, -17.02763017648989674, -74.45290918797269342 ) ) ;
#15498 = CARTESIAN_POINT ( 'NONE',  ( 53.25888871246099399, -49.10877824327850050, -26.73652702851729757 ) ) ;
#15499 = CARTESIAN_POINT ( 'NONE',  ( 55.87190314012450187, -50.61618894623149600, -76.15909243498199999 ) ) ;
#15500 = B_SPLINE_CURVE_WITH_KNOTS ( 'NONE', 3,
 ( #1512, #36894, #9390, #1767 ),
 .UNSPECIFIED., .F., .F.,
 ( 4, 4 ),
 ( 0.000000000000000000, 19.53260001849420036 ),
 .UNSPECIFIED. ) ;
#15502 = CARTESIAN_POINT ( 'NONE',  ( 10.90462376991689197, -55.27285976101147469, -44.90618179855681547 ) ) ;
#15501 = CARTESIAN_POINT ( 'NONE',  ( -0.7705598404263119816, 21.64162338028269872, -8.889730355579660070 ) ) ;
#15503 = CARTESIAN_POINT ( 'NONE',  ( 63.18512348867459849, 1.274277262446069869, -68.71132524057000523 ) ) ;
#15504 = FACE_OUTER_BOUND ( 'NONE', #28728, .T. ) ;
#15505 = EDGE_LOOP ( 'NONE', ( #10635, #37882, #5376, #15903 ) ) ;
#15506 = CARTESIAN_POINT ( 'NONE',  ( 52.81743982411089888, -49.66737340927319622, -48.47378032971909789 ) ) ;
#15507 = CARTESIAN_POINT ( 'NONE',  ( 47.64197321496929760, 23.30135080481779752, -55.08764324752890218 ) ) ;
#15508 = CARTESIAN_POINT ( 'NONE',  ( 58.56772413253199971, -45.48424304623870285, -26.36790636083469863 ) ) ;
#15509 = CARTESIAN_POINT ( 'NONE',  ( 9.978830895481387131, -20.62644581997769322, -66.57488575740745773 ) ) ;
#15510 = CARTESIAN_POINT ( 'NONE',  ( 61.54546893286627096, -45.33071755016126758, -47.27434214225175424 ) ) ;
#15511 = CARTESIAN_POINT ( 'NONE',  ( 22.68119848469680377, -12.06090188681830000, -74.07430842319459430 ) ) ;
#15512 = CARTESIAN_POINT ( 'NONE',  ( 51.94901983112990251, 18.29135666841079910, -77.02691475221409689 ) ) ;
#15513 = CARTESIAN_POINT ( 'NONE',  ( 53.00383623833999991, 18.33733721602849798, -48.79311473309799396 ) ) ;
#15514 = CARTESIAN_POINT ( 'NONE',  ( 17.16952425154805084, -23.52718332138170254, -70.25066653995565957 ) ) ;
#15515 = CARTESIAN_POINT ( 'NONE',  ( 53.13663702127480093, -49.50013705438340139, -48.80285956223989530 ) ) ;
#15516 = CARTESIAN_POINT ( 'NONE',  ( 50.10204865863599366, 22.25438125613730023, -54.90071668138480732 ) ) ;
#15517 = EDGE_CURVE ( 'NONE', #44163, #14960, #19892, .T. ) ;
#15518 = CARTESIAN_POINT ( 'NONE',  ( 21.73319121277129540, -21.20477496534300244, -61.75735875115385909 ) ) ;
#15519 = CARTESIAN_POINT ( 'NONE',  ( 53.36049947297766494, -49.20080844630853534, -27.35403009910411498 ) ) ;
#15520 = AXIS2_PLACEMENT_3D ( 'NONE', #79, #47018, #19467 ) ;
#15521 = CARTESIAN_POINT ( 'NONE',  ( 11.63245656709279707, 20.65389878998962203, -69.46507341771521737 ) ) ;
#15522 = CARTESIAN_POINT ( 'NONE',  ( 64.49515523001039696, -31.53426064655560168, -17.03999220943040172 ) ) ;
#15523 = CARTESIAN_POINT ( 'NONE',  ( 71.15378634064809660, 1.278021359705819870, -60.68135466038360448 ) ) ;
#15524 = CARTESIAN_POINT ( 'NONE',  ( 11.13393739769619906, 32.19619796063980033, -43.75331349279139914 ) ) ;
#15525 = CARTESIAN_POINT ( 'NONE',  ( 72.57226300143969411, 1.394112346784049938, -61.91536134543299852 ) ) ;
#15526 = DIRECTION ( 'NONE',  ( 0.000000000000000000, -1.000000000000000000, 0.000000000000000000 ) ) ;
#15527 = CARTESIAN_POINT ( 'NONE',  ( 61.28610861988966718, -45.23040055124666736, -28.05484073064822326 ) ) ;
#15528 = ORIENTED_EDGE ( 'NONE', *, *, #12073, .T. ) ;
#15529 = ORIENTED_EDGE ( 'NONE', *, *, #34538, .F. ) ;
#15530 = DIRECTION ( 'NONE',  ( 0.000000000000000000, 0.000000000000000000, -1.000000000000000000 ) ) ;
#15531 = CARTESIAN_POINT ( 'NONE',  ( 55.55365133010059964, -45.11618894467940066, -14.32025150907159983 ) ) ;
#15532 = ORIENTED_EDGE ( 'NONE', *, *, #2345, .T. ) ;
#15533 = CARTESIAN_POINT ( 'NONE',  ( 12.17133881455110078, -65.27733590913939565, -46.10644673425740336 ) ) ;
#15534 = DIRECTION ( 'NONE',  ( 0.3294064756440925335, -0.9441882088883222224, -3.330669073875471100E-16 ) ) ;
#15535 = PLANE ( 'NONE',  #51261 ) ;
#15536 = DIRECTION ( 'NONE',  ( 0.000000000000000000, -1.000000000000000000, 0.000000000000000000 ) ) ;
#15537 = ORIENTED_EDGE ( 'NONE', *, *, #41065, .T. ) ;
#15538 = CARTESIAN_POINT ( 'NONE',  ( 22.17097752751971029, -18.77408084603302996, -80.60639082325192817 ) ) ;
#15539 = CARTESIAN_POINT ( 'NONE',  ( 44.88993838878230491, 6.796999361193691414, -65.86996340926405935 ) ) ;
#15540 = CARTESIAN_POINT ( 'NONE',  ( 11.60842185034129947, 33.48988549690440664, -24.06199962910709900 ) ) ;
#15541 = EDGE_LOOP ( 'NONE', ( #8747, #11454 ) ) ;
#15542 = CARTESIAN_POINT ( 'NONE',  ( 23.66514557999009938, -18.97232114870620023, -35.92577143160979602 ) ) ;
#15543 = FACE_OUTER_BOUND ( 'NONE', #14435, .T. ) ;
#15544 = CARTESIAN_POINT ( 'NONE',  ( 71.33393739769628894, 10.88381105532070059, -62.44999999999999574 ) ) ;
#15545 = SHAPE_REPRESENTATION_RELATIONSHIP ( 'NONE' , 'NONE' ,  #50919, #2932 ) ;
#15546 = CARTESIAN_POINT ( 'NONE',  ( 64.11006012897030359, -29.74545742325380360, -16.36070032634080107 ) ) ;
#15547 = CARTESIAN_POINT ( 'NONE',  ( 9.366946845712353920, -14.73032155540524535, -63.49448697528727337 ) ) ;
#15548 = CARTESIAN_POINT ( 'NONE',  ( 47.11430437939870330, -54.02739288645709337, -75.65564156953989539 ) ) ;
#15549 = CARTESIAN_POINT ( 'NONE',  ( 22.51775971307619884, -20.18056844656550197, -70.21007469161699532 ) ) ;
#15550 = FACE_OUTER_BOUND ( 'NONE', #35122, .T. ) ;
#15551 = AXIS2_PLACEMENT_3D ( 'NONE', #43216, #34811, #11243 ) ;
#15552 = CARTESIAN_POINT ( 'NONE',  ( 42.05083776483330382, 14.02818861621179991, -6.331737915367179781 ) ) ;
#15553 = CIRCLE ( 'NONE', #33932, 49.07571608970680188 ) ;
#15554 = ADVANCED_FACE ( 'NONE', ( #24577 ), #45641, .T. ) ;
#15555 = CARTESIAN_POINT ( 'NONE',  ( 15.05440318628110141, 21.88381105532300097, -76.14999999999999147 ) ) ;
#15556 = ADVANCED_FACE ( 'NONE', ( #29842 ), #51073, .F. ) ;
#15557 = EDGE_CURVE ( 'NONE', #4775, #51752, #45862, .T. ) ;
#15558 = CARTESIAN_POINT ( 'NONE',  ( 84.42287661217571326, -43.28755984482599928, -47.36827274406740429 ) ) ;
#15559 = CARTESIAN_POINT ( 'NONE',  ( 16.13393739769620083, -15.61618894467929941, -19.14999999999999858 ) ) ;
#15560 = EDGE_CURVE ( 'NONE', #33030, #1308, #10731, .T. ) ;
#15561 = CARTESIAN_POINT ( 'NONE',  ( 11.65838256785770000, -8.691441319380301067, -44.82502897017919707 ) ) ;
#15562 = ORIENTED_EDGE ( 'NONE', *, *, #1431, .F. ) ;
#15563 = FACE_OUTER_BOUND ( 'NONE', #30804, .T. ) ;
#15564 = CARTESIAN_POINT ( 'NONE',  ( 14.18385191392540001, -50.83394888710610360, -21.44137102719459875 ) ) ;
#15565 = CARTESIAN_POINT ( 'NONE',  ( 75.68173550483029999, -14.05264239439859963, -11.58966857824820096 ) ) ;
#15566 = LINE ( 'NONE', #23390, #37185 ) ;
#15567 = CARTESIAN_POINT ( 'NONE',  ( 18.13393739769620083, -37.52509124488599923, -54.64999999999999858 ) ) ;
#15568 = FACE_OUTER_BOUND ( 'NONE', #9404, .T. ) ;
#15569 = CARTESIAN_POINT ( 'NONE',  ( 47.18324198357279897, 23.57489020266570279, -54.61058319554400242 ) ) ;
#15570 = CARTESIAN_POINT ( 'NONE',  ( 9.543106074036904474, -17.38758878367239546, -49.36948704940078869 ) ) ;
#15571 = CARTESIAN_POINT ( 'NONE',  ( 82.30072302861961475, -45.28580905185120287, -47.18357684934780139 ) ) ;
#15572 = CARTESIAN_POINT ( 'NONE',  ( 57.36123080243149985, -50.13537922777889833, -52.61896049783310048 ) ) ;
#15573 = CARTESIAN_POINT ( 'NONE',  ( 42.28714465471179551, 13.04424985412589955, -5.063832622360679991 ) ) ;
#15574 = CARTESIAN_POINT ( 'NONE',  ( -21.36606260230379917, 31.88381105532059934, 11.84999999999999964 ) ) ;
#15575 = CARTESIAN_POINT ( 'NONE',  ( 63.55130486076469509, 0.9860880133283429494, -61.77606584740410511 ) ) ;
#15576 = CARTESIAN_POINT ( 'NONE',  ( 53.41693480158270546, -49.35328119387190071, -48.75416851881880120 ) ) ;
#15577 = VECTOR ( 'NONE', #49166, 1000.000000000000000 ) ;
#15578 = CARTESIAN_POINT ( 'NONE',  ( 68.13393739769841773, -50.61618894467878960, -73.25000000000220268 ) ) ;
#15579 = CARTESIAN_POINT ( 'NONE',  ( 67.33936456850589991, -1.038934691447770176, -17.45360882802740221 ) ) ;
#15580 = CARTESIAN_POINT ( 'NONE',  ( 18.23140400112239945, -51.35642126253560491, -74.98719232986280758 ) ) ;
#15582 = EDGE_CURVE ( 'NONE', #27219, #29806, #11772, .T. ) ;
#15581 = CARTESIAN_POINT ( 'NONE',  ( 41.56669578563739975, -43.85542471345180360, -4.650716833944319895 ) ) ;
#15583 = CARTESIAN_POINT ( 'NONE',  ( 21.05717860469869862, -21.20800352994709925, -61.33755441249169849 ) ) ;
#15584 = CARTESIAN_POINT ( 'NONE',  ( 23.83903669993742369, -13.54550867393122360, -77.70899529891561031 ) ) ;
#15585 = CARTESIAN_POINT ( 'NONE',  ( 49.39082779805520573, -53.49490451538980551, -54.14527087032600150 ) ) ;
#15586 = ORIENTED_EDGE ( 'NONE', *, *, #22963, .F. ) ;
#15587 = DIRECTION ( 'NONE',  ( -1.224646799147353207E-16, 1.000000000000000000, 0.000000000000000000 ) ) ;
#15588 = CARTESIAN_POINT ( 'NONE',  ( 10.86459002806530272, -19.89652023075066722, -35.23569143810544091 ) ) ;
#15589 = CARTESIAN_POINT ( 'NONE',  ( 72.81780655506248934, 1.383161449028130097, -68.67155289007729380 ) ) ;
#15590 = CYLINDRICAL_SURFACE ( 'NONE', #34032, 6.766999999999998572 ) ;
#15591 = VECTOR ( 'NONE', #23015, 1000.000000000000000 ) ;
#15592 = CARTESIAN_POINT ( 'NONE',  ( 11.09570125422289877, -9.916272040889650086, -81.23899999999999011 ) ) ;
#15593 = ORIENTED_EDGE ( 'NONE', *, *, #42495, .F. ) ;
#15594 = CARTESIAN_POINT ( 'NONE',  ( 18.22113377645400334, 20.91311638024189890, -75.69337827730609547 ) ) ;
#15595 = AXIS2_PLACEMENT_3D ( 'NONE', #11873, #7677, #47513 ) ;
#15596 = VERTEX_POINT ( 'NONE', #51593 ) ;
#15597 = ORIENTED_EDGE ( 'NONE', *, *, #34452, .F. ) ;
#15598 = CARTESIAN_POINT ( 'NONE',  ( 56.75109370957449784, -45.11618894467940066, -15.55230934101460072 ) ) ;
#15599 = CARTESIAN_POINT ( 'NONE',  ( 23.55432945165479808, -14.23915780199780023, -81.23899999999999011 ) ) ;
#15600 = CARTESIAN_POINT ( 'NONE',  ( 61.70952355081560370, 13.92643276180479894, -46.78415134525790364 ) ) ;
#15601 = EDGE_CURVE ( 'NONE', #44049, #41820, #40221, .T. ) ;
#15602 = ORIENTED_EDGE ( 'NONE', *, *, #13673, .F. ) ;
#15603 = CARTESIAN_POINT ( 'NONE',  ( 22.52288591994712164, -13.38583005777697466, -80.34591106198659816 ) ) ;
#15604 = VERTEX_POINT ( 'NONE', #19866 ) ;
#15605 = CARTESIAN_POINT ( 'NONE',  ( 12.14985691594747941, -8.703636955929068719, -63.12566558101337222 ) ) ;
#15606 = CARTESIAN_POINT ( 'NONE',  ( 54.17308944977700236, 19.38381105532069881, -77.01198594365929750 ) ) ;
#15607 = ORIENTED_EDGE ( 'NONE', *, *, #44250, .F. ) ;
#15608 = CARTESIAN_POINT ( 'NONE',  ( 72.78346131865960444, 1.386342629514219826, -62.63353618948930546 ) ) ;
#15609 = CARTESIAN_POINT ( 'NONE',  ( 52.31626067747389897, -50.93885350010000224, -76.18456440015900455 ) ) ;
#15610 = CARTESIAN_POINT ( 'NONE',  ( 60.53374381014149463, 14.50344111463789787, -47.62958190853139939 ) ) ;
#15611 = AXIS2_PLACEMENT_3D ( 'NONE', #29215, #49423, #22124 ) ;
#15612 = CARTESIAN_POINT ( 'NONE',  ( 13.16593781093261128, -9.467269466126328581, -39.80947853294870242 ) ) ;
#15613 = DIRECTION ( 'NONE',  ( -1.000000000000000000, 9.391392475159538137E-33, -1.071169953407190059E-15 ) ) ;
#15614 = CARTESIAN_POINT ( 'NONE',  ( -4.949082834145499987, 16.40845028330949873, -5.527623173694479419 ) ) ;
#15615 = CARTESIAN_POINT ( 'NONE',  ( 41.13393739769620083, -15.61618894467929941, -84.65000000000000568 ) ) ;
#15616 = VECTOR ( 'NONE', #5197, 1000.000000000000000 ) ;
#15617 = DIRECTION ( 'NONE',  ( 1.000000000000000000, 0.000000000000000000, 0.000000000000000000 ) ) ;
#15618 = EDGE_CURVE ( 'NONE', #48970, #32793, #43246, .T. ) ;
#15619 = CARTESIAN_POINT ( 'NONE',  ( 9.787898087487839405, -10.99942240775409985, -56.48770572707109494 ) ) ;
#15620 = EDGE_LOOP ( 'NONE', ( #3998, #10198, #14051, #39964 ) ) ;
#15621 = TOROIDAL_SURFACE ( 'NONE', #50790, 16.49999999930319916, 0.5000000000336690675 ) ;
#15622 = DIRECTION ( 'NONE',  ( -1.000000000000000000, 0.000000000000000000, 0.000000000000000000 ) ) ;
#15623 = DIRECTION ( 'NONE',  ( -0.8090169943749474513, -0.5877852522924732481, 0.000000000000000000 ) ) ;
#15624 = CARTESIAN_POINT ( 'NONE',  ( 71.61742398551369604, 1.231980527806860071, -70.40894576833619567 ) ) ;
#15625 = CARTESIAN_POINT ( 'NONE',  ( 43.65187991923512101, -39.92530307977908421, -68.34537732784100683 ) ) ;
#15626 = CARTESIAN_POINT ( 'NONE',  ( 0.3209249304026170480, -10.53407907283069989, -34.64999999999999858 ) ) ;
#15627 = DIRECTION ( 'NONE',  ( 0.000000000000000000, 0.000000000000000000, 1.000000000000000000 ) ) ;
#15628 = CARTESIAN_POINT ( 'NONE',  ( 12.98727014170039951, 18.78214033880969680, -21.05372677356080047 ) ) ;
#15629 = CARTESIAN_POINT ( 'NONE',  ( 63.46279604660929863, 1.371509258145880095, -68.88889814452589633 ) ) ;
#15630 = CARTESIAN_POINT ( 'NONE',  ( 48.29783768768939467, -54.14418088742089452, -54.68165175005749745 ) ) ;
#15631 = DIRECTION ( 'NONE',  ( 0.000000000000000000, -1.000000000000000000, 0.000000000000000000 ) ) ;
#15632 = CARTESIAN_POINT ( 'NONE',  ( 64.19260248505071331, 1.000485720979659821, -70.17481423849019961 ) ) ;
#15633 = CARTESIAN_POINT ( 'NONE',  ( 47.73411684492059948, 23.25915219497479924, -55.05916737018710450 ) ) ;
#15634 = ORIENTED_EDGE ( 'NONE', *, *, #5975, .T. ) ;
#15635 = CARTESIAN_POINT ( 'NONE',  ( 11.69292874863820053, -9.634204615267030647, -38.36406440404199714 ) ) ;
#15636 = CARTESIAN_POINT ( 'NONE',  ( 14.36264681009404498, -22.20705100211725735, -77.03616734294827495 ) ) ;
#15637 = ORIENTED_EDGE ( 'NONE', *, *, #6403, .F. ) ;
#15638 = CARTESIAN_POINT ( 'NONE',  ( 71.56838563924230812, 1.003508719580009867, -70.56164792957919474 ) ) ;
#15639 = CARTESIAN_POINT ( 'NONE',  ( 60.67119852934060020, -45.61627437969990240, -47.47040929001600063 ) ) ;
#15640 = CARTESIAN_POINT ( 'NONE',  ( 48.08635818190295197, -54.25091888102404880, -54.70531615945150605 ) ) ;
#15641 = CARTESIAN_POINT ( 'NONE',  ( 51.67587649748470113, -33.96749857170579645, -77.01363636363508647 ) ) ;
#15643 = CARTESIAN_POINT ( 'NONE',  ( 17.81845769390660195, -8.767470046512547910, -58.42394785367769572 ) ) ;
#15642 = CARTESIAN_POINT ( 'NONE',  ( 16.13393740133140142, -15.61618822260889949, -4.296537984153929735 ) ) ;
#15644 = CARTESIAN_POINT ( 'NONE',  ( 30.20787008543632268, 4.384392329102540842, -84.60813810823577796 ) ) ;
#15645 = CARTESIAN_POINT ( 'NONE',  ( 18.20469318812960324, -7.911110394061046769, -67.09100018836774382 ) ) ;
#15646 = ORIENTED_EDGE ( 'NONE', *, *, #9818, .T. ) ;
#15647 = CARTESIAN_POINT ( 'NONE',  ( 0.08561865832223169992, 19.91752656751279815, -35.04144726298140000 ) ) ;
#15648 = ORIENTED_EDGE ( 'NONE', *, *, #8148, .F. ) ;
#15649 = ORIENTED_EDGE ( 'NONE', *, *, #22435, .T. ) ;
#15650 = DIRECTION ( 'NONE',  ( 0.000000000000000000, 0.000000000000000000, 1.000000000000000000 ) ) ;
#15651 = CARTESIAN_POINT ( 'NONE',  ( 68.13393739769618662, -2.032350560841069687, -65.65000000000000568 ) ) ;
#15652 = DIRECTION ( 'NONE',  ( 0.000000000000000000, 0.000000000000000000, -1.000000000000000000 ) ) ;
#15653 = CARTESIAN_POINT ( 'NONE',  ( 12.78992083550290104, -65.50145383207738803, -47.67074661757159504 ) ) ;
#15654 = AXIS2_PLACEMENT_3D ( 'NONE', #22770, #34571, #2881 ) ;
#15655 = ORIENTED_EDGE ( 'NONE', *, *, #41294, .F. ) ;
#15656 = ADVANCED_FACE ( 'NONE', ( #23522 ), #23781, .F. ) ;
#15657 = CARTESIAN_POINT ( 'NONE',  ( 40.79482532997379707, -39.62505393422780031, -82.14319696191608955 ) ) ;
#15658 = LINE ( 'NONE', #24001, #15351 ) ;
#15659 = EDGE_CURVE ( 'NONE', #9581, #14446, #4227, .T. ) ;
#15660 = CARTESIAN_POINT ( 'NONE',  ( 56.47388559847290423, -50.68647850825969670, -53.28105505440640144 ) ) ;
#15661 = CARTESIAN_POINT ( 'NONE',  ( 22.85093860592767712, -14.77854013293515756, -46.41334110918311495 ) ) ;
#15662 = CARTESIAN_POINT ( 'NONE',  ( 62.85974396480249737, -0.1941458833951940077, -16.61913982835589820 ) ) ;
#15663 = CARTESIAN_POINT ( 'NONE',  ( 51.86329228654000190, -49.90667831135039734, -76.68384409933040047 ) ) ;
#15664 = ADVANCED_FACE ( 'NONE', ( #23264 ), #39282, .T. ) ;
#15665 = CARTESIAN_POINT ( 'NONE',  ( 13.92283413501615641, -52.20691909688449783, -75.61049359302393214 ) ) ;
#15666 = VERTEX_POINT ( 'NONE', #19357 ) ;
#15667 = CARTESIAN_POINT ( 'NONE',  ( 63.11679429741240455, 0.8888742037077590474, -68.94068779328429741 ) ) ;
#15668 = CARTESIAN_POINT ( 'NONE',  ( 75.47966807050509885, 12.14072485751589880, -13.40512917118210012 ) ) ;
#15669 = CARTESIAN_POINT ( 'NONE',  ( 16.13393739769620083, -15.61618894467929941, -18.58999999999999986 ) ) ;
#15670 = CARTESIAN_POINT ( 'NONE',  ( 8.313598522135590585, -14.96117179759260019, -51.03909337422119563 ) ) ;
#15671 = AXIS2_PLACEMENT_3D ( 'NONE', #15559, #11629, #27590 ) ;
#15672 = CARTESIAN_POINT ( 'NONE',  ( 13.31385794004649981, -50.34529401456639874, -21.15365131572360013 ) ) ;
#15673 = CARTESIAN_POINT ( 'NONE',  ( 54.92799477121080542, 19.38381105532069881, -76.61226657363050663 ) ) ;
#15674 = CARTESIAN_POINT ( 'NONE',  ( 22.90024361696743327, -15.00864283141770628, -64.81860591268294058 ) ) ;
#15675 = CARTESIAN_POINT ( 'NONE',  ( 61.28085240419530066, -45.60177449860450594, -47.67834116410560341 ) ) ;
#15676 = CARTESIAN_POINT ( 'NONE',  ( 61.25735456197249817, -45.31055611515090220, -47.12428047004050313 ) ) ;
#15677 = CARTESIAN_POINT ( 'NONE',  ( -7.616062602303800055, -62.11618894467930119, 16.35000000000000142 ) ) ;
#15678 = CARTESIAN_POINT ( 'NONE',  ( 19.36900924991789807, -21.88331502330690270, -53.19549840347880121 ) ) ;
#15679 = CARTESIAN_POINT ( 'NONE',  ( 47.13393649688870113, -39.28050833195659663, -53.76790015415899404 ) ) ;
#15680 = EDGE_CURVE ( 'NONE', #34403, #31549, #20823, .T. ) ;
#15681 = ORIENTED_EDGE ( 'NONE', *, *, #40504, .T. ) ;
#15682 = CARTESIAN_POINT ( 'NONE',  ( 47.38034241041940220, 22.97049268725260163, -75.36289877400470516 ) ) ;
#15683 = CARTESIAN_POINT ( 'NONE',  ( 64.85231939490250852, 0.9948723650351710690, -60.63592931576840073 ) ) ;
#15684 = CARTESIAN_POINT ( 'NONE',  ( 43.05757823653970462, -45.97758008170070099, -7.621845463222870265 ) ) ;
#15685 = FACE_OUTER_BOUND ( 'NONE', #25251, .T. ) ;
#15686 = CARTESIAN_POINT ( 'NONE',  ( 8.897806153503669435, -49.24610395064770074, -34.65445009297679491 ) ) ;
#15687 = CIRCLE ( 'NONE', #37457, 2.576499999999998902 ) ;
#15688 = CARTESIAN_POINT ( 'NONE',  ( 16.13393739769620083, -15.61618894467939889, -15.76422791930239953 ) ) ;
#15689 = CARTESIAN_POINT ( 'NONE',  ( 11.75081654934500008, 34.19154675346119632, -18.04875625362609881 ) ) ;
#15690 = DIRECTION ( 'NONE',  ( 0.000000000000000000, -1.000000000000000000, 0.000000000000000000 ) ) ;
#15691 = CARTESIAN_POINT ( 'NONE',  ( 23.04647541986281567, -19.60029266307493501, -57.95899793902382413 ) ) ;
#15692 = DIRECTION ( 'NONE',  ( 0.000000000000000000, 0.000000000000000000, -1.000000000000000000 ) ) ;
#15693 = CARTESIAN_POINT ( 'NONE',  ( 49.13365608953889563, 22.61156095028849933, -54.78978433424439487 ) ) ;
#15694 = ORIENTED_EDGE ( 'NONE', *, *, #36784, .T. ) ;
#15695 = CARTESIAN_POINT ( 'NONE',  ( 52.91120713071100568, -49.63374342014000007, -48.91474119692630040 ) ) ;
#15696 = ORIENTED_EDGE ( 'NONE', *, *, #14670, .F. ) ;
#15697 = CARTESIAN_POINT ( 'NONE',  ( 44.82719368195827769, 6.561635999693602450, -66.13899901678205140 ) ) ;
#15698 = CARTESIAN_POINT ( 'NONE',  ( 19.54197266774264818, -21.52907415010898973, -74.78615355739535175 ) ) ;
#15699 = DIRECTION ( 'NONE',  ( 1.000000000000000000, 0.000000000000000000, 0.000000000000000000 ) ) ;
#15700 = CARTESIAN_POINT ( 'NONE',  ( 84.12560615065849845, 12.73461698676060116, -46.88422054015599372 ) ) ;
#15701 = CARTESIAN_POINT ( 'NONE',  ( 9.173233944167900944, -16.75248385739550017, -59.40131228588499823 ) ) ;
#15702 = CARTESIAN_POINT ( 'NONE',  ( 52.84698447334999827, 18.45389268692349916, -48.96050381634810122 ) ) ;
#15703 = CARTESIAN_POINT ( 'NONE',  ( 56.67833308803319881, -45.12936355862790094, -15.96402177979890169 ) ) ;
#15704 = CARTESIAN_POINT ( 'NONE',  ( 55.05148602120549839, 15.77693620304509992, -25.60753014925489879 ) ) ;
#15705 = ORIENTED_EDGE ( 'NONE', *, *, #46958, .T. ) ;
#15706 = CARTESIAN_POINT ( 'NONE',  ( 8.426038367632161297, -14.14138701712409940, -46.34768255092779299 ) ) ;
#15707 = VERTEX_POINT ( 'NONE', #19614 ) ;
#15708 = CARTESIAN_POINT ( 'NONE',  ( 11.24176308004020086, -65.23165686211650893, -17.63707663737670117 ) ) ;
#15709 = CARTESIAN_POINT ( 'NONE',  ( 10.74482708285359855, 32.66128207971850372, -45.52152800640289598 ) ) ;
#15710 = CARTESIAN_POINT ( 'NONE',  ( 73.03159560797669769, 0.9395704634982890990, -62.18392983749130565 ) ) ;
#15711 =( BOUNDED_CURVE ( )  B_SPLINE_CURVE ( 3, ( #31791, #28120, #47807, #16083 ),
 .UNSPECIFIED., .F., .T. ) 
 B_SPLINE_CURVE_WITH_KNOTS ( ( 4, 4 ),
 ( 1.570796326794896558, 2.356194490192344837 ),
 .UNSPECIFIED. ) 
 CURVE ( )  GEOMETRIC_REPRESENTATION_ITEM ( )  RATIONAL_B_SPLINE_CURVE ( ( 1.000000000000000000, 0.9492530216741911220, 0.9492530216741911220, 1.000000000000000000 ) ) 
 REPRESENTATION_ITEM ( '' )  );
#15712 = CARTESIAN_POINT ( 'NONE',  ( 50.81914176117260240, -52.16949926219270139, -52.52140270191939919 ) ) ;
#15713 = CARTESIAN_POINT ( 'NONE',  ( 8.808908491334550561, 32.01182072428549930, -46.67060441505820023 ) ) ;
#15714 = CARTESIAN_POINT ( 'NONE',  ( 23.06214062797170072, -3.616188944679339823, -32.14999999999999858 ) ) ;
#15715 = ORIENTED_EDGE ( 'NONE', *, *, #44786, .F. ) ;
#15716 = CARTESIAN_POINT ( 'NONE',  ( 64.72587551647490045, 1.099344084866029858, -70.54350063839000029 ) ) ;
#15717 = CARTESIAN_POINT ( 'NONE',  ( 11.13393739769619906, -63.13870896646790953, -43.91241718390689641 ) ) ;
#15718 = EDGE_CURVE ( 'NONE', #3924, #9734, #5732, .T. ) ;
#15719 = CYLINDRICAL_SURFACE ( 'NONE', #38636, 6.766999999999998572 ) ;
#15720 = ORIENTED_EDGE ( 'NONE', *, *, #16495, .F. ) ;
#15721 = CARTESIAN_POINT ( 'NONE',  ( 23.53669455186071602, -48.92556967366427756, -34.79644561402096770 ) ) ;
#15722 = CARTESIAN_POINT ( 'NONE',  ( 56.84186848070030607, 19.14734183112060251, -52.83665659353640365 ) ) ;
#15723 = ADVANCED_FACE ( 'NONE', ( #29206 ), #50764, .F. ) ;
#15724 = CARTESIAN_POINT ( 'NONE',  ( 60.70500520956167634, -60.18725675654477669, 17.35000000000000142 ) ) ;
#15725 = ORIENTED_EDGE ( 'NONE', *, *, #29492, .F. ) ;
#15726 = CARTESIAN_POINT ( 'NONE',  ( 19.40270147970570136, 17.88381105532069881, -34.64999999999999858 ) ) ;
#15727 = CARTESIAN_POINT ( 'NONE',  ( 53.62552786343490396, 20.09834016026489678, -75.58099297212140755 ) ) ;
#15728 = CARTESIAN_POINT ( 'NONE',  ( 82.78853260230212641, -45.02051515586381925, -46.36933949548377853 ) ) ;
#15729 = VECTOR ( 'NONE', #46169, 1000.000000000000000 ) ;
#15730 = CARTESIAN_POINT ( 'NONE',  ( 50.95939078474921047, 17.38381105532069881, -76.37902184192927280 ) ) ;
#15731 = CARTESIAN_POINT ( 'NONE',  ( 11.42407264781889964, -22.38375084641400292, -76.48586413618279778 ) ) ;
#15732 = DIRECTION ( 'NONE',  ( 1.000000000000000000, 0.000000000000000000, 0.000000000000000000 ) ) ;
#15733 = CARTESIAN_POINT ( 'NONE',  ( 65.03603135424580728, -1.463538230407920082, -19.52361391316370032 ) ) ;
#15734 = VECTOR ( 'NONE', #20769, 1000.000000000000000 ) ;
#15735 =( NAMED_UNIT ( * ) PLANE_ANGLE_UNIT ( ) SI_UNIT ( $, .RADIAN. ) );
#15736 = ORIENTED_EDGE ( 'NONE', *, *, #43362, .T. ) ;
#15737 = VERTEX_POINT ( 'NONE', #21859 ) ;
#15738 = CARTESIAN_POINT ( 'NONE',  ( 12.66219100592389957, -9.024249109064799157, -67.57835607597777994 ) ) ;
#15739 = CARTESIAN_POINT ( 'NONE',  ( 16.13393739769620083, -15.61618894467929941, 14.34999999999999964 ) ) ;
#15740 = DIRECTION ( 'NONE',  ( 0.000000000000000000, 0.000000000000000000, -1.000000000000000000 ) ) ;
#15741 = EDGE_CURVE ( 'NONE', #51345, #25615, #14016, .T. ) ;
#15742 = CARTESIAN_POINT ( 'NONE',  ( 47.02179957962620449, 23.06926496360710033, -75.47109446400469324 ) ) ;
#15743 = EDGE_CURVE ( 'NONE', #18887, #8568, #2223, .T. ) ;
#15744 = CARTESIAN_POINT ( 'NONE',  ( 16.13393739769620083, -15.61618894467929941, -5.966499999999999915 ) ) ;
#15745 = DIRECTION ( 'NONE',  ( 0.8090169943749462300, -0.5877852522924749135, 0.000000000000000000 ) ) ;
#15746 = CARTESIAN_POINT ( 'NONE',  ( 11.79921494304880092, 33.80856205050040586, -16.52202905012969936 ) ) ;
#15747 = CARTESIAN_POINT ( 'NONE',  ( 21.93114081399549775, -21.47922171441739891, -71.75946553180968124 ) ) ;
#15748 = CARTESIAN_POINT ( 'NONE',  ( 19.73427364139330109, -22.64788242709790111, -32.14999999999999858 ) ) ;
#15749 = CARTESIAN_POINT ( 'NONE',  ( 57.01957019932739712, -50.62831541463020102, -74.14894682937750758 ) ) ;
#15751 = CARTESIAN_POINT ( 'NONE',  ( 46.63393739769619373, -15.61618894467929941, -35.14999999999999858 ) ) ;
#15750 = CARTESIAN_POINT ( 'NONE',  ( -11.22445290707359966, 10.55079285699060243, -5.475728648851799996 ) ) ;
#15752 = CARTESIAN_POINT ( 'NONE',  ( 63.16529205807979963, 1.278021359705819870, -68.66984894295178776 ) ) ;
#15753 = B_SPLINE_CURVE_WITH_KNOTS ( 'NONE', 3,
 ( #26661, #39258, #39772, #38753, #43703, #15668 ),
 .UNSPECIFIED., .F., .F.,
 ( 4, 2, 4 ),
 ( 0.000000000000000000, 0.5000000000000000000, 1.000000000000000000 ),
 .UNSPECIFIED. ) ;
#15754 = CARTESIAN_POINT ( 'NONE',  ( 61.30530709542880174, 13.98952859230019996, -46.58604879334039595 ) ) ;
#15755 = CARTESIAN_POINT ( 'NONE',  ( 57.50723796702470025, -45.11618894467940066, -17.93019253464870033 ) ) ;
#15756 = ORIENTED_EDGE ( 'NONE', *, *, #44254, .F. ) ;
#15757 = CARTESIAN_POINT ( 'NONE',  ( 53.41693480158970431, -49.35328119386819878, -48.75416851881659852 ) ) ;
#15758 = VECTOR ( 'NONE', #19590, 1000.000000000000000 ) ;
#15759 = CARTESIAN_POINT ( 'NONE',  ( 59.02328509747849949, -45.43582055027459887, -26.47283546404650068 ) ) ;
#15760 = CARTESIAN_POINT ( 'NONE',  ( 12.37461265888050654, -22.60375392215577151, -66.44936340057275004 ) ) ;
#15761 = CARTESIAN_POINT ( 'NONE',  ( 56.50431216083380548, 15.03356263069209930, -26.27578698830990334 ) ) ;
#15762 = CARTESIAN_POINT ( 'NONE',  ( 9.476745794552989821, -12.27126835306809838, -71.38086476703149685 ) ) ;
#15763 = CARTESIAN_POINT ( 'NONE',  ( 51.30775034956080560, 17.47491416869410230, -76.60305689054860068 ) ) ;
#15764 = CARTESIAN_POINT ( 'NONE',  ( 52.93241475290810172, 18.38021004741200315, -48.85493842486449978 ) ) ;
#15765 = DIRECTION ( 'NONE',  ( -1.000000000000000000, 0.000000000000000000, 0.000000000000000000 ) ) ;
#15766 = DIRECTION ( 'NONE',  ( 0.000000000000000000, 0.000000000000000000, -1.000000000000000000 ) ) ;
#15767 = VERTEX_POINT ( 'NONE', #1704 ) ;
#15768 = DIRECTION ( 'NONE',  ( -0.8545454545454611583, 0.000000000000000000, 0.5193766129849238800 ) ) ;
#15769 = CARTESIAN_POINT ( 'NONE',  ( 47.63442634882579796, -54.53229989956079748, -54.97162067429140109 ) ) ;
#15770 = CARTESIAN_POINT ( 'NONE',  ( 8.428830500064028897, -13.54553434705470139, -36.87566510236762696 ) ) ;
#15771 = DIRECTION ( 'NONE',  ( 1.000000000000000000, 0.000000000000000000, 0.000000000000000000 ) ) ;
#15772 = CARTESIAN_POINT ( 'NONE',  ( 61.55531029558209610, -30.52545227551890150, -16.28638563878910261 ) ) ;
#15773 = CARTESIAN_POINT ( 'NONE',  ( 71.44807725908989937, 0.8904513541338849869, -60.64834380034769623 ) ) ;
#15774 = CARTESIAN_POINT ( 'NONE',  ( 11.13393739769619906, 31.93056987172010608, -43.74365520157400056 ) ) ;
#15775 = CARTESIAN_POINT ( 'NONE',  ( 72.67592461730299647, 1.176186365485209828, -61.77681041909720250 ) ) ;
#15776 = CARTESIAN_POINT ( 'NONE',  ( 51.02532063986365074, -35.17600456832372657, -76.41498861430551415 ) ) ;
#15777 = LINE ( 'NONE', #47252, #16764 ) ;
#15778 = VERTEX_POINT ( 'NONE', #13513 ) ;
#15779 = ORIENTED_EDGE ( 'NONE', *, *, #48943, .F. ) ;
#15780 = CARTESIAN_POINT ( 'NONE',  ( 22.46008894638382003, -10.75449222223970658, -55.58399371059939398 ) ) ;
#15781 = ADVANCED_FACE ( 'NONE', ( #45215 ), #34165, .T. ) ;
#15782 = CARTESIAN_POINT ( 'NONE',  ( 10.72266589679370341, -19.77492157605291467, -59.24448682388644727 ) ) ;
#15783 = EDGE_LOOP ( 'NONE', ( #31228, #45303, #15195, #21476, #22292, #27479, #13109, #33815, #48449, #51799, #47167, #21055, #22609 ) ) ;
#15784 = DIRECTION ( 'NONE',  ( -1.000000000000000000, 0.000000000000000000, 0.000000000000000000 ) ) ;
#15785 = CARTESIAN_POINT ( 'NONE',  ( 1.055648624548729986, -8.645219027462792027, -34.65000333055159842 ) ) ;
#15786 = ORIENTED_EDGE ( 'NONE', *, *, #48761, .F. ) ;
#15787 = CARTESIAN_POINT ( 'NONE',  ( -0.1295185695944109927, -31.87964491196989414, -59.64999999999999147 ) ) ;
#15788 = CARTESIAN_POINT ( 'NONE',  ( 45.02469926346807938, 6.813230800168343926, -65.19619103482980904 ) ) ;
#15789 = CARTESIAN_POINT ( 'NONE',  ( 14.06333294549902924, -7.911069592903273495, -34.92433389901778895 ) ) ;
#15790 = CARTESIAN_POINT ( 'NONE',  ( 11.77815578209330027, -8.615482796503201257, -45.11516743498959414 ) ) ;
#15791 = DIRECTION ( 'NONE',  ( -1.000000000000000000, 0.000000000000000000, 0.000000000000000000 ) ) ;
#15792 = CARTESIAN_POINT ( 'NONE',  ( 24.04493240159784406, -15.62537587214817059, -49.79270004542557615 ) ) ;
#15793 = CARTESIAN_POINT ( 'NONE',  ( 59.32366520224450568, -28.27453674296199537, -15.67709929047940065 ) ) ;
#15794 = DIRECTION ( 'NONE',  ( -0.2260571801428161165, 0.000000000000000000, 0.9741140340359943917 ) ) ;
#15795 = CARTESIAN_POINT ( 'NONE',  ( 11.65470348258009992, -9.172338300440578962, -71.31913972650768585 ) ) ;
#15796 = FACE_OUTER_BOUND ( 'NONE', #27894, .T. ) ;
#15797 = AXIS2_PLACEMENT_3D ( 'NONE', #49198, #44993, #29247 ) ;
#15798 = CARTESIAN_POINT ( 'NONE',  ( 40.90034125862820247, 13.87198803079870046, -5.606156744188270480 ) ) ;
#15799 = AXIS2_PLACEMENT_3D ( 'NONE', #11276, #15465, #3930 ) ;
#15800 = EDGE_CURVE ( 'NONE', #31302, #637, #30682, .T. ) ;
#15801 = CARTESIAN_POINT ( 'NONE',  ( 14.90761372254600126, 21.75858530671060009, -76.14999999999999147 ) ) ;
#15802 = B_SPLINE_CURVE_WITH_KNOTS ( 'NONE', 3,
 ( #13716, #42009, #49874, #29670, #10031, #13969, #28897, #9528, #40960, #25997, #21033, #49108, #45680, #25218, #13208, #24949, #25732, #41740, #36759, #9781, #871, #37034, #25475, #16865, #9271, #32812, #5845, #48838, #21289, #21549, #12941 ),
 .UNSPECIFIED., .F., .F.,
 ( 4, 2, 1, 1, 1, 2, 2, 2, 2, 2, 2, 2, 2, 2, 2, 2, 4 ),
 ( 0.4999999368682983003, 0.5009764994916026115, 0.5019530621149068672, 0.5039061873615149345, 0.5078124378547310691, 0.5156249388411637824, 0.5312499408140293200, 0.5624999447597606173, 0.6249999526512233228, 0.6874999605426860283, 0.7499999684341487338, 0.8124999763256113283, 0.8749999842170741449, 0.9062499881628056642, 0.9374999921085371835, 0.9687499960542684807, 1.000000000000000000 ),
 .UNSPECIFIED. ) ;
#15803 = CARTESIAN_POINT ( 'NONE',  ( 83.13571748553259511, -44.95166435745220213, -46.75830440892689666 ) ) ;
#15804 = CARTESIAN_POINT ( 'NONE',  ( 23.04647657677116612, -11.63208738592670421, -57.62566460569046711 ) ) ;
#15805 = CARTESIAN_POINT ( 'NONE',  ( 13.00458990189400055, -23.24441973297430053, -42.13158531401599305 ) ) ;
#15806 = EDGE_LOOP ( 'NONE', ( #8227, #17628, #13542, #27157 ) ) ;
#15807 = DIRECTION ( 'NONE',  ( 1.000000000000000000, 0.000000000000000000, 0.000000000000000000 ) ) ;
#15808 = CARTESIAN_POINT ( 'NONE',  ( 13.96942586497290151, -50.35282484553089688, -20.94633231277909857 ) ) ;
#15809 = CARTESIAN_POINT ( 'NONE',  ( 22.32536594118367645, -20.56154573459575374, -39.72222021323458563 ) ) ;
#15810 = CARTESIAN_POINT ( 'NONE',  ( 22.90034296864962471, -15.71306839012465772, -56.45738126217962360 ) ) ;
#15811 = CARTESIAN_POINT ( 'NONE',  ( 56.46551567295650642, -50.77616483221130750, -74.14999999999999147 ) ) ;
#15812 = ORIENTED_EDGE ( 'NONE', *, *, #7504, .F. ) ;
#15813 = CARTESIAN_POINT ( 'NONE',  ( -9.070458372979668837, -44.11014026221840112, -5.806348201939020015 ) ) ;
#15814 = CARTESIAN_POINT ( 'NONE',  ( 11.27232597222496757, -21.94240453461146245, -38.50066575436082417 ) ) ;
#15815 = DIRECTION ( 'NONE',  ( 0.000000000000000000, 0.000000000000000000, 1.000000000000000000 ) ) ;
#15816 = CARTESIAN_POINT ( 'NONE',  ( 63.39699138880700247, 1.369885150286800135, -62.57510434557890733 ) ) ;
#15817 = CARTESIAN_POINT ( 'NONE',  ( 13.68960069945450009, 19.17906422713569725, -21.10128301701960041 ) ) ;
#15818 = CARTESIAN_POINT ( 'NONE',  ( 57.55751162050889747, -50.61165563123979894, -53.76309025934260433 ) ) ;
#15819 = CARTESIAN_POINT ( 'NONE',  ( 42.34652499213279953, 12.85456310532500090, -4.929786138809819640 ) ) ;
#15820 = CARTESIAN_POINT ( 'NONE',  ( 17.01981217550311598, -22.38317801499556481, -64.91115475112107447 ) ) ;
#15821 = CARTESIAN_POINT ( 'NONE',  ( 0.3188172270368339611, 15.01558124385560156, -34.65000333199999716 ) ) ;
#15822 = CARTESIAN_POINT ( 'NONE',  ( 54.26618122617689721, -48.93283047810160014, -48.76497828246320410 ) ) ;
#15823 = CARTESIAN_POINT ( 'NONE',  ( 68.13393739769840352, -50.61618894467879670, -73.25000000000220268 ) ) ;
#15824 = CARTESIAN_POINT ( 'NONE',  ( 10.72255721402834361, -19.77478218903828378, -63.24448401478402815 ) ) ;
#15825 = DIRECTION ( 'NONE',  ( 0.000000000000000000, 0.000000000000000000, -1.000000000000000000 ) ) ;
#15826 = PRODUCT_DEFINITION ( 'UNKNOWN', '', #900, #46835 ) ;
#15827 = CARTESIAN_POINT ( 'NONE',  ( 16.40674540481250077, -23.06147403858910039, -63.55568448227298717 ) ) ;
#15828 = CARTESIAN_POINT ( 'NONE',  ( 19.13393739769600188, 18.38381105532069881, -34.64999999999999858 ) ) ;
#15829 = CARTESIAN_POINT ( 'NONE',  ( 59.57331641441849968, -46.90860258996760024, -48.88667301442139745 ) ) ;
#15830 = ORIENTED_EDGE ( 'NONE', *, *, #19585, .F. ) ;
#15831 = CARTESIAN_POINT ( 'NONE',  ( 22.15575932996830133, -54.10246922935670000, -34.93361312117490058 ) ) ;
#15832 = CARTESIAN_POINT ( 'NONE',  ( 9.366668810525878186, -15.61604052661200015, -35.45282021618999835 ) ) ;
#15833 = CARTESIAN_POINT ( 'NONE',  ( 73.23405285996879854, 0.9209334348186318797, -68.81061689070359932 ) ) ;
#15834 = CIRCLE ( 'NONE', #31698, 3.000000000000005773 ) ;
#15835 = CARTESIAN_POINT ( 'NONE',  ( 72.86589732295999511, 1.383811055320669947, -62.77400398868049081 ) ) ;
#15836 = AXIS2_PLACEMENT_3D ( 'NONE', #25432, #44859, #41183 ) ;
#15837 = CARTESIAN_POINT ( 'NONE',  ( 9.023362915854630018, -14.22815957666089837, -81.23899999999999011 ) ) ;
#15838 = ORIENTED_EDGE ( 'NONE', *, *, #23203, .F. ) ;
#15839 = CARTESIAN_POINT ( 'NONE',  ( 17.21347160910339724, 21.88381105532300097, -76.14999999999999147 ) ) ;
#15840 = ORIENTED_EDGE ( 'NONE', *, *, #25631, .T. ) ;
#15841 = EDGE_CURVE ( 'NONE', #33091, #1308, #22613, .T. ) ;
#15842 = AXIS2_PLACEMENT_3D ( 'NONE', #51671, #3206, #27549 ) ;
#15843 = ORIENTED_EDGE ( 'NONE', *, *, #2776, .T. ) ;
#15844 = CARTESIAN_POINT ( 'NONE',  ( 56.86403571658450318, -45.97907451721239624, -26.24559329655039974 ) ) ;
#15845 = CARTESIAN_POINT ( 'NONE',  ( 21.39066400359539699, -9.703911137440838885, -81.23899999999999011 ) ) ;
#15846 = ADVANCED_FACE ( 'NONE', ( #1184 ), #44774, .T. ) ;
#15847 = CARTESIAN_POINT ( 'NONE',  ( -11.26666115314075967, -34.90345733776890569, -44.56356395724966291 ) ) ;
#15848 = EDGE_CURVE ( 'NONE', #15326, #45555, #31844, .T. ) ;
#15849 = VERTEX_POINT ( 'NONE', #38382 ) ;
#15850 = EDGE_CURVE ( 'NONE', #32096, #38625, #31000, .T. ) ;
#15851 = CARTESIAN_POINT ( 'NONE',  ( 8.223360643215830379, -15.61635149015999957, -74.50766849176298479 ) ) ;
#15852 = EDGE_LOOP ( 'NONE', ( #13450, #47881, #23755, #31661 ) ) ;
#15853 = CARTESIAN_POINT ( 'NONE',  ( 11.67620015026735203, -64.89165383396532150, -23.88711004025349283 ) ) ;
#15854 = B_SPLINE_CURVE_WITH_KNOTS ( 'NONE', 3,
 ( #44535, #17023, #502, #20929 ),
 .UNSPECIFIED., .F., .F.,
 ( 4, 4 ),
 ( 0.000000000000000000, 1.000000000000000000 ),
 .UNSPECIFIED. ) ;
#15855 = CARTESIAN_POINT ( 'NONE',  ( 16.13393739769620083, -15.61618894467929941, -1.149999999999999911 ) ) ;
#15856 = ORIENTED_EDGE ( 'NONE', *, *, #50060, .F. ) ;
#15857 = ORIENTED_EDGE ( 'NONE', *, *, #5319, .F. ) ;
#15858 = B_SPLINE_CURVE_WITH_KNOTS ( 'NONE', 3,
 ( #49639, #26011, #25746, #17395, #5092, #14237, #29685, #29940, #30207, #37048, #45955, #42021, #46224, #10312, #17141, #21046, #33092, #1145, #49124, #41495 ),
 .UNSPECIFIED., .F., .F.,
 ( 4, 2, 2, 2, 2, 2, 2, 2, 2, 4 ),
 ( -3.516439999999999908E-13, 0.4027787201731649613, 0.8630972575143259773, 1.150796343352550100, 1.294645886271670099, 1.524805154942250107, 1.789982511918259966, 2.002124397499069897, 2.214266283079879827, 2.301592686705460356 ),
 .UNSPECIFIED. ) ;
#15859 = CARTESIAN_POINT ( 'NONE',  ( 8.222546438703959737, -15.61603098320130201, -50.50766849176299900 ) ) ;
#15860 = DIRECTION ( 'NONE',  ( -0.4316160343590924597, 0.9020574254913767964, 0.000000000000000000 ) ) ;
#15861 = CARTESIAN_POINT ( 'NONE',  ( 60.58628810321520319, 14.54561104465429899, -47.73487494779390516 ) ) ;
#15862 = DIRECTION ( 'NONE',  ( 1.000000000000000000, 0.000000000000000000, 0.000000000000000000 ) ) ;
#15863 = ADVANCED_FACE ( 'NONE', ( #50693 ), #30577, .T. ) ;
#15864 = CARTESIAN_POINT ( 'NONE',  ( 11.13393739769619906, 31.88305279702909800, -43.74348518090240390 ) ) ;
#15865 = CARTESIAN_POINT ( 'NONE',  ( -8.878336496226518548, 13.03716217029489854, -5.682102490148450258 ) ) ;
#15866 = VECTOR ( 'NONE', #46309, 1000.000000000000000 ) ;
#15867 = VECTOR ( 'NONE', #26217, 1000.000000000000000 ) ;
#15868 = VECTOR ( 'NONE', #33774, 1000.000000000000000 ) ;
#15869 = CARTESIAN_POINT ( 'NONE',  ( 47.06490849475201088, 23.30732314589785048, -75.17786410262570485 ) ) ;
#15870 = CARTESIAN_POINT ( 'NONE',  ( 59.43897480784050202, 14.27109403266730148, -26.69952124243079794 ) ) ;
#15871 = AXIS2_PLACEMENT_3D ( 'NONE', #44312, #20705, #36696 ) ;
#15872 = AXIS2_PLACEMENT_3D ( 'NONE', #9778, #1908, #49872 ) ;
#15873 = CARTESIAN_POINT ( 'NONE',  ( 10.66331371621759949, -21.24282423753659899, -62.03303090152439125 ) ) ;
#15874 = ORIENTED_EDGE ( 'NONE', *, *, #51064, .T. ) ;
#15875 = CARTESIAN_POINT ( 'NONE',  ( 56.62432785517989942, -50.71560893929350300, -53.83726655417689955 ) ) ;
#15877 = CIRCLE ( 'NONE', #45174, 5.499999999999998224 ) ;
#15876 = CARTESIAN_POINT ( 'NONE',  ( 10.13393739769619906, -54.15188668067469990, -54.64999999999999858 ) ) ;
#15878 = CARTESIAN_POINT ( 'NONE',  ( 13.00893739769619906, 34.28605925116850273, -47.75434321273180416 ) ) ;
#15879 = CARTESIAN_POINT ( 'NONE',  ( 72.55770162222249553, 1.107037132887370046, -69.69638372295169404 ) ) ;
#15880 = CARTESIAN_POINT ( 'NONE',  ( 42.24293144673103484, -39.79048127957475600, -75.15823207472831768 ) ) ;
#15882 = EDGE_CURVE ( 'NONE', #31947, #8290, #31967, .T. ) ;
#15881 = DIRECTION ( 'NONE',  ( 1.000000000000000000, 0.000000000000000000, 0.000000000000000000 ) ) ;
#15883 = CARTESIAN_POINT ( 'NONE',  ( 14.27580295341549999, -22.41985674678640095, -45.43204315924410253 ) ) ;
#15884 = CARTESIAN_POINT ( 'NONE',  ( 61.48313171494003626, 14.13204535159540853, -47.33723770254623275 ) ) ;
#15885 = CARTESIAN_POINT ( 'NONE',  ( 48.69693219778879723, -54.06267158604929790, -55.01166712023250227 ) ) ;
#15886 = CARTESIAN_POINT ( 'NONE',  ( 51.88783817057427683, -32.77378372426147735, -18.83067710447933507 ) ) ;
#15887 = LINE ( 'NONE', #15375, #5114 ) ;
#15888 = CARTESIAN_POINT ( 'NONE',  ( 11.27220924270882207, -9.290061667250862243, -71.08398583345959310 ) ) ;
#15889 = ORIENTED_EDGE ( 'NONE', *, *, #7531, .F. ) ;
#15890 = CARTESIAN_POINT ( 'NONE',  ( 14.83834572504270000, -8.683358393905999506, -80.28837282723659996 ) ) ;
#15891 = CARTESIAN_POINT ( 'NONE',  ( 22.90093737956978970, -16.50199041861013782, -76.49448436988512867 ) ) ;
#15892 = EDGE_LOOP ( 'NONE', ( #10576, #22919, #21047, #14902, #47991 ) ) ;
#15893 = CARTESIAN_POINT ( 'NONE',  ( 71.42252419164299226, 1.263738073398970041, -70.48213147351589214 ) ) ;
#15894 = CARTESIAN_POINT ( 'NONE',  ( 60.76922410162809740, -45.54289718728929870, -47.36000494951569806 ) ) ;
#15895 = CARTESIAN_POINT ( 'NONE',  ( 49.30791778510987911, -53.55500811875207745, -54.21103610183089927 ) ) ;
#15896 = CARTESIAN_POINT ( 'NONE',  ( 51.13393739769620083, -15.61618894467929941, 9.349999999999999645 ) ) ;
#15898 = CARTESIAN_POINT ( 'NONE',  ( 24.04508668034977248, -15.61618904219531778, -35.79233368253564862 ) ) ;
#15897 = CARTESIAN_POINT ( 'NONE',  ( 41.30555080485065389, 8.453905220434588585, -79.68287709513984396 ) ) ;
#15899 = CARTESIAN_POINT ( 'NONE',  ( 29.58089024243311371, 4.434971018804394483, -84.61624959000400281 ) ) ;
#15900 = CARTESIAN_POINT ( 'NONE',  ( 20.99565532440523441, -9.290055542993323812, -67.21599983764021147 ) ) ;
#15901 = ORIENTED_EDGE ( 'NONE', *, *, #50427, .T. ) ;
#15902 = DIRECTION ( 'NONE',  ( -0.1961161351381840445, 0.000000000000000000, -0.9805806756909201116 ) ) ;
#15903 = ORIENTED_EDGE ( 'NONE', *, *, #14833, .T. ) ;
#15904 = ORIENTED_EDGE ( 'NONE', *, *, #5742, .T. ) ;
#15905 = DIRECTION ( 'NONE',  ( -0.2260571801428161443, -2.775557561562891351E-17, 0.9741140340359945027 ) ) ;
#15907 = CARTESIAN_POINT ( 'NONE',  ( 53.51410843436200082, -49.43305938620899553, -49.22423862607029577 ) ) ;
#15906 = AXIS2_PLACEMENT_3D ( 'NONE', #46491, #30214, #2967 ) ;
#15908 = CARTESIAN_POINT ( 'NONE',  ( 56.01715054582741260, 14.67189247168751720, -25.73175519691123014 ) ) ;
#15909 = EDGE_CURVE ( 'NONE', #10572, #2360, #902, .T. ) ;
#15910 = VECTOR ( 'NONE', #19849, 1000.000000000000000 ) ;
#15911 = CARTESIAN_POINT ( 'NONE',  ( 76.39217513833645512, -17.42905162351204851, -12.76281908793090203 ) ) ;
#15912 = CIRCLE ( 'NONE', #19272, 2.000000000000000000 ) ;
#15913 = ORIENTED_EDGE ( 'NONE', *, *, #4554, .T. ) ;
#15914 = AXIS2_PLACEMENT_3D ( 'NONE', #28643, #44644, #40716 ) ;
#15915 = EDGE_CURVE ( 'NONE', #26391, #3281, #6612, .T. ) ;
#15916 = DIRECTION ( 'NONE',  ( 0.000000000000000000, -1.000000000000000000, 0.000000000000000000 ) ) ;
#15917 = CARTESIAN_POINT ( 'NONE',  ( 57.13225691960569463, -45.15146943985669736, -25.30757468707000157 ) ) ;
#15918 = CARTESIAN_POINT ( 'NONE',  ( 14.23915348030984873, -9.102733633742271735, -45.86270462862681541 ) ) ;
#15919 = CARTESIAN_POINT ( 'NONE',  ( 60.87922264735060196, -0.7885390955128780410, -16.21936628598430019 ) ) ;
#15920 = CARTESIAN_POINT ( 'NONE',  ( 52.11524330449060471, -49.86368024659240206, -76.92610723711719345 ) ) ;
#15921 = ORIENTED_EDGE ( 'NONE', *, *, #17285, .F. ) ;
#15922 = CARTESIAN_POINT ( 'NONE',  ( 68.13393739769620083, -42.11618894467930119, -65.65000000000000568 ) ) ;
#15923 = CARTESIAN_POINT ( 'NONE',  ( 52.93656365064889968, -50.31421972478020166, -77.15175517354180101 ) ) ;
#15924 = CARTESIAN_POINT ( 'NONE',  ( 11.66468727650932102, -10.49346430533042529, -33.72439379513514979 ) ) ;
#15925 = DIRECTION ( 'NONE',  ( -1.000000000000000000, 0.000000000000000000, 0.000000000000000000 ) ) ;
#15926 = CARTESIAN_POINT ( 'NONE',  ( 9.390298412734489730, -19.62992546220089807, -54.84160206527489123 ) ) ;
#15927 = DIRECTION ( 'NONE',  ( 1.000000000000000000, 0.000000000000000000, 0.000000000000000000 ) ) ;
#15928 = DIRECTION ( 'NONE',  ( 0.000000000000000000, 0.000000000000000000, -1.000000000000000000 ) ) ;
#15929 = ADVANCED_FACE ( 'NONE', ( #30186 ), #23337, .T. ) ;
#15930 = CARTESIAN_POINT ( 'NONE',  ( 66.13393739769620083, -15.61618894467929941, -16.65000000000000213 ) ) ;
#15931 = CARTESIAN_POINT ( 'NONE',  ( 56.56302216566690078, 13.88381105532070059, -15.29297957052069989 ) ) ;
#15932 = LINE ( 'NONE', #35841, #9808 ) ;
#15933 = CARTESIAN_POINT ( 'NONE',  ( 22.72481220864853668, -17.38742840828553327, -38.53615641829414074 ) ) ;
#15934 = CARTESIAN_POINT ( 'NONE',  ( 22.89967574327219779, -17.60800816681120295, -54.93831488687830245 ) ) ;
#15935 = CARTESIAN_POINT ( 'NONE',  ( 46.47536507427530239, -40.11920440292289669, -54.64999999999999858 ) ) ;
#15936 = ORIENTED_EDGE ( 'NONE', *, *, #35104, .T. ) ;
#15937 = CARTESIAN_POINT ( 'NONE',  ( 47.48065468354979402, 23.09789384912840049, -75.12259495528830655 ) ) ;
#15938 = CARTESIAN_POINT ( 'NONE',  ( 47.21829295900949575, -54.77949880278709571, -54.61684610847309784 ) ) ;
#15939 = CARTESIAN_POINT ( 'NONE',  ( 16.13393739769620083, -45.61618894467940066, -34.64999999999999858 ) ) ;
#15940 = CARTESIAN_POINT ( 'NONE',  ( 10.72257637282393361, -11.45757118250618944, -37.66115420151670179 ) ) ;
#15941 = CARTESIAN_POINT ( 'NONE',  ( 11.75935880766958519, -64.97634148314350000, -23.85050166126463012 ) ) ;
#15942 = AXIS2_PLACEMENT_3D ( 'NONE', #12258, #48679, #24272 ) ;
#15943 = DIRECTION ( 'NONE',  ( 0.000000000000000000, 0.000000000000000000, 1.000000000000000000 ) ) ;
#15944 = AXIS2_PLACEMENT_3D ( 'NONE', #17308, #37221, #25398 ) ;
#15945 = EDGE_CURVE ( 'NONE', #35705, #33975, #34372, .T. ) ;
#15947 = AXIS2_PLACEMENT_3D ( 'NONE', #9737, #25696, #21769 ) ;
#15946 = CARTESIAN_POINT ( 'NONE',  ( -0.007164378094141890356, 19.48649803870589992, -34.77269719633950018 ) ) ;
#15949 = EDGE_CURVE ( 'NONE', #11777, #38817, #19172, .T. ) ;
#15948 = DIRECTION ( 'NONE',  ( -1.000000000000000000, -1.016537000000000039E-13, -1.878770999999999851E-12 ) ) ;
#15950 = CARTESIAN_POINT ( 'NONE',  ( 18.29760214348302227, -7.981476198048588877, -65.09563924883536856 ) ) ;
#15952 = CARTESIAN_POINT ( 'NONE',  ( 9.221482312219526634, -19.60043670736297372, -74.34100170688905962 ) ) ;
#15951 = CARTESIAN_POINT ( 'NONE',  ( 0.4394934780714839784, -8.845007899843928101, -35.02127583263639821 ) ) ;
#15953 = DIRECTION ( 'NONE',  ( 0.000000000000000000, 0.000000000000000000, 1.000000000000000000 ) ) ;
#15954 = CARTESIAN_POINT ( 'NONE',  ( 49.40264607704519761, 22.51715297631980306, -54.82400704780420142 ) ) ;
#15955 = VERTEX_POINT ( 'NONE', #50385 ) ;
#15956 = CARTESIAN_POINT ( 'NONE',  ( 53.21057599194470100, -49.49334818133160496, -49.03900858120630346 ) ) ;
#15957 = B_SPLINE_CURVE_WITH_KNOTS ( 'NONE', 3,
 ( #22800, #31429, #38822, #43267, #46692, #18880 ),
 .UNSPECIFIED., .F., .F.,
 ( 4, 1, 1, 4 ),
 ( 0.000000000000000000, 0.3333333333333329263, 0.6666666666666669627, 1.000000000000000000 ),
 .UNSPECIFIED. ) ;
#15958 = ORIENTED_EDGE ( 'NONE', *, *, #23615, .F. ) ;
#15959 = CARTESIAN_POINT ( 'NONE',  ( 44.91829444253557568, 7.853016399853718355, -66.18824355412928639 ) ) ;
#15960 = CARTESIAN_POINT ( 'NONE',  ( 14.13393739769620439, -41.61618894467939356, -35.01561944896766221 ) ) ;
#15961 = CARTESIAN_POINT ( 'NONE',  ( 84.24534987432259925, 12.60397863988419864, -47.12743895163409746 ) ) ;
#15962 = CARTESIAN_POINT ( 'NONE',  ( 11.81604877385439956, -21.19278257598529791, -51.16254345526859737 ) ) ;
#15963 = DIRECTION ( 'NONE',  ( 1.000000000000000000, 0.000000000000000000, 0.000000000000000000 ) ) ;
#15964 = CARTESIAN_POINT ( 'NONE',  ( 56.21279806897850762, -45.28513128442910585, -16.23752131442829949 ) ) ;
#15965 = CARTESIAN_POINT ( 'NONE',  ( 53.18037562183940281, 17.96329376868539995, -26.81634874583109962 ) ) ;
#15966 = ORIENTED_EDGE ( 'NONE', *, *, #14542, .T. ) ;
#15967 = CARTESIAN_POINT ( 'NONE',  ( 23.88558989793769882, -16.84037508194900212, -43.33736317051029374 ) ) ;
#15968 = VERTEX_POINT ( 'NONE', #22830 ) ;
#15969 = CARTESIAN_POINT ( 'NONE',  ( 11.41186172778549945, -65.13766231309419652, -17.00495023108739900 ) ) ;
#15970 = CARTESIAN_POINT ( 'NONE',  ( 12.92260290766840036, 34.28065277568710201, -47.72142139346610179 ) ) ;
#15971 = CARTESIAN_POINT ( 'NONE',  ( 73.02809924467999281, 1.186515949276290227, -62.33540229050490211 ) ) ;
#15972 = ADVANCED_FACE ( 'NONE', ( #31205 ), #46724, .T. ) ;
#15973 = CARTESIAN_POINT ( 'NONE',  ( 52.27072484100800409, -50.81380991892629595, -50.92202115719549482 ) ) ;
#15974 = CARTESIAN_POINT ( 'NONE',  ( 8.807322927776979782, 32.00291607516390258, -46.67042760097810117 ) ) ;
#15975 = LINE ( 'NONE', #11538, #51048 ) ;
#15976 = ORIENTED_EDGE ( 'NONE', *, *, #26461, .F. ) ;
#15977 = EDGE_CURVE ( 'NONE', #7222, #17870, #15104, .T. ) ;
#15978 = DIRECTION ( 'NONE',  ( -0.6911981449639432729, -0.7226652920947591596, 0.000000000000000000 ) ) ;
#15979 = CARTESIAN_POINT ( 'NONE',  ( 11.13393739769619906, -63.26646877388989054, -43.74576002344679893 ) ) ;
#15980 = CARTESIAN_POINT ( 'NONE',  ( 68.13393739769810509, 19.38381105532030091, -71.50000000000198952 ) ) ;
#15981 = VERTEX_POINT ( 'NONE', #10289 ) ;
#15982 = CARTESIAN_POINT ( 'NONE',  ( 68.03757080751434216, -32.00242907265933923, -18.68196741761224189 ) ) ;
#15983 = CARTESIAN_POINT ( 'NONE',  ( 56.87160281683760132, 19.05665430235150026, -52.71743055004790790 ) ) ;
#15984 = CARTESIAN_POINT ( 'NONE',  ( 11.72616103466483573, 24.14067372595003036, -21.92230300879598559 ) ) ;
#15985 = CARTESIAN_POINT ( 'NONE',  ( 9.560391798445262879, -11.12854194998381274, -48.69820437222687559 ) ) ;
#15986 = VERTEX_POINT ( 'NONE', #26252 ) ;
#15987 = DIRECTION ( 'NONE',  ( 0.000000000000000000, 0.000000000000000000, -1.000000000000000000 ) ) ;
#15988 = CARTESIAN_POINT ( 'NONE',  ( 52.71259303052651290, 20.20049112655129875, -75.79898569453698087 ) ) ;
#15989 = AXIS2_PLACEMENT_3D ( 'NONE', #29474, #17435, #24486 ) ;
#15990 = CARTESIAN_POINT ( 'NONE',  ( 9.807871728238577447, -10.75438317229078322, -56.71600161805649520 ) ) ;
#15991 = CARTESIAN_POINT ( 'NONE',  ( 7.635415421591210894, -60.86027260432054931, -20.56421356237310150 ) ) ;
#15992 = AXIS2_PLACEMENT_3D ( 'NONE', #28002, #11015, #27494 ) ;
#15993 = CARTESIAN_POINT ( 'NONE',  ( 9.021811926696198469, -11.44481131364510063, -76.96117772256459943 ) ) ;
#15994 = CARTESIAN_POINT ( 'NONE',  ( 16.13393739769620083, -15.61618894467929941, -76.14999999999999147 ) ) ;
#15995 = CARTESIAN_POINT ( 'NONE',  ( 46.64491461174982589, -38.21744283867312220, -57.09507837764103755 ) ) ;
#15996 = ORIENTED_EDGE ( 'NONE', *, *, #470, .T. ) ;
#15997 = CARTESIAN_POINT ( 'NONE',  ( 8.718662699962571594, -16.33757300486989905, -65.20178814406908430 ) ) ;
#15998 = LINE ( 'NONE', #36159, #47329 ) ;
#15999 = CARTESIAN_POINT ( 'NONE',  ( 10.02935865344080035, -20.22754759784489664, -32.14999999999999858 ) ) ;
#16000 = CARTESIAN_POINT ( 'NONE',  ( 47.00221134363980013, 23.02870449882369641, -75.51940564623940588 ) ) ;
#16001 = CARTESIAN_POINT ( 'NONE',  ( 11.13393739769619906, 24.07008072128950005, -43.74348518090240390 ) ) ;
#16002 = PRODUCT ( 'Wheel Axle Bolt', 'Wheel Axle Bolt', '', ( #12578 ) ) ;
#16003 = CARTESIAN_POINT ( 'NONE',  ( 0.1039241094638853335, 19.62646979462214603, -34.69896165024965029 ) ) ;
#16004 = CARTESIAN_POINT ( 'NONE',  ( 9.500562652744140024, -10.71914287566930035, -72.71009270457309981 ) ) ;
#16005 = EDGE_CURVE ( 'NONE', #32504, #20085, #46463, .T. ) ;
#16006 = CARTESIAN_POINT ( 'NONE',  ( 55.56331440656450127, -50.69060432040659947, -75.70197983327919644 ) ) ;
#16008 = CARTESIAN_POINT ( 'NONE',  ( 47.38073022375075283, 23.41843073406132802, -54.64585026063956974 ) ) ;
#16007 = CARTESIAN_POINT ( 'NONE',  ( 88.13393739769620083, -33.11618894467940066, -65.65000000000000568 ) ) ;
#16009 = CARTESIAN_POINT ( 'NONE',  ( 63.40852617131290003, 1.383411777981069957, -68.54655896616850441 ) ) ;
#16010 = CARTESIAN_POINT ( 'NONE',  ( 61.19897335096789703, 14.07984942462570110, -47.06088098606709735 ) ) ;
#16011 = CARTESIAN_POINT ( 'NONE',  ( 84.13393739769618662, -30.31618894467939995, -65.65000000000000568 ) ) ;
#16012 = EDGE_CURVE ( 'NONE', #22570, #4148, #26318, .T. ) ;
#16013 = ORIENTED_EDGE ( 'NONE', *, *, #31597, .F. ) ;
#16014 =( BOUNDED_SURFACE ( )  B_SPLINE_SURFACE ( 2, 2, ( 
 ( #45593, #25903, #21715, #25649, #37727, #42703, #26169, #46385, #14392 ),
 ( #34030, #22752, #2604, #38772, #49786, #42179, #45857, #18577, #50307 ),
 ( #1822, #30617, #13878, #29838, #50040, #30357, #9943, #41918, #38244 ) ),
 .UNSPECIFIED., .F., .T., .T. ) 
 B_SPLINE_SURFACE_WITH_KNOTS ( ( 3, 3 ),
 ( 3, 2, 2, 2, 3 ),
 ( -0.06696923885014899325, 0.06696923885011449307 ),
 ( -3.141592653589790007, -1.570796326794899889, 0.000000000000000000, 1.570796326794899889, 3.141592653589790007 ),
 .UNSPECIFIED. ) 
 GEOMETRIC_REPRESENTATION_ITEM ( )  RATIONAL_B_SPLINE_SURFACE ( (
 ( 1.000000000000000000, 0.7071067811865480168, 1.000000000000000000, 0.7071067811865480168, 1.000000000000000000, 0.7071067811865480168, 1.000000000000000000, 0.7071067811865480168, 1.000000000000000000),
 ( 0.9977583984878120038, 0.7055217295565610058, 0.9977583984878120038, 0.7055217295565610058, 0.9977583984878120038, 0.7055217295565610058, 0.9977583984878120038, 0.7055217295565610058, 0.9977583984878120038),
 ( 1.000000000000000000, 0.7071067811865480168, 1.000000000000000000, 0.7071067811865480168, 1.000000000000000000, 0.7071067811865480168, 1.000000000000000000, 0.7071067811865480168, 1.000000000000000000) ) ) 
 REPRESENTATION_ITEM ( '' )  SURFACE ( )  );
#16015 = CARTESIAN_POINT ( 'NONE',  ( 52.88731329286200378, -49.63076474127340276, -48.71031102133859747 ) ) ;
#16016 = AXIS2_PLACEMENT_3D ( 'NONE', #23683, #44653, #36521 ) ;
#16017 = CARTESIAN_POINT ( 'NONE',  ( 57.87157263515249639, -45.40826915251930274, -26.12905093743479767 ) ) ;
#16018 = CARTESIAN_POINT ( 'NONE',  ( 12.91798985874082639, -22.86794439454725847, -66.42520807091403867 ) ) ;
#16019 = CARTESIAN_POINT ( 'NONE',  ( 61.25735466683790520, 14.07817815260590066, -47.12428023552489975 ) ) ;
#16020 = VECTOR ( 'NONE', #43690, 1000.000000000000000 ) ;
#16021 = CARTESIAN_POINT ( 'NONE',  ( 19.39019095385939906, -22.31719682283620187, -70.58867545639529339 ) ) ;
#16022 = CARTESIAN_POINT ( 'NONE',  ( 51.85163418285049630, 18.34999185856599979, -76.86771305873580218 ) ) ;
#16023 = CARTESIAN_POINT ( 'NONE',  ( 53.40908402083690731, 18.14278958704170108, -48.94486837258570233 ) ) ;
#16024 = CARTESIAN_POINT ( 'NONE',  ( 71.34180821298970443, 0.9214125008369580261, -70.72054727061200197 ) ) ;
#16025 = CARTESIAN_POINT ( 'NONE',  ( -0.2175830584369590204, -45.44300788545632486, -34.95572367894526877 ) ) ;
#16026 = ORIENTED_EDGE ( 'NONE', *, *, #20615, .T. ) ;
#16027 = DIRECTION ( 'NONE',  ( -0.5193766129849320956, 0.000000000000000000, -0.8545454545454562734 ) ) ;
#16028 = CARTESIAN_POINT ( 'NONE',  ( 47.61882127642510198, -54.54439795203430208, -55.10468976659860374 ) ) ;
#16029 = CARTESIAN_POINT ( 'NONE',  ( -10.45347530935170077, 11.54094627956400032, -5.983182295913979765 ) ) ;
#16030 = DIRECTION ( 'NONE',  ( -0.5109955813515499878, -0.8595833385072046973, 0.000000000000000000 ) ) ;
#16031 = CARTESIAN_POINT ( 'NONE',  ( 59.67048302056260667, -29.19628695015689956, -15.77538394522889931 ) ) ;
#16032 = CARTESIAN_POINT ( 'NONE',  ( 71.23851365796429036, 1.390208944942409985, -61.02997314496759884 ) ) ;
#16033 = CARTESIAN_POINT ( 'NONE',  ( 11.13393739769619906, 31.88305279702909800, -43.74348518090240390 ) ) ;
#16034 = CARTESIAN_POINT ( 'NONE',  ( 72.79412820737060485, 1.158194067776799896, -61.92810128176829920 ) ) ;
#16035 = CARTESIAN_POINT ( 'NONE',  ( 51.45476229416896530, -34.38915632507681863, -76.74519247898817298 ) ) ;
#16036 = EDGE_CURVE ( 'NONE', #36314, #26336, #36051, .T. ) ;
#16037 = CARTESIAN_POINT ( 'NONE',  ( 22.34855670084171209, -12.85190603941985721, -66.31973049179434554 ) ) ;
#16038 = ORIENTED_EDGE ( 'NONE', *, *, #34344, .T. ) ;
#16039 = ORIENTED_EDGE ( 'NONE', *, *, #51371, .T. ) ;
#16040 = DIRECTION ( 'NONE',  ( 0.000000000000000000, 0.000000000000000000, -1.000000000000000000 ) ) ;
#16041 = CARTESIAN_POINT ( 'NONE',  ( 68.13393739769618662, -30.31618894467939995, -65.65000000000000568 ) ) ;
#16042 = VERTEX_POINT ( 'NONE', #31974 ) ;
#16043 = CARTESIAN_POINT ( 'NONE',  ( 17.16941547515002497, -7.705179032722160315, -59.04929731532414650 ) ) ;
#16044 = CARTESIAN_POINT ( 'NONE',  ( 12.43552644545811425, -9.914939322250329923, -49.76975001323243930 ) ) ;
#16045 = VERTEX_POINT ( 'NONE', #32224 ) ;
#16046 = CARTESIAN_POINT ( 'NONE',  ( 10.75772284190022710, 33.13535827837971937, -23.47630699481211636 ) ) ;
#16047 = CARTESIAN_POINT ( 'NONE',  ( 42.00942139458377511, 6.392864097679653135, -80.27251128686401671 ) ) ;
#16048 = CARTESIAN_POINT ( 'NONE',  ( 60.91971420063490683, 14.46337360283989959, -47.74179738751160329 ) ) ;
#16049 = CARTESIAN_POINT ( 'NONE',  ( 24.21273651960749973, -13.96824331337349889, -39.72828012266349873 ) ) ;
#16050 = CARTESIAN_POINT ( 'NONE',  ( 24.04507396969289346, -15.61618901627517531, -67.50767071486835391 ) ) ;
#16051 = CARTESIAN_POINT ( 'NONE',  ( 10.78192289013670013, 33.70626262526499772, -17.70651626560779945 ) ) ;
#16052 = CARTESIAN_POINT ( 'NONE',  ( 62.34145908511610656, -30.26177483428519821, -16.23785720254290155 ) ) ;
#16053 = CIRCLE ( 'NONE', #5182, 2.500000000000003553 ) ;
#16054 = CARTESIAN_POINT ( 'NONE',  ( 15.09848046148962020, -23.52719988351775982, -42.33399791108317345 ) ) ;
#16055 = CARTESIAN_POINT ( 'NONE',  ( 8.318016906984530223, -16.32137358708479979, -80.98384931626918615 ) ) ;
#16056 = AXIS2_PLACEMENT_3D ( 'NONE', #42012, #34905, #6112 ) ;
#16057 = CIRCLE ( 'NONE', #31069, 25.00000000000000355 ) ;
#16058 = CARTESIAN_POINT ( 'NONE',  ( 41.36999407038749865, 14.03644748879320048, -6.004979454220869428 ) ) ;
#16059 = CARTESIAN_POINT ( 'NONE',  ( 19.13393739769620083, -49.61618894467939356, -35.14999999999999858 ) ) ;
#16060 = CARTESIAN_POINT ( 'NONE',  ( 84.27240597999899308, -43.88482305096810165, -47.25334685439979410 ) ) ;
#16061 = CARTESIAN_POINT ( 'NONE',  ( 64.51140068127359939, 1.434916633744939940, -70.06045877469239258 ) ) ;
#16062 = CARTESIAN_POINT ( 'NONE',  ( 8.035678613309558571, -14.06669697307060041, -46.56784545357859173 ) ) ;
#16063 = ORIENTED_EDGE ( 'NONE', *, *, #23278, .T. ) ;
#16064 = CARTESIAN_POINT ( 'NONE',  ( 53.25910687114200215, -49.18441974074990242, -27.17009175550089850 ) ) ;
#16065 = ADVANCED_FACE ( 'NONE', ( #7651 ), #12341, .T. ) ;
#16066 = CARTESIAN_POINT ( 'NONE',  ( 14.30723785210539845, -50.71453875907170072, -21.19168582719299820 ) ) ;
#16067 = CARTESIAN_POINT ( 'NONE',  ( 22.85082190356551735, -19.82021127139173799, -39.68565907844063645 ) ) ;
#16068 = CARTESIAN_POINT ( 'NONE',  ( 9.221496127252056141, -19.60046032720535436, -64.62566521129184594 ) ) ;
#16069 = CARTESIAN_POINT ( 'NONE',  ( 15.01109173769490113, 12.72875286183729848, -62.64999999999999858 ) ) ;
#16070 = CARTESIAN_POINT ( 'NONE',  ( 72.38393739883420608, 11.88381105532070059, -61.44999999999999574 ) ) ;
#16071 = VERTEX_POINT ( 'NONE', #20441 ) ;
#16072 = CARTESIAN_POINT ( 'NONE',  ( -8.073139882959649682, -45.00859888370850115, -5.631272549003790040 ) ) ;
#16073 = CARTESIAN_POINT ( 'NONE',  ( -0.007164427059776000244, -4.186223695871990280, -34.77269723891829756 ) ) ;
#16074 = CARTESIAN_POINT ( 'NONE',  ( 9.366959721612127865, -16.50215060180284254, -49.41115363279539707 ) ) ;
#16075 = CARTESIAN_POINT ( 'NONE',  ( 63.11172336169240538, 1.097085799869280009, -62.44531798733959960 ) ) ;
#16076 = CARTESIAN_POINT ( 'NONE',  ( 57.49861655706580166, -50.10448309126950051, -52.59177543263909627 ) ) ;
#16077 = CARTESIAN_POINT ( 'NONE',  ( 42.86117915671640333, 12.27262101796790006, -4.698036889951329620 ) ) ;
#16078 = CARTESIAN_POINT ( 'NONE',  ( 14.06328960009770412, -7.911080816989770170, -61.20899688243854087 ) ) ;
#16079 = DIRECTION ( 'NONE',  ( 0.000000000000000000, 0.000000000000000000, -1.000000000000000000 ) ) ;
#16080 = CARTESIAN_POINT ( 'NONE',  ( 58.27624582431690214, -46.80735200045160127, -47.55852830428500511 ) ) ;
#16081 = CARTESIAN_POINT ( 'NONE',  ( 8.428794369977973489, -13.54566571443409906, -74.87568142060762000 ) ) ;
#16082 = CARTESIAN_POINT ( 'NONE',  ( 68.13393739769625768, -15.41618894467850076, -103.0993275156848910 ) ) ;
#16083 = CARTESIAN_POINT ( 'NONE',  ( 20.53650276133985031, -41.76263555408612405, -34.79644660940672907 ) ) ;
#16084 = AXIS2_PLACEMENT_3D ( 'NONE', #12487, #28712, #44456 ) ;
#16085 = CARTESIAN_POINT ( 'NONE',  ( 17.16957569431084707, -7.705201912737116743, -73.04933477425599619 ) ) ;
#16086 = DIRECTION ( 'NONE',  ( -0.000000000000000000, 1.000000000000000000, 0.000000000000000000 ) ) ;
#16087 = EDGE_LOOP ( 'NONE', ( #1736, #36515, #7498, #44202 ) ) ;
#16088 = CARTESIAN_POINT ( 'NONE',  ( -18.86606260230390220, 19.38381105532060289, 11.34999999999999964 ) ) ;
#16089 = CARTESIAN_POINT ( 'NONE',  ( 45.07858682377059978, 14.88010818488339915, -9.026855431852879974 ) ) ;
#16090 = DIRECTION ( 'NONE',  ( 0.000000000000000000, -1.000000000000000000, 0.000000000000000000 ) ) ;
#16091 = CARTESIAN_POINT ( 'NONE',  ( 11.95635311929369848, -9.163797422253020741, -81.23899999999999011 ) ) ;
#16092 = EDGE_LOOP ( 'NONE', ( #45068, #28836 ) ) ;
#16093 = EDGE_CURVE ( 'NONE', #46682, #14108, #19688, .T. ) ;
#16094 = CARTESIAN_POINT ( 'NONE',  ( 17.92031055095850078, 21.20322725566390076, -75.94942944171690158 ) ) ;
#16095 = VERTEX_POINT ( 'NONE', #35681 ) ;
#16096 = ADVANCED_FACE ( 'NONE', ( #23847 ), #48247, .T. ) ;
#16097 = ORIENTED_EDGE ( 'NONE', *, *, #41777, .T. ) ;
#16098 = DIRECTION ( 'NONE',  ( 1.000000000000000000, 0.000000000000000000, 0.000000000000000000 ) ) ;
#16099 = CARTESIAN_POINT ( 'NONE',  ( 21.83477058027380124, -10.19727932716529928, -81.23899999999999011 ) ) ;
#16100 = CARTESIAN_POINT ( 'NONE',  ( 61.69769988959340168, 13.93882227395219964, -46.83837617009780274 ) ) ;
#16101 = DIRECTION ( 'NONE',  ( 0.000000000000000000, 0.000000000000000000, -1.000000000000000000 ) ) ;
#16102 = B_SPLINE_SURFACE_WITH_KNOTS ( 'NONE', 1, 3, ( 
 ( #15585, #8226, #7726, #39687, #16342, #35752, #39945, #31539 ),
 ( #47558, #11653, #51734, #12166, #20260, #32298, #15829, #47812 ) ),
 .UNSPECIFIED., .F., .F., .F.,
 ( 2, 2 ),
 ( 4, 2, 2, 4 ),
 ( 0.1261347826432950014, 0.9339437630689100267 ),
 ( 3.992643801987300289, 8.116559215544439709, 13.46070403139630045, 18.66056373795289858 ),
 .UNSPECIFIED. ) ;
#16103 = CARTESIAN_POINT ( 'NONE',  ( 12.02928788648473635, 34.13296709268954743, -17.22609660999479431 ) ) ;
#16104 = ORIENTED_EDGE ( 'NONE', *, *, #518, .T. ) ;
#16105 = CARTESIAN_POINT ( 'NONE',  ( 17.77056402554710246, -8.755867344676808273, -42.42172377882659617 ) ) ;
#16106 = DIRECTION ( 'NONE',  ( -0.8732394366197182567, 0.4872913772396111343, 0.000000000000000000 ) ) ;
#16107 = VERTEX_POINT ( 'NONE', #44052 ) ;
#16108 = EDGE_LOOP ( 'NONE', ( #33752, #14930, #45562, #50 ) ) ;
#16109 = DIRECTION ( 'NONE',  ( 0.000000000000000000, 1.000000000000000000, 0.000000000000000000 ) ) ;
#16110 = DIRECTION ( 'NONE',  ( 0.000000000000000000, 1.784214116308896997E-11, 1.000000000000000000 ) ) ;
#16111 = CARTESIAN_POINT ( 'NONE',  ( 61.12170114217160233, 14.23482143552810086, -47.45407097581740175 ) ) ;
#16112 = CARTESIAN_POINT ( 'NONE',  ( 22.13393739769589885, 22.91950879131610108, -54.64999999999999858 ) ) ;
#16113 = CARTESIAN_POINT ( 'NONE',  ( 41.83063930241080186, -43.61086970063350066, -3.362295850879169823 ) ) ;
#16114 = CARTESIAN_POINT ( 'NONE',  ( -2.656266623734050203, 17.48898290397159982, -4.829465371942860408 ) ) ;
#16115 = CIRCLE ( 'NONE', #47124, 17.63819660112499932 ) ;
#16116 = AXIS2_PLACEMENT_3D ( 'NONE', #12375, #12125, #23881 ) ;
#16117 = CARTESIAN_POINT ( 'NONE',  ( 47.07822794249411658, 23.33748126006274859, -75.12259495526954822 ) ) ;
#16118 = CARTESIAN_POINT ( 'NONE',  ( 55.22144174253947568, 14.83847152459031449, -16.34786475617187307 ) ) ;
#16119 = CARTESIAN_POINT ( 'NONE',  ( 19.39616629670310033, -8.478639589776950203, -60.92396586663380020 ) ) ;
#16120 = EDGE_LOOP ( 'NONE', ( #33359, #31971, #23332, #34074 ) ) ;
#16121 = CARTESIAN_POINT ( 'NONE',  ( 57.40277299468780114, 16.17492991088059995, -48.23107244050790143 ) ) ;
#16122 = EDGE_CURVE ( 'NONE', #7703, #39662, #16523, .T. ) ;
#16123 = CARTESIAN_POINT ( 'NONE',  ( 41.06759784644540190, 14.27213265972969936, -6.034531555287039772 ) ) ;
#16124 = CARTESIAN_POINT ( 'NONE',  ( 12.15072521531869931, 34.03384901777550198, -46.19630097385869760 ) ) ;
#16125 = CARTESIAN_POINT ( 'NONE',  ( 72.54736496963849390, 1.191618978581419963, -69.67374006097030303 ) ) ;
#16126 = CARTESIAN_POINT ( 'NONE',  ( 44.17593333301926606, -39.96876567252856205, -65.80818625478011086 ) ) ;
#16127 = EDGE_CURVE ( 'NONE', #29610, #17159, #28566, .T. ) ;
#16128 = PRESENTATION_STYLE_ASSIGNMENT (( #35539 ) ) ;
#16129 = CARTESIAN_POINT ( 'NONE',  ( 13.23399064597960084, 18.92162210823540036, -21.05825742057550087 ) ) ;
#16130 = CARTESIAN_POINT ( 'NONE',  ( 46.93194736084949881, 22.96293243065590062, -75.61358166513510071 ) ) ;
#16131 = CARTESIAN_POINT ( 'NONE',  ( 48.64767879017799856, -53.93625458155220542, -54.52761353198660288 ) ) ;
#16132 = CARTESIAN_POINT ( 'NONE',  ( -3.979110003385970540, 17.20385159207049952, -5.632303519440180040 ) ) ;
#16133 = VECTOR ( 'NONE', #36703, 1000.000000000000114 ) ;
#16134 = DIRECTION ( 'NONE',  ( 0.000000000000000000, 1.000000000000000000, 0.000000000000000000 ) ) ;
#16135 = DIRECTION ( 'NONE',  ( 0.000000000000000000, 1.000000000000000000, 0.000000000000000000 ) ) ;
#16136 = ORIENTED_EDGE ( 'NONE', *, *, #230, .T. ) ;
#16137 = CARTESIAN_POINT ( 'NONE',  ( 9.810283122618720597, -11.67688811027330154, -34.24467998873389973 ) ) ;
#16138 = CARTESIAN_POINT ( 'NONE',  ( 15.67962062493140074, -50.86266781791879765, -20.15000000000000213 ) ) ;
#16139 = ORIENTED_EDGE ( 'NONE', *, *, #25881, .F. ) ;
#16140 = CARTESIAN_POINT ( 'NONE',  ( 57.24929578595760660, 21.38381105532069881, -63.99406948319570887 ) ) ;
#16141 = CARTESIAN_POINT ( 'NONE',  ( 60.63571203433270540, -45.60655262937140719, -47.39339951304060605 ) ) ;
#16142 = CYLINDRICAL_SURFACE ( 'NONE', #19557, 3.000000000000000444 ) ;
#16143 = LINE ( 'NONE', #43680, #41147 ) ;
#16144 = EDGE_CURVE ( 'NONE', #35823, #27459, #21856, .T. ) ;
#16146 = CARTESIAN_POINT ( 'NONE',  ( 44.66436339216802764, -33.16345305600000870, -44.75696816342043860 ) ) ;
#16145 = CARTESIAN_POINT ( 'NONE',  ( 42.89541628683672059, 8.623681277660011801, -72.00529067016060480 ) ) ;
#16147 = DIRECTION ( 'NONE',  ( -1.000000000000000000, 0.000000000000000000, 0.000000000000000000 ) ) ;
#16148 = CARTESIAN_POINT ( 'NONE',  ( 8.943569970476740849, -49.33365190531349498, -34.64999999999999858 ) ) ;
#16149 = ORIENTED_EDGE ( 'NONE', *, *, #31890, .T. ) ;
#16150 = CARTESIAN_POINT ( 'NONE',  ( 83.34325726105160470, -45.31017261718839251, -47.50551966704799867 ) ) ;
#16151 = VERTEX_POINT ( 'NONE', #41151 ) ;
#16152 = VERTEX_POINT ( 'NONE', #45353 ) ;
#16153 = ADVANCED_FACE ( 'NONE', ( #37227 ), #13643, .F. ) ;
#16154 = ORIENTED_EDGE ( 'NONE', *, *, #33573, .T. ) ;
#16155 = CARTESIAN_POINT ( 'NONE',  ( 16.13393739769620083, -15.61618894467929941, -32.14999999999999858 ) ) ;
#16156 = CARTESIAN_POINT ( 'NONE',  ( 53.99784841347855036, -50.61618894465041052, -77.02981973011630146 ) ) ;
#16157 = VECTOR ( 'NONE', #43610, 1000.000000000000000 ) ;
#16158 = CARTESIAN_POINT ( 'NONE',  ( 76.39889860447665626, -19.26176533219966203, -12.79180084499177816 ) ) ;
#16159 = CARTESIAN_POINT ( 'NONE',  ( 53.21144349652569616, -51.94262854214029801, -53.42264529815139440 ) ) ;
#16160 = CIRCLE ( 'NONE', #23655, 2.000000000000001776 ) ;
#16161 = ORIENTED_EDGE ( 'NONE', *, *, #20255, .F. ) ;
#16162 = ORIENTED_EDGE ( 'NONE', *, *, #35076, .F. ) ;
#16163 = CARTESIAN_POINT ( 'NONE',  ( 11.27214541155795047, -21.94226801064548837, -56.21594714068361043 ) ) ;
#16164 = CARTESIAN_POINT ( 'NONE',  ( -20.68272678989470847, -2.738091952025576425, -53.00346737314672652 ) ) ;
#16165 = FACE_OUTER_BOUND ( 'NONE', #50342, .T. ) ;
#16166 = CARTESIAN_POINT ( 'NONE',  ( 40.57649240635721100, 6.328436186825659782, -83.97002642401369599 ) ) ;
#16167 = CARTESIAN_POINT ( 'NONE',  ( 62.09645049968020203, 0.05786461624523400044, -16.78440013667709962 ) ) ;
#16168 = CARTESIAN_POINT ( 'NONE',  ( 9.894687805641389389, -53.60726374558549878, -34.64999999999999858 ) ) ;
#16169 = ORIENTED_EDGE ( 'NONE', *, *, #32427, .T. ) ;
#16170 = CARTESIAN_POINT ( 'NONE',  ( 62.88393739769619373, 4.883811055320659733, -84.94863984844531046 ) ) ;
#16171 = CARTESIAN_POINT ( 'NONE',  ( 53.45777095194249995, -50.57384060062700115, -76.87859158467649934 ) ) ;
#16172 = CARTESIAN_POINT ( 'NONE',  ( 18.23096359433825242, -9.164089042641412775, -34.05282851151127232 ) ) ;
#16173 = CARTESIAN_POINT ( 'NONE',  ( 57.55751162087899786, 17.38381105532069881, -53.92796738110899923 ) ) ;
#16174 = CARTESIAN_POINT ( 'NONE',  ( 15.83244136102879907, -23.45811777191660141, -54.52472634102049653 ) ) ;
#16175 = CARTESIAN_POINT ( 'NONE',  ( 13.51862060011250044, -50.60094953679219998, -21.33274412383610041 ) ) ;
#16176 = CIRCLE ( 'NONE', #45477, 10.00000000000000711 ) ;
#16177 = FACE_OUTER_BOUND ( 'NONE', #51492, .T. ) ;
#16178 = CARTESIAN_POINT ( 'NONE',  ( 18.49554612515125740, -51.29571572326634765, -15.70772097152689106 ) ) ;
#16179 = CARTESIAN_POINT ( 'NONE',  ( 68.13393739769790614, -49.95860450174040324, -75.14853292321149070 ) ) ;
#16180 = CARTESIAN_POINT ( 'NONE',  ( 68.38970075077773458, -0.8918033001876759513, -18.15384973117020451 ) ) ;
#16181 = LINE ( 'NONE', #40296, #42172 ) ;
#16182 = CARTESIAN_POINT ( 'NONE',  ( 23.02971233589060063, -14.13603787934130018, -54.77987702475120102 ) ) ;
#16183 = FACE_BOUND ( 'NONE', #28077, .T. ) ;
#16184 = ORIENTED_EDGE ( 'NONE', *, *, #12920, .F. ) ;
#16185 = CARTESIAN_POINT ( 'NONE',  ( 47.32111516514320471, 22.89537558975190024, -75.47461153638720077 ) ) ;
#16186 = EDGE_CURVE ( 'NONE', #621, #32837, #33792, .T. ) ;
#16187 = AXIS2_PLACEMENT_3D ( 'NONE', #9899, #48712, #17256 ) ;
#16188 = CARTESIAN_POINT ( 'NONE',  ( 47.36150376523510630, -54.68114167742809428, -54.82442221309270280 ) ) ;
#16189 = DIRECTION ( 'NONE',  ( 1.000000000000000000, 0.000000000000000000, 0.000000000000000000 ) ) ;
#16190 = CARTESIAN_POINT ( 'NONE',  ( 22.46010233604985373, -10.75451059975396895, -37.29933751133587805 ) ) ;
#16191 = DIRECTION ( 'NONE',  ( 0.000000000000000000, -1.000000000000000000, 0.000000000000000000 ) ) ;
#16192 = EDGE_CURVE ( 'NONE', #5413, #8909, #21480, .T. ) ;
#16193 = VECTOR ( 'NONE', #11089, 1000.000000000000000 ) ;
#16194 = CARTESIAN_POINT ( 'NONE',  ( 23.87157417762563227, -13.91310202843878230, -55.43871031765390001 ) ) ;
#16195 = AXIS2_PLACEMENT_3D ( 'NONE', #24410, #32272, #334 ) ;
#16196 = CARTESIAN_POINT ( 'NONE',  ( 9.543025643916356771, -13.84508154717068962, -75.53614680028508133 ) ) ;
#16197 = EDGE_CURVE ( 'NONE', #42105, #37038, #37742, .T. ) ;
#16198 = CARTESIAN_POINT ( 'NONE',  ( 10.61751707708940096, 33.59325229226949716, -18.17421237877550411 ) ) ;
#16200 = CARTESIAN_POINT ( 'NONE',  ( 15.09847792035051128, -23.52719957632157488, -74.04933483335966571 ) ) ;
#16199 = LINE ( 'NONE', #48172, #21467 ) ;
#16201 = CARTESIAN_POINT ( 'NONE',  ( 14.92239344893164699, -52.74445246665722919, -76.12392058102736314 ) ) ;
#16202 = CARTESIAN_POINT ( 'NONE',  ( 48.56556163587730168, 22.87165378742070132, -54.94029309988020060 ) ) ;
#16203 = ORIENTED_EDGE ( 'NONE', *, *, #24022, .F. ) ;
#16204 = CARTESIAN_POINT ( 'NONE',  ( 52.70624018093069907, -49.74719148043480033, -48.71312393436970467 ) ) ;
#16205 = ORIENTED_EDGE ( 'NONE', *, *, #41269, .F. ) ;
#16206 = CARTESIAN_POINT ( 'NONE',  ( 42.09413162889060089, 6.247507344166270293, -79.82720547731395300 ) ) ;
#16207 = CARTESIAN_POINT ( 'NONE',  ( 49.40552051342540096, 22.26542118999089936, -54.15739458345379376 ) ) ;
#16208 = DIRECTION ( 'NONE',  ( 1.000000000000000000, 0.000000000000000000, 0.000000000000000000 ) ) ;
#16210 = CARTESIAN_POINT ( 'NONE',  ( 55.17839213106780250, 15.74952588299860246, -26.00983945363739736 ) ) ;
#16209 = CARTESIAN_POINT ( 'NONE',  ( 83.48374992014450413, 13.50741312754700019, -46.79909128427029685 ) ) ;
#16211 = CARTESIAN_POINT ( 'NONE',  ( 21.84466674371100225, -11.47733293930889964, -62.25319380417529658 ) ) ;
#16212 = CARTESIAN_POINT ( 'NONE',  ( 53.12218290940240450, 18.34074958227849805, -49.13784296393349393 ) ) ;
#16213 = CARTESIAN_POINT ( 'NONE',  ( 56.10980393773469643, -45.40982727206459657, -16.53355515139729803 ) ) ;
#16214 = CARTESIAN_POINT ( 'NONE',  ( 55.91596999402320023, 14.67228162054319895, -25.32543311652580087 ) ) ;
#16215 = AXIS2_PLACEMENT_3D ( 'NONE', #4694, #1028, #48730 ) ;
#16216 = ORIENTED_EDGE ( 'NONE', *, *, #23519, .T. ) ;
#16217 = CARTESIAN_POINT ( 'NONE',  ( 9.244168744909480040, -11.85881804280390028, -44.44642820540079953 ) ) ;
#16218 = B_SPLINE_CURVE_WITH_KNOTS ( 'NONE', 3,
 ( #42534, #27046, #50645, #47245, #3471, #43307, #10817, #22585, #47496, #19442, #19181, #14741, #30711, #35692, #35425, #15770, #11593, #46474 ),
 .UNSPECIFIED., .F., .F.,
 ( 4, 2, 2, 2, 2, 2, 2, 2, 4 ),
 ( 0.4999984352163039381, 0.5624986308142660985, 0.6249988264122281478, 0.6874990220101903082, 0.7499992176081524686, 0.8124994132061142960, 0.8749996088040762343, 0.9374998044020381727, 1.000000000000000000 ),
 .UNSPECIFIED. ) ;
#16219 = EDGE_CURVE ( 'NONE', #4886, #42739, #16950, .T. ) ;
#16220 = ORIENTED_EDGE ( 'NONE', *, *, #29496, .T. ) ;
#16221 = CARTESIAN_POINT ( 'NONE',  ( 12.02928808077719935, -65.36534498448229158, -17.22609656285550273 ) ) ;
#16222 = CARTESIAN_POINT ( 'NONE',  ( 11.52812372297789878, 33.73647174606139743, -46.36286941860509359 ) ) ;
#16223 = DIRECTION ( 'NONE',  ( 0.000000000000000000, 0.000000000000000000, 1.000000000000000000 ) ) ;
#16224 = CARTESIAN_POINT ( 'NONE',  ( 47.88526556163500913, -54.30197853586789591, -54.48901645874850175 ) ) ;
#16225 = DIRECTION ( 'NONE',  ( 1.000000000000000000, 0.000000000000000000, 0.000000000000000000 ) ) ;
#16226 = CARTESIAN_POINT ( 'NONE',  ( 0.03129314105497079529, -10.48887801743429904, -34.73925587534019854 ) ) ;
#16227 = ORIENTED_EDGE ( 'NONE', *, *, #12178, .T. ) ;
#16228 = DIRECTION ( 'NONE',  ( 1.000000000000000000, 1.222653822078627158E-29, -4.718060457820110146E-11 ) ) ;
#16229 = CARTESIAN_POINT ( 'NONE',  ( 11.10557205223450161, -63.32885013192529300, -44.25322260217060233 ) ) ;
#16230 = CARTESIAN_POINT ( 'NONE',  ( 13.72056387933040433, 20.81200738410580442, -75.33783710294623859 ) ) ;
#16231 = VERTEX_POINT ( 'NONE', #45873 ) ;
#16232 = CARTESIAN_POINT ( 'NONE',  ( 17.20688454841970128, 14.56395709402249850, -35.14999999999999858 ) ) ;
#16233 = CARTESIAN_POINT ( 'NONE',  ( 50.17499495802539400, -49.21634929470250341, -76.14999999999999147 ) ) ;
#16234 = DIRECTION ( 'NONE',  ( 0.000000000000000000, 0.000000000000000000, -1.000000000000000000 ) ) ;
#16235 = AXIS2_PLACEMENT_3D ( 'NONE', #34821, #30880, #19619 ) ;
#16236 = ORIENTED_EDGE ( 'NONE', *, *, #32723, .F. ) ;
#16237 = CARTESIAN_POINT ( 'NONE',  ( 53.63393739769619373, -53.11618894467930119, 11.84999999999999964 ) ) ;
#16238 = CARTESIAN_POINT ( 'NONE',  ( 53.29384558423090112, -50.54670888882439783, -38.31189016485959797 ) ) ;
#16239 = DIRECTION ( 'NONE',  ( 0.000000000000000000, 0.000000000000000000, 1.000000000000000000 ) ) ;
#16240 = CARTESIAN_POINT ( 'NONE',  ( 2.423250969874880312, -25.81972099615670047, -35.01387690002259490 ) ) ;
#16241 = EDGE_CURVE ( 'NONE', #25078, #7053, #27525, .T. ) ;
#16242 = CARTESIAN_POINT ( 'NONE',  ( 14.23060326220489991, -23.63865983740360122, -72.36647972087459380 ) ) ;
#16243 = CARTESIAN_POINT ( 'NONE',  ( 11.34407006786130623, -55.32883834980184190, -21.54741951671798716 ) ) ;
#16244 = DIRECTION ( 'NONE',  ( 0.000000000000000000, 1.000000000000000000, 0.000000000000000000 ) ) ;
#16245 = PRODUCT_CONTEXT ( 'NONE', #37159, 'mechanical' ) ;
#16246 = ORIENTED_EDGE ( 'NONE', *, *, #22376, .T. ) ;
#16247 = CARTESIAN_POINT ( 'NONE',  ( 17.66480776815700082, -22.90749402086359865, -62.66678235003330144 ) ) ;
#16248 = CARTESIAN_POINT ( 'NONE',  ( 72.13393739769620083, -1.116188944679340045, -20.65000000000000213 ) ) ;
#16249 = CYLINDRICAL_SURFACE ( 'NONE', #17826, 0.4999999999999991118 ) ;
#16250 = VECTOR ( 'NONE', #41444, 1000.000000000000000 ) ;
#16251 = CARTESIAN_POINT ( 'NONE',  ( 47.26713003401719959, 23.41039128977789829, -74.72332766641309831 ) ) ;
#16252 = DIRECTION ( 'NONE',  ( 1.000000000000000000, 0.000000000000000000, 0.000000000000000000 ) ) ;
#16253 = DIRECTION ( 'NONE',  ( -1.681987882033212302E-11, 1.000000000000000000, 0.000000000000000000 ) ) ;
#16254 = EDGE_CURVE ( 'NONE', #49131, #28918, #37793, .T. ) ;
#16255 = B_SPLINE_CURVE_WITH_KNOTS ( 'NONE', 3,
 ( #4642, #12520, #48160, #29008, #8591, #49210, #37144, #8073, #24535, #20108, #36100, #8326, #5185, #20617, #44744, #17230, #16702, #20883 ),
 .UNSPECIFIED., .F., .F.,
 ( 4, 2, 2, 2, 2, 2, 2, 2, 4 ),
 ( 0.5000002878041880372, 0.5625002518286645881, 0.6250002158531410279, 0.6875001798776174677, 0.7500001439020940186, 0.8125001079265705695, 0.8750000719510470093, 0.9375000359755234491, 1.000000000000000000 ),
 .UNSPECIFIED. ) ;
#16256 = CARTESIAN_POINT ( 'NONE',  ( 12.26707159645439837, 33.49137753132240647, -15.95265749176260073 ) ) ;
#16257 = CARTESIAN_POINT ( 'NONE',  ( 10.34509433763069985, -21.48747643008940145, -78.25541787902648139 ) ) ;
#16258 = EDGE_CURVE ( 'NONE', #37842, #1665, #14355, .T. ) ;
#16259 = B_SPLINE_CURVE_WITH_KNOTS ( 'NONE', 3,
 ( #30133, #18093, #50335, #34061, #14423, #31670, #7090, #46673, #19890, #18862 ),
 .UNSPECIFIED., .F., .F.,
 ( 4, 1, 1, 1, 1, 1, 1, 4 ),
 ( 0.5000036202821666054, 0.5662063123692606670, 0.6454252434329685872, 0.7246441744965181897, 0.8038631055600700126, 0.8830820366237779329, 0.9623009676873275353, 1.000000000000000000 ),
 .UNSPECIFIED. ) ;
#16261 = CARTESIAN_POINT ( 'NONE',  ( 11.89321892218980103, -65.43602743108449715, -22.25048313876769868 ) ) ;
#16260 = DIRECTION ( 'NONE',  ( 0.000000000000000000, 0.000000000000000000, -1.000000000000000000 ) ) ;
#16262 = AXIS2_PLACEMENT_3D ( 'NONE', #23288, #19384, #31414 ) ;
#16263 = CARTESIAN_POINT ( 'NONE',  ( 63.03382193542370260, 0.9209334348186318797, -68.81061689070359932 ) ) ;
#16264 = CARTESIAN_POINT ( 'NONE',  ( 61.51108477065319846, 13.91219452496449982, -46.37201720214299883 ) ) ;
#16265 = CARTESIAN_POINT ( 'NONE',  ( 11.27231895528897887, -9.289978665370313138, -78.79933570999904191 ) ) ;
#16266 = FACE_OUTER_BOUND ( 'NONE', #4687, .T. ) ;
#16267 = ORIENTED_EDGE ( 'NONE', *, *, #39349, .T. ) ;
#16268 = CARTESIAN_POINT ( 'NONE',  ( 53.00700885799259510, -49.56805288106040308, -48.78176285252619948 ) ) ;
#16269 = CARTESIAN_POINT ( 'NONE',  ( 59.96235233370940421, -45.26212046306700643, -26.64974492922270244 ) ) ;
#16270 = DIRECTION ( 'NONE',  ( 0.000000000000000000, 0.000000000000000000, -1.000000000000000000 ) ) ;
#16271 = CARTESIAN_POINT ( 'NONE',  ( 13.86909323948760075, 19.40590670161929765, -21.27400668797769612 ) ) ;
#16272 = CARTESIAN_POINT ( 'NONE',  ( 57.12645307100470404, 14.55895300901689993, -26.23065065375599758 ) ) ;
#16273 = CARTESIAN_POINT ( 'NONE',  ( 23.06556184739849868, -18.34735651441920012, -78.35213070062998497 ) ) ;
#16274 = CARTESIAN_POINT ( 'NONE',  ( 51.15791182533700265, 19.03874145082539826, -76.23077825227480275 ) ) ;
#16275 = CARTESIAN_POINT ( 'NONE',  ( 52.80366186835330211, 18.44443676282890010, -48.66065998140030047 ) ) ;
#16276 = CARTESIAN_POINT ( 'NONE',  ( 71.22645170866519493, 1.102581332775290024, -70.73820378408520071 ) ) ;
#16277 = FACE_OUTER_BOUND ( 'NONE', #16092, .T. ) ;
#16278 = EDGE_LOOP ( 'NONE', ( #18138, #12423, #51537, #4525, #33251 ) ) ;
#16279 = CARTESIAN_POINT ( 'NONE',  ( -1.839728563314089849, -28.30269090235150031, -54.64999999999999858 ) ) ;
#16280 = CARTESIAN_POINT ( 'NONE',  ( 47.53109895159769849, -54.58212600392469938, -54.89453521545159731 ) ) ;
#16281 = DIRECTION ( 'NONE',  ( 1.000000000000000000, 0.000000000000000000, 0.000000000000000000 ) ) ;
#16282 = CARTESIAN_POINT ( 'NONE',  ( 22.90093739391126348, -16.50198413763800431, -70.49448988769137259 ) ) ;
#16283 = CARTESIAN_POINT ( 'NONE',  ( 56.39270695421159729, 19.29512507422779777, -52.86271299482670116 ) ) ;
#16284 = CARTESIAN_POINT ( 'NONE',  ( 71.46564822584178955, 0.9966178393190270324, -60.66877295535580572 ) ) ;
#16285 = LINE ( 'NONE', #32491, #18296 ) ;
#16286 = CARTESIAN_POINT ( 'NONE',  ( 71.79848734841181113, 0.9405967369903619479, -60.89823624368939647 ) ) ;
#16287 = CARTESIAN_POINT ( 'NONE',  ( 24.04493430405305787, -15.62427045307345530, -71.50799773700714468 ) ) ;
#16288 = CARTESIAN_POINT ( 'NONE',  ( 64.92606658240281092, 0.9214125008369580261, -70.72054727061200197 ) ) ;
#16289 = ORIENTED_EDGE ( 'NONE', *, *, #40885, .F. ) ;
#16290 = ORIENTED_EDGE ( 'NONE', *, *, #7509, .T. ) ;
#16291 = CIRCLE ( 'NONE', #37249, 2.576499999999998902 ) ;
#16292 = CARTESIAN_POINT ( 'NONE',  ( 72.33393739769915953, 11.38368607098440499, -61.44999999999753015 ) ) ;
#16293 = FACE_BOUND ( 'NONE', #10438, .T. ) ;
#16294 = VERTEX_POINT ( 'NONE', #23023 ) ;
#16295 = CARTESIAN_POINT ( 'NONE',  ( 12.14971906056685924, -8.703714936188482909, -58.84096898769573869 ) ) ;
#16296 = CARTESIAN_POINT ( 'NONE',  ( 11.00289117509757553, -11.15506890091918457, -49.68074223147661428 ) ) ;
#16297 = ORIENTED_EDGE ( 'NONE', *, *, #43095, .F. ) ;
#16298 = DIRECTION ( 'NONE',  ( 0.9313175168445364527, 0.3616257875448561365, 0.04329517988286096797 ) ) ;
#16299 = CARTESIAN_POINT ( 'NONE',  ( 42.30872906436815128, 6.440492890468437537, -78.77604134614341547 ) ) ;
#16300 = CARTESIAN_POINT ( 'NONE',  ( 19.17739448125563584, -22.99139521707102318, -65.88280214780220945 ) ) ;
#16301 = EDGE_CURVE ( 'NONE', #41415, #3035, #23702, .T. ) ;
#16302 = CARTESIAN_POINT ( 'NONE',  ( 23.84659521662570114, -18.53125831332900120, -45.90735674562579760 ) ) ;
#16303 = EDGE_CURVE ( 'NONE', #20524, #29117, #10227, .T. ) ;
#16304 = CARTESIAN_POINT ( 'NONE',  ( 9.807787300107081663, -20.47788638414121820, -68.29933457388374052 ) ) ;
#16305 = AXIS2_PLACEMENT_3D ( 'NONE', #14463, #46457, #14980 ) ;
#16306 = CARTESIAN_POINT ( 'NONE',  ( 42.22142201539555373, -37.65884987249721405, -79.21256181789661355 ) ) ;
#16307 = B_SPLINE_CURVE_WITH_KNOTS ( 'NONE', 3,
 ( #29731, #48642, #41027, #936, #36566, #41543 ),
 .UNSPECIFIED., .F., .F.,
 ( 4, 1, 1, 4 ),
 ( 0.000000000000000000, 0.3333333332445770347, 0.6666666664890291694, 1.000000000000000000 ),
 .UNSPECIFIED. ) ;
#16308 = EDGE_CURVE ( 'NONE', #48268, #32800, #51087, .T. ) ;
#16309 = ORIENTED_EDGE ( 'NONE', *, *, #37930, .F. ) ;
#16310 = CARTESIAN_POINT ( 'NONE',  ( 10.65234009212060151, -63.87410165361089298, -23.62431477846339689 ) ) ;
#16311 = CARTESIAN_POINT ( 'NONE',  ( 19.48351169319580123, -22.27104024610400046, -38.58422730669299483 ) ) ;
#16312 = CARTESIAN_POINT ( 'NONE',  ( 44.99439540629440160, 14.59120791265710082, -8.742832391549649529 ) ) ;
#16313 = CARTESIAN_POINT ( 'NONE',  ( 14.15413451811019918, 20.61624280354940097, -75.59143512441710300 ) ) ;
#16314 = CARTESIAN_POINT ( 'NONE',  ( 16.78922646229311511, -23.56772248962323246, -60.26586126249986819 ) ) ;
#16315 =( BOUNDED_CURVE ( )  B_SPLINE_CURVE ( 3, ( #7818, #3889, #23771, #15166 ),
 .UNSPECIFIED., .F., .T. ) 
 B_SPLINE_CURVE_WITH_KNOTS ( ( 4, 4 ),
 ( 5.907914484323606885, 5.977569058052071505 ),
 .UNSPECIFIED. ) 
 CURVE ( )  GEOMETRIC_REPRESENTATION_ITEM ( )  RATIONAL_B_SPLINE_CURVE ( ( 1.000000000000000000, 0.9995957275622183724, 0.9995957275622183724, 1.000000000000000000 ) ) 
 REPRESENTATION_ITEM ( '' )  );
#16316 = CARTESIAN_POINT ( 'NONE',  ( 82.88019469981989573, -45.12199509848900192, -46.94529082815019194 ) ) ;
#16317 = CARTESIAN_POINT ( 'NONE',  ( 24.04527307164895333, -15.61618901697373119, -57.79233174308600951 ) ) ;
#16318 = CARTESIAN_POINT ( 'NONE',  ( 8.895242482623048730, -11.66852930440259861, -44.66659110805180433 ) ) ;
#16319 = EDGE_CURVE ( 'NONE', #38732, #20276, #28725, .T. ) ;
#16320 = ORIENTED_EDGE ( 'NONE', *, *, #11528, .F. ) ;
#16321 = CARTESIAN_POINT ( 'NONE',  ( 53.24319873876810050, -49.24894743539400110, -27.32017878002559996 ) ) ;
#16322 = VECTOR ( 'NONE', #27648, 1000.000000000000114 ) ;
#16323 = CARTESIAN_POINT ( 'NONE',  ( 15.10819245919740084, -50.76188580677340667, -20.77789291004060246 ) ) ;
#16324 = CARTESIAN_POINT ( 'NONE',  ( 50.30446722783852920, -36.40950912720241917, -76.16831878770071285 ) ) ;
#16325 = CARTESIAN_POINT ( 'NONE',  ( 20.99566134352006586, -21.94231754292628267, -64.08399974622017226 ) ) ;
#16326 = CARTESIAN_POINT ( 'NONE',  ( 21.54526434311726746, -19.77485224925768037, -56.66111849060637695 ) ) ;
#16327 = CARTESIAN_POINT ( 'NONE',  ( 12.28937802692940018, -50.00765210412139794, -21.14656546108620105 ) ) ;
#16328 = ORIENTED_EDGE ( 'NONE', *, *, #11092, .T. ) ;
#16329 = CARTESIAN_POINT ( 'NONE',  ( -7.625187662226220020, -45.45404276017920608, -5.684751090845729493 ) ) ;
#16330 = CARTESIAN_POINT ( 'NONE',  ( 47.43160242963380568, 23.39460843266559920, -54.67048143933339333 ) ) ;
#16331 = CARTESIAN_POINT ( 'NONE',  ( 12.72604749850384032, -21.52915785728961851, -49.11948754903311709 ) ) ;
#16332 = CARTESIAN_POINT ( 'NONE',  ( 63.11571638736320011, 0.9242073871622918935, -62.36095669330580193 ) ) ;
#16333 = CARTESIAN_POINT ( 'NONE',  ( 12.82931922587579976, 19.41533729766869953, -21.34049584734400185 ) ) ;
#16334 = CARTESIAN_POINT ( 'NONE',  ( 72.33393739769618946, 1.383811055320669947, -68.84999999999999432 ) ) ;
#16335 = CARTESIAN_POINT ( 'NONE',  ( 41.75077269581309736, 13.19527022550269990, -5.046632968629480409 ) ) ;
#16336 = DIRECTION ( 'NONE',  ( 1.000000000000000000, 0.000000000000000000, 0.000000000000000000 ) ) ;
#16337 = CARTESIAN_POINT ( 'NONE',  ( 60.31639983755060541, -45.83544975381190056, -47.65366050515999774 ) ) ;
#16338 = CARTESIAN_POINT ( 'NONE',  ( 68.13393739769841773, -50.61618894467878960, -73.25000000000220268 ) ) ;
#16339 = CARTESIAN_POINT ( 'NONE',  ( 64.68494473060239613, 1.102139304147779830, -60.78391614187979997 ) ) ;
#16340 = CARTESIAN_POINT ( 'NONE',  ( 17.21347160910390173, -53.11618894467930119, -76.14999999999999147 ) ) ;
#16341 = CARTESIAN_POINT ( 'NONE',  ( 23.04647718490594599, -11.63208852034076202, -73.34100123405998772 ) ) ;
#16342 = CARTESIAN_POINT ( 'NONE',  ( 53.39190020003140091, -49.64277996747850352, -49.50885269097420149 ) ) ;
#16343 = EDGE_LOOP ( 'NONE', ( #12171, #26111, #7114, #15838 ) ) ;
#16344 = FACE_OUTER_BOUND ( 'NONE', #7472, .T. ) ;
#16345 = CARTESIAN_POINT ( 'NONE',  ( 10.14520404402119880, 32.04273756952679975, -45.99312054747319678 ) ) ;
#16346 = CARTESIAN_POINT ( 'NONE',  ( 22.86366527778791280, -16.34140995983870681, -34.48697822539197944 ) ) ;
#16347 = CARTESIAN_POINT ( 'NONE',  ( 9.254905727752488431, -13.06732500719120083, -81.23899999999999011 ) ) ;
#16348 = VERTEX_POINT ( 'NONE', #47171 ) ;
#16349 = CARTESIAN_POINT ( 'NONE',  ( 18.11674004330059873, 20.32108400380180058, -75.32473453343510528 ) ) ;
#16350 = VERTEX_POINT ( 'NONE', #46915 ) ;
#16351 = VERTEX_POINT ( 'NONE', #10741 ) ;
#16352 = ORIENTED_EDGE ( 'NONE', *, *, #50149, .T. ) ;
#16353 = FACE_OUTER_BOUND ( 'NONE', #2320, .T. ) ;
#16354 = CYLINDRICAL_SURFACE ( 'NONE', #32779, 2.000000000000000000 ) ;
#16355 = CARTESIAN_POINT ( 'NONE',  ( 11.27232706326269884, -9.289972531400195521, -62.79933563852407730 ) ) ;
#16356 = CARTESIAN_POINT ( 'NONE',  ( 61.75019923867180438, 13.88381043675840054, -46.43277563447490053 ) ) ;
#16357 = B_SPLINE_CURVE_WITH_KNOTS ( 'NONE', 3,
 ( #35333, #51585, #3636, #34552, #31128, #42702, #10470, #6799, #22751, #51332, #14906, #2863, #14648, #15432, #31383, #43465, #22493, #18828 ),
 .UNSPECIFIED., .F., .F.,
 ( 4, 2, 2, 2, 2, 2, 2, 2, 4 ),
 ( 0.000000000000000000, 0.06249981704674846539, 0.1249996340934969308, 0.1874994511402454100, 0.2499992681869938616, 0.3124990852337423131, 0.3749989022804908201, 0.4374987193272392716, 0.4999985363739877231 ),
 .UNSPECIFIED. ) ;
#16358 = EDGE_LOOP ( 'NONE', ( #19539, #30567, #38133, #10358 ) ) ;
#16359 = CARTESIAN_POINT ( 'NONE',  ( 75.29334099864146879, 5.095336761201883391, -12.50187872901068964 ) ) ;
#16360 = CIRCLE ( 'NONE', #29737, 3.000000000000001776 ) ;
#16361 = CARTESIAN_POINT ( 'NONE',  ( 22.90100569266936148, -15.61618883250986300, -34.84718217067427304 ) ) ;
#16362 = ORIENTED_EDGE ( 'NONE', *, *, #799, .T. ) ;
#16363 = CARTESIAN_POINT ( 'NONE',  ( 50.20833736503800537, -46.19202927519189927, -12.60658152119249920 ) ) ;
#16364 = AXIS2_PLACEMENT_3D ( 'NONE', #1557, #6011, #48747 ) ;
#16365 = EDGE_CURVE ( 'NONE', #2651, #41542, #2621, .T. ) ;
#16366 = DIRECTION ( 'NONE',  ( -1.822422554782380175E-11, -1.784227544494129940E-11, -1.000000000000000000 ) ) ;
#16367 = EDGE_CURVE ( 'NONE', #9892, #12485, #3457, .T. ) ;
#16368 = ORIENTED_EDGE ( 'NONE', *, *, #19142, .F. ) ;
#16369 = VERTEX_POINT ( 'NONE', #18076 ) ;
#16370 = CARTESIAN_POINT ( 'NONE',  ( -8.766062602303898998, -15.61618894467929941, 8.450000000000024158 ) ) ;
#16371 = CARTESIAN_POINT ( 'NONE',  ( 21.50893739769619728, 1.920825481955539926, -35.14999999999999858 ) ) ;
#16372 = CARTESIAN_POINT ( 'NONE',  ( 60.81833024471840332, 14.35563499692709932, -47.52759458687679484 ) ) ;
#16373 = CARTESIAN_POINT ( 'NONE',  ( 51.26921915167240229, 14.36187956967640034, -12.86592481132139909 ) ) ;
#16374 = DIRECTION ( 'NONE',  ( -1.000000000000000000, -1.004313591354993529E-15, 0.000000000000000000 ) ) ;
#16375 = CARTESIAN_POINT ( 'NONE',  ( -6.133771980677649616, 15.17810994771089916, -4.670463077492210680 ) ) ;
#16376 = DIRECTION ( 'NONE',  ( 0.6339889056055382222, 0.000000000000000000, -0.7733421413379021336 ) ) ;
#16377 = CARTESIAN_POINT ( 'NONE',  ( 55.91595717589669334, 14.67227259378219983, -17.93019253464870033 ) ) ;
#16378 = CARTESIAN_POINT ( 'NONE',  ( 14.95417985139190087, -23.37472748715750015, -65.83553959257810106 ) ) ;
#16379 = EDGE_CURVE ( 'NONE', #30000, #45437, #19999, .T. ) ;
#16380 = ORIENTED_EDGE ( 'NONE', *, *, #2724, .F. ) ;
#16381 = CARTESIAN_POINT ( 'NONE',  ( 52.56521993351449851, -49.86179673305689874, -28.15000000000000213 ) ) ;
#16382 = CARTESIAN_POINT ( 'NONE',  ( 23.53017837589169048, -48.93815596428016335, -34.78557451168259718 ) ) ;
#16383 = CARTESIAN_POINT ( 'NONE',  ( 12.25380415244200094, 34.08744772712660165, -46.27199321433290180 ) ) ;
#16384 = PRODUCT_DEFINITION_CONTEXT ( 'detailed design', #16716, 'design' ) ;
#16385 = EDGE_CURVE ( 'NONE', #50858, #2213, #34044, .T. ) ;
#16386 = CARTESIAN_POINT ( 'NONE',  ( 72.59802144691040837, 1.334524132314419909, -69.46667700706710491 ) ) ;
#16387 = CARTESIAN_POINT ( 'NONE',  ( 42.67110578209099714, -39.83399799466496205, -73.09004855766275455 ) ) ;
#16388 = CARTESIAN_POINT ( 'NONE',  ( 10.87995450790350205, -64.97548900853969656, -17.51161086048150040 ) ) ;
#16389 = CARTESIAN_POINT ( 'NONE',  ( 12.27824370503539875, 18.91995526668989669, -21.14999999870460101 ) ) ;
#16390 = CARTESIAN_POINT ( 'NONE',  ( 46.80616873440099823, 22.71927177964060007, -75.82639822421660369 ) ) ;
#16391 = CARTESIAN_POINT ( 'NONE',  ( 48.68378925563050075, -54.05006251182930299, -54.91526356565999833 ) ) ;
#16392 = AXIS2_PLACEMENT_3D ( 'NONE', #47039, #35478, #26564 ) ;
#16393 = LINE ( 'NONE', #40758, #17269 ) ;
#16394 = DIRECTION ( 'NONE',  ( -1.000000000000000000, 4.735514272306495889E-33, 9.834501533011742432E-16 ) ) ;
#16395 = CARTESIAN_POINT ( 'NONE',  ( 8.222957392148765976, -16.65188279910073987, -38.46600194893341040 ) ) ;
#16396 = DIRECTION ( 'NONE',  ( 1.000000000000000000, 0.000000000000000000, 0.000000000000000000 ) ) ;
#16397 = VERTEX_POINT ( 'NONE', #19367 ) ;
#16398 = CARTESIAN_POINT ( 'NONE',  ( 19.16281492688910149, -22.42299401398249969, -43.43407599211369075 ) ) ;
#16399 = CARTESIAN_POINT ( 'NONE',  ( 64.66082326855099893, 1.024253516290730026, -60.76832953309080665 ) ) ;
#16400 = ORIENTED_EDGE ( 'NONE', *, *, #389, .F. ) ;
#16401 = CYLINDRICAL_SURFACE ( 'NONE', #783, 0.4999999999999983347 ) ;
#16402 = CARTESIAN_POINT ( 'NONE',  ( 60.69273398595009894, -45.54451186045000100, -47.19142213667469576 ) ) ;
#16403 = CARTESIAN_POINT ( 'NONE',  ( 10.40721626785641440, -10.10600253351913480, -81.03610924078645894 ) ) ;
#16404 = CARTESIAN_POINT ( 'NONE',  ( 12.86222958136720074, 18.76465491334460012, -21.07385132223840074 ) ) ;
#16406 = DIRECTION ( 'NONE',  ( 0.000000000000000000, -1.000000000000000000, 0.000000000000000000 ) ) ;
#16405 = CARTESIAN_POINT ( 'NONE',  ( 42.55931733926811233, 8.590583294249910296, -73.62972220888975983 ) ) ;
#16407 = CARTESIAN_POINT ( 'NONE',  ( 29.75529164732110132, 4.407650919513039334, -84.61197749185016903 ) ) ;
#16408 = CYLINDRICAL_SURFACE ( 'NONE', #19419, 0.4999999999999982236 ) ;
#16409 = ORIENTED_EDGE ( 'NONE', *, *, #44531, .F. ) ;
#16410 = CARTESIAN_POINT ( 'NONE',  ( 83.01976156432699838, -45.38357736965039635, -47.45812318453789658 ) ) ;
#16411 = VERTEX_POINT ( 'NONE', #43483 ) ;
#16412 = VERTEX_POINT ( 'NONE', #16207 ) ;
#16413 = ORIENTED_EDGE ( 'NONE', *, *, #39575, .F. ) ;
#16414 = CARTESIAN_POINT ( 'NONE',  ( 61.51109188950590578, -45.14456777294489598, -46.47690995681890058 ) ) ;
#16415 = CARTESIAN_POINT ( 'NONE',  ( 52.58812961169699918, -49.84012128000139796, -48.57103837950110403 ) ) ;
#16416 = CARTESIAN_POINT ( 'NONE',  ( 12.08165151496428713, -55.41053553174391055, -22.62766840197337714 ) ) ;
#16417 = CARTESIAN_POINT ( 'NONE',  ( 76.44536772384181234, -6.686551103978267463, -12.99199962697529998 ) ) ;
#16418 = CARTESIAN_POINT ( 'NONE',  ( 22.90122453025153249, -15.61618899996915211, -58.45282045073077626 ) ) ;
#16419 = CIRCLE ( 'NONE', #6406, 5.499999999999998224 ) ;
#16420 = VERTEX_POINT ( 'NONE', #7326 ) ;
#16421 = ORIENTED_EDGE ( 'NONE', *, *, #45568, .T. ) ;
#16422 = CARTESIAN_POINT ( 'NONE',  ( -0.2999272097369983237, 14.12533709486001499, -35.02742413524038767 ) ) ;
#16423 = TOROIDAL_SURFACE ( 'NONE', #44784, 5.500000000000000000, 0.5000000000000000000 ) ;
#16424 = CARTESIAN_POINT ( 'NONE',  ( 0.1457841021255935343, -22.91266753744946527, -34.68167779225149161 ) ) ;
#16425 = CARTESIAN_POINT ( 'NONE',  ( 56.27102574643829769, -50.57722701405970156, -52.87266565438959987 ) ) ;
#16426 = EDGE_CURVE ( 'NONE', #16669, #49951, #12500, .T. ) ;
#16427 = CARTESIAN_POINT ( 'NONE',  ( 22.72481302096315403, -13.84495347910004881, -36.36948437006035562 ) ) ;
#16428 = CARTESIAN_POINT ( 'NONE',  ( 23.79191524431698213, -13.56499663094212949, -59.70900831695890787 ) ) ;
#16429 = CARTESIAN_POINT ( 'NONE',  ( 61.28398356449380202, -45.60471458446119897, -47.68178229846480320 ) ) ;
#16430 = ORIENTED_EDGE ( 'NONE', *, *, #2281, .T. ) ;
#16431 = CYLINDRICAL_SURFACE ( 'NONE', #40040, 0.4999999999999993894 ) ;
#16432 = CARTESIAN_POINT ( 'NONE',  ( 52.23775024128120492, -49.82363818699889890, -77.10775516233969995 ) ) ;
#16433 = CARTESIAN_POINT ( 'NONE',  ( 60.23889825737600745, 14.54821815915974703, -47.30579064662337885 ) ) ;
#16434 = CARTESIAN_POINT ( 'NONE',  ( 11.27233804322889199, -21.94241366705713148, -54.21600271639588442 ) ) ;
#16435 = CIRCLE ( 'NONE', #24790, 40.00000000000000711 ) ;
#16436 = CARTESIAN_POINT ( 'NONE',  ( 16.18108977866110010, -7.768608155381779845, -51.51440696060279834 ) ) ;
#16437 = AXIS2_PLACEMENT_3D ( 'NONE', #51729, #24169, #36502 ) ;
#16438 = DIRECTION ( 'NONE',  ( 0.000000000000000000, 0.000000000000000000, 1.000000000000000000 ) ) ;
#16439 = CARTESIAN_POINT ( 'NONE',  ( 41.23309865046339695, -44.72123908719060381, -5.265645747893140438 ) ) ;
#16440 = CARTESIAN_POINT ( 'NONE',  ( 15.67962062493140074, -50.86266781791879765, -20.15000000000000213 ) ) ;
#16441 = CYLINDRICAL_SURFACE ( 'NONE', #34052, 6.100000000000001421 ) ;
#16442 = CYLINDRICAL_SURFACE ( 'NONE', #26249, 1.000000000000003775 ) ;
#16443 = CARTESIAN_POINT ( 'NONE',  ( 15.12242003932709977, -22.59611672426049722, -49.39298971242499192 ) ) ;
#16444 = CARTESIAN_POINT ( 'NONE',  ( 18.38332337263111427, -52.17615710686938968, -75.56421430878999956 ) ) ;
#16445 = EDGE_LOOP ( 'NONE', ( #2247, #44192, #24252, #24120 ) ) ;
#16446 = CARTESIAN_POINT ( 'NONE',  ( 14.43104019203130051, -52.03647206054819918, -75.81086730487160708 ) ) ;
#16447 = CARTESIAN_POINT ( 'NONE',  ( 47.23375364729769643, -54.76822368793749973, -54.67325007366670064 ) ) ;
#16448 = FACE_OUTER_BOUND ( 'NONE', #3674, .T. ) ;
#16449 = EDGE_CURVE ( 'NONE', #434, #49131, #39448, .T. ) ;
#16450 = CARTESIAN_POINT ( 'NONE',  ( 9.366933260303092368, -14.73042100787367481, -37.49448701325534472 ) ) ;
#16451 = CARTESIAN_POINT ( 'NONE',  ( 84.22672017751912676, 12.55805222647083497, -46.99906225624759770 ) ) ;
#16452 = DIRECTION ( 'NONE',  ( 0.000000000000000000, 0.000000000000000000, -1.000000000000000000 ) ) ;
#16453 = CIRCLE ( 'NONE', #44937, 0.4905819419822178840 ) ;
#16454 = CARTESIAN_POINT ( 'NONE',  ( 55.48509142758890533, -46.00752295928280233, -16.66509390011597702 ) ) ;
#16456 = CARTESIAN_POINT ( 'NONE',  ( 17.16955932200438184, -23.52717831220308753, -73.96600144092269602 ) ) ;
#16455 = CARTESIAN_POINT ( 'NONE',  ( 61.31807988003849630, -45.64188066314479642, -47.72348187468949732 ) ) ;
#16457 = FACE_BOUND ( 'NONE', #3807, .T. ) ;
#16458 = CARTESIAN_POINT ( 'NONE',  ( 48.68901951993020560, 22.76098662308300291, -54.71436045317769725 ) ) ;
#16459 = ORIENTED_EDGE ( 'NONE', *, *, #513, .F. ) ;
#16460 = CARTESIAN_POINT ( 'NONE',  ( 52.63212581583610472, -49.79676770012090259, -48.50959626792249679 ) ) ;
#16461 = EDGE_LOOP ( 'NONE', ( #27008, #50407, #6377, #48421 ) ) ;
#16462 = DIRECTION ( 'NONE',  ( 0.000000000000000000, 1.000000000000000000, 0.000000000000000000 ) ) ;
#16463 = CARTESIAN_POINT ( 'NONE',  ( 14.13393739769619906, -41.61618894467930119, -35.14999999999999858 ) ) ;
#16464 = DIRECTION ( 'NONE',  ( 0.000000000000000000, 0.000000000000000000, 1.000000000000000000 ) ) ;
#16466 = CARTESIAN_POINT ( 'NONE',  ( 55.77169211825290063, 15.03234804280600123, -25.85730881726700048 ) ) ;
#16465 = CARTESIAN_POINT ( 'NONE',  ( 84.38939444912799104, 12.25052432195479923, -47.32729711157580255 ) ) ;
#16467 = CARTESIAN_POINT ( 'NONE',  ( 17.13287240097439934, -22.59792852417169939, -68.90758401351929763 ) ) ;
#16468 = CARTESIAN_POINT ( 'NONE',  ( 52.57890692814670075, 18.61498511809359968, -48.49302657703999841 ) ) ;
#16469 = CARTESIAN_POINT ( 'NONE',  ( 55.65085491148499841, -45.30818602241870252, -15.56796338809930091 ) ) ;
#16470 = CARTESIAN_POINT ( 'NONE',  ( -31.36606260230380272, 31.88381105532069881, 17.35000000000000142 ) ) ;
#16471 = VERTEX_POINT ( 'NONE', #7840 ) ;
#16472 = B_SPLINE_CURVE_WITH_KNOTS ( 'NONE', 3,
 ( #27209, #43221, #23779, #35603, #27975, #11509, #27467, #31642, #3641, #3899 ),
 .UNSPECIFIED., .F., .F.,
 ( 4, 2, 2, 2, 4 ),
 ( 0.000000000000000000, 0.3550177484190761845, 0.6750337469940175250, 0.8750437461033545583, 1.000000000000000000 ),
 .UNSPECIFIED. ) ;
#16473 = ORIENTED_EDGE ( 'NONE', *, *, #5162, .F. ) ;
#16474 = CARTESIAN_POINT ( 'NONE',  ( 11.84416398830530071, -65.08858756582790761, -16.58498012168669788 ) ) ;
#16475 = CARTESIAN_POINT ( 'NONE',  ( 12.85003218997280072, 34.27383497643789667, -47.67045162685929682 ) ) ;
#16476 = CARTESIAN_POINT ( 'NONE',  ( 18.86789271246039945, 20.55440458018300021, -15.81497037201279987 ) ) ;
#16477 = CARTESIAN_POINT ( 'NONE',  ( 68.13393739769618662, -30.66618894467940137, -65.65000000000000568 ) ) ;
#16478 = CARTESIAN_POINT ( 'NONE',  ( 10.97349868895814318, -64.80942964233447867, -23.22353997969214845 ) ) ;
#16479 = DIRECTION ( 'NONE',  ( 8.604228440844980354E-13, 0.9739538916850960515, -0.2267461507312888980 ) ) ;
#16480 = ORIENTED_EDGE ( 'NONE', *, *, #50363, .T. ) ;
#16481 = CARTESIAN_POINT ( 'NONE',  ( 20.11802023908898818, -8.703636772384703235, -75.17430357709265820 ) ) ;
#16482 = CARTESIAN_POINT ( 'NONE',  ( 11.10543711150969948, -63.21940129908220030, -44.25051057170020385 ) ) ;
#16483 = VECTOR ( 'NONE', #19081, 1000.000000000000000 ) ;
#16484 = EDGE_CURVE ( 'NONE', #7979, #16490, #27642, .T. ) ;
#16485 = CARTESIAN_POINT ( 'NONE',  ( 8.428833774104951715, -17.68685544396012688, -60.42434371803280158 ) ) ;
#16486 = CARTESIAN_POINT ( 'NONE',  ( 18.13393739769630031, 0.3838110553206460218, -34.64999999999999858 ) ) ;
#16487 = FACE_OUTER_BOUND ( 'NONE', #37669, .T. ) ;
#16488 = EDGE_CURVE ( 'NONE', #50414, #7343, #224, .T. ) ;
#16489 = CARTESIAN_POINT ( 'NONE',  ( 18.20462312208350397, -23.32128729342234763, -43.92436229106515810 ) ) ;
#16490 = VERTEX_POINT ( 'NONE', #16463 ) ;
#16491 = ADVANCED_FACE ( 'NONE', ( #12284 ), #35866, .F. ) ;
#16492 = DIRECTION ( 'NONE',  ( -0.6047562208151069374, 0.7964106436917012255, 0.000000000000000000 ) ) ;
#16493 = CARTESIAN_POINT ( 'NONE',  ( 56.66762828736870006, -50.37953306433199430, -52.77094437832339935 ) ) ;
#16494 = CARTESIAN_POINT ( 'NONE',  ( 56.42249077807360180, 19.27081265489739792, -52.83600065022080372 ) ) ;
#16495 = EDGE_CURVE ( 'NONE', #29027, #31864, #7647, .T. ) ;
#16496 = CARTESIAN_POINT ( 'NONE',  ( 10.24818704271000058, -9.842051535964911224, -69.03928461620270696 ) ) ;
#16497 = CARTESIAN_POINT ( 'NONE',  ( 11.53605495837543948, -55.35105376503654639, -21.73576846289474318 ) ) ;
#16498 = CARTESIAN_POINT ( 'NONE',  ( 54.35193248541229849, 19.95680887633289657, -75.41416007314899161 ) ) ;
#16499 = CARTESIAN_POINT ( 'NONE',  ( 46.68683961171959851, -53.36165723267750138, -76.07661161287319374 ) ) ;
#16500 = EDGE_LOOP ( 'NONE', ( #15840, #49765, #45044, #501, #49029, #11378 ) ) ;
#16501 = CARTESIAN_POINT ( 'NONE',  ( 21.24562006453919949, -10.19609723709329963, -59.97333869387029637 ) ) ;
#16502 = CARTESIAN_POINT ( 'NONE',  ( 52.67142628424050343, -49.78173758010149896, -48.75814597207470058 ) ) ;
#16503 = AXIS2_PLACEMENT_3D ( 'NONE', #24872, #20954, #31964 ) ;
#16504 = LINE ( 'NONE', #16248, #9673 ) ;
#16505 = DIRECTION ( 'NONE',  ( 1.000000000000000000, 0.000000000000000000, 0.000000000000000000 ) ) ;
#16506 = CARTESIAN_POINT ( 'NONE',  ( 46.37528053896889446, 21.71340314309550124, -76.14999999999999147 ) ) ;
#16507 = CARTESIAN_POINT ( 'NONE',  ( 19.21160129066574740, -52.77196524774721809, -16.16879274230204899 ) ) ;
#16508 = EDGE_CURVE ( 'NONE', #19900, #1406, #36368, .T. ) ;
#16509 = CARTESIAN_POINT ( 'NONE',  ( 58.91181031229810117, 15.24198406853699872, -47.44472854892460134 ) ) ;
#16510 = DIRECTION ( 'NONE',  ( -1.000000000000000000, 0.000000000000000000, 0.000000000000000000 ) ) ;
#16511 = CARTESIAN_POINT ( 'NONE',  ( 10.73767760254780157, -21.85021661002049953, -72.23477911819139763 ) ) ;
#16512 = DIRECTION ( 'NONE',  ( 0.000000000000000000, 0.000000000000000000, -1.000000000000000000 ) ) ;
#16514 = DIRECTION ( 'NONE',  ( -9.408764999999898798E-18, 1.274833000000000002E-16, 1.000000000000000000 ) ) ;
#16513 = DIRECTION ( 'NONE',  ( -1.000000000000000000, 0.000000000000000000, 0.000000000000000000 ) ) ;
#16515 = CARTESIAN_POINT ( 'NONE',  ( 63.39147977162330960, 1.370118064600899910, -68.71049874078630637 ) ) ;
#16516 = CARTESIAN_POINT ( 'NONE',  ( 61.50836220838129975, 13.91397026120830027, -46.46408765477929848 ) ) ;
#16517 = CARTESIAN_POINT ( 'NONE',  ( 20.11809781826896781, -8.703683167413712951, -79.17433641915961573 ) ) ;
#16518 = CARTESIAN_POINT ( 'NONE',  ( -17.94291051752670185, -51.49525275629270027, -52.69725456403789821 ) ) ;
#16519 = EDGE_LOOP ( 'NONE', ( #37767, #46603, #18942, #9594 ) ) ;
#16520 = CARTESIAN_POINT ( 'NONE',  ( 53.13663702127480093, -49.50013705438340139, -48.80285956223989530 ) ) ;
#16521 = EDGE_CURVE ( 'NONE', #4162, #7979, #476, .T. ) ;
#16522 = CARTESIAN_POINT ( 'NONE',  ( 57.98146860794130220, -45.12919884128839954, -25.62231485056000224 ) ) ;
#16523 = LINE ( 'NONE', #28305, #45273 ) ;
#16524 = CARTESIAN_POINT ( 'NONE',  ( 57.38644999245990164, 14.57387751478819915, -26.27655890715150022 ) ) ;
#16525 = CARTESIAN_POINT ( 'NONE',  ( 9.788246253542011388, -12.53807871279539832, -39.59657951998019598 ) ) ;
#16526 = CARTESIAN_POINT ( 'NONE',  ( 51.38510966839819361, 18.87816813940790439, -76.33916217765379031 ) ) ;
#16527 = CARTESIAN_POINT ( 'NONE',  ( 52.88917638043529479, 18.40237379729330058, -48.82176621297229246 ) ) ;
#16528 = CARTESIAN_POINT ( 'NONE',  ( 71.30079129029560647, 1.267233196669030004, -70.54626486029009413 ) ) ;
#16529 = CARTESIAN_POINT ( 'NONE',  ( 46.35275103504439898, 21.67755452994670406, -76.14999999999999147 ) ) ;
#16530 = CARTESIAN_POINT ( 'NONE',  ( 64.44836340493399973, -45.11618894467940066, -12.01833907808290114 ) ) ;
#16531 = ORIENTED_EDGE ( 'NONE', *, *, #8613, .F. ) ;
#16532 = CARTESIAN_POINT ( 'NONE',  ( 63.43393739769620510, 0.8838110553206759423, -62.79342862858290886 ) ) ;
#16533 = CARTESIAN_POINT ( 'NONE',  ( 47.58415360336899624, -54.56008480908929670, -55.08758729138420307 ) ) ;
#16534 = CARTESIAN_POINT ( 'NONE',  ( -6.140345868814909736, 15.17335822560399983, -4.613862305479059955 ) ) ;
#16535 = CARTESIAN_POINT ( 'NONE',  ( 40.64814283787880100, 13.41987867678509971, -4.018323132419280519 ) ) ;
#16536 = CARTESIAN_POINT ( 'NONE',  ( 57.35949929755079779, 19.07198536079580364, -52.80982651506389658 ) ) ;
#16537 = CARTESIAN_POINT ( 'NONE',  ( 71.42224537953511287, 1.096044978595160035, -60.67935125044880351 ) ) ;
#16538 = CARTESIAN_POINT ( 'NONE',  ( 16.65420337844999921, -51.11618894467930119, -20.15000000000000213 ) ) ;
#16539 = CARTESIAN_POINT ( 'NONE',  ( 71.69810449264960539, 1.236214136008269904, -60.94130379687539545 ) ) ;
#16540 = AXIS2_PLACEMENT_3D ( 'NONE', #48425, #12267, #20364 ) ;
#16541 = DIRECTION ( 'NONE',  ( 0.5320619775582980937, 0.8460488748893841837, -0.03333696649607501700 ) ) ;
#16542 = CARTESIAN_POINT ( 'NONE',  ( 65.27736602627911111, 1.383811055320669947, -70.34999999999999432 ) ) ;
#16543 = ORIENTED_EDGE ( 'NONE', *, *, #3732, .F. ) ;
#16544 = VERTEX_POINT ( 'NONE', #23273 ) ;
#16545 = CARTESIAN_POINT ( 'NONE',  ( 14.12233147434080038, -51.14020415405890674, -22.75736350782009865 ) ) ;
#16546 = AXIS2_PLACEMENT_3D ( 'NONE', #17647, #44640, #48843 ) ;
#16547 = CARTESIAN_POINT ( 'NONE',  ( 15.83040942711627963, -50.94062305526537671, -15.66031378978091304 ) ) ;
#16548 = VERTEX_POINT ( 'NONE', #24301 ) ;
#16549 = DIRECTION ( 'NONE',  ( 0.8889875008987390137, -0.4579314612972278375, 0.000000000000000000 ) ) ;
#16550 = CARTESIAN_POINT ( 'NONE',  ( 57.39214507209349847, -45.11761009216159835, -25.32322608115779872 ) ) ;
#16551 = DIRECTION ( 'NONE',  ( 1.000000000000000000, 0.000000000000000000, 0.000000000000000000 ) ) ;
#16552 = ORIENTED_EDGE ( 'NONE', *, *, #31136, .T. ) ;
#16553 = FACE_OUTER_BOUND ( 'NONE', #30006, .T. ) ;
#16554 = CARTESIAN_POINT ( 'NONE',  ( 11.94575855162158895, -10.22828773375895750, -71.74277772556011712 ) ) ;
#16555 = CARTESIAN_POINT ( 'NONE',  ( 61.25346184070040323, 14.37618061013010085, -47.68486562037010401 ) ) ;
#16556 = EDGE_CURVE ( 'NONE', #10857, #49956, #2634, .T. ) ;
#16557 = CARTESIAN_POINT ( 'NONE',  ( 24.36831978584559977, -16.03769427284349902, -47.80861109115269869 ) ) ;
#16558 = CARTESIAN_POINT ( 'NONE',  ( 11.27227490617820749, -21.94236589989201747, -68.21600100673204281 ) ) ;
#16559 = CARTESIAN_POINT ( 'NONE',  ( 41.92858229088276545, -37.61218635125683107, -80.67670930047889044 ) ) ;
#16560 =( LENGTH_UNIT ( ) NAMED_UNIT ( * ) SI_UNIT ( .MILLI., .METRE. ) );
#16561 = ORIENTED_EDGE ( 'NONE', *, *, #27382, .T. ) ;
#16562 = CARTESIAN_POINT ( 'NONE',  ( 8.222959289743867473, -16.65189668176488524, -42.75066481758663883 ) ) ;
#16563 = CARTESIAN_POINT ( 'NONE',  ( 23.96502783409409787, -16.12685520490740387, -80.03322214350599495 ) ) ;
#16564 = DIRECTION ( 'NONE',  ( 1.000000000000000000, 0.000000000000000000, 0.000000000000000000 ) ) ;
#16565 = CARTESIAN_POINT ( 'NONE',  ( 14.12425648473279871, 20.57417486552859742, -75.54540032568620234 ) ) ;
#16566 = EDGE_CURVE ( 'NONE', #6481, #25686, #23533, .T. ) ;
#16567 = CARTESIAN_POINT ( 'NONE',  ( 22.94235624568159793, -19.78777630944221855, -59.96754204519741904 ) ) ;
#16568 = CARTESIAN_POINT ( 'NONE',  ( 82.65203287802668797, -45.07757861141610078, -46.57208626984790101 ) ) ;
#16569 = CARTESIAN_POINT ( 'NONE',  ( 63.66395377270059441, 1.424118951467219896, -69.15359763556290318 ) ) ;
#16570 = CARTESIAN_POINT ( 'NONE',  ( 14.48159539877110014, -23.69409007229680242, -40.07189310636189816 ) ) ;
#16571 = ORIENTED_EDGE ( 'NONE', *, *, #14833, .F. ) ;
#16572 = CARTESIAN_POINT ( 'NONE',  ( 52.81005256294240269, -49.67124369057780342, -28.15000000000000213 ) ) ;
#16573 = CARTESIAN_POINT ( 'NONE',  ( 15.70006563680280109, -50.87966732221310195, -20.26432904851890271 ) ) ;
#16574 = CARTESIAN_POINT ( 'NONE',  ( 23.57991226013853847, -18.40053178290571978, -39.62147127257066614 ) ) ;
#16575 = CARTESIAN_POINT ( 'NONE',  ( 15.09849564581118209, -23.52720172089252060, -64.33399919163787217 ) ) ;
#16576 = CARTESIAN_POINT ( 'NONE',  ( 22.90150103265647630, -15.56225260969818969, -56.84464468012870242 ) ) ;
#16577 = CARTESIAN_POINT ( 'NONE',  ( 49.42599753308910238, 14.94798595550149933, -12.04388482386629988 ) ) ;
#16578 = VERTEX_POINT ( 'NONE', #36121 ) ;
#16579 = CARTESIAN_POINT ( 'NONE',  ( -2.895883733608759947, -49.14352575125250411, -5.678499124190959257 ) ) ;
#16580 = CARTESIAN_POINT ( 'NONE',  ( 47.38766415547200239, 23.43125296332900120, -54.78230785539219738 ) ) ;
#16581 = EDGE_CURVE ( 'NONE', #5608, #9812, #41949, .T. ) ;
#16582 = CARTESIAN_POINT ( 'NONE',  ( 22.04686341290252471, -19.02415327330857764, -48.61948854829778810 ) ) ;
#16583 = CARTESIAN_POINT ( 'NONE',  ( 63.03407832914061260, 0.8840451408750739093, -62.48896739026430680 ) ) ;
#16584 = CARTESIAN_POINT ( 'NONE',  ( 54.68494843651092197, 16.77593801893483416, -26.71884417013828994 ) ) ;
#16585 = CARTESIAN_POINT ( 'NONE',  ( 11.10349381579360006, 33.92246930422219720, -17.61839574234429762 ) ) ;
#16586 = DIRECTION ( 'NONE',  ( 7.800826455589531184E-12, 7.212287414728286387E-06, 0.9999999999739914713 ) ) ;
#16587 = CARTESIAN_POINT ( 'NONE',  ( 20.99563245081073148, -9.290037288924558823, -61.50066264437961649 ) ) ;
#16588 = FACE_OUTER_BOUND ( 'NONE', #26825, .T. ) ;
#16589 = CARTESIAN_POINT ( 'NONE',  ( 55.65042755000810359, -48.32738405545750027, -48.64421902443349666 ) ) ;
#16590 = CARTESIAN_POINT ( 'NONE',  ( 24.04468182044177738, -15.61618932230105017, -75.79232603942232060 ) ) ;
#16591 = EDGE_CURVE ( 'NONE', #260, #39471, #23642, .T. ) ;
#16592 = CARTESIAN_POINT ( 'NONE',  ( 64.91485532786460055, 1.370853092582090094, -60.97060118797210038 ) ) ;
#16593 = CARTESIAN_POINT ( 'NONE',  ( 17.21347160910390173, -53.11618894467930119, -76.14999999999999147 ) ) ;
#16594 = EDGE_CURVE ( 'NONE', #10696, #45486, #15447, .T. ) ;
#16595 = CARTESIAN_POINT ( 'NONE',  ( 9.366929594780975421, -16.50193003949960868, -61.41115669688573320 ) ) ;
#16596 = CARTESIAN_POINT ( 'NONE',  ( 51.75217146148440150, 13.88381105532070059, -11.53056162591239975 ) ) ;
#16597 = VERTEX_POINT ( 'NONE', #28765 ) ;
#16598 = CARTESIAN_POINT ( 'NONE',  ( 20.13393739496619972, 24.18330852864180258, -20.65000000000000213 ) ) ;
#16599 = CARTESIAN_POINT ( 'NONE',  ( 10.13628986064439985, 31.90905804943249535, -45.99669294954719589 ) ) ;
#16600 = CYLINDRICAL_SURFACE ( 'NONE', #48569, 0.4999999999999982236 ) ;
#16601 = CARTESIAN_POINT ( 'NONE',  ( 12.97929546375549847, -8.510229299769831002, -81.23899999999999011 ) ) ;
#16602 = VERTEX_POINT ( 'NONE', #37165 ) ;
#16603 = CARTESIAN_POINT ( 'NONE',  ( 18.84633586404639871, 20.57176844745119837, -74.52171359303420672 ) ) ;
#16604 = VERTEX_POINT ( 'NONE', #41603 ) ;
#16605 = VERTEX_POINT ( 'NONE', #17000 ) ;
#16606 = EDGE_LOOP ( 'NONE', ( #15017, #31077, #10400, #32051 ) ) ;
#16607 = CARTESIAN_POINT ( 'NONE',  ( 10.02596761237749945, -63.80904651843830067, -46.25874165023890328 ) ) ;
#16608 = CARTESIAN_POINT ( 'NONE',  ( 28.63393739769619728, -8.399310579809030841, -34.64999999999999858 ) ) ;
#16609 = CARTESIAN_POINT ( 'NONE',  ( 21.50583062810030199, -20.19292315969019924, -81.23899999999999011 ) ) ;
#16610 = EDGE_CURVE ( 'NONE', #16107, #44442, #40048, .T. ) ;
#16611 = CARTESIAN_POINT ( 'NONE',  ( 61.62707301771609991, 13.89267493316299884, -46.47916889091800385 ) ) ;
#16612 = ORIENTED_EDGE ( 'NONE', *, *, #14736, .T. ) ;
#16613 = TOROIDAL_SURFACE ( 'NONE', #31671, 3.000000013056939974, 2.000000000021340263 ) ;
#16614 = CARTESIAN_POINT ( 'NONE',  ( 9.396225823997797377, -16.96132441765022136, -69.78389659178685633 ) ) ;
#16615 = CIRCLE ( 'NONE', #20822, 20.79999999999999716 ) ;
#16616 = CIRCLE ( 'NONE', #15799, 1.999999999999998224 ) ;
#16617 = EDGE_CURVE ( 'NONE', #9565, #31436, #29016, .T. ) ;
#16618 = CARTESIAN_POINT ( 'NONE',  ( 12.63673173825685936, -65.49512871884734011, -22.96425544219204440 ) ) ;
#16619 = ORIENTED_EDGE ( 'NONE', *, *, #13162, .F. ) ;
#16620 = CARTESIAN_POINT ( 'NONE',  ( 11.20408340530847902, -64.05422569580414915, -24.10527562562518611 ) ) ;
#16621 = DIRECTION ( 'NONE',  ( 0.8090169943749515591, 0.000000000000000000, -0.5877852522924675860 ) ) ;
#16622 = AXIS2_PLACEMENT_3D ( 'NONE', #46209, #29668, #6106 ) ;
#16623 = CARTESIAN_POINT ( 'NONE',  ( 19.40270147970570136, 17.88381105532069881, -34.64999999999999858 ) ) ;
#16624 = ORIENTED_EDGE ( 'NONE', *, *, #16319, .F. ) ;
#16626 = ORIENTED_EDGE ( 'NONE', *, *, #8119, .T. ) ;
#16625 =( BOUNDED_CURVE ( )  B_SPLINE_CURVE ( 3, ( #5714, #25088, #17005, #40837 ),
 .UNSPECIFIED., .F., .T. ) 
 B_SPLINE_CURVE_WITH_KNOTS ( ( 4, 4 ),
 ( 6.078858056860969583, 6.232210822545849460 ),
 .UNSPECIFIED. ) 
 CURVE ( )  GEOMETRIC_REPRESENTATION_ITEM ( )  RATIONAL_B_SPLINE_CURVE ( ( 1.000000000000000000, 0.9980412040773770643, 0.9980412040773770643, 1.000000000000000000 ) ) 
 REPRESENTATION_ITEM ( '' )  );
#16627 = CARTESIAN_POINT ( 'NONE',  ( 11.49541412067671509, -65.34930666582664571, -17.78290583432579908 ) ) ;
#16628 = CARTESIAN_POINT ( 'NONE',  ( 71.09324853129349719, 12.47263593864819953, -12.19466500508340090 ) ) ;
#16629 = CARTESIAN_POINT ( 'NONE',  ( 19.34932770686961945, -3.616188944679342931, -22.15000000000000924 ) ) ;
#16630 = CARTESIAN_POINT ( 'NONE',  ( 12.06284766121009966, 32.21085600226960111, -22.25048313876769868 ) ) ;
#16631 = CARTESIAN_POINT ( 'NONE',  ( -6.441449436784619564, 14.95323763042179976, -4.672284524380850179 ) ) ;
#16632 = DIRECTION ( 'NONE',  ( 0.000000000000000000, 1.000000000000000000, 0.000000000000000000 ) ) ;
#16633 = CARTESIAN_POINT ( 'NONE',  ( 61.35834738731979598, 13.96262971120960117, -28.10103293363079757 ) ) ;
#16634 = CARTESIAN_POINT ( 'NONE',  ( 11.80820626746120006, -22.16407397513750155, -59.97333869387029637 ) ) ;
#16635 = EDGE_LOOP ( 'NONE', ( #21224, #19605, #44252, #28314 ) ) ;
#16636 = CARTESIAN_POINT ( 'NONE',  ( 17.98749448546718455, 1.245406012443906807, -34.79644291222912500 ) ) ;
#16637 = CARTESIAN_POINT ( 'NONE',  ( 23.32557412215910020, -49.33122573608360284, -34.65000333295999724 ) ) ;
#16638 = CARTESIAN_POINT ( 'NONE',  ( 12.18715281654259996, 34.05328359747860389, -46.13824078873810208 ) ) ;
#16639 = CARTESIAN_POINT ( 'NONE',  ( 72.15779067374299416, 1.443559558797639975, -69.80991579785110446 ) ) ;
#16640 = CARTESIAN_POINT ( 'NONE',  ( 43.29044952474772145, -39.89310745266933367, -70.09458329593303461 ) ) ;
#16641 = AXIS2_PLACEMENT_3D ( 'NONE', #16630, #12717, #33118 ) ;
#16642 = CARTESIAN_POINT ( 'NONE',  ( 14.06327089604441127, -23.32129222870931784, -36.37566369939185762 ) ) ;
#16643 = CARTESIAN_POINT ( 'NONE',  ( 12.75999515594850031, 18.86331954735589989, -21.12209177392130144 ) ) ;
#16644 = AXIS2_PLACEMENT_3D ( 'NONE', #18286, #17527, #29563 ) ;
#16645 = CARTESIAN_POINT ( 'NONE',  ( -0.3016046179078940015, -10.91500322974829906, -35.02873218748179340 ) ) ;
#16646 = CARTESIAN_POINT ( 'NONE',  ( 49.03570248356319894, -53.73371453229830763, -54.39120251675719686 ) ) ;
#16647 = CARTESIAN_POINT ( 'NONE',  ( -3.454818612163319536, 17.59177618004110144, -5.676727923997320069 ) ) ;
#16648 = EDGE_CURVE ( 'NONE', #39953, #19884, #48806, .T. ) ;
#16649 = VECTOR ( 'NONE', #39365, 1000.000000000000114 ) ;
#16650 = CARTESIAN_POINT ( 'NONE',  ( 8.520859443580489412, -17.83227332291358280, -34.41746388773530185 ) ) ;
#16651 = CARTESIAN_POINT ( 'NONE',  ( 65.04848046133125195, -32.26190002985004668, -17.85478322451875854 ) ) ;
#16652 = CARTESIAN_POINT ( 'NONE',  ( 9.221456941219052794, -19.60039333794279415, -54.62566536593503486 ) ) ;
#16653 = EDGE_CURVE ( 'NONE', #28355, #29283, #46152, .T. ) ;
#16654 = EDGE_LOOP ( 'NONE', ( #21106, #8343, #42698, #25371 ) ) ;
#16655 = CARTESIAN_POINT ( 'NONE',  ( 10.97781814925719956, -20.99402574345059946, -45.81064392402229402 ) ) ;
#16656 = CARTESIAN_POINT ( 'NONE',  ( 63.99945660972100825, 1.277726347179370059, -61.38577996275480331 ) ) ;
#16657 = ORIENTED_EDGE ( 'NONE', *, *, #32687, .F. ) ;
#16658 = DIRECTION ( 'NONE',  ( 0.000000000000000000, 1.000000000000000000, 0.000000000000000000 ) ) ;
#16659 = CARTESIAN_POINT ( 'NONE',  ( 60.37202493514429591, -45.79855239338960615, -47.62297778162039918 ) ) ;
#16660 = CARTESIAN_POINT ( 'NONE',  ( 57.12444641458250061, 19.38683328974900277, -53.89324253167760048 ) ) ;
#16661 = CARTESIAN_POINT ( 'NONE',  ( 61.75019796695539753, 13.88381105532070059, -46.37203261889099792 ) ) ;
#16663 = CARTESIAN_POINT ( 'NONE',  ( -0.03447620312152044342, -8.421650097910747590, -34.79644660940672196 ) ) ;
#16662 = CARTESIAN_POINT ( 'NONE',  ( 42.51301359343917596, 8.585954781958603732, -73.85330097299451779 ) ) ;
#16664 = CARTESIAN_POINT ( 'NONE',  ( 9.965766340832269421, -12.19621453136610079, -60.00832647495010264 ) ) ;
#16665 = PLANE ( 'NONE',  #193 ) ;
#16666 = ORIENTED_EDGE ( 'NONE', *, *, #35768, .F. ) ;
#16667 = CARTESIAN_POINT ( 'NONE',  ( 83.63395638909621255, -44.98627285813419974, -47.37153147893519645 ) ) ;
#16668 = VERTEX_POINT ( 'NONE', #25081 ) ;
#16669 = VERTEX_POINT ( 'NONE', #45545 ) ;
#16670 = EDGE_LOOP ( 'NONE', ( #4611, #20470, #3161, #35255, #36533, #45255, #41296, #33649, #24240 ) ) ;
#16671 = FACE_OUTER_BOUND ( 'NONE', #3803, .T. ) ;
#16672 = DIRECTION ( 'NONE',  ( 1.000000000000000000, 0.000000000000000000, 0.000000000000000000 ) ) ;
#16673 = CARTESIAN_POINT ( 'NONE',  ( 76.44639894005106839, -6.601916875635619242, -12.99644329064062909 ) ) ;
#16674 = CARTESIAN_POINT ( 'NONE',  ( 51.34626689658080068, -52.95676961735540544, -54.59842079273609272 ) ) ;
#16675 = AXIS2_PLACEMENT_3D ( 'NONE', #8907, #28280, #44029 ) ;
#16676 = ORIENTED_EDGE ( 'NONE', *, *, #22944, .T. ) ;
#16677 = VERTEX_POINT ( 'NONE', #21416 ) ;
#16678 = EDGE_CURVE ( 'NONE', #34659, #586, #40571, .T. ) ;
#16679 = CARTESIAN_POINT ( 'NONE',  ( 28.28038400710291356, -22.62894316431776431, -34.79644660940672907 ) ) ;
#16680 = CARTESIAN_POINT ( 'NONE',  ( 16.15069456443690044, 19.81939336389048734, -20.15000000000000213 ) ) ;
#16681 = CARTESIAN_POINT ( 'NONE',  ( 25.43010376912519988, -1.113097814880039893, -35.14999999999999858 ) ) ;
#16682 = CARTESIAN_POINT ( 'NONE',  ( 8.808591387964359143, -63.24239172143919774, -46.67055361988870033 ) ) ;
#16683 = EDGE_CURVE ( 'NONE', #35448, #31343, #39430, .T. ) ;
#16684 = CARTESIAN_POINT ( 'NONE',  ( 24.04215776945413907, -15.38968793046390182, -59.78321309548368134 ) ) ;
#16685 = FACE_OUTER_BOUND ( 'NONE', #3282, .T. ) ;
#16686 = AXIS2_PLACEMENT_3D ( 'NONE', #28795, #36653, #16754 ) ;
#16687 = ORIENTED_EDGE ( 'NONE', *, *, #36092, .T. ) ;
#16688 = CARTESIAN_POINT ( 'NONE',  ( 53.63393739769619373, -53.11618894467930119, 11.84999999999999964 ) ) ;
#16689 = CARTESIAN_POINT ( 'NONE',  ( 53.07595679201899941, -50.38449176261200080, -77.13124877896089515 ) ) ;
#16690 = CARTESIAN_POINT ( 'NONE',  ( 64.89987712417480736, 0.8859637708054459715, -70.70388507757908769 ) ) ;
#16691 = CARTESIAN_POINT ( 'NONE',  ( 60.83884119656880074, 14.23235859654429980, -47.05422022228049883 ) ) ;
#16692 = AXIS2_PLACEMENT_3D ( 'NONE', #37234, #48773, #17319 ) ;
#16693 = AXIS2_PLACEMENT_3D ( 'NONE', #23537, #47432, #27745 ) ;
#16694 = CARTESIAN_POINT ( 'NONE',  ( 12.47698802750519853, -8.672597014313410568, -67.35819317332689593 ) ) ;
#16695 = DIRECTION ( 'NONE',  ( -0.3918900565005491998, 0.9200120562340454722, 0.000000000000000000 ) ) ;
#16696 = B_SPLINE_CURVE_WITH_KNOTS ( 'NONE', 3,
 ( #32939, #29023, #16991, #468, #41087, #12802, #31905, #8863, #8339, #28758, #40823, #47925, #4924, #28501, #12027, #48432 ),
 .UNSPECIFIED., .F., .F.,
 ( 4, 2, 2, 2, 2, 2, 2, 4 ),
 ( 0.000000000000000000, 0.1775020625791663698, 0.3375039218054580181, 0.4375050838218894067, 0.5000058100821596074, 0.6250072626026996758, 0.7914782147670768042, 1.000000000000000000 ),
 .UNSPECIFIED. ) ;
#16697 = CARTESIAN_POINT ( 'NONE',  ( 43.67695093021549724, -43.30705450646729560, -4.963296560282329573 ) ) ;
#16698 = LINE ( 'NONE', #16440, #35125 ) ;
#16699 = CARTESIAN_POINT ( 'NONE',  ( 57.20485010882750743, 13.88381105532070059, -16.39258517501439982 ) ) ;
#16700 = CARTESIAN_POINT ( 'NONE',  ( 61.47037426737699661, -45.40940486849099500, -47.41703440505000344 ) ) ;
#16701 = CARTESIAN_POINT ( 'NONE',  ( 63.96720938203739593, 1.277721779380850187, -69.88196296493690340 ) ) ;
#16702 = CARTESIAN_POINT ( 'NONE',  ( 8.222963058980525375, -14.58045360959418169, -40.83399815091998164 ) ) ;
#16703 = ORIENTED_EDGE ( 'NONE', *, *, #32788, .F. ) ;
#16704 = CARTESIAN_POINT ( 'NONE',  ( 14.57025157893530043, -52.06302405750739837, -75.84958893011570069 ) ) ;
#16705 = CARTESIAN_POINT ( 'NONE',  ( 47.33575985341339987, -54.69488657390869690, -54.69046143333279986 ) ) ;
#16706 = CARTESIAN_POINT ( 'NONE',  ( 15.09839247718639932, -7.705188636603384822, -36.96600318730514090 ) ) ;
#16707 = LINE ( 'NONE', #25063, #44734 ) ;
#16708 = CARTESIAN_POINT ( 'NONE',  ( 60.86909712740357747, -45.45332394799820719, -47.09890482454854066 ) ) ;
#16709 = CARTESIAN_POINT ( 'NONE',  ( 22.19862325585670249, -12.11392824337299956, -32.14999999999999858 ) ) ;
#16710 = FACE_OUTER_BOUND ( 'NONE', #14428, .T. ) ;
#16711 = CARTESIAN_POINT ( 'NONE',  ( 47.68046934622199728, -54.51757764637919479, -55.10164272630390059 ) ) ;
#16713 = CARTESIAN_POINT ( 'NONE',  ( 12.89984684562703343, -50.74322487993451603, -21.40242722397054109 ) ) ;
#16712 = CARTESIAN_POINT ( 'NONE',  ( 8.222937397696199469, -15.61618894467929941, -32.14999999999999858 ) ) ;
#16714 = ADVANCED_FACE ( 'NONE', ( #33214 ), #1000, .T. ) ;
#16715 = DIRECTION ( 'NONE',  ( 1.000000000000000000, 0.000000000000000000, 0.000000000000000000 ) ) ;
#16716 = APPLICATION_CONTEXT ( 'automotive_design' ) ;
#16717 = CARTESIAN_POINT ( 'NONE',  ( 48.39474571203390241, 22.93079767860760043, -54.88276765605429830 ) ) ;
#16718 = AXIS2_PLACEMENT_3D ( 'NONE', #18496, #6452, #42351 ) ;
#16719 = ORIENTED_EDGE ( 'NONE', *, *, #8461, .F. ) ;
#16720 = VECTOR ( 'NONE', #39265, 1000.000000000000000 ) ;
#16721 = CARTESIAN_POINT ( 'NONE',  ( 13.95270971513190084, -8.909117678376349048, -68.24709530556648929 ) ) ;
#16722 = ORIENTED_EDGE ( 'NONE', *, *, #49918, .T. ) ;
#16723 = AXIS2_PLACEMENT_3D ( 'NONE', #27784, #2665, #11307 ) ;
#16724 = CARTESIAN_POINT ( 'NONE',  ( 2.458146360389407370, -5.580163940743402051, -34.79644291222906105 ) ) ;
#16725 = CARTESIAN_POINT ( 'NONE',  ( -27.57791469522849681, 115.8715079793770144, -50.15833750720749862 ) ) ;
#16726 = CARTESIAN_POINT ( 'NONE',  ( 16.13393739769620083, -15.61618894467929941, -28.45282021618999835 ) ) ;
#16728 = CARTESIAN_POINT ( 'NONE',  ( 53.41792665956379693, 17.70733950191389994, -26.73822481760680247 ) ) ;
#16727 = CARTESIAN_POINT ( 'NONE',  ( 82.62217614637150120, 13.83472246775060022, -46.37143498965760102 ) ) ;
#16729 = AXIS2_PLACEMENT_3D ( 'NONE', #34782, #51306, #15400 ) ;
#16730 = CARTESIAN_POINT ( 'NONE',  ( 11.77719006542909952, -21.16247701684149973, -67.16476753011978928 ) ) ;
#16731 = DIRECTION ( 'NONE',  ( -0.5516667872527352134, -0.8340645993220461296, 0.000000000000000000 ) ) ;
#16732 = CARTESIAN_POINT ( 'NONE',  ( 56.32875602673239968, -45.28046490780249655, -16.42171413587569972 ) ) ;
#16733 = B_SPLINE_SURFACE_WITH_KNOTS ( 'NONE', 3, 3, ( 
 ( #37824, #5852, #45430, #17649, #3731, #15523, #50397, #35428, #38864, #51172 ),
 ( #2953, #26782, #43053, #39373, #39119, #14483, #35165, #31475, #19184, #34907 ),
 ( #7665, #34643, #7402, #18669, #50648, #50906, #15265, #31221, #3213, #47248 ),
 ( #47499, #26520, #2696, #11081, #30714, #22589, #30454, #38606, #46477, #10563 ),
 ( #46736, #42537, #6625, #14744, #11597, #30966, #11338, #27556, #10820, #27302 ),
 ( #23608, #42797, #39628, #19703, #6893, #14998, #22843, #18923, #43564, #43310 ),
 ( #23350, #46996, #27049, #7149, #3474, #23101, #19445, #51427, #40135, #48782 ),
 ( #15773, #8171, #44848, #5018, #12889, #36706, #8431, #28845, #7914, #16808 ),
 ( #32238, #28582, #4231, #16537, #20455, #43815, #8953, #40908, #36445, #551 ),
 ( #44067, #40392, #16284, #24895, #35695, #302, #32489, #32757, #12107, #44582 ),
 ( #19948, #39886, #24377, #24115, #28320, #23863, #20716, #51679, #807, #20205 ),
 ( #3985, #36192, #35938, #58, #48517, #48261, #12622, #12355, #24638, #16032 ),
 ( #8686, #40651, #31988, #31727, #47753, #4749, #44321, #4486, #11860, #27815 ),
 ( #48008, #28064, #20980, #6050, #9473, #21750, #45621, #25421, #49310, #13657 ),
 ( #9721, #36979, #5790, #2112, #41682, #5541, #37760, #30132, #5282, #29867 ),
 ( #41170, #21496, #1856, #17834, #25680, #33807, #14164, #18091, #49050, #25164 ) ),
 .UNSPECIFIED., .F., .F., .F.,
 ( 4, 2, 2, 2, 2, 2, 2, 4 ),
 ( 4, 1, 1, 1, 1, 1, 1, 4 ),
 ( -8.599659000000000768E-15, 0.07216186899280199740, 0.1546325764131580016, 0.2061767685508799908, 0.2319488646197410131, 0.2731842183299189597, 0.3391607842662029970, 0.4123535371017689743 ),
 ( 0.000000000000000000, 0.1428571428571430157, 0.2857142857142860315, 0.4285714285714289917, 0.5714285714285709528, 0.7142857142857139685, 0.8571428571428569843, 1.000000000000000000 ),
 .UNSPECIFIED. ) ;
#16734 = LINE ( 'NONE', #8879, #44865 ) ;
#16735 = ORIENTED_EDGE ( 'NONE', *, *, #45449, .T. ) ;
#16736 = AXIS2_PLACEMENT_3D ( 'NONE', #24839, #36385, #1019 ) ;
#16737 = EDGE_LOOP ( 'NONE', ( #14877, #35343, #43058, #37364 ) ) ;
#16738 = CARTESIAN_POINT ( 'NONE',  ( 12.04145588157719970, -65.07204108492659600, -16.48289738546709771 ) ) ;
#16739 = CARTESIAN_POINT ( 'NONE',  ( 10.92611299134039982, 33.35840257386460195, -46.27040258753400082 ) ) ;
#16740 = DIRECTION ( 'NONE',  ( 0.000000000000000000, 0.000000000000000000, -1.000000000000000000 ) ) ;
#16741 = CARTESIAN_POINT ( 'NONE',  ( 52.70905074378630673, -49.70817001306580352, -48.28317273910510465 ) ) ;
#16742 = CARTESIAN_POINT ( 'NONE',  ( 23.04647760069162032, -19.60028859616953412, -63.67433653012798089 ) ) ;
#16743 = ORIENTED_EDGE ( 'NONE', *, *, #41482, .F. ) ;
#16744 = EDGE_CURVE ( 'NONE', #4837, #29074, #51152, .T. ) ;
#16745 = CARTESIAN_POINT ( 'NONE',  ( 14.06315725531258387, -7.911115082366269924, -74.92430270396020831 ) ) ;
#16746 = CARTESIAN_POINT ( 'NONE',  ( 68.13393739769618662, -31.81618894467930403, -65.65000000000000568 ) ) ;
#16747 = CARTESIAN_POINT ( 'NONE',  ( 49.20928845107640370, 22.41119391493339918, -54.30076444815649950 ) ) ;
#16748 = EDGE_CURVE ( 'NONE', #4775, #13785, #36924, .T. ) ;
#16749 = DIRECTION ( 'NONE',  ( -0.5897727341282608116, 0.3900873262218075288, 0.7071067811865454633 ) ) ;
#16750 = CARTESIAN_POINT ( 'NONE',  ( 50.85761971603020015, -50.68614562676760471, -76.14999999999999147 ) ) ;
#16751 = CARTESIAN_POINT ( 'NONE',  ( 22.37318698975099807, -53.60726374558549878, -34.64999999999999858 ) ) ;
#16752 = VERTEX_POINT ( 'NONE', #8871 ) ;
#16753 = CARTESIAN_POINT ( 'NONE',  ( 14.36278203781940555, -9.025291871498199114, -67.86948588150255546 ) ) ;
#16754 = DIRECTION ( 'NONE',  ( 0.4145156864928219997, 0.9100421669633689259, 0.000000000000000000 ) ) ;
#16755 = ORIENTED_EDGE ( 'NONE', *, *, #37633, .F. ) ;
#16756 = CARTESIAN_POINT ( 'NONE',  ( 51.13393739769659874, -50.61618894467899565, 16.85000000000000142 ) ) ;
#16757 = CARTESIAN_POINT ( 'NONE',  ( 45.68512934788851965, 2.192362318393687115, -54.50653973161867327 ) ) ;
#16758 = CARTESIAN_POINT ( 'NONE',  ( 20.10897586428119865, -22.38276145748530155, -32.34342564320699864 ) ) ;
#16759 = CARTESIAN_POINT ( 'NONE',  ( 13.79441456740149974, -51.27878729324490337, -22.92979596798970121 ) ) ;
#16760 = CARTESIAN_POINT ( 'NONE',  ( 53.62535340796430461, 20.09876804296569830, -75.58067205068070393 ) ) ;
#16761 = CARTESIAN_POINT ( 'NONE',  ( 47.48804938961460209, -54.57746163137669981, -74.50208837960660446 ) ) ;
#16762 = VERTEX_POINT ( 'NONE', #42913 ) ;
#16763 = PLANE ( 'NONE',  #7794 ) ;
#16764 = VECTOR ( 'NONE', #30973, 1000.000000000000000 ) ;
#16765 = CARTESIAN_POINT ( 'NONE',  ( 17.18916429022859660, -22.99136284164080024, -68.68742111086839941 ) ) ;
#16767 = CARTESIAN_POINT ( 'NONE',  ( 52.70648214874140081, -49.76125733399389617, -48.81430935866210064 ) ) ;
#16766 = AXIS2_PLACEMENT_3D ( 'NONE', #10823, #6896, #14487 ) ;
#16768 = DIRECTION ( 'NONE',  ( -0.000000000000000000, -1.000000000000000000, -0.000000000000000000 ) ) ;
#16769 = FACE_OUTER_BOUND ( 'NONE', #40026, .T. ) ;
#16770 = AXIS2_PLACEMENT_3D ( 'NONE', #26734, #10518, #22544 ) ;
#16771 = CARTESIAN_POINT ( 'NONE',  ( 46.35275103504439898, 21.67755452994670406, -76.14999999999999147 ) ) ;
#16772 = CARTESIAN_POINT ( 'NONE',  ( 19.80201486048481030, -54.46428635315598399, -17.67512396564999833 ) ) ;
#16773 = B_SPLINE_CURVE_WITH_KNOTS ( 'NONE', 3,
 ( #47811, #51733, #42130, #7459, #6230, #43873, #38196, #50256, #47310, #35494 ),
 .UNSPECIFIED., .F., .F.,
 ( 4, 2, 2, 2, 4 ),
 ( 0.000000000000000000, 0.2009658351805388987, 0.5348857748336580675, 0.9393348933166768555, 1.000000000000000000 ),
 .UNSPECIFIED. ) ;
#16774 = PRODUCT_RELATED_PRODUCT_CATEGORY ( 'part', '', ( #34076 ) ) ;
#16775 = CARTESIAN_POINT ( 'NONE',  ( 16.13393739769620083, -15.61618894467929941, -22.64999999999999858 ) ) ;
#16776 =( BOUNDED_CURVE ( )  B_SPLINE_CURVE ( 3, ( #1981, #18989, #14810, #46018 ),
 .UNSPECIFIED., .F., .T. ) 
 B_SPLINE_CURVE_WITH_KNOTS ( ( 4, 4 ),
 ( 2.356194490192476731, 3.141592653589780237 ),
 .UNSPECIFIED. ) 
 CURVE ( )  GEOMETRIC_REPRESENTATION_ITEM ( )  RATIONAL_B_SPLINE_CURVE ( ( 1.000000000000000000, 0.9492530216742096627, 0.9492530216742096627, 1.000000000000000000 ) ) 
 REPRESENTATION_ITEM ( '' )  );
#16777 = CARTESIAN_POINT ( 'NONE',  ( 12.29622276841139872, 33.50355195994969648, -15.96315064374149983 ) ) ;
#16778 = PLANE ( 'NONE',  #19696 ) ;
#16779 = CARTESIAN_POINT ( 'NONE',  ( 68.13393739769618662, -30.31618894467939995, -65.65000000000000568 ) ) ;
#16781 = FACE_OUTER_BOUND ( 'NONE', #31710, .T. ) ;
#16780 = DIRECTION ( 'NONE',  ( -1.822422554782380175E-11, -1.784227544494129940E-11, -1.000000000000000000 ) ) ;
#16782 = ADVANCED_FACE ( 'NONE', ( #49993 ), #14328, .T. ) ;
#16783 = CARTESIAN_POINT ( 'NONE',  ( 63.17541640582520301, 1.096153228089730147, -68.95757157983499042 ) ) ;
#16784 = CARTESIAN_POINT ( 'NONE',  ( 61.33122422115619798, 14.00089233987130122, -46.85723822856199661 ) ) ;
#16785 = CARTESIAN_POINT ( 'NONE',  ( -33.14787555410379838, -25.36774897639840276, -57.37579723497079698 ) ) ;
#16786 = EDGE_CURVE ( 'NONE', #38464, #51752, #34411, .T. ) ;
#16787 = VERTEX_POINT ( 'NONE', #30570 ) ;
#16788 = CARTESIAN_POINT ( 'NONE',  ( 52.83465167515200278, -49.65874968186350458, -48.65907986970169929 ) ) ;
#16789 = EDGE_CURVE ( 'NONE', #51255, #24834, #44989, .T. ) ;
#16790 = CARTESIAN_POINT ( 'NONE',  ( 18.65687415773260582, -13.78316809304479662, -28.02168704970069868 ) ) ;
#16791 = DIRECTION ( 'NONE',  ( 0.4646601886423053496, 0.000000000000000000, 0.8854890790353641128 ) ) ;
#16792 = CARTESIAN_POINT ( 'NONE',  ( 56.29024440006210739, 14.53176988408540105, -25.89618347059580117 ) ) ;
#16793 = CARTESIAN_POINT ( 'NONE',  ( 22.66051486065669707, -12.94292402765340100, -38.32907662296229745 ) ) ;
#16794 = ADVANCED_FACE ( 'NONE', ( #46071 ), #43638, .T. ) ;
#16795 = CARTESIAN_POINT ( 'NONE',  ( 50.35727174223609381, 17.94937212879660038, -76.16289466383139484 ) ) ;
#16796 = CARTESIAN_POINT ( 'NONE',  ( 52.87179753541859384, 18.40851527081879979, -48.76566975022370087 ) ) ;
#16797 = CARTESIAN_POINT ( 'NONE',  ( 71.14534185144368905, 1.334812829108570131, -70.51979614837409827 ) ) ;
#16798 = DIRECTION ( 'NONE',  ( 1.000000000000000000, 0.000000000000000000, 0.000000000000000000 ) ) ;
#16799 = CARTESIAN_POINT ( 'NONE',  ( 64.36428085589631110, -45.11618894467940066, -12.32250341870529908 ) ) ;
#16800 = ORIENTED_EDGE ( 'NONE', *, *, #40826, .T. ) ;
#16801 = DIRECTION ( 'NONE',  ( 0.7071067811865457964, 0.000000000000000000, -0.7071067811865492381 ) ) ;
#16802 = CARTESIAN_POINT ( 'NONE',  ( 8.732168080967809942, -16.46501479270679980, -64.03099806865479593 ) ) ;
#16803 = CARTESIAN_POINT ( 'NONE',  ( 72.93015195551900831, 1.326578174762039986, -68.82808305222700085 ) ) ;
#16804 = CARTESIAN_POINT ( 'NONE',  ( 47.65145214304179433, -54.48884158768570529, -54.70160429609599362 ) ) ;
#16805 = DIRECTION ( 'NONE',  ( 0.000000000000000000, 0.000000000000000000, -1.000000000000000000 ) ) ;
#16806 = CARTESIAN_POINT ( 'NONE',  ( 13.39998208310050032, -51.78678246903520233, -23.15000000000000213 ) ) ;
#16807 = CARTESIAN_POINT ( 'NONE',  ( 60.41042365232780043, 14.86001756475369895, -48.11601410346130336 ) ) ;
#16808 = CARTESIAN_POINT ( 'NONE',  ( 71.17189893730710537, 1.387131204727290124, -61.00757424182599920 ) ) ;
#16809 = CARTESIAN_POINT ( 'NONE',  ( 29.63393739769620083, -15.61618894467929941, 17.35000000000000142 ) ) ;
#16810 = CARTESIAN_POINT ( 'NONE',  ( 71.42517083710241366, 1.394012070863459796, -61.05800084754509527 ) ) ;
#16811 = AXIS2_PLACEMENT_3D ( 'NONE', #25030, #30004, #45763 ) ;
#16812 = AXIS2_PLACEMENT_3D ( 'NONE', #7602, #31413, #11274 ) ;
#16813 = CARTESIAN_POINT ( 'NONE',  ( 24.04424254486977475, -15.72944168295483536, -71.51222841874697167 ) ) ;
#16814 = CARTESIAN_POINT ( 'NONE',  ( 64.84324960441189489, 0.8888742037077569380, -70.66714310028379487 ) ) ;
#16815 = ORIENTED_EDGE ( 'NONE', *, *, #13433, .T. ) ;
#16816 = ORIENTED_EDGE ( 'NONE', *, *, #51702, .T. ) ;
#16817 = CARTESIAN_POINT ( 'NONE',  ( 11.63393739769600010, 10.38381105532060111, -34.64999999999999858 ) ) ;
#16818 = CARTESIAN_POINT ( 'NONE',  ( 68.13393739769618662, -2.032350560841069687, -102.2016796975542690 ) ) ;
#16819 = ORIENTED_EDGE ( 'NONE', *, *, #12652, .F. ) ;
#16820 = EDGE_CURVE ( 'NONE', #39844, #11209, #18264, .T. ) ;
#16821 = CARTESIAN_POINT ( 'NONE',  ( 10.45980683277509904, -11.42729869705060075, -72.04960399662019199 ) ) ;
#16822 = CARTESIAN_POINT ( 'NONE',  ( 9.543049661443221865, -13.84499421749102943, -69.53615381081331748 ) ) ;
#16823 = DIRECTION ( 'NONE',  ( 0.000000000000000000, 0.000000000000000000, 1.000000000000000000 ) ) ;
#16824 = CARTESIAN_POINT ( 'NONE',  ( 52.21153807214869857, 19.18935477659329791, -76.55085343138060239 ) ) ;
#16825 = ORIENTED_EDGE ( 'NONE', *, *, #6568, .T. ) ;
#16826 = CARTESIAN_POINT ( 'NONE',  ( 9.366426063424411197, -15.61626247110940113, -71.45282021618990598 ) ) ;
#16827 = CARTESIAN_POINT ( 'NONE',  ( 24.04491815576623637, -15.63504520850458590, -65.50842498917839407 ) ) ;
#16828 = CARTESIAN_POINT ( 'NONE',  ( 8.063529214243020604, -13.92762985232080020, -46.85798391838919486 ) ) ;
#16829 = CARTESIAN_POINT ( 'NONE',  ( 15.50293243011315525, -8.820692638884411352, -55.92317534179022687 ) ) ;
#16830 = CARTESIAN_POINT ( 'NONE',  ( 41.70677336635860399, -37.57567824672890566, -81.78581377007661501 ) ) ;
#16831 = ORIENTED_EDGE ( 'NONE', *, *, #37139, .F. ) ;
#16832 = CARTESIAN_POINT ( 'NONE',  ( 13.04106483549849926, -65.52043803436799863, -23.35241516560489927 ) ) ;
#16833 = CARTESIAN_POINT ( 'NONE',  ( 17.29212060902849757, -22.97589718985749840, -36.68297296116619322 ) ) ;
#16834 = EDGE_CURVE ( 'NONE', #21125, #49316, #34232, .T. ) ;
#16835 = CARTESIAN_POINT ( 'NONE',  ( 22.46008322700772908, -10.75448448616132957, -33.29933195708130000 ) ) ;
#16836 = CARTESIAN_POINT ( 'NONE',  ( 14.51655170844479947, 20.71403734715240219, -75.77237669558989808 ) ) ;
#16837 = CARTESIAN_POINT ( 'NONE',  ( 51.84382198560120258, 18.03478096587799939, -77.06468273675109515 ) ) ;
#16838 = AXIS2_PLACEMENT_3D ( 'NONE', #46334, #2555, #10420 ) ;
#16839 = CONICAL_SURFACE ( 'NONE', #47828, 19.50000000000000000, 0.2449786631268651149 ) ;
#16840 = CARTESIAN_POINT ( 'NONE',  ( 84.12560615065839897, -43.96699487611929413, -46.88422054015599372 ) ) ;
#16841 = CARTESIAN_POINT ( 'NONE',  ( 63.57990658082609770, 1.404649297339839897, -68.94572984764299406 ) ) ;
#16842 = CIRCLE ( 'NONE', #43642, 7.599999999999996092 ) ;
#16843 = CARTESIAN_POINT ( 'NONE',  ( 8.644136429342630379, -19.06373911304890001, -50.37035414463240102 ) ) ;
#16844 = ORIENTED_EDGE ( 'NONE', *, *, #50658, .T. ) ;
#16845 = CARTESIAN_POINT ( 'NONE',  ( 53.08857600003049981, -49.42354551114720351, -27.55244750385169894 ) ) ;
#16846 = CARTESIAN_POINT ( 'NONE',  ( 16.36412298843900004, -51.09682246409949613, -20.14982337726360129 ) ) ;
#16847 = CARTESIAN_POINT ( 'NONE',  ( 53.63393739769619373, -63.11618894467929408, 11.84999999999999964 ) ) ;
#16848 = CARTESIAN_POINT ( 'NONE',  ( 54.51878663346509057, 12.23944275751169286, -7.640492836310381009 ) ) ;
#16849 = FACE_OUTER_BOUND ( 'NONE', #24323, .T. ) ;
#16850 = CARTESIAN_POINT ( 'NONE',  ( 24.04460285965960864, -15.61618860597671876, -65.79233133698019742 ) ) ;
#16851 = EDGE_CURVE ( 'NONE', #46513, #621, #35245, .T. ) ;
#16852 = EDGE_LOOP ( 'NONE', ( #45626, #28763, #30852, #22971 ) ) ;
#16853 = CARTESIAN_POINT ( 'NONE',  ( -6.547816903263669275, -46.29994198797230354, -5.461245372614969895 ) ) ;
#16854 = EDGE_CURVE ( 'NONE', #12115, #8205, #36096, .T. ) ;
#16855 = CARTESIAN_POINT ( 'NONE',  ( 47.46651691217249436, 23.36841135167989947, -54.65114297014489608 ) ) ;
#16856 = CARTESIAN_POINT ( 'NONE',  ( 63.37726551317079782, 1.370937308141420230, -62.62705977251020784 ) ) ;
#16857 = CARTESIAN_POINT ( 'NONE',  ( 68.13393739769618662, -0.5161889446793590519, -49.64999999999999858 ) ) ;
#16858 = CARTESIAN_POINT ( 'NONE',  ( 41.93138973097610034, 13.29046345406609930, -5.197897844688459834 ) ) ;
#16859 = ADVANCED_FACE ( 'NONE', ( #22960 ), #31887, .F. ) ;
#16860 = FACE_OUTER_BOUND ( 'NONE', #51094, .T. ) ;
#16861 = CARTESIAN_POINT ( 'NONE',  ( 83.95017614158776098, -44.74867211454660776, -47.46180894508327697 ) ) ;
#16862 = CARTESIAN_POINT ( 'NONE',  ( 68.13393739769618662, -0.5161889446793590519, -65.65000000000000568 ) ) ;
#16863 = CARTESIAN_POINT ( 'NONE',  ( 58.32272783024919960, -46.80742713280790213, -47.80927467149849974 ) ) ;
#16864 = B_SPLINE_CURVE_WITH_KNOTS ( 'NONE', 3,
 ( #7526, #32106, #19568, #4605 ),
 .UNSPECIFIED., .F., .F.,
 ( 4, 4 ),
 ( 0.6437608425907387355, 1.000000000000000000 ),
 .UNSPECIFIED. ) ;
#16865 = CARTESIAN_POINT ( 'NONE',  ( 11.62079934899224476, -20.68763287804364737, -67.18421635681791315 ) ) ;
#16866 = CARTESIAN_POINT ( 'NONE',  ( 64.69948915615019303, 1.003508719580009867, -60.73835207042080242 ) ) ;
#16867 = CARTESIAN_POINT ( 'NONE',  ( 17.52098156358690062, -52.86909850055779714, -76.12391999848780699 ) ) ;
#16868 = CARTESIAN_POINT ( 'NONE',  ( 14.06329967161854633, -7.911078209043669318, -77.20899686763637249 ) ) ;
#16869 = CARTESIAN_POINT ( 'NONE',  ( 55.55365133010059964, 13.88381105532070059, -14.32025150907159983 ) ) ;
#16870 = ORIENTED_EDGE ( 'NONE', *, *, #14441, .T. ) ;
#16871 = CARTESIAN_POINT ( 'NONE',  ( 37.88393739769619373, -42.11618894467939356, -35.14999999999999858 ) ) ;
#16872 = CARTESIAN_POINT ( 'NONE',  ( 9.292254072159270351, 32.01117642126040153, -46.52992118075790273 ) ) ;
#16873 = CARTESIAN_POINT ( 'NONE',  ( 46.03122142033570441, 13.88381105532070059, -7.582879021622040305 ) ) ;
#16874 = EDGE_CURVE ( 'NONE', #36898, #10310, #45807, .T. ) ;
#16875 = CARTESIAN_POINT ( 'NONE',  ( 66.71082852131469565, -30.88066898215729950, -17.22174391961319984 ) ) ;
#16876 = ORIENTED_EDGE ( 'NONE', *, *, #5742, .F. ) ;
#16877 = B_SPLINE_CURVE_WITH_KNOTS ( 'NONE', 3,
 ( #6849, #42753, #26476, #18879, #15477, #51122, #23056, #46431 ),
 .UNSPECIFIED., .F., .F.,
 ( 4, 2, 2, 4 ),
 ( 0.000000000000000000, 0.1749999999997750855, 0.3749999999995158317, 0.4999999271553960956 ),
 .UNSPECIFIED. ) ;
#16878 = CARTESIAN_POINT ( 'NONE',  ( 18.06569355283950173, 20.03470611338460472, -74.90176971618339508 ) ) ;
#16879 = VERTEX_POINT ( 'NONE', #6487 ) ;
#16880 = ORIENTED_EDGE ( 'NONE', *, *, #22908, .F. ) ;
#16881 = EDGE_LOOP ( 'NONE', ( #10110, #24212, #21757, #4912 ) ) ;
#16882 = ADVANCED_FACE ( 'NONE', ( #38451 ), #38631, .T. ) ;
#16883 = CARTESIAN_POINT ( 'NONE',  ( 12.21006104367689993, -65.32600393230370628, -46.80110686342489856 ) ) ;
#16884 = DIRECTION ( 'NONE',  ( -0.000000000000000000, 1.000000000000000000, 0.000000000000000000 ) ) ;
#16885 = CARTESIAN_POINT ( 'NONE',  ( 22.89050912567230256, -18.23020240017759974, -81.23899999999999011 ) ) ;
#16886 = CIRCLE ( 'NONE', #46185, 14.50000000000000178 ) ;
#16887 = CARTESIAN_POINT ( 'NONE',  ( 61.68987301043100047, 13.88502391956650150, -46.42924174078329713 ) ) ;
#16888 = ORIENTED_EDGE ( 'NONE', *, *, #5430, .T. ) ;
#16889 = AXIS2_PLACEMENT_3D ( 'NONE', #30787, #7226, #23176 ) ;
#16890 = ORIENTED_EDGE ( 'NONE', *, *, #20981, .T. ) ;
#16891 = AXIS2_PLACEMENT_3D ( 'NONE', #20504, #13204, #350 ) ;
#16892 = CARTESIAN_POINT ( 'NONE',  ( 11.89321892218980103, -65.43602743108449715, -22.25048313876769868 ) ) ;
#16893 = ORIENTED_EDGE ( 'NONE', *, *, #1875, .F. ) ;
#16894 = CARTESIAN_POINT ( 'NONE',  ( 47.27830075994679504, -46.14751112267819622, -10.52819442205299971 ) ) ;
#16895 = CARTESIAN_POINT ( 'NONE',  ( 47.13393657218789912, 8.048130458325550407, -53.76789950451890121 ) ) ;
#16896 = CARTESIAN_POINT ( 'NONE',  ( 15.21636614235080032, -50.60415920577569437, -15.65000000000000036 ) ) ;
#16897 = ORIENTED_EDGE ( 'NONE', *, *, #42232, .T. ) ;
#16898 = ORIENTED_EDGE ( 'NONE', *, *, #4012, .F. ) ;
#16899 = DIRECTION ( 'NONE',  ( 0.000000000000000000, 0.000000000000000000, 1.000000000000000000 ) ) ;
#16900 = DIRECTION ( 'NONE',  ( 0.000000000000000000, -8.635067969306036542E-13, -1.000000000000000000 ) ) ;
#16901 = CARTESIAN_POINT ( 'NONE',  ( 61.25419824969329596, 14.37591664557439941, -47.68510568119449999 ) ) ;
#16902 = EDGE_CURVE ( 'NONE', #4255, #46423, #34505, .T. ) ;
#16903 = EDGE_CURVE ( 'NONE', #42065, #9584, #38723, .T. ) ;
#16904 = CARTESIAN_POINT ( 'NONE',  ( 51.64028867487969876, 13.97398019946970038, -12.35102539111250053 ) ) ;
#16905 = CARTESIAN_POINT ( 'NONE',  ( 14.06328963345900895, -23.32129707982529254, -68.37566384021832278 ) ) ;
#16906 = CARTESIAN_POINT ( 'NONE',  ( -8.011283399686980999, 13.73034950201170012, -5.061381373397489725 ) ) ;
#16907 = DIRECTION ( 'NONE',  ( 1.000000000000000000, 0.000000000000000000, 0.000000000000000000 ) ) ;
#16908 = CARTESIAN_POINT ( 'NONE',  ( 60.17742417565860080, 14.13461826297539936, -26.93847057974990022 ) ) ;
#16909 = CARTESIAN_POINT ( 'NONE',  ( 23.64653095223680168, -17.88504025480479953, -71.38086476703149685 ) ) ;
#16910 = EDGE_LOOP ( 'NONE', ( #48844, #8234, #40628, #17965 ) ) ;
#16911 = CARTESIAN_POINT ( 'NONE',  ( 16.13393739769620083, -15.61618894467929941, -28.45282021618999835 ) ) ;
#16912 = CARTESIAN_POINT ( 'NONE',  ( 22.90107427039792398, -15.30119754763367723, -76.83237175912924499 ) ) ;
#16913 = CARTESIAN_POINT ( 'NONE',  ( 12.62473742531370036, 34.22812217844730043, -47.06777474994189703 ) ) ;
#16914 = UNCERTAINTY_MEASURE_WITH_UNIT (LENGTH_MEASURE( 1.000000000000000082E-05 ), #16560, 'distance_accuracy_value', 'NONE');
#16915 = CARTESIAN_POINT ( 'NONE',  ( 72.38974652088450057, 1.200157260841289819, -69.84239033162910459 ) ) ;
#16916 = CARTESIAN_POINT ( 'NONE',  ( 41.33525829054640610, -39.68972903983045342, -79.53966819202405247 ) ) ;
#16917 = EDGE_CURVE ( 'NONE', #16944, #35239, #40333, .T. ) ;
#16918 = VECTOR ( 'NONE', #3858, 1000.000000000000000 ) ;
#16919 = AXIS2_PLACEMENT_3D ( 'NONE', #29489, #2244, #25546 ) ;
#16920 =( LENGTH_UNIT ( ) NAMED_UNIT ( * ) SI_UNIT ( .MILLI., .METRE. ) );
#16921 = CARTESIAN_POINT ( 'NONE',  ( 8.983363407049850480, -12.11911435556131522, -64.65261122085350110 ) ) ;
#16922 = ADVANCED_FACE ( 'NONE', ( #13829 ), #26906, .T. ) ;
#16923 = CARTESIAN_POINT ( 'NONE',  ( 47.15609049642320372, 23.45578653585020135, -74.81054835449099016 ) ) ;
#16924 = CARTESIAN_POINT ( 'NONE',  ( 49.51373360999449602, -53.70010315684200464, -54.78591011099970132 ) ) ;
#16925 = CARTESIAN_POINT ( 'NONE',  ( 68.13393739769620083, -42.61618894467930119, -71.15000000000000568 ) ) ;
#16926 = CARTESIAN_POINT ( 'NONE',  ( 23.94899987533918662, -16.86903691006758521, -33.55826008002186001 ) ) ;
#16927 = DIRECTION ( 'NONE',  ( 0.000000000000000000, 0.000000000000000000, -1.000000000000000000 ) ) ;
#16928 = CARTESIAN_POINT ( 'NONE',  ( 57.14903038794989953, 13.88381105532070059, -16.26185532857629923 ) ) ;
#16929 = VERTEX_POINT ( 'NONE', #35810 ) ;
#16930 = CARTESIAN_POINT ( 'NONE',  ( 9.035825935529210540, -17.87970567954010193, -45.96908178614949492 ) ) ;
#16931 = CARTESIAN_POINT ( 'NONE',  ( 63.97587150976810477, 1.409763019284750118, -61.55987120268989798 ) ) ;
#16932 = ORIENTED_EDGE ( 'NONE', *, *, #704, .F. ) ;
#16933 = DIRECTION ( 'NONE',  ( 1.000000000000000000, 0.000000000000000000, 0.000000000000000000 ) ) ;
#16934 = CARTESIAN_POINT ( 'NONE',  ( 61.16964974363630603, -45.44848929056309572, -47.43903885526919595 ) ) ;
#16935 = CARTESIAN_POINT ( 'NONE',  ( 44.13393739769620083, 4.883811055320659733, -44.64999999999999858 ) ) ;
#16936 = CARTESIAN_POINT ( 'NONE',  ( 46.02646716740153465, -43.52997999968917497, -5.570501089956091612 ) ) ;
#16938 = CARTESIAN_POINT ( 'NONE',  ( 44.66663217887202109, -33.16386166677794733, -44.71403636873775156 ) ) ;
#16937 = CARTESIAN_POINT ( 'NONE',  ( 42.57056998323533747, 8.591712343070616598, -73.57535562139177898 ) ) ;
#16939 = DIRECTION ( 'NONE',  ( 8.877345525967771201E-15, 1.000000000000000000, 1.071590398323126076E-14 ) ) ;
#16940 = CARTESIAN_POINT ( 'NONE',  ( 68.13393739769620083, -15.61618894467929941, -65.65000000000000568 ) ) ;
#16941 = EDGE_LOOP ( 'NONE', ( #39866, #5677 ) ) ;
#16942 = CARTESIAN_POINT ( 'NONE',  ( 84.24389573796460695, -44.17152221330420048, -47.41156961578170126 ) ) ;
#16943 = EDGE_LOOP ( 'NONE', ( #37206, #48014, #1463, #39306 ) ) ;
#16944 = VERTEX_POINT ( 'NONE', #15896 ) ;
#16945 = ORIENTED_EDGE ( 'NONE', *, *, #47880, .F. ) ;
#16946 = DIRECTION ( 'NONE',  ( 1.000000000000000000, 0.000000000000000000, 0.000000000000000000 ) ) ;
#16947 = CARTESIAN_POINT ( 'NONE',  ( 53.36551680243020002, -49.48411605007570557, -49.20677719568929831 ) ) ;
#16948 = CARTESIAN_POINT ( 'NONE',  ( 3.633937397696210159, -22.83306730954970121, -34.64999999999999858 ) ) ;
#16949 = CARTESIAN_POINT ( 'NONE',  ( 76.45881442385368132, -5.621145002420384174, -13.04994345818161072 ) ) ;
#16950 =( BOUNDED_CURVE ( )  B_SPLINE_CURVE ( 3, ( #40891, #17313, #9957, #29602 ),
 .UNSPECIFIED., .F., .T. ) 
 B_SPLINE_CURVE_WITH_KNOTS ( ( 4, 4 ),
 ( 0.7853981633974557175, 1.570796326794896558 ),
 .UNSPECIFIED. ) 
 CURVE ( )  GEOMETRIC_REPRESENTATION_ITEM ( )  RATIONAL_B_SPLINE_CURVE ( ( 1.000000000000000000, 0.9492530216741921212, 0.9492530216741921212, 1.000000000000000000 ) ) 
 REPRESENTATION_ITEM ( '' )  );
#16951 = DIRECTION ( 'NONE',  ( 0.000000000000000000, 0.000000000000000000, -1.000000000000000000 ) ) ;
#16952 = EDGE_LOOP ( 'NONE', ( #5695, #14504, #16687 ) ) ;
#16953 = EDGE_LOOP ( 'NONE', ( #34446, #31332, #24775, #46572, #24654, #20010 ) ) ;
#16954 = CARTESIAN_POINT ( 'NONE',  ( -0.1800306480951155419, 14.24857142054698755, -34.92293865398471553 ) ) ;
#16955 = CARTESIAN_POINT ( 'NONE',  ( 23.21788048646474323, -12.02478094032549727, -77.35840597922448580 ) ) ;
#16956 = CYLINDRICAL_SURFACE ( 'NONE', #34599, 0.4999999999999985012 ) ;
#16957 = CARTESIAN_POINT ( 'NONE',  ( 13.73527022026340028, -50.20735447812900532, -20.93080062776369843 ) ) ;
#16958 = CARTESIAN_POINT ( 'NONE',  ( 16.13393739769620083, -1.759782484128330049, -35.14999999999999858 ) ) ;
#16959 = CARTESIAN_POINT ( 'NONE',  ( 29.13393739769619728, 4.883811055320659733, -81.65000000000000568 ) ) ;
#16960 = CARTESIAN_POINT ( 'NONE',  ( 9.543053068164105923, -13.84498183095752744, -53.53615381170569520 ) ) ;
#16961 = AXIS2_PLACEMENT_3D ( 'NONE', #39763, #35308, #39511 ) ;
#16962 = ORIENTED_EDGE ( 'NONE', *, *, #15203, .F. ) ;
#16963 = CARTESIAN_POINT ( 'NONE',  ( 16.13393739769620083, -15.61618894467929941, -84.65000000000000568 ) ) ;
#16965 = CARTESIAN_POINT ( 'NONE',  ( 52.47683827954009672, -49.96152992937280857, -77.24560335664398281 ) ) ;
#16964 = VECTOR ( 'NONE', #41901, 1000.000000000000114 ) ;
#16966 = CARTESIAN_POINT ( 'NONE',  ( 9.543042969328475067, -17.38735874139107196, -47.36946835774308084 ) ) ;
#16967 = DIRECTION ( 'NONE',  ( -0.9441882088883221114, -0.3294064756440929775, 0.000000000000000000 ) ) ;
#16968 = EDGE_CURVE ( 'NONE', #19040, #3407, #32986, .T. ) ;
#16969 = CARTESIAN_POINT ( 'NONE',  ( 22.24317136614079971, -20.54203992805110346, -60.22848937760110033 ) ) ;
#16970 = ADVANCED_FACE ( 'NONE', ( #27930 ), #33627, .F. ) ;
#16971 = DIRECTION ( 'NONE',  ( 1.000000000000000000, 0.000000000000000000, 0.000000000000000000 ) ) ;
#16972 = CARTESIAN_POINT ( 'NONE',  ( 41.90536115952740204, -44.14555587430140093, -4.781910971784859576 ) ) ;
#16973 = DIRECTION ( 'NONE',  ( 0.000000000000000000, 0.000000000000000000, 1.000000000000000000 ) ) ;
#16974 = EDGE_CURVE ( 'NONE', #41755, #34714, #15385, .T. ) ;
#16975 = CARTESIAN_POINT ( 'NONE',  ( 71.69261393255278847, 0.9208623934718319637, -60.81910352240609541 ) ) ;
#16976 = CARTESIAN_POINT ( 'NONE',  ( 61.50420641992440096, -45.37395360146110335, -47.35413577371650007 ) ) ;
#16977 = CARTESIAN_POINT ( 'NONE',  ( 64.18261223640590174, 1.342504466669670160, -70.01010272223928155 ) ) ;
#16978 = CARTESIAN_POINT ( 'NONE',  ( -11.00461184790393432, 20.00401265374111759, -51.06967761013340379 ) ) ;
#16979 = CARTESIAN_POINT ( 'NONE',  ( 66.62369684436269779, 1.869841767515120212, -20.10141910231079976 ) ) ;
#16980 = EDGE_LOOP ( 'NONE', ( #22630, #24097 ) ) ;
#16981 = CARTESIAN_POINT ( 'NONE',  ( 13.60694591982639956, -51.71967070379349707, -74.96248001587449039 ) ) ;
#16982 = CARTESIAN_POINT ( 'NONE',  ( 47.32222669057270537, -54.70165496723960530, -54.63504270530570039 ) ) ;
#16983 = CARTESIAN_POINT ( 'NONE',  ( 0.3188167964973340207, 19.48786055945209839, -34.65000333314139169 ) ) ;
#16984 = PLANE ( 'NONE',  #11263 ) ;
#16985 = CARTESIAN_POINT ( 'NONE',  ( 24.04492723490795569, -15.60308853973110743, -55.50714508028963934 ) ) ;
#16986 = CARTESIAN_POINT ( 'NONE',  ( 22.58420829334310298, -19.63597092156729573, -32.14999999999999858 ) ) ;
#16987 = DIRECTION ( 'NONE',  ( 0.000000000000000000, 0.000000000000000000, -1.000000000000000000 ) ) ;
#16988 = ADVANCED_FACE ( 'NONE', ( #28184 ), #4092, .T. ) ;
#16989 = CARTESIAN_POINT ( 'NONE',  ( 47.82353814990229779, -54.39218320395399786, -54.71742302521079893 ) ) ;
#16991 = CARTESIAN_POINT ( 'NONE',  ( -10.40242566545200020, -42.83441872489630242, -6.165522616775290565 ) ) ;
#16990 = CARTESIAN_POINT ( 'NONE',  ( 14.03113113058140016, 19.93369484661189617, -22.86118033164979835 ) ) ;
#16992 = CARTESIAN_POINT ( 'NONE',  ( 56.32099966199259455, 19.34387771064809769, -52.90109585754750299 ) ) ;
#16993 = CARTESIAN_POINT ( 'NONE',  ( 48.44635283126329739, 22.88212911225959800, -54.78388658047989423 ) ) ;
#16994 = ORIENTED_EDGE ( 'NONE', *, *, #36590, .F. ) ;
#16995 = AXIS2_PLACEMENT_3D ( 'NONE', #33212, #44505, #8608 ) ;
#16996 = CARTESIAN_POINT ( 'NONE',  ( 9.399672476051630809, -17.71195494773369816, -61.75114295834970335 ) ) ;
#16997 = CIRCLE ( 'NONE', #14485, 2.000000000000000000 ) ;
#16998 = ORIENTED_EDGE ( 'NONE', *, *, #19351, .F. ) ;
#16999 = LINE ( 'NONE', #12541, #261 ) ;
#17000 = CARTESIAN_POINT ( 'NONE',  ( 9.367462981151710721, -15.61611677545310073, -63.45282021618999124 ) ) ;
#17001 = CARTESIAN_POINT ( 'NONE',  ( 0.4371248283887909647, -22.38658506580789975, -35.02873218748179340 ) ) ;
#17003 = CARTESIAN_POINT ( 'NONE',  ( 53.57711009519410084, 17.56838801165940112, -26.77252265506880136 ) ) ;
#17002 = CARTESIAN_POINT ( 'NONE',  ( 83.24078296369471275, 13.59326884860229967, -46.48094294254000403 ) ) ;
#17004 = CARTESIAN_POINT ( 'NONE',  ( 15.76846082554300033, -8.572824296172690595, -61.93631807992079530 ) ) ;
#17005 = CARTESIAN_POINT ( 'NONE',  ( 82.55417034916339958, -45.62620260807315020, -47.70637854188411353 ) ) ;
#17006 = CARTESIAN_POINT ( 'NONE',  ( 55.75440718692259878, -45.11618894467940066, -14.47054954719470032 ) ) ;
#17007 = FACE_OUTER_BOUND ( 'NONE', #18171, .T. ) ;
#17008 = ORIENTED_EDGE ( 'NONE', *, *, #9836, .F. ) ;
#17009 = ORIENTED_EDGE ( 'NONE', *, *, #7215, .F. ) ;
#17010 = CARTESIAN_POINT ( 'NONE',  ( 11.90346178786399811, -64.96824711458259571, -16.35924802167970427 ) ) ;
#17011 = CARTESIAN_POINT ( 'NONE',  ( 12.20877050462410018, 34.09266550635960158, -46.79949035583759809 ) ) ;
#17012 = CARTESIAN_POINT ( 'NONE',  ( 61.05618096262753625, -45.35086615659341902, -46.88538666599615112 ) ) ;
#17013 = CARTESIAN_POINT ( 'NONE',  ( 52.17625961327589579, -50.29609475764150517, -49.30498256536409940 ) ) ;
#17014 = CARTESIAN_POINT ( 'NONE',  ( 9.366937397696199596, -15.61618894467949836, -28.45282021618999835 ) ) ;
#17015 = EDGE_LOOP ( 'NONE', ( #28776, #20581, #3436, #40595 ) ) ;
#17016 = CARTESIAN_POINT ( 'NONE',  ( 11.13393739769619906, 24.07008072128950005, -43.74348518090240390 ) ) ;
#17017 = DIRECTION ( 'NONE',  ( 1.000000000000000000, 0.000000000000000000, 0.000000000000000000 ) ) ;
#17018 = DIRECTION ( 'NONE',  ( 0.000000000000000000, -1.000000000000000000, 0.000000000000000000 ) ) ;
#17019 = CARTESIAN_POINT ( 'NONE',  ( 71.90108049458170569, 1.446932438105679841, -69.97684691838689730 ) ) ;
#17020 = CARTESIAN_POINT ( 'NONE',  ( 50.03007040746729928, -48.61618473956929876, -76.14999999999999147 ) ) ;
#17021 = CARTESIAN_POINT ( 'NONE',  ( 22.33082320214449723, -53.70417188095220240, -34.65604926186109935 ) ) ;
#17022 = ORIENTED_EDGE ( 'NONE', *, *, #24110, .F. ) ;
#17023 = CARTESIAN_POINT ( 'NONE',  ( 17.16548900651949694, -43.89919387818898855, -61.51477253168923909 ) ) ;
#17024 = CYLINDRICAL_SURFACE ( 'NONE', #35079, 0.4999999999999994449 ) ;
#17025 = VERTEX_POINT ( 'NONE', #39232 ) ;
#17026 = LINE ( 'NONE', #13110, #48614 ) ;
#17027 = LINE ( 'NONE', #20933, #16964 ) ;
#17028 = CARTESIAN_POINT ( 'NONE',  ( 16.39598596041420109, -23.45951012094470300, -32.50186350533419954 ) ) ;
#17029 = EDGE_CURVE ( 'NONE', #13057, #46423, #16143, .T. ) ;
#17030 = CARTESIAN_POINT ( 'NONE',  ( 13.61605695543079975, -51.38252537174340517, -22.70458615691660142 ) ) ;
#17031 = FACE_OUTER_BOUND ( 'NONE', #39206, .T. ) ;
#17032 = CARTESIAN_POINT ( 'NONE',  ( 47.39374880179290273, -54.43861217925859819, -75.00425604315580586 ) ) ;
#17033 = ORIENTED_EDGE ( 'NONE', *, *, #18335, .T. ) ;
#17034 = CARTESIAN_POINT ( 'NONE',  ( 55.91593944087500034, 14.67229672235290039, -17.77972553223289864 ) ) ;
#17035 = CARTESIAN_POINT ( 'NONE',  ( 57.03355805182570037, -50.46038680774910290, -53.04057969670439832 ) ) ;
#17036 = CARTESIAN_POINT ( 'NONE',  ( 23.02517239383359993, -17.11733762112250190, -32.91545205119220441 ) ) ;
#17037 = CARTESIAN_POINT ( 'NONE',  ( 0.08961746015897585627, -22.88023971159056202, -34.70268271585497644 ) ) ;
#17038 = CARTESIAN_POINT ( 'NONE',  ( 46.73880816492100365, 22.29221772442059901, -76.02645024177060407 ) ) ;
#17039 = CYLINDRICAL_SURFACE ( 'NONE', #35955, 6.100000000000001421 ) ;
#17040 = DIRECTION ( 'NONE',  ( -1.000000000000000000, 2.473715676742926917E-14, 0.000000000000000000 ) ) ;
#17041 = CARTESIAN_POINT ( 'NONE',  ( 12.36320305067610015, 33.31445045643330616, -15.76422791930239953 ) ) ;
#17042 = CARTESIAN_POINT ( 'NONE',  ( 12.13393739769630031, -55.41568642894329599, -76.14999999999999147 ) ) ;
#17043 = EDGE_CURVE ( 'NONE', #32099, #31690, #38666, .T. ) ;
#17044 = FACE_BOUND ( 'NONE', #5627, .T. ) ;
#17045 = VECTOR ( 'NONE', #49491, 999.9999999999998863 ) ;
#17046 = DIRECTION ( 'NONE',  ( -1.000000000000000000, 0.000000000000000000, 0.000000000000000000 ) ) ;
#17048 = DIRECTION ( 'NONE',  ( 0.000000000000000000, 0.000000000000000000, -1.000000000000000000 ) ) ;
#17047 = PRESENTATION_STYLE_ASSIGNMENT (( #48758 ) ) ;
#17049 = EDGE_CURVE ( 'NONE', #17080, #13415, #7264, .T. ) ;
#17050 = CARTESIAN_POINT ( 'NONE',  ( 9.133937397696369587, 7.383811055320710359, -59.64999999999999147 ) ) ;
#17051 = CARTESIAN_POINT ( 'NONE',  ( -0.3561701380305670184, -63.29997699608469475, -50.35138997524259707 ) ) ;
#17052 = ORIENTED_EDGE ( 'NONE', *, *, #22376, .F. ) ;
#17053 = CARTESIAN_POINT ( 'NONE',  ( 52.74229065118059623, -49.71327796806070154, -48.57746011431329691 ) ) ;
#17054 = CARTESIAN_POINT ( 'NONE',  ( 16.13393739769620083, -15.61618894467929941, -18.08174999999999955 ) ) ;
#17055 = CARTESIAN_POINT ( 'NONE',  ( 49.72648160330889766, -53.64673639094029767, -55.11972614036120177 ) ) ;
#17056 = CARTESIAN_POINT ( 'NONE',  ( 13.29207020058240118, 19.63039169006109930, -21.61097671908079931 ) ) ;
#17057 = CARTESIAN_POINT ( 'NONE',  ( 57.41578767303399644, 14.06885415636270054, -25.91887996722570264 ) ) ;
#17058 = CARTESIAN_POINT ( 'NONE',  ( 23.17990796417380395, -15.92769928319889772, -32.46687572425449275 ) ) ;
#17059 = CARTESIAN_POINT ( 'NONE',  ( 50.92008762292839918, 19.20681001037759827, -76.16477590611239634 ) ) ;
#17060 = CARTESIAN_POINT ( 'NONE',  ( 53.50263409105239987, 18.15269513763240283, -49.11500990822519697 ) ) ;
#17061 = CARTESIAN_POINT ( 'NONE',  ( 71.17456103962899761, 1.276058558775519991, -70.60879112794539481 ) ) ;
#17062 = CARTESIAN_POINT ( 'NONE',  ( 40.36721523010999846, -44.88645108046029719, -4.296538310233220415 ) ) ;
#17063 = CARTESIAN_POINT ( 'NONE',  ( 46.81019908227018789, 22.25026678916544753, -76.02856692465805111 ) ) ;
#17064 = B_SPLINE_CURVE_WITH_KNOTS ( 'NONE', 3,
 ( #11672, #10899, #26865, #43130, #7224, #47831, #46812, #19004, #34981, #3288, #19261, #23429, #35250, #15344, #7480, #39454, #3552, #19522 ),
 .UNSPECIFIED., .F., .F.,
 ( 4, 2, 2, 2, 2, 2, 2, 2, 4 ),
 ( 0.000000000000000000, 0.06250019099276141188, 0.1250003819855228238, 0.1875005729782842356, 0.2500007639710456475, 0.3125009549638070316, 0.3750011459565684713, 0.4375013369493299109, 0.5000015279420912950 ),
 .UNSPECIFIED. ) ;
#17065 = ORIENTED_EDGE ( 'NONE', *, *, #43621, .F. ) ;
#17066 = CARTESIAN_POINT ( 'NONE',  ( 23.58315219326460266, -15.49012044018099843, -73.06195620990739314 ) ) ;
#17067 = ORIENTED_EDGE ( 'NONE', *, *, #45697, .T. ) ;
#17068 = CARTESIAN_POINT ( 'NONE',  ( 72.76396860142250489, 1.388715606738730068, -68.72506404892941134 ) ) ;
#17069 = CARTESIAN_POINT ( 'NONE',  ( 47.48443198299139567, -54.60544348543930226, -54.82495138136360424 ) ) ;
#17070 = CARTESIAN_POINT ( 'NONE',  ( 24.04460130197620416, -15.53725597405745518, -49.78915545177867585 ) ) ;
#17071 = DIRECTION ( 'NONE',  ( 1.000000000000000000, 0.000000000000000000, 0.000000000000000000 ) ) ;
#17072 = B_SPLINE_CURVE_WITH_KNOTS ( 'NONE', 3,
 ( #30610, #46632, #22744, #38762, #3115, #2857, #18821, #11237, #30863, #50808, #22999, #51063, #15163, #20106, #20356, #27456 ),
 .UNSPECIFIED., .F., .F.,
 ( 4, 2, 2, 2, 2, 2, 2, 4 ),
 ( -1.891009999999999936E-14, 0.07216186899279498912, 0.1546325764131530334, 0.2061767685508769932, 0.2319488646197389869, 0.2731842183299179605, 0.3391607842662049954, 0.4123535371017730267 ),
 .UNSPECIFIED. ) ;
#17073 = CARTESIAN_POINT ( 'NONE',  ( 57.31413766567600021, 18.54505573934330087, -52.15320908590850024 ) ) ;
#17074 = CARTESIAN_POINT ( 'NONE',  ( 52.98014233026830055, 18.34975111832529748, -48.77045026161920305 ) ) ;
#17075 = PLANE ( 'NONE',  #35134 ) ;
#17076 = CIRCLE ( 'NONE', #3683, 0.5000000000000004441 ) ;
#17077 = CARTESIAN_POINT ( 'NONE',  ( 72.00214641803239601, 1.437400661353670062, -61.36421840665509819 ) ) ;
#17078 = DIRECTION ( 'NONE',  ( -1.000000000000000000, 0.000000000000000000, 0.000000000000000000 ) ) ;
#17079 = CARTESIAN_POINT ( 'NONE',  ( 65.01767771978660448, 0.9212109678634080590, -70.77727272727270247 ) ) ;
#17080 = VERTEX_POINT ( 'NONE', #23471 ) ;
#17081 = ORIENTED_EDGE ( 'NONE', *, *, #4200, .T. ) ;
#17082 = CARTESIAN_POINT ( 'NONE',  ( 8.792282373222519709, -63.15413706425750462, -46.67070408018280148 ) ) ;
#17083 = CYLINDRICAL_SURFACE ( 'NONE', #44449, 6.766999999999998572 ) ;
#17084 = ORIENTED_EDGE ( 'NONE', *, *, #14445, .T. ) ;
#17085 = CARTESIAN_POINT ( 'NONE',  ( 9.366799914231096480, -15.30430012326571187, -71.86184190070434852 ) ) ;
#17086 = DIRECTION ( 'NONE',  ( 0.5547001962252313678, 0.000000000000000000, 0.8320502943378423888 ) ) ;
#17087 = DIRECTION ( 'NONE',  ( 1.000000000000000000, 0.000000000000000000, 0.000000000000000000 ) ) ;
#17088 = CARTESIAN_POINT ( 'NONE',  ( 52.30891881186520465, 19.23820029767140127, -76.54990093770538806 ) ) ;
#17089 = ORIENTED_EDGE ( 'NONE', *, *, #33034, .T. ) ;
#17090 = CARTESIAN_POINT ( 'NONE',  ( 30.13393739769619728, -38.61618894467930119, -72.14999999999999147 ) ) ;
#17091 = CARTESIAN_POINT ( 'NONE',  ( 9.366927855485558396, -14.73794263637672053, -71.49414492364064699 ) ) ;
#17092 = CARTESIAN_POINT ( 'NONE',  ( 23.64088913729917962, -13.06713224951208829, -43.68817631689275771 ) ) ;
#17093 = CARTESIAN_POINT ( 'NONE',  ( 9.048772758708359731, -19.83319761130199765, -54.62143916262379406 ) ) ;
#17094 = VECTOR ( 'NONE', #20927, 1000.000000000000000 ) ;
#17095 = EDGE_CURVE ( 'NONE', #566, #9786, #14905, .T. ) ;
#17096 = CARTESIAN_POINT ( 'NONE',  ( 53.70553476669380188, 20.08271752784780162, -75.56421356237311215 ) ) ;
#17097 = CARTESIAN_POINT ( 'NONE',  ( 42.64205722919412267, -37.72423225234104649, -77.10933407075954449 ) ) ;
#17098 = VERTEX_POINT ( 'NONE', #51544 ) ;
#17099 = CARTESIAN_POINT ( 'NONE',  ( 11.69299373377159945, -65.25245614431548802, -23.21666815710909759 ) ) ;
#17100 = CARTESIAN_POINT ( 'NONE',  ( 20.84347298952850025, -9.843237505908138729, -37.95047585818409885 ) ) ;
#17101 = CARTESIAN_POINT ( 'NONE',  ( 44.34217248106909892, 14.86060539202009956, -8.529414471301580036 ) ) ;
#17102 = CONICAL_SURFACE ( 'NONE', #9577, 1.715179901029911802, 0.08257045569470247703 ) ;
#17103 = CARTESIAN_POINT ( 'NONE',  ( 14.14316338426450059, 20.82672717200830093, -75.71427953954510315 ) ) ;
#17104 = AXIS2_PLACEMENT_3D ( 'NONE', #36187, #44315, #31983 ) ;
#17105 = CARTESIAN_POINT ( 'NONE',  ( 51.90728449415519918, 18.14319716981249897, -77.08408619744250245 ) ) ;
#17106 = CARTESIAN_POINT ( 'NONE',  ( 83.93027249483731111, -44.24138390648490571, -46.75947739037560069 ) ) ;
#17107 = CARTESIAN_POINT ( 'NONE',  ( 12.59142764408279902, -8.170831642673661577, -56.86630649184929354 ) ) ;
#17108 = ORIENTED_EDGE ( 'NONE', *, *, #29155, .F. ) ;
#17109 = CARTESIAN_POINT ( 'NONE',  ( 53.65698216514989838, -48.90957431119100107, -27.12425740866480339 ) ) ;
#17110 = CARTESIAN_POINT ( 'NONE',  ( 16.35031946893619903, -51.11201358154099950, -20.80740584792820158 ) ) ;
#17111 = CYLINDRICAL_SURFACE ( 'NONE', #25697, 10.00000000000000888 ) ;
#17113 = ADVANCED_FACE ( 'NONE', ( #11975 ), #48122, .T. ) ;
#17112 = CARTESIAN_POINT ( 'NONE',  ( 22.74102521302617319, -13.57078198115511825, -70.75098275705227024 ) ) ;
#17114 = AXIS2_PLACEMENT_3D ( 'NONE', #44737, #8841, #15928 ) ;
#17115 = CARTESIAN_POINT ( 'NONE',  ( 68.13393739769620083, -49.36618894467930829, -76.75000000000000000 ) ) ;
#17116 = EDGE_LOOP ( 'NONE', ( #36984, #13731, #40657, #33019 ) ) ;
#17117 = CARTESIAN_POINT ( 'NONE',  ( -7.621746992312569802, -45.29489141125190343, -5.208053594245360074 ) ) ;
#17118 = CARTESIAN_POINT ( 'NONE',  ( 47.23856716980339598, 23.53214383509299878, -54.65873215110720196 ) ) ;
#17119 = CARTESIAN_POINT ( 'NONE',  ( 63.26014808640670140, 1.265401080857970095, -62.43968814002079881 ) ) ;
#17120 = CARTESIAN_POINT ( 'NONE',  ( 18.08251218718402953, -41.66761415519155776, -34.89146800830128825 ) ) ;
#17121 = CARTESIAN_POINT ( 'NONE',  ( 11.09248976068989911, 33.92026768257339597, -17.64371789481230124 ) ) ;
#17122 = CARTESIAN_POINT ( 'NONE',  ( 9.366359996283680545, -15.61618532483699973, -43.84717978381009118 ) ) ;
#17123 = DIRECTION ( 'NONE',  ( -1.000000000000000000, 0.000000000000000000, 0.000000000000000000 ) ) ;
#17124 = LINE ( 'NONE', #49105, #15734 ) ;
#17125 = CARTESIAN_POINT ( 'NONE',  ( 57.08353988017420022, -47.57643501793450014, -48.30860928975249635 ) ) ;
#17126 = CARTESIAN_POINT ( 'NONE',  ( 10.72855169901638561, 33.70933666265226236, -18.17421237785139709 ) ) ;
#17127 = CIRCLE ( 'NONE', #29637, 5.251829701412240148 ) ;
#17128 = CARTESIAN_POINT ( 'NONE',  ( 54.44122174944140369, 20.40605896927280227, -54.00583347857779870 ) ) ;
#17129 = CARTESIAN_POINT ( 'NONE',  ( 22.72480946629929832, -17.38744196642808149, -60.53615444368751497 ) ) ;
#17130 = CARTESIAN_POINT ( 'NONE',  ( 9.367504675961500382, -15.61621390379479912, -67.84717978381009118 ) ) ;
#17131 = ORIENTED_EDGE ( 'NONE', *, *, #19140, .T. ) ;
#17132 = DIRECTION ( 'NONE',  ( -1.000000000000000000, 0.000000000000000000, 0.000000000000000000 ) ) ;
#17133 = CARTESIAN_POINT ( 'NONE',  ( 8.978915886419921222, 32.05342364452790349, -46.63388789120410394 ) ) ;
#17134 = CARTESIAN_POINT ( 'NONE',  ( 33.38393739769599478, 10.88381105532080007, -35.14999999999999858 ) ) ;
#17135 = VECTOR ( 'NONE', #11506, 1000.000000000000000 ) ;
#17136 = CARTESIAN_POINT ( 'NONE',  ( 67.87921200600509053, -30.71850411471519848, -17.86500106063319748 ) ) ;
#17137 = EDGE_LOOP ( 'NONE', ( #19561, #44648, #15073, #25556 ) ) ;
#17138 = CARTESIAN_POINT ( 'NONE',  ( 17.98151656396600018, 19.91124285304369934, -74.53071772762450564 ) ) ;
#17139 = ORIENTED_EDGE ( 'NONE', *, *, #16610, .F. ) ;
#17140 = VERTEX_POINT ( 'NONE', #15641 ) ;
#17141 = CARTESIAN_POINT ( 'NONE',  ( 47.96474501199910634, 23.16479111562100002, -55.26734477448599847 ) ) ;
#17142 = CIRCLE ( 'NONE', #31357, 1.500000000000001332 ) ;
#17143 = EDGE_LOOP ( 'NONE', ( #23369, #11355, #713, #37528 ) ) ;
#17144 = CARTESIAN_POINT ( 'NONE',  ( 10.36556321007419967, -63.68101588646130296, -45.87904799880939777 ) ) ;
#17145 = CARTESIAN_POINT ( 'NONE',  ( 56.71466712695590218, -45.83984592708740280, -26.16804175456279680 ) ) ;
#17146 = CARTESIAN_POINT ( 'NONE',  ( 19.78634850713340043, -21.45480175648069832, -81.23899999999999011 ) ) ;
#17147 = CARTESIAN_POINT ( 'NONE',  ( 61.62976647988480039, 13.89047783355900023, -46.42559179425300186 ) ) ;
#17148 = CARTESIAN_POINT ( 'NONE',  ( 64.45847733817470271, 1.439519383694989996, -61.26834731818230040 ) ) ;
#17149 = VERTEX_POINT ( 'NONE', #8029 ) ;
#17150 = VERTEX_POINT ( 'NONE', #39746 ) ;
#17151 = CARTESIAN_POINT ( 'NONE',  ( 20.51938203757293167, -21.13981406646989214, -35.13358212097380573 ) ) ;
#17152 = VERTEX_POINT ( 'NONE', #19822 ) ;
#17153 = CARTESIAN_POINT ( 'NONE',  ( 49.68658769026319533, -45.96991040253789862, -12.09272027885839940 ) ) ;
#17154 = EDGE_CURVE ( 'NONE', #50665, #4707, #27755, .T. ) ;
#17155 = DIRECTION ( 'NONE',  ( 0.000000000000000000, 0.000000000000000000, -1.000000000000000000 ) ) ;
#17156 = DIRECTION ( 'NONE',  ( 6.940534999999999567E-13, 2.999089000000000026E-13, 1.000000000000000000 ) ) ;
#17157 = VERTEX_POINT ( 'NONE', #19307 ) ;
#17158 = ADVANCED_FACE ( 'NONE', ( #43932 ), #15200, .F. ) ;
#17159 = VERTEX_POINT ( 'NONE', #40258 ) ;
#17160 = EDGE_CURVE ( 'NONE', #37505, #19930, #35020, .T. ) ;
#17161 = DIRECTION ( 'NONE',  ( 0.000000000000000000, 1.000000000000000000, 0.000000000000000000 ) ) ;
#17162 = CARTESIAN_POINT ( 'NONE',  ( 47.20319696544930110, -54.79145866998830172, -74.14999999999999147 ) ) ;
#17163 = CARTESIAN_POINT ( 'NONE',  ( 70.65074043265579462, 13.88381329038599965, -13.75217218087989934 ) ) ;
#17164 = EDGE_CURVE ( 'NONE', #22272, #10985, #34283, .T. ) ;
#17165 = CARTESIAN_POINT ( 'NONE',  ( 53.92601192165510327, 15.01257601730690006, -15.35060719856840095 ) ) ;
#17166 = CARTESIAN_POINT ( 'NONE',  ( 23.83903636936457104, -17.68687080692383162, -67.87566263859582705 ) ) ;
#17167 = B_SPLINE_CURVE_WITH_KNOTS ( 'NONE', 3,
 ( #8644, #7174, #19214, #31507, #35196, #47278, #27843, #36665, #4708, #40609, #31761, #15294, #51705, #43843, #20676, #23638, #31248, #39146 ),
 .UNSPECIFIED., .F., .F.,
 ( 4, 2, 2, 2, 2, 2, 2, 2, 4 ),
 ( 0.4999986293838318829, 0.5624988007108528976, 0.6249989720378739122, 0.6874991433648949268, 0.7499993146919159415, 0.8124994860189369561, 0.8749996573459579707, 0.9374998286729789854, 1.000000000000000000 ),
 .UNSPECIFIED. ) ;
#17168 = CARTESIAN_POINT ( 'NONE',  ( 16.39219225208960040, -22.66429958545629830, -63.33552157962199658 ) ) ;
#17169 = CARTESIAN_POINT ( 'NONE',  ( 58.59489568202110377, 14.12396963892440027, -26.25482318927760161 ) ) ;
#17170 = CARTESIAN_POINT ( 'NONE',  ( 23.09183490400689820, -19.24584601868189893, -73.44055697468560595 ) ) ;
#17171 = B_SPLINE_SURFACE_WITH_KNOTS ( 'NONE', 3, 3, ( 
 ( #44108, #7949, #8207, #32528, #7705, #32276, #43602, #23648, #39924, #40173 ),
 ( #12146, #4268, #16573, #20492, #51465, #27595, #35975, #51714, #15808, #94 ),
 ( #28100, #28358, #44362, #20238, #36228, #16323, #36483, #3514, #48047, #48298 ),
 ( #8467, #35473, #39664, #12395, #47791, #40426, #19981, #16066, #48556, #32022 ),
 ( #11897, #27852, #39414, #24414, #43853, #12664, #28617, #44618, #15564, #23388 ),
 ( #31518, #47536, #11633, #49090, #41462, #13695, #41722, #45660, #5317, #1377 ),
 ( #16846, #1895, #13193, #17872, #24934, #49347, #29655, #40687, #13948, #9763 ),
 ( #25714, #5829, #21792, #17110, #5057, #33843, #29907, #48818, #25202, #37015 ),
 ( #37800, #25457, #29405, #45405, #49859, #12926, #17364, #8724, #24674, #4787 ),
 ( #20755, #1114, #36742, #32795, #29142, #28882, #21273, #5578, #849, #33331 ) ),
 .UNSPECIFIED., .F., .F., .F.,
 ( 4, 1, 1, 1, 1, 1, 1, 4 ),
 ( 4, 2, 2, 2, 4 ),
 ( -7.647483565995659741E-05, 0.1428571428571430157, 0.2857142857142860315, 0.4285714285714289917, 0.5714285714285709528, 0.7142857142857139685, 0.8571428571428569843, 1.000068219203670061 ),
 ( -7.344577000600000058E-05, 0.1578379958887999868, 0.4200977637876570081, 0.7377509475170059838, 0.8959923838504209037 ),
 .UNSPECIFIED. ) ;
#17172 = VERTEX_POINT ( 'NONE', #13528 ) ;
#17173 = CARTESIAN_POINT ( 'NONE',  ( 60.26929283095309842, 14.55540890537130139, -47.49574889169500125 ) ) ;
#17174 = CARTESIAN_POINT ( 'NONE',  ( -11.32756405082269957, -41.88149022528619980, -6.268906610209949548 ) ) ;
#17175 = CARTESIAN_POINT ( 'NONE',  ( 15.36759650335590166, -50.68854986405820284, -15.64999996598500154 ) ) ;
#17177 = EDGE_CURVE ( 'NONE', #30462, #48001, #17417, .T. ) ;
#17176 = CARTESIAN_POINT ( 'NONE',  ( 72.73876892620509693, 1.391735898526219817, -68.90669866800179477 ) ) ;
#17178 = DIRECTION ( 'NONE',  ( 0.000000000000000000, 0.000000000000000000, -1.000000000000000000 ) ) ;
#17179 = CARTESIAN_POINT ( 'NONE',  ( 23.83903293615504637, -13.54548993678350222, -43.42431647374369419 ) ) ;
#17180 = CARTESIAN_POINT ( 'NONE',  ( 47.09613377138079926, 23.32416568916539745, -75.12131136925759733 ) ) ;
#17181 = CARTESIAN_POINT ( 'NONE',  ( 49.48213591681090406, -53.75081833664800257, -55.18208724449640101 ) ) ;
#17182 = CARTESIAN_POINT ( 'NONE',  ( 51.18395887421012702, -31.66627047883219248, -17.12905876552815698 ) ) ;
#17183 = CARTESIAN_POINT ( 'NONE',  ( 76.76118738540560571, -43.17102546891605641, -14.50675714471237931 ) ) ;
#17184 = CARTESIAN_POINT ( 'NONE',  ( 8.222281512103441159, -15.61614627842319969, -76.50766849176299900 ) ) ;
#17185 = ORIENTED_EDGE ( 'NONE', *, *, #25145, .F. ) ;
#17186 = CARTESIAN_POINT ( 'NONE',  ( 23.29546477256420189, -17.67026294465070180, -39.15625371467830007 ) ) ;
#17187 = CARTESIAN_POINT ( 'NONE',  ( 64.68898706140620902, 1.405464757956139898, -61.12024232051220451 ) ) ;
#17188 = EDGE_LOOP ( 'NONE', ( #20520, #9432, #30402, #36664, #42122, #24520 ) ) ;
#17189 = CARTESIAN_POINT ( 'NONE',  ( 0.1155611319282749960, -51.17475502668380472, -35.14999999933320396 ) ) ;
#17190 = CARTESIAN_POINT ( 'NONE',  ( 60.76390515915409907, -45.61011419412700008, -47.53678005598290213 ) ) ;
#17191 = CARTESIAN_POINT ( 'NONE',  ( 56.84932596551129791, 19.42421318737730118, -53.85230338955989993 ) ) ;
#17192 = CARTESIAN_POINT ( 'NONE',  ( 60.86353915101335588, -43.43619376203384519, -9.316164839326646074 ) ) ;
#17193 = CARTESIAN_POINT ( 'NONE',  ( 45.02421615755568496, 8.799843003901896665, -61.69522525134451740 ) ) ;
#17194 = EDGE_CURVE ( 'NONE', #14108, #19168, #28444, .T. ) ;
#17195 = VECTOR ( 'NONE', #12386, 1000.000000000000114 ) ;
#17196 = DIRECTION ( 'NONE',  ( 0.6522074047277948150, -0.2731766849828846100, 0.7071067811865450192 ) ) ;
#17197 = CYLINDRICAL_SURFACE ( 'NONE', #42030, 7.910999999999997812 ) ;
#17198 = VERTEX_POINT ( 'NONE', #45490 ) ;
#17199 = VECTOR ( 'NONE', #49713, 1000.000000000000000 ) ;
#17200 = ORIENTED_EDGE ( 'NONE', *, *, #17729, .T. ) ;
#17201 = EDGE_LOOP ( 'NONE', ( #8722, #39517 ) ) ;
#17202 = ORIENTED_EDGE ( 'NONE', *, *, #22352, .F. ) ;
#17203 = CARTESIAN_POINT ( 'NONE',  ( 61.65765287950929974, -45.18895564470849990, -46.92879811375530608 ) ) ;
#17204 = CARTESIAN_POINT ( 'NONE',  ( 63.43393739769620510, 1.383811055320669947, -68.50657137141709541 ) ) ;
#17205 = CARTESIAN_POINT ( 'NONE',  ( 54.49456226560189975, -51.49951853336879992, -53.42564530602280115 ) ) ;
#17206 = EDGE_LOOP ( 'NONE', ( #11707, #38945, #50829, #44076, #39507 ) ) ;
#17207 = ORIENTED_EDGE ( 'NONE', *, *, #51867, .T. ) ;
#17208 = PLANE ( 'NONE',  #25129 ) ;
#17209 = ORIENTED_EDGE ( 'NONE', *, *, #21679, .F. ) ;
#17210 = CARTESIAN_POINT ( 'NONE',  ( 56.52536539877740296, 19.51942783438209972, -53.84278118897309895 ) ) ;
#17211 = DIRECTION ( 'NONE',  ( -0.6522074047277899300, 0.2731766849828906607, 0.7071067811865471286 ) ) ;
#17212 = CARTESIAN_POINT ( 'NONE',  ( 16.13393739769620083, -15.61618894467929941, -17.89999999999999858 ) ) ;
#17213 = CARTESIAN_POINT ( 'NONE',  ( 8.812257860101720297, -63.26324333009419831, -46.67111697731629505 ) ) ;
#17214 = CYLINDRICAL_SURFACE ( 'NONE', #45199, 2.999999999999999556 ) ;
#17215 = ORIENTED_EDGE ( 'NONE', *, *, #48367, .T. ) ;
#17216 = CARTESIAN_POINT ( 'NONE',  ( 57.36123081458359962, -50.13537923174280309, -52.61896056486340001 ) ) ;
#17217 = CARTESIAN_POINT ( 'NONE',  ( 52.96724630752039786, -50.54849023173969869, -76.71296415157679860 ) ) ;
#17218 = CARTESIAN_POINT ( 'NONE',  ( 20.92206059044043442, -20.39804927675944413, -46.70260504768381793 ) ) ;
#17219 = CARTESIAN_POINT ( 'NONE',  ( -13.73674066540309902, -30.55263188852779876, -46.71145918530379504 ) ) ;
#17220 = AXIS2_PLACEMENT_3D ( 'NONE', #38731, #42660, #37684 ) ;
#17221 = EDGE_CURVE ( 'NONE', #31048, #7271, #16053, .T. ) ;
#17222 = CARTESIAN_POINT ( 'NONE',  ( 22.48828768571790349, -11.01086810800570071, -61.81286799887340067 ) ) ;
#17223 = CARTESIAN_POINT ( 'NONE',  ( 11.63393739769619906, -41.61618894467930119, -35.14999999999999858 ) ) ;
#17224 = CARTESIAN_POINT ( 'NONE',  ( 45.93003902655789972, 13.88381108677270070, -7.538626085152499989 ) ) ;
#17225 = CARTESIAN_POINT ( 'NONE',  ( 41.49029323204549513, -44.57544611689359471, -5.136314801332729552 ) ) ;
#17226 = CARTESIAN_POINT ( 'NONE',  ( 72.67981544229699864, 0.9952277120690129486, -61.73279890693489591 ) ) ;
#17227 = CARTESIAN_POINT ( 'NONE',  ( 61.43330014371199610, -45.44825325816589867, -47.47801797575630189 ) ) ;
#17228 = CARTESIAN_POINT ( 'NONE',  ( 64.42805214825888527, 1.442148388150169991, -70.01405398929449575 ) ) ;
#17229 = AXIS2_PLACEMENT_3D ( 'NONE', #9628, #13814, #17235 ) ;
#17230 = CARTESIAN_POINT ( 'NONE',  ( 8.428887576146721017, -13.54532682478765615, -40.87566479360295801 ) ) ;
#17231 = CARTESIAN_POINT ( 'NONE',  ( 66.86288126489500883, 1.795758268595449847, -19.74634579401690360 ) ) ;
#17232 = VERTEX_POINT ( 'NONE', #4350 ) ;
#17233 = CARTESIAN_POINT ( 'NONE',  ( 14.51934924390189963, -51.60940715663139855, -75.47164421335219231 ) ) ;
#17234 = CARTESIAN_POINT ( 'NONE',  ( 57.33058001265040104, 19.23207308441419983, -53.14947967088009761 ) ) ;
#17235 = DIRECTION ( 'NONE',  ( 0.8090169943749473402, 0.5877852522924732481, 0.000000000000000000 ) ) ;
#17236 = CARTESIAN_POINT ( 'NONE',  ( 83.92831069525388443, 12.99935915314664037, -46.72265495489138942 ) ) ;
#17237 = CARTESIAN_POINT ( 'NONE',  ( 16.13393739769620083, -15.61618894467929941, -32.14999999999999858 ) ) ;
#17238 = CARTESIAN_POINT ( 'NONE',  ( 22.49678922309009721, -12.58636461612879920, -32.14999999999999858 ) ) ;
#17239 = CARTESIAN_POINT ( 'NONE',  ( 55.45161425650417186, -46.01554884395809353, -16.61969664790585810 ) ) ;
#17240 = CARTESIAN_POINT ( 'NONE',  ( 47.73911847905110051, -54.48427846072730318, -54.99607381330790901 ) ) ;
#17242 = CARTESIAN_POINT ( 'NONE',  ( 14.54299284624212341, -46.73222572554120546, -21.73578643762710527 ) ) ;
#17241 = CARTESIAN_POINT ( 'NONE',  ( 22.90073451867936072, -15.61618922653637931, -60.45281425156898791 ) ) ;
#17243 = CARTESIAN_POINT ( 'NONE',  ( 56.33032549915870391, 19.43049768199900029, -53.07630012612180082 ) ) ;
#17244 = CARTESIAN_POINT ( 'NONE',  ( 48.71617454467180153, 22.66482838071829775, -54.49917290083569554 ) ) ;
#17245 = ORIENTED_EDGE ( 'NONE', *, *, #31202, .F. ) ;
#17246 = CARTESIAN_POINT ( 'NONE',  ( 22.18801361179549758, -19.23429899943539922, -63.01864585536749530 ) ) ;
#17247 = ORIENTED_EDGE ( 'NONE', *, *, #22464, .F. ) ;
#17248 = CIRCLE ( 'NONE', #46560, 1.999999999984542365 ) ;
#17249 = CARTESIAN_POINT ( 'NONE',  ( 2.501736331312110373, -5.785742375864720621, -34.68801049095939959 ) ) ;
#17250 = DIRECTION ( 'NONE',  ( 0.000000000000000000, 0.000000000000000000, 1.000000000000000000 ) ) ;
#17251 = CARTESIAN_POINT ( 'NONE',  ( 8.222963976945624864, -14.58044688709260761, -40.54933510552366016 ) ) ;
#17253 = CARTESIAN_POINT ( 'NONE',  ( 52.98397839259559561, 18.23000655168990036, -27.44922917074499935 ) ) ;
#17252 = CARTESIAN_POINT ( 'NONE',  ( 82.86439673227779679, 14.20358350717769902, -47.48719404937710209 ) ) ;
#17254 = EDGE_CURVE ( 'NONE', #30077, #24770, #37464, .T. ) ;
#17255 = CARTESIAN_POINT ( 'NONE',  ( 9.364619995196390434, -17.59581027231719830, -63.36225883906600131 ) ) ;
#17256 = DIRECTION ( 'NONE',  ( 0.8090169943749515591, 0.000000000000000000, 0.5877852522924675860 ) ) ;
#17257 = DIRECTION ( 'NONE',  ( 0.000000000000000000, 1.000000000000000000, 0.000000000000000000 ) ) ;
#17258 = CARTESIAN_POINT ( 'NONE',  ( 57.34776334542480214, -45.81180625069929846, -26.27178910182970029 ) ) ;
#17259 = VECTOR ( 'NONE', #41022, 1000.000000000000000 ) ;
#17260 = EDGE_CURVE ( 'NONE', #9581, #22075, #4228, .T. ) ;
#17261 = ORIENTED_EDGE ( 'NONE', *, *, #40229, .T. ) ;
#17262 = EDGE_LOOP ( 'NONE', ( #14659, #10539, #43700, #47464 ) ) ;
#17263 = EDGE_CURVE ( 'NONE', #35448, #51296, #31926, .T. ) ;
#17264 = CARTESIAN_POINT ( 'NONE',  ( 11.63839622732749923, -64.98507644367438729, -16.51998659930730184 ) ) ;
#17265 = CARTESIAN_POINT ( 'NONE',  ( 12.14904065733069949, 34.04125641336589325, -46.43067368610769563 ) ) ;
#17266 = CYLINDRICAL_SURFACE ( 'NONE', #43277, 3.000000000000005773 ) ;
#17267 = CYLINDRICAL_SURFACE ( 'NONE', #33558, 1.999999999999998224 ) ;
#17268 = DIRECTION ( 'NONE',  ( 0.000000000000000000, 0.000000000000000000, -1.000000000000000000 ) ) ;
#17269 = VECTOR ( 'NONE', #28169, 1000.000000000000000 ) ;
#17270 = ORIENTED_EDGE ( 'NONE', *, *, #49976, .T. ) ;
#17271 = CARTESIAN_POINT ( 'NONE',  ( -22.71231100707319683, -11.80202241275389952, -54.61438712110569327 ) ) ;
#17272 = AXIS2_PLACEMENT_3D ( 'NONE', #3079, #27163, #19824 ) ;
#17273 = CARTESIAN_POINT ( 'NONE',  ( 68.13393739769618662, -30.31618894467939995, -65.65000000000000568 ) ) ;
#17274 = DIRECTION ( 'NONE',  ( 0.000000000000000000, -1.000000000000000000, 0.000000000000000000 ) ) ;
#17275 = DIRECTION ( 'NONE',  ( 0.000000000000000000, 1.000000000000000000, 0.000000000000000000 ) ) ;
#17276 = CARTESIAN_POINT ( 'NONE',  ( 72.70940061843029412, 1.399433130755119992, -68.88399041770809106 ) ) ;
#17277 = CARTESIAN_POINT ( 'NONE',  ( 50.12047694534370379, -49.40224992130570314, -76.14999999999999147 ) ) ;
#17278 = LINE ( 'NONE', #5485, #17905 ) ;
#17279 = ORIENTED_EDGE ( 'NONE', *, *, #29715, .T. ) ;
#17280 = FACE_BOUND ( 'NONE', #28761, .T. ) ;
#17281 = CARTESIAN_POINT ( 'NONE',  ( 68.13393739769649926, -48.11618894468163887, -75.95000000000023022 ) ) ;
#17282 = ORIENTED_EDGE ( 'NONE', *, *, #45729, .T. ) ;
#17283 = CARTESIAN_POINT ( 'NONE',  ( 56.46551647426587550, -50.77616449088402817, -74.41179840258179468 ) ) ;
#17284 = CARTESIAN_POINT ( 'NONE',  ( 68.13393739769620083, 17.38381105532069881, -65.65000000000000568 ) ) ;
#17285 = EDGE_CURVE ( 'NONE', #28130, #21618, #8536, .T. ) ;
#17286 = CARTESIAN_POINT ( 'NONE',  ( 23.93509063369040035, -16.46986088408009863, -38.04718867978759533 ) ) ;
#17287 = CARTESIAN_POINT ( 'NONE',  ( 14.03111719544759950, -51.16607778725470013, -22.86119529785250037 ) ) ;
#17288 = FACE_OUTER_BOUND ( 'NONE', #27628, .T. ) ;
#17289 = CARTESIAN_POINT ( 'NONE',  ( 47.49946256140629686, -54.59426934545189880, -74.36173831268348522 ) ) ;
#17290 = ORIENTED_EDGE ( 'NONE', *, *, #50685, .T. ) ;
#17291 = CARTESIAN_POINT ( 'NONE',  ( 56.10793225295759612, 14.17759732785500049, -16.53469904412530056 ) ) ;
#17292 = CARTESIAN_POINT ( 'NONE',  ( 56.96373072582949959, -50.33643366695780230, -52.80952917442810701 ) ) ;
#17293 = AXIS2_PLACEMENT_3D ( 'NONE', #32026, #8472, #7444 ) ;
#17294 = CARTESIAN_POINT ( 'NONE',  ( 9.294981350531470454, -13.89246061358539919, -35.92577143160979602 ) ) ;
#17295 = DIRECTION ( 'NONE',  ( -0.4999999999999998890, 0.8660254037844387076, 0.000000000000000000 ) ) ;
#17296 = CIRCLE ( 'NONE', #46601, 3.000000000000004885 ) ;
#17297 = ORIENTED_EDGE ( 'NONE', *, *, #24022, .T. ) ;
#17298 = CARTESIAN_POINT ( 'NONE',  ( 47.45608139774180501, 23.29801033333230009, -74.72332766641309831 ) ) ;
#17299 = CARTESIAN_POINT ( 'NONE',  ( 20.02454065068388189, -55.10211906991936104, -18.88252341927455902 ) ) ;
#17300 = CARTESIAN_POINT ( 'NONE',  ( 75.12017559335848205, -26.67552810556109932, -11.65274274207780714 ) ) ;
#17301 = CARTESIAN_POINT ( 'NONE',  ( 12.36320305067610015, 33.31445045643330616, -15.76422791930239953 ) ) ;
#17302 = VECTOR ( 'NONE', #39361, 1000.000000000000000 ) ;
#17303 = CARTESIAN_POINT ( 'NONE',  ( 22.26030898828220117, -21.13465079480659981, -81.74105084582579650 ) ) ;
#17304 = AXIS2_PLACEMENT_3D ( 'NONE', #41548, #26067, #37888 ) ;
#17305 = CARTESIAN_POINT ( 'NONE',  ( 11.89321892218980103, -65.43602743108449715, -22.25048313876769868 ) ) ;
#17307 = CARTESIAN_POINT ( 'NONE',  ( 44.49954724606238443, -40.10969356087659321, -63.76892652563923036 ) ) ;
#17306 = CARTESIAN_POINT ( 'NONE',  ( 22.90093739769620029, -15.61618894467913243, -28.45282021618999835 ) ) ;
#17308 = CARTESIAN_POINT ( 'NONE',  ( 21.78494278233659998, -33.82423023735729828, -74.14999999999999147 ) ) ;
#17309 = CARTESIAN_POINT ( 'NONE',  ( -0.1608700869902630060, -61.64316105046779626, -48.65898601561310244 ) ) ;
#17310 = VERTEX_POINT ( 'NONE', #1719 ) ;
#17311 = CARTESIAN_POINT ( 'NONE',  ( 53.04797527815239988, -49.54715477933019940, -48.83268162150049818 ) ) ;
#17312 = CARTESIAN_POINT ( 'NONE',  ( 60.14908144350449959, -45.12251587736449210, -26.30467219823789904 ) ) ;
#17313 = CARTESIAN_POINT ( 'NONE',  ( 16.13393739769620083, -29.75141864441723882, -34.70142521051216278 ) ) ;
#17314 = CARTESIAN_POINT ( 'NONE',  ( 56.79136515448639955, 14.01381614805959863, -25.29529548441849940 ) ) ;
#17315 = CARTESIAN_POINT ( 'NONE',  ( 21.39220184427749771, -20.31653082709010150, -34.68500579403580275 ) ) ;
#17316 = CARTESIAN_POINT ( 'NONE',  ( 51.12155852695169500, 18.48105606206009810, -76.32652952292480109 ) ) ;
#17317 = CARTESIAN_POINT ( 'NONE',  ( 53.11153472725679592, 18.30627989090099916, -49.01452488218580328 ) ) ;
#17318 = CARTESIAN_POINT ( 'NONE',  ( 71.28621524259639841, 1.327322800621349996, -70.45801890699070213 ) ) ;
#17319 = DIRECTION ( 'NONE',  ( 0.000000000000000000, 0.000000000000000000, 1.000000000000000000 ) ) ;
#17320 = LINE ( 'NONE', #38793, #7234 ) ;
#17321 = ADVANCED_FACE ( 'NONE', ( #23346 ), #12699, .F. ) ;
#17322 = VECTOR ( 'NONE', #2391, 1000.000000000000000 ) ;
#17323 = VERTEX_POINT ( 'NONE', #51168 ) ;
#17324 = CARTESIAN_POINT ( 'NONE',  ( 9.004889010588179588, -17.78029694363090130, -77.97352993585178638 ) ) ;
#17325 = EDGE_CURVE ( 'NONE', #42078, #40450, #24905, .T. ) ;
#17326 = CARTESIAN_POINT ( 'NONE',  ( 73.07317914023670369, 1.000225705806889964, -69.04426126474540126 ) ) ;
#17327 = CARTESIAN_POINT ( 'NONE',  ( 47.40072637641420528, -54.65652856110890667, -54.81947631438220014 ) ) ;
#17328 = CARTESIAN_POINT ( 'NONE',  ( 14.34562453388149805, -7.882998418872065649, -49.21996134945802481 ) ) ;
#17329 = CARTESIAN_POINT ( 'NONE',  ( 73.22214118178139586, 1.102581332775290024, -62.55748568903110396 ) ) ;
#17330 = LINE ( 'NONE', #806, #10121 ) ;
#17331 = LINE ( 'NONE', #33294, #10403 ) ;
#17332 = CARTESIAN_POINT ( 'NONE',  ( 2.528703657258640103, -25.32162763854480048, -34.65800258959620095 ) ) ;
#17333 = CARTESIAN_POINT ( 'NONE',  ( 71.92139930889749166, 1.254613999359859955, -61.09530678593939967 ) ) ;
#17334 = CARTESIAN_POINT ( 'NONE',  ( 8.222546438703959737, -15.61603098320130201, -50.50766849176299900 ) ) ;
#17335 = VERTEX_POINT ( 'NONE', #50199 ) ;
#17336 = CARTESIAN_POINT ( 'NONE',  ( 65.05161336175061138, 1.196343736543249880, -70.67573229508370503 ) ) ;
#17337 = ORIENTED_EDGE ( 'NONE', *, *, #40177, .T. ) ;
#17338 = CARTESIAN_POINT ( 'NONE',  ( 9.745678311054680520, -63.30192500947659795, -46.29763742019599704 ) ) ;
#17339 = CARTESIAN_POINT ( 'NONE',  ( 15.67962062535580081, -50.86266781815560023, -15.65622421709140077 ) ) ;
#17340 = ORIENTED_EDGE ( 'NONE', *, *, #19027, .F. ) ;
#17341 = CARTESIAN_POINT ( 'NONE',  ( 11.13393739477719890, -63.63465712356870796, -43.78329177822379847 ) ) ;
#17342 = CARTESIAN_POINT ( 'NONE',  ( 22.04684518689748529, -12.20819050132398154, -70.28615616242308306 ) ) ;
#17343 = FACE_OUTER_BOUND ( 'NONE', #45377, .T. ) ;
#17344 = CARTESIAN_POINT ( 'NONE',  ( 52.19402247633719583, 19.67376017629629814, -76.20338399122979922 ) ) ;
#17345 = ORIENTED_EDGE ( 'NONE', *, *, #33638, .T. ) ;
#17346 = LINE ( 'NONE', #33313, #51076 ) ;
#17347 = CIRCLE ( 'NONE', #44116, 18.00000000000000355 ) ;
#17348 = CARTESIAN_POINT ( 'NONE',  ( 12.76916528160270836, -22.79959822632163835, -66.14710272702825478 ) ) ;
#17349 = EDGE_CURVE ( 'NONE', #7773, #10572, #9374, .T. ) ;
#17350 = CARTESIAN_POINT ( 'NONE',  ( 20.57352930747810049, -8.668330013286569269, -57.47332068091419188 ) ) ;
#17351 = CARTESIAN_POINT ( 'NONE',  ( 10.29045043687441918, -12.08236487558636263, -55.62624849296779672 ) ) ;
#17352 = CARTESIAN_POINT ( 'NONE',  ( 42.30362988516652223, -37.67198729731079254, -78.80153692937045662 ) ) ;
#17353 = ADVANCED_FACE ( 'NONE', ( #37886 ), #5888, .T. ) ;
#17354 = ORIENTED_EDGE ( 'NONE', *, *, #22169, .T. ) ;
#17355 = CARTESIAN_POINT ( 'NONE',  ( 57.17168871552530618, -45.85041182722559228, -26.25507473453999907 ) ) ;
#17356 = CARTESIAN_POINT ( 'NONE',  ( 20.10156355740380008, -9.310268198115061011, -41.91142241136510194 ) ) ;
#17357 = CARTESIAN_POINT ( 'NONE',  ( 10.83099421739539991, -11.18954735718040006, -32.14999999999999858 ) ) ;
#17358 = CARTESIAN_POINT ( 'NONE',  ( 13.48116298479809849, 20.36471648394369893, -74.34810712130391153 ) ) ;
#17359 = CARTESIAN_POINT ( 'NONE',  ( 17.63529210099531142, -51.92835184178156993, -75.76245441612823583 ) ) ;
#17360 = DIRECTION ( 'NONE',  ( -0.8660254037844381525, -0.5000000000000007772, 0.000000000000000000 ) ) ;
#17361 = CARTESIAN_POINT ( 'NONE',  ( 16.57604039667560158, -7.382886712447779942, -57.02474435397640207 ) ) ;
#17362 = ORIENTED_EDGE ( 'NONE', *, *, #28279, .T. ) ;
#17363 = CARTESIAN_POINT ( 'NONE',  ( 53.11249465950879767, -49.29926820387549924, -27.16890043460400150 ) ) ;
#17364 = CARTESIAN_POINT ( 'NONE',  ( 15.45006552727480020, -51.11619292586900087, -21.87030236029440289 ) ) ;
#17365 = CARTESIAN_POINT ( 'NONE',  ( 12.63912502739619903, 33.58996157896420698, -16.00788927292039787 ) ) ;
#17366 = LINE ( 'NONE', #13952, #4553 ) ;
#17367 = DIRECTION ( 'NONE',  ( -0.3487035033511760029, -0.9372330909387569520, 0.000000000000000000 ) ) ;
#17368 = EDGE_LOOP ( 'NONE', ( #15120, #31677, #31347, #9480 ) ) ;
#17369 = CARTESIAN_POINT ( 'NONE',  ( -11.32734370190460105, -41.88171845330919751, -6.430192534648670133 ) ) ;
#17370 = CARTESIAN_POINT ( 'NONE',  ( 47.21062522706190379, 23.55319570774130256, -54.63464825132839309 ) ) ;
#17371 = CIRCLE ( 'NONE', #5675, 0.9999999999999991118 ) ;
#17372 = CARTESIAN_POINT ( 'NONE',  ( 56.50535457420483709, -50.75957590060649238, -53.84464170001397321 ) ) ;
#17373 = CARTESIAN_POINT ( 'NONE',  ( 63.49388541862201407, 1.387412027389909985, -62.60488565353588797 ) ) ;
#17374 = CARTESIAN_POINT ( 'NONE',  ( 56.02488392748924895, 15.50430221806558606, -26.35754376592503689 ) ) ;
#17375 = CARTESIAN_POINT ( 'NONE',  ( 11.63826667102929946, 34.15960232121609863, -17.83149736357780313 ) ) ;
#17376 = DIRECTION ( 'NONE',  ( 0.000000000000000000, 0.000000000000000000, -1.000000000000000000 ) ) ;
#17377 = FACE_OUTER_BOUND ( 'NONE', #46020, .T. ) ;
#17378 = FACE_OUTER_BOUND ( 'NONE', #27313, .T. ) ;
#17379 = CARTESIAN_POINT ( 'NONE',  ( 57.73173547914959158, -47.11702968912669576, -47.92373006181999529 ) ) ;
#17380 = CARTESIAN_POINT ( 'NONE',  ( 53.40280527584940273, 17.93096761773750103, -27.32835562702450005 ) ) ;
#17381 = EDGE_CURVE ( 'NONE', #25261, #44616, #5443, .T. ) ;
#17382 = CIRCLE ( 'NONE', #3174, 4.960803362786369242 ) ;
#17383 = CARTESIAN_POINT ( 'NONE',  ( 55.90187133018510224, 19.50246215684880013, -52.91463811559199826 ) ) ;
#17384 = CARTESIAN_POINT ( 'NONE',  ( 63.47373889294079419, 1.158192848841449907, -69.37188851713681004 ) ) ;
#17385 = CARTESIAN_POINT ( 'NONE',  ( 55.00116069800729690, 13.88381105532070059, -13.90662172087169957 ) ) ;
#17386 = ORIENTED_EDGE ( 'NONE', *, *, #9913, .T. ) ;
#17387 = CARTESIAN_POINT ( 'NONE',  ( 18.86789271246039945, 20.55440458018300021, -15.81497037201279987 ) ) ;
#17388 = CARTESIAN_POINT ( 'NONE',  ( 9.745662885843259460, 32.06938234726919745, -46.29763386374680323 ) ) ;
#17389 = DIRECTION ( 'NONE',  ( 0.000000000000000000, 0.000000000000000000, 1.000000000000000000 ) ) ;
#17390 = B_SPLINE_CURVE_WITH_KNOTS ( 'NONE', 3,
 ( #37380, #1483, #30275, #14049, #17467, #49705, #49452, #13546, #38157, #18230, #34195, #50214, #14306, #12406, #33343, #9524, #40956, #5073 ),
 .UNSPECIFIED., .F., .F.,
 ( 4, 2, 2, 2, 2, 2, 2, 2, 4 ),
 ( 0.4999987081369468012, 0.5624988696198284233, 0.6249990311027100454, 0.6874991925855915564, 0.7499993540684731785, 0.8124995155513548006, 0.8749996770342365338, 0.9374998385171182669, 1.000000000000000000 ),
 .UNSPECIFIED. ) ;
#17391 = CARTESIAN_POINT ( 'NONE',  ( 67.25969285220541849, -30.55435842736649832, -17.44085799406789761 ) ) ;
#17392 = CARTESIAN_POINT ( 'NONE',  ( 18.03195613579949708, 20.10714342530040000, -75.06145659859170394 ) ) ;
#17393 = EDGE_LOOP ( 'NONE', ( #20310, #51234, #11665, #33639 ) ) ;
#17394 = ORIENTED_EDGE ( 'NONE', *, *, #33300, .T. ) ;
#17395 = CARTESIAN_POINT ( 'NONE',  ( 49.22498099147640005, 22.62797864033339934, -55.23666898610209586 ) ) ;
#17396 = EDGE_LOOP ( 'NONE', ( #3165, #21300, #49134, #35753 ) ) ;
#17397 = CARTESIAN_POINT ( 'NONE',  ( 9.877817271165479696, -63.39606316702139566, -46.22144567296060558 ) ) ;
#17398 = CARTESIAN_POINT ( 'NONE',  ( 57.43249943431290205, -45.60969068493010070, -26.20294208203680242 ) ) ;
#17399 = DIRECTION ( 'NONE',  ( 0.000000000000000000, 0.000000000000000000, -1.000000000000000000 ) ) ;
#17400 =( BOUNDED_SURFACE ( )  B_SPLINE_SURFACE ( 2, 2, ( 
 ( #48064, #28119, #32041, #51480, #12163, #27868, #44125, #23916, #23408 ),
 ( #39941, #8223, #11134, #43619, #16082, #39428, #31790, #3528, #27613 ),
 ( #19499, #3264, #50957, #40194, #4284, #7455, #47047, #15319, #34958 ) ),
 .UNSPECIFIED., .F., .T., .T. ) 
 B_SPLINE_SURFACE_WITH_KNOTS ( ( 3, 3 ),
 ( 3, 2, 2, 2, 3 ),
 ( -0.06696923885014899325, 0.06696923885011449307 ),
 ( -3.141592653589790007, -1.570796326794899889, 0.000000000000000000, 1.570796326794899889, 3.141592653589790007 ),
 .UNSPECIFIED. ) 
 GEOMETRIC_REPRESENTATION_ITEM ( )  RATIONAL_B_SPLINE_SURFACE ( (
 ( 1.000000000000000000, 0.7071067811865480168, 1.000000000000000000, 0.7071067811865480168, 1.000000000000000000, 0.7071067811865480168, 1.000000000000000000, 0.7071067811865480168, 1.000000000000000000),
 ( 0.9977583984878120038, 0.7055217295565610058, 0.9977583984878120038, 0.7055217295565610058, 0.9977583984878120038, 0.7055217295565610058, 0.9977583984878120038, 0.7055217295565610058, 0.9977583984878120038),
 ( 1.000000000000000000, 0.7071067811865480168, 1.000000000000000000, 0.7071067811865480168, 1.000000000000000000, 0.7071067811865480168, 1.000000000000000000, 0.7071067811865480168, 1.000000000000000000) ) ) 
 REPRESENTATION_ITEM ( '' )  SURFACE ( )  );
#17401 = CARTESIAN_POINT ( 'NONE',  ( 61.73009041877960357, 13.88381044681140075, -46.43160995025269244 ) ) ;
#17402 = CARTESIAN_POINT ( 'NONE',  ( 17.16548900651931220, 12.66681598883031867, -61.51477253168783221 ) ) ;
#17403 = VERTEX_POINT ( 'NONE', #42109 ) ;
#17404 = CARTESIAN_POINT ( 'NONE',  ( 75.24562878474803540, 2.899702436808165640, -12.26857522025693825 ) ) ;
#17405 = EDGE_LOOP ( 'NONE', ( #16409, #45657, #5668, #16755 ) ) ;
#17406 = CARTESIAN_POINT ( 'NONE',  ( 53.14291664956020611, -45.11618894460600160, -12.84078445876880004 ) ) ;
#17407 = CARTESIAN_POINT ( 'NONE',  ( 24.04491986954906935, -15.63419043126502217, -33.79305392942131192 ) ) ;
#17408 = ADVANCED_FACE ( 'NONE', ( #46054 ), #22168, .F. ) ;
#17409 = CARTESIAN_POINT ( 'NONE',  ( 9.366602974803960535, -15.61605382581650048, -49.84717978381009118 ) ) ;
#17410 = EDGE_LOOP ( 'NONE', ( #51283, #14595, #12486, #43897 ) ) ;
#17411 = CARTESIAN_POINT ( 'NONE',  ( -35.14957093606200544, -34.88797072816932143, -65.33131159457242632 ) ) ;
#17412 = CARTESIAN_POINT ( 'NONE',  ( 47.18055146300900304, -54.80119377569329941, -74.36335264244719667 ) ) ;
#17413 = CARTESIAN_POINT ( 'NONE',  ( 60.83513156569119928, 14.48683582043410034, -47.74920551991019835 ) ) ;
#17414 = CARTESIAN_POINT ( 'NONE',  ( 47.61773923874600456, 14.33581883698849957, -10.25420216154219943 ) ) ;
#17415 = ADVANCED_FACE ( 'NONE', ( #5951 ), #25517, .T. ) ;
#17416 = AXIS2_PLACEMENT_3D ( 'NONE', #601, #44631, #16586 ) ;
#17417 = B_SPLINE_CURVE_WITH_KNOTS ( 'NONE', 3,
 ( #20318, #8808, #1458, #36307, #28966, #13268, #17448, #25285, #16404, #40513, #1200, #672, #49431, #40770, #4871, #29485 ),
 .UNSPECIFIED., .F., .F.,
 ( 4, 2, 2, 2, 2, 2, 2, 4 ),
 ( -1.909583999999999989E-14, 0.4484665168913320454, 0.8527180250750849844, 1.105375217689929856, 1.263285963074209928, 1.579107453842770070, 2.084421839072459814, 2.526571926148439839 ),
 .UNSPECIFIED. ) ;
#17418 = DIRECTION ( 'NONE',  ( 0.000000000000000000, 0.000000000000000000, -1.000000000000000000 ) ) ;
#17419 =( REPRESENTATION_RELATIONSHIP ('NONE','NONE', #29764, #4374 ) REPRESENTATION_RELATIONSHIP_WITH_TRANSFORMATION ( #4447 )SHAPE_REPRESENTATION_RELATIONSHIP( ) );
#17420 = DIRECTION ( 'NONE',  ( -0.9899494936611664686, 0.000000000000000000, 0.1414213562373098920 ) ) ;
#17421 = CARTESIAN_POINT ( 'NONE',  ( 10.62796209095821354, 24.00384274327042888, -21.20043923476212910 ) ) ;
#17422 = CARTESIAN_POINT ( 'NONE',  ( 59.23839464417140022, 13.99532105124600001, -26.26701623619180026 ) ) ;
#17423 = CARTESIAN_POINT ( 'NONE',  ( 8.698833068341928154, -13.10501953685350074, -74.39118414744899610 ) ) ;
#17424 = ORIENTED_EDGE ( 'NONE', *, *, #110, .F. ) ;
#17425 = CARTESIAN_POINT ( 'NONE',  ( 53.58118161341838004, 18.18361553717124579, -49.23682030730962822 ) ) ;
#17426 = CARTESIAN_POINT ( 'NONE',  ( -10.62062192548610007, -41.45185578373610014, -4.375821978402089307 ) ) ;
#17427 = CARTESIAN_POINT ( 'NONE',  ( 22.90076005816202809, -15.61619656631699193, -74.84717351858182610 ) ) ;
#17428 = B_SPLINE_CURVE_WITH_KNOTS ( 'NONE', 3,
 ( #15262, #23347, #7146, #6890, #23605, #31218, #39116, #3210, #6622, #26517, #46993 ),
 .UNSPECIFIED., .F., .F.,
 ( 4, 1, 1, 1, 1, 1, 1, 1, 4 ),
 ( 0.000000000000000000, 0.1250000000000000000, 0.2500000000000000000, 0.3750000000000000000, 0.5000000000000000000, 0.6250000000000000000, 0.7500000000000000000, 0.8750000000000000000, 1.000000000000000000 ),
 .UNSPECIFIED. ) ;
#17429 = CARTESIAN_POINT ( 'NONE',  ( 72.62341919120400746, 1.419970371292329947, -69.11014492780159912 ) ) ;
#17430 = CARTESIAN_POINT ( 'NONE',  ( 14.28038400710293487, -41.76263555408612405, -34.79644660940672907 ) ) ;
#17431 = CARTESIAN_POINT ( 'NONE',  ( 47.38033551211754713, -54.20286183681685088, -75.36291177508510941 ) ) ;
#17432 = CARTESIAN_POINT ( 'NONE',  ( 49.57777172146020206, -53.70720745051439593, -55.02952289821030263 ) ) ;
#17433 = CARTESIAN_POINT ( 'NONE',  ( 51.20713017066216821, -31.70237965034690575, -17.16575294922130368 ) ) ;
#17434 = EDGE_CURVE ( 'NONE', #50028, #9032, #50748, .T. ) ;
#17435 = DIRECTION ( 'NONE',  ( 8.462868000000000073E-18, -1.066343000000000058E-17, 1.000000000000000000 ) ) ;
#17436 = CARTESIAN_POINT ( 'NONE',  ( 18.78670792145450008, -51.59710020169690381, -74.14993170018701107 ) ) ;
#17437 = CARTESIAN_POINT ( 'NONE',  ( 57.50723796702470025, 13.88381105532070059, -17.67940111168049810 ) ) ;
#17438 = ORIENTED_EDGE ( 'NONE', *, *, #27626, .T. ) ;
#17439 = ADVANCED_FACE ( 'NONE', ( #3308 ), #45348, .T. ) ;
#17440 = CARTESIAN_POINT ( 'NONE',  ( 8.738279572154599606, -16.51671082994739947, -48.02877399380358980 ) ) ;
#17441 = EDGE_CURVE ( 'NONE', #44194, #14297, #46862, .T. ) ;
#17442 = CARTESIAN_POINT ( 'NONE',  ( 64.14331810339599826, 1.010053820890950194, -61.16840880232479805 ) ) ;
#17443 = ORIENTED_EDGE ( 'NONE', *, *, #7869, .T. ) ;
#17444 = CARTESIAN_POINT ( 'NONE',  ( 0.07473234491190286488, -51.15631565001774561, -35.09349432427395499 ) ) ;
#17445 = CARTESIAN_POINT ( 'NONE',  ( 60.90359205743109783, -45.68240515407420332, -47.72054110957569861 ) ) ;
#17446 = FACE_OUTER_BOUND ( 'NONE', #30990, .T. ) ;
#17447 = COLOUR_RGB ( '', 0.08235294, 0.09019608, 0.10196078) ;
#17448 = CARTESIAN_POINT ( 'NONE',  ( 12.98727014690059889, 18.78214035054229925, -21.05372677721659969 ) ) ;
#17450 = CARTESIAN_POINT ( 'NONE',  ( 18.20469504372072223, -7.911110918348574828, -35.37566324252046002 ) ) ;
#17449 = CARTESIAN_POINT ( 'NONE',  ( 44.64173248798216775, 8.772533778425639639, -63.54959783062244583 ) ) ;
#17451 = EDGE_CURVE ( 'NONE', #5164, #39608, #9601, .T. ) ;
#17452 = CARTESIAN_POINT ( 'NONE',  ( 22.79638959291578360, -13.83202789291152968, -60.76326040478846124 ) ) ;
#17453 = CARTESIAN_POINT ( 'NONE',  ( 16.13393739769620083, -15.61618894467929941, -9.721247897589949005 ) ) ;
#17454 = VERTEX_POINT ( 'NONE', #47848 ) ;
#17455 = ORIENTED_EDGE ( 'NONE', *, *, #16786, .T. ) ;
#17456 = ORIENTED_EDGE ( 'NONE', *, *, #27469, .F. ) ;
#17457 = ORIENTED_EDGE ( 'NONE', *, *, #45482, .F. ) ;
#17458 = CARTESIAN_POINT ( 'NONE',  ( 61.55597312494089834, -45.14216928434709786, -46.59921423066880664 ) ) ;
#17459 = CARTESIAN_POINT ( 'NONE',  ( -11.32734372065470119, 10.64934054434680100, -6.430561461456250072 ) ) ;
#17460 = CARTESIAN_POINT ( 'NONE',  ( 22.52295300047549276, -13.38580680388945332, -80.74026669357201058 ) ) ;
#17461 = ORIENTED_EDGE ( 'NONE', *, *, #23203, .T. ) ;
#17462 = ORIENTED_EDGE ( 'NONE', *, *, #44104, .F. ) ;
#17463 = VERTEX_POINT ( 'NONE', #398 ) ;
#17464 = CARTESIAN_POINT ( 'NONE',  ( 10.72251481771434811, -19.77472772824552294, -73.24445191944960243 ) ) ;
#17465 = CARTESIAN_POINT ( 'NONE',  ( 13.47700760496488925, -9.082944478799559462, -46.22423246988032020 ) ) ;
#17466 = CYLINDRICAL_SURFACE ( 'NONE', #25340, 0.4999999999999993894 ) ;
#17467 = CARTESIAN_POINT ( 'NONE',  ( 21.54528854056280451, -19.77481887735858024, -52.66115150407350143 ) ) ;
#17468 = EDGE_CURVE ( 'NONE', #42744, #22490, #48103, .T. ) ;
#17469 = LINE ( 'NONE', #41826, #46032 ) ;
#17470 = VERTEX_POINT ( 'NONE', #36549 ) ;
#17471 = FACE_OUTER_BOUND ( 'NONE', #11560, .T. ) ;
#17472 = CARTESIAN_POINT ( 'NONE',  ( 52.64727089593759501, -50.60815907346550091, -76.52291747471450378 ) ) ;
#17473 = CARTESIAN_POINT ( 'NONE',  ( 17.82378463084905462, -22.18374869735217558, -46.87269942184638438 ) ) ;
#17474 = DIRECTION ( 'NONE',  ( 0.04332574401194498603, 0.02501412996813699718, -0.9987478026047158508 ) ) ;
#17475 = CARTESIAN_POINT ( 'NONE',  ( 8.908058192899041217, -12.55458522942449839, -65.14006310354548646 ) ) ;
#17476 = CARTESIAN_POINT ( 'NONE',  ( 8.644451877215649560, 17.52530927293000218, -35.10565360069929852 ) ) ;
#17477 = CARTESIAN_POINT ( 'NONE',  ( 45.63996532923849969, 13.90945843731140030, -7.778295627879400875 ) ) ;
#17478 = CARTESIAN_POINT ( 'NONE',  ( 42.35079386031210191, -44.32234244509449894, -5.113119501825009294 ) ) ;
#17479 = CARTESIAN_POINT ( 'NONE',  ( 70.03247032090770574, -49.95860450174168221, -71.35146707679193412 ) ) ;
#17480 = FACE_OUTER_BOUND ( 'NONE', #4046, .T. ) ;
#17481 = AXIS2_PLACEMENT_3D ( 'NONE', #7691, #31759, #19725 ) ;
#17482 = EDGE_CURVE ( 'NONE', #27600, #39738, #24476, .T. ) ;
#17483 = CARTESIAN_POINT ( 'NONE',  ( 64.23479494327480666, 1.179519272898400084, -70.17061531731100388 ) ) ;
#17484 = CARTESIAN_POINT ( 'NONE',  ( 68.13393739769620083, 11.88381105532070059, -65.65000000000000568 ) ) ;
#17485 = CARTESIAN_POINT ( 'NONE',  ( 67.45418716456319430, 1.609579353070809793, -19.55846898103779807 ) ) ;
#17486 = ORIENTED_EDGE ( 'NONE', *, *, #38437, .F. ) ;
#17487 = CARTESIAN_POINT ( 'NONE',  ( 13.73894405924890094, -52.05919180694159820, -75.36996982820370761 ) ) ;
#17488 = CARTESIAN_POINT ( 'NONE',  ( 57.33945456437729860, 19.08983581863999746, -52.87108254538590302 ) ) ;
#17489 = CARTESIAN_POINT ( 'NONE',  ( -18.86606260230360022, -50.61618894467959962, 16.21999999999999886 ) ) ;
#17490 = DIRECTION ( 'NONE',  ( 0.05643417272666773760, -0.04100182651872436024, -0.9975640502598241977 ) ) ;
#17491 = CARTESIAN_POINT ( 'NONE',  ( 23.24784027632620109, -14.48172169338479875, -32.14999999999999858 ) ) ;
#17492 = DIRECTION ( 'NONE',  ( 0.8660254037844390407, 0.4999999999999995004, 2.775557561562887037E-17 ) ) ;
#17493 = CARTESIAN_POINT ( 'NONE',  ( 11.11361097580029877, 33.96900867391000389, -17.79075125673440283 ) ) ;
#17495 = CARTESIAN_POINT ( 'NONE',  ( 8.768740832044489508, -12.62132957242803322, -44.63073338636281306 ) ) ;
#17494 = CARTESIAN_POINT ( 'NONE',  ( 14.34417029198830029, 19.88381105532299742, -22.49240188329279988 ) ) ;
#17496 = CARTESIAN_POINT ( 'NONE',  ( 56.46328101745149297, 19.53148718691070229, -53.62057548195900125 ) ) ;
#17497 = CARTESIAN_POINT ( 'NONE',  ( 8.223528471986069732, -15.61608932669300032, -46.79233150823699816 ) ) ;
#17498 = CARTESIAN_POINT ( 'NONE',  ( 48.25395546892340093, 22.92590509088350004, -54.66662523256869832 ) ) ;
#17499 = EDGE_CURVE ( 'NONE', #11866, #37399, #4329, .T. ) ;
#17500 = CARTESIAN_POINT ( 'NONE',  ( 9.216187797245829927, -14.24239869871029995, -61.90958082047689004 ) ) ;
#17501 = ORIENTED_EDGE ( 'NONE', *, *, #22992, .F. ) ;
#17502 = DIRECTION ( 'NONE',  ( 0.5193766129849299862, 0.000000000000000000, 0.8545454545454573836 ) ) ;
#17503 = CARTESIAN_POINT ( 'NONE',  ( 65.05887334876679517, 1.388715606738730068, -61.01996879627380110 ) ) ;
#17504 = LINE ( 'NONE', #21927, #17045 ) ;
#17506 = CARTESIAN_POINT ( 'NONE',  ( 54.85035616863589780, 16.02459751768919816, -25.69268928997570001 ) ) ;
#17505 = CARTESIAN_POINT ( 'NONE',  ( 83.38337402972518930, 13.83610802003009965, -47.24826086172119233 ) ) ;
#17507 = CARTESIAN_POINT ( 'NONE',  ( 21.00866568523840172, -10.51917189357370042, -76.19572567137240071 ) ) ;
#17509 = EDGE_CURVE ( 'NONE', #38446, #25427, #14951, .T. ) ;
#17508 = CARTESIAN_POINT ( 'NONE',  ( 16.13393739769620083, -15.61618894467929941, -11.65000000000000036 ) ) ;
#17510 = CARTESIAN_POINT ( 'NONE',  ( 56.44264214053460904, -45.11618894467940066, -15.14376385419089921 ) ) ;
#17511 = CARTESIAN_POINT ( 'NONE',  ( 16.13393739846139852, -15.61618894397629909, 14.85000000048049884 ) ) ;
#17512 = ORIENTED_EDGE ( 'NONE', *, *, #30909, .F. ) ;
#17513 = EDGE_LOOP ( 'NONE', ( #2186, #623, #27562, #129 ) ) ;
#17514 = CARTESIAN_POINT ( 'NONE',  ( 11.54952630610340059, -65.01896633571658413, -16.63601099843520004 ) ) ;
#17515 = CARTESIAN_POINT ( 'NONE',  ( 12.95024349288270038, 34.28238369627520399, -47.68553644283399962 ) ) ;
#17516 = CARTESIAN_POINT ( 'NONE',  ( 23.63393739769620083, -48.77866774226020397, -34.64999999999999858 ) ) ;
#17517 = AXIS2_PLACEMENT_3D ( 'NONE', #2909, #39836, #39323 ) ;
#17518 = CARTESIAN_POINT ( 'NONE',  ( 11.72329413022310085, 33.70814486805359422, -45.18478288877800253 ) ) ;
#17519 = CARTESIAN_POINT ( 'NONE',  ( 47.64143405400680109, 23.30250925609140111, -74.14999999999999147 ) ) ;
#17520 = VECTOR ( 'NONE', #27010, 1000.000000000000000 ) ;
#17521 = AXIS2_PLACEMENT_3D ( 'NONE', #23402, #50446, #23662 ) ;
#17522 = ORIENTED_EDGE ( 'NONE', *, *, #12660, .T. ) ;
#17523 = CARTESIAN_POINT ( 'NONE',  ( -22.55228448404800190, -11.83808067235150041, -54.37716480558419363 ) ) ;
#17524 = CARTESIAN_POINT ( 'NONE',  ( 53.82322419959533732, 17.55874272043913109, -27.07946608715714731 ) ) ;
#17525 = AXIS2_PLACEMENT_3D ( 'NONE', #42007, #2168, #41477 ) ;
#17526 = CARTESIAN_POINT ( 'NONE',  ( 52.81501434156309926, 18.37449448283769726, -48.45418012326710056 ) ) ;
#17527 = DIRECTION ( 'NONE',  ( 0.000000000000000000, 0.000000000000000000, 1.000000000000000000 ) ) ;
#17528 = ADVANCED_FACE ( 'NONE', ( #654 ), #48683, .F. ) ;
#17529 = CARTESIAN_POINT ( 'NONE',  ( 50.83757486290169680, -48.61618577117480555, -76.31330845207050118 ) ) ;
#17530 = CARTESIAN_POINT ( 'NONE',  ( 16.13393739769599833, 14.38381105532070059, -49.33749999999999858 ) ) ;
#17531 = ORIENTED_EDGE ( 'NONE', *, *, #16678, .T. ) ;
#17532 = CARTESIAN_POINT ( 'NONE',  ( 9.366764248923921343, -15.61602670952840199, -67.45282021618999124 ) ) ;
#17533 = LINE ( 'NONE', #33502, #41005 ) ;
#17534 = ORIENTED_EDGE ( 'NONE', *, *, #39575, .T. ) ;
#17535 = CARTESIAN_POINT ( 'NONE',  ( 22.90093739769620029, -15.61618894467913243, -28.45282021618999835 ) ) ;
#17536 = DIRECTION ( 'NONE',  ( 0.000000000000000000, 0.000000000000000000, 1.000000000000000000 ) ) ;
#17537 = CARTESIAN_POINT ( 'NONE',  ( 11.16127494616910099, -9.544997455588569935, -33.29405281597039590 ) ) ;
#17538 = CARTESIAN_POINT ( 'NONE',  ( 13.79106882486509988, -51.24459767255270037, -22.61434474859899879 ) ) ;
#17539 = CARTESIAN_POINT ( 'NONE',  ( 57.13424245449340333, 19.38601785914529785, -74.14888481814519139 ) ) ;
#17540 = CARTESIAN_POINT ( 'NONE',  ( 47.18871270837350806, -53.98686607640210156, -75.65958371907380808 ) ) ;
#17541 = ORIENTED_EDGE ( 'NONE', *, *, #49196, .F. ) ;
#17542 = CARTESIAN_POINT ( 'NONE',  ( 54.77399211316150485, 14.69977379240920001, -15.76359807579460082 ) ) ;
#17543 = CARTESIAN_POINT ( 'NONE',  ( 56.91872543020900110, -50.64361015893680218, -53.86107397471379699 ) ) ;
#17544 = EDGE_CURVE ( 'NONE', #25171, #45038, #22411, .T. ) ;
#17545 = CARTESIAN_POINT ( 'NONE',  ( 21.14288210468430051, -10.65101126812110088, -32.59857632693769602 ) ) ;
#17546 = CARTESIAN_POINT ( 'NONE',  ( 1.058369240368480124, -8.644356418428410294, -34.64999999999999858 ) ) ;
#17547 = EDGE_CURVE ( 'NONE', #40988, #34513, #11869, .T. ) ;
#17548 = CARTESIAN_POINT ( 'NONE',  ( 46.58993879724850018, 22.02491853214390005, -76.11254988220410667 ) ) ;
#17549 = CARTESIAN_POINT ( 'NONE',  ( 65.14992021336850314, 1.382840740411490188, -60.95335679887120506 ) ) ;
#17550 = VECTOR ( 'NONE', #10413, 1000.000000000000000 ) ;
#17551 = CARTESIAN_POINT ( 'NONE',  ( 40.84819990301859605, -45.40787957530859842, -5.828857708371039337 ) ) ;
#17552 = CIRCLE ( 'NONE', #46867, 1.000000000000000888 ) ;
#17553 = CARTESIAN_POINT ( 'NONE',  ( 44.76356921293569968, -45.10235736362039916, -7.023953210218369492 ) ) ;
#17554 = LINE ( 'NONE', #41919, #36538 ) ;
#17555 = AXIS2_PLACEMENT_3D ( 'NONE', #41101, #13835, #29792 ) ;
#17556 = TOROIDAL_SURFACE ( 'NONE', #31748, 15.56227766038949945, 0.9999999999568489617 ) ;
#17557 = CARTESIAN_POINT ( 'NONE',  ( 24.09704775629829854, -13.47827939507680028, -81.42417512157139470 ) ) ;
#17558 = CARTESIAN_POINT ( 'NONE',  ( 82.35525732794108933, 13.87593127045350094, -46.40107902847420007 ) ) ;
#17559 = CARTESIAN_POINT ( 'NONE',  ( 73.25400818986750551, 0.9960089569207349891, -68.76188247756290650 ) ) ;
#17561 = CARTESIAN_POINT ( 'NONE',  ( 44.86670720216029196, -39.15407246580593892, -66.17957604452888631 ) ) ;
#17560 = CARTESIAN_POINT ( 'NONE',  ( 14.13393739769600010, 14.38381105532060111, -62.64999999999999858 ) ) ;
#17562 = AXIS2_PLACEMENT_3D ( 'NONE', #5143, #5396, #16933 ) ;
#17563 = CARTESIAN_POINT ( 'NONE',  ( 61.03999680408450246, 14.12696753779889924, -46.86320879711829690 ) ) ;
#17564 = CARTESIAN_POINT ( 'NONE',  ( -31.60239111126589862, -24.98565332602689892, -55.64697389277930029 ) ) ;
#17565 = ORIENTED_EDGE ( 'NONE', *, *, #50302, .T. ) ;
#17566 = EDGE_CURVE ( 'NONE', #41648, #51612, #25263, .T. ) ;
#17567 = CARTESIAN_POINT ( 'NONE',  ( 53.10865797006830036, -49.51857916385080216, -48.88762732764140395 ) ) ;
#17568 = ORIENTED_EDGE ( 'NONE', *, *, #11914, .T. ) ;
#17569 = CARTESIAN_POINT ( 'NONE',  ( 61.26000939124259759, -45.11942681417600198, -27.10278859166270138 ) ) ;
#17570 = CARTESIAN_POINT ( 'NONE',  ( 56.53714865535440737, 14.14923065729820095, -25.50329352154150087 ) ) ;
#17571 = CARTESIAN_POINT ( 'NONE',  ( 20.59223919530819913, -10.15120003544670091, -38.17063876083509655 ) ) ;
#17572 = CARTESIAN_POINT ( 'NONE',  ( 28.63393739769619728, -26.55370255794280254, -34.64999999999999858 ) ) ;
#17574 = EDGE_CURVE ( 'NONE', #3482, #31804, #5379, .T. ) ;
#17573 = CARTESIAN_POINT ( 'NONE',  ( 53.21885458705129679, 18.27078423299469989, -49.08533969520789952 ) ) ;
#17575 = CARTESIAN_POINT ( 'NONE',  ( 60.64847374440059724, -45.56447532782619447, -47.14388410539569918 ) ) ;
#17576 = CARTESIAN_POINT ( 'NONE',  ( 71.76678105856730383, -45.11618894467940066, -14.40246108749630061 ) ) ;
#17577 = ORIENTED_EDGE ( 'NONE', *, *, #14618, .T. ) ;
#17578 = CARTESIAN_POINT ( 'NONE',  ( 10.43935959611360076, -10.81218249130760078, -78.29040566010630187 ) ) ;
#17579 = CARTESIAN_POINT ( 'NONE',  ( 72.83620669801349834, 1.369719003397489976, -68.81308079741751271 ) ) ;
#17580 = CARTESIAN_POINT ( 'NONE',  ( 47.46120807750819637, -54.60632935821639933, -54.66578937757580547 ) ) ;
#17581 = CARTESIAN_POINT ( 'NONE',  ( 10.66328804357033633, -9.855181135427269368, -49.05049542099398963 ) ) ;
#17582 = CARTESIAN_POINT ( 'NONE',  ( 73.13559359734860266, 0.8904513541338849869, -62.33586013860640662 ) ) ;
#17583 = CARTESIAN_POINT ( 'NONE',  ( 11.43201365335179887, -65.36003045264970979, -18.10223070864369888 ) ) ;
#17584 = CARTESIAN_POINT ( 'NONE',  ( 53.06963667952179975, 18.30286252129070235, -48.79723990062230143 ) ) ;
#17585 = CARTESIAN_POINT ( 'NONE',  ( 23.94268579721757817, -16.91034996406515489, -75.84458980966927300 ) ) ;
#17586 = CARTESIAN_POINT ( 'NONE',  ( 22.90092890316272900, -15.60509115818101122, -62.45230633468198533 ) ) ;
#17587 = CARTESIAN_POINT ( 'NONE',  ( 24.02073126551701776, -16.28883017867714855, -45.53480547859069816 ) ) ;
#17588 = CARTESIAN_POINT ( 'NONE',  ( 64.95277593799409033, 1.369976237678190101, -70.34495568738229565 ) ) ;
#17589 = ORIENTED_EDGE ( 'NONE', *, *, #21396, .F. ) ;
#17590 = CARTESIAN_POINT ( 'NONE',  ( 9.742198651190470571, -63.26564277683720405, -46.29734320245890444 ) ) ;
#17591 = CARTESIAN_POINT ( 'NONE',  ( 68.13393739769618662, -28.80002732851770020, -102.2016796975542690 ) ) ;
#17592 = VERTEX_POINT ( 'NONE', #49154 ) ;
#17593 = CARTESIAN_POINT ( 'NONE',  ( 38.67452568954050207, -36.11618894467930119, -81.65000000000000568 ) ) ;
#17594 = LINE ( 'NONE', #33038, #41121 ) ;
#17595 = CARTESIAN_POINT ( 'NONE',  ( 9.400903757049320575, -16.99286248564640900, -53.78241387521948269 ) ) ;
#17596 = CIRCLE ( 'NONE', #34284, 5.999999999999998224 ) ;
#17597 = CARTESIAN_POINT ( 'NONE',  ( 53.75480394283020047, 19.75577102335120117, -75.91868723632779847 ) ) ;
#17598 = CIRCLE ( 'NONE', #11729, 2.700000000000230216 ) ;
#17599 = ORIENTED_EDGE ( 'NONE', *, *, #20863, .F. ) ;
#17600 = CARTESIAN_POINT ( 'NONE',  ( 16.13393739769620083, -15.61618894467939889, 17.35000000000000142 ) ) ;
#17601 = CIRCLE ( 'NONE', #36804, 2.000000000000001776 ) ;
#17602 = DIRECTION ( 'NONE',  ( 0.000000000000000000, -1.000000000000000000, 0.000000000000000000 ) ) ;
#17603 = LINE ( 'NONE', #49327, #37041 ) ;
#17604 = AXIS2_PLACEMENT_3D ( 'NONE', #37826, #50134, #34123 ) ;
#17605 = AXIS2_PLACEMENT_3D ( 'NONE', #44405, #37316, #16101 ) ;
#17606 = B_SPLINE_SURFACE_WITH_KNOTS ( 'NONE', 3, 3, ( 
 ( #7270, #3337, #19316, #35296, #1206, #28450, #13017, #44452, #24239, #44972, #12227, #8559, #4876, #32109, #20844, #28190 ),
 ( #24501, #8291, #36313, #24766, #16942, #947, #36841, #44709, #40266, #12752, #32886, #48921, #16150, #48128, #40519, #28708 ),
 ( #423, #678, #4356, #28973, #9074, #25022, #48386, #41036, #5153, #32367, #16667, #21107, #48653, #16410, #173, #37109 ),
 ( #44193, #20325, #4608, #12483, #20582, #36575, #32625, #8815, #40776, #23134, #88, #23643, #31511, #47530, #4263, #11628 ),
 ( #15297, #27082, #31253, #16060, #43341, #35724, #8201, #333, #11114, #31764, #19217, #23893, #24147, #35970, #35465, #27846 ),
 ( #28095, #32017, #43597, #39659, #47283, #3245, #40168, #51459, #20233, #11373, #51708, #48041, #43086, #16316, #36221, #12140 ),
 ( #27589, #44101, #3509, #7435, #47028, #7178, #35202, #7699, #23383, #39148, #51205, #11892, #15803, #47783, #27337, #39406 ),
 ( #19476, #15558, #3763, #19733, #43848, #7944, #39918, #4013, #19975, #40682, #33325, #45138, #21529, #48292, #16568, #41203 ),
 ( #32522, #37011, #28877, #843, #13188, #17106, #40421, #4781, #48551, #44879, #5053, #44356, #8719, #29138, #37526, #9505 ),
 ( #21012, #12922, #4514, #40942, #16840, #20749, #8984, #1629, #12658, #12387, #1109, #28612, #20487, #32271, #49343, #33058 ) ),
 .UNSPECIFIED., .F., .F., .F.,
 ( 4, 1, 1, 1, 1, 1, 1, 4 ),
 ( 4, 2, 2, 2, 2, 2, 2, 4 ),
 ( -1.166380231000000015E-05, 0.1428571428571430157, 0.2857142857142860315, 0.4285714285714289917, 0.5714285714285709528, 0.7142857142857139685, 0.8571428571428569843, 1.000014690989259991 ),
 ( -1.570796326794899889, -1.322743703599180032, -1.039254991375500037, -0.8620745462357000122, -0.7734843236657999999, -0.6317399675539610016, -0.4049489977750179714, -0.1533416749778369892 ),
 .UNSPECIFIED. ) ;
#17607 = CARTESIAN_POINT ( 'NONE',  ( 16.35167375485299956, -23.85847691190700104, -48.28392467753440087 ) ) ;
#17608 = CARTESIAN_POINT ( 'NONE',  ( 12.92633465669690551, -9.590651413721559493, -55.79692252247223649 ) ) ;
#17609 = CARTESIAN_POINT ( 'NONE',  ( 44.33306693287859446, -37.96050983500394693, -68.65435001593694153 ) ) ;
#17610 = ORIENTED_EDGE ( 'NONE', *, *, #13218, .F. ) ;
#17611 = PLANE ( 'NONE',  #22509 ) ;
#17612 = CARTESIAN_POINT ( 'NONE',  ( 10.15437084639799892, -11.17192548897130067, -41.43610882498329318 ) ) ;
#17613 = CARTESIAN_POINT ( 'NONE',  ( 52.67198760255850232, -49.78119412946660560, -48.75777783608979377 ) ) ;
#17614 = CARTESIAN_POINT ( 'NONE',  ( 45.07859124227709202, 14.88014128531450098, -9.026881354359289844 ) ) ;
#17615 = EDGE_CURVE ( 'NONE', #41914, #27414, #18710, .T. ) ;
#17616 = CARTESIAN_POINT ( 'NONE',  ( 13.71097881326609880, 20.32289363718010122, -74.92517623884199907 ) ) ;
#17617 = ADVANCED_FACE ( 'NONE', ( #45726 ), #28865, .T. ) ;
#17618 = CARTESIAN_POINT ( 'NONE',  ( 20.11811997673071772, -8.703696410388799265, -51.45899645242261045 ) ) ;
#17619 = CARTESIAN_POINT ( 'NONE',  ( 45.06694394734220310, -45.15390109120389894, -7.502817270234459990 ) ) ;
#17620 = CARTESIAN_POINT ( 'NONE',  ( 23.85449792131219482, -13.85627121030026565, -61.43635185904214779 ) ) ;
#17621 = CARTESIAN_POINT ( 'NONE',  ( 20.78413717728000165, -22.42488652343350353, -57.81693366461269079 ) ) ;
#17622 = ORIENTED_EDGE ( 'NONE', *, *, #51861, .F. ) ;
#17623 = CARTESIAN_POINT ( 'NONE',  ( 52.66238559624279958, -49.77034287296790183, -28.07828440529620195 ) ) ;
#17624 = CARTESIAN_POINT ( 'NONE',  ( 55.63096065035139759, -50.93928849674639991, -74.97610068968259611 ) ) ;
#17625 = CARTESIAN_POINT ( 'NONE',  ( 12.47113786592370133, 33.67127610693530215, -16.09695680451569899 ) ) ;
#17626 = CARTESIAN_POINT ( 'NONE',  ( 9.367163129351689932, -15.61602587752549809, -57.45282021618999835 ) ) ;
#17627 = CARTESIAN_POINT ( 'NONE',  ( 54.47259832750690123, 15.01994964729280113, -15.76422791930239953 ) ) ;
#17628 = ORIENTED_EDGE ( 'NONE', *, *, #10700, .T. ) ;
#17629 = AXIS2_PLACEMENT_3D ( 'NONE', #4385, #20611, #36602 ) ;
#17630 = CARTESIAN_POINT ( 'NONE',  ( -8.086920474589250674, -44.91374637176360096, -5.311490494450340272 ) ) ;
#17631 = VECTOR ( 'NONE', #41144, 1000.000000000000000 ) ;
#17632 = CARTESIAN_POINT ( 'NONE',  ( 47.46673305269209919, 23.38706694144839915, -54.94265356273070466 ) ) ;
#17633 = CARTESIAN_POINT ( 'NONE',  ( 55.92677794998609642, -45.89053595373002992, -25.32409385810630909 ) ) ;
#17634 = CARTESIAN_POINT ( 'NONE',  ( 63.15779899367210248, 0.9281439705311369526, -62.29764659744859756 ) ) ;
#17635 = CARTESIAN_POINT ( 'NONE',  ( 60.77432506344459284, 14.26616040630690030, -47.09778254978269274 ) ) ;
#17636 = AXIS2_PLACEMENT_3D ( 'NONE', #28731, #3620, #7807 ) ;
#17637 = CARTESIAN_POINT ( 'NONE',  ( 10.87995435926830012, 33.74311107132329823, -17.51161114007549813 ) ) ;
#17638 = CARTESIAN_POINT ( 'NONE',  ( 51.80595387025849874, 17.96077523470199822, -77.05313553437329688 ) ) ;
#17640 = ADVANCED_FACE ( 'NONE', ( #3772 ), #17171, .T. ) ;
#17639 = FACE_OUTER_BOUND ( 'NONE', #30265, .T. ) ;
#17641 = CARTESIAN_POINT ( 'NONE',  ( 47.18324198357279897, -54.80726809202429450, -54.61059023085309860 ) ) ;
#17642 = CARTESIAN_POINT ( 'NONE',  ( 53.29384558423090112, -50.54670888882439783, -28.15000000000000213 ) ) ;
#17643 = CARTESIAN_POINT ( 'NONE',  ( 54.10076142776490116, 17.30991513604229937, -26.94462959976219807 ) ) ;
#17644 = CARTESIAN_POINT ( 'NONE',  ( 54.32603732818120079, 20.33894821613250059, -53.45081835463139441 ) ) ;
#17645 = CARTESIAN_POINT ( 'NONE',  ( 63.61467066632980760, 1.258805424669340089, -69.48497663681300196 ) ) ;
#17646 = CARTESIAN_POINT ( 'NONE',  ( 12.02928808077719935, -65.36534498448229158, -17.22609656285550273 ) ) ;
#17647 = CARTESIAN_POINT ( 'NONE',  ( 32.61507622778040627, -15.61618894467929941, -7.049999999999999822 ) ) ;
#17648 = EDGE_LOOP ( 'NONE', ( #22198, #3992, #40841, #35944 ) ) ;
#17649 = CARTESIAN_POINT ( 'NONE',  ( 71.22645170866519493, 1.102581332775290024, -60.56179621591489592 ) ) ;
#17650 = CARTESIAN_POINT ( 'NONE',  ( 10.97872622502669948, 32.01874292912219744, -44.74211950928979320 ) ) ;
#17651 = CYLINDRICAL_SURFACE ( 'NONE', #46039, 6.766999999999998572 ) ;
#17652 = CARTESIAN_POINT ( 'NONE',  ( 66.66072342652930161, -29.91655757336389954, -17.00118403369340214 ) ) ;
#17653 = CARTESIAN_POINT ( 'NONE',  ( 22.88157195713212744, -16.89179476805239943, -46.90719394731226544 ) ) ;
#17654 = ORIENTED_EDGE ( 'NONE', *, *, #19775, .T. ) ;
#17655 = ORIENTED_EDGE ( 'NONE', *, *, #18506, .T. ) ;
#17656 = CARTESIAN_POINT ( 'NONE',  ( 16.13393739769620083, -1.590680505402594314, -34.79644660940672196 ) ) ;
#17657 = VERTEX_POINT ( 'NONE', #9510 ) ;
#17658 = CARTESIAN_POINT ( 'NONE',  ( 9.869349599861529043, -63.31974513753180389, -46.22151743515530598 ) ) ;
#17659 = CARTESIAN_POINT ( 'NONE',  ( 56.83034892914880487, -45.92143544903500185, -26.22419937669090118 ) ) ;
#17660 = CARTESIAN_POINT ( 'NONE',  ( 22.91042337000040163, -19.72316792142765962, -77.68106494717130772 ) ) ;
#17661 = CARTESIAN_POINT ( 'NONE',  ( 61.59490267384730089, 13.91893133687459994, -46.70618209336589643 ) ) ;
#17662 = LINE ( 'NONE', #31938, #38501 ) ;
#17663 = ORIENTED_EDGE ( 'NONE', *, *, #37973, .F. ) ;
#17664 = CARTESIAN_POINT ( 'NONE',  ( 45.57987257403829773, 6.876088038916404521, -62.42029362287482996 ) ) ;
#17665 = ORIENTED_EDGE ( 'NONE', *, *, #32972, .T. ) ;
#17666 = CARTESIAN_POINT ( 'NONE',  ( 45.87783615456250175, -45.55524548511859706, -9.057579235710109700 ) ) ;
#17667 = DIRECTION ( 'NONE',  ( 0.000000000000000000, 1.000000000000000000, 0.000000000000000000 ) ) ;
#17668 = CARTESIAN_POINT ( 'NONE',  ( -14.37046249213279658, -15.61618894467929941, 7.349999999999999645 ) ) ;
#17669 = ORIENTED_EDGE ( 'NONE', *, *, #12229, .F. ) ;
#17670 = CARTESIAN_POINT ( 'NONE',  ( -0.007164426707907000161, -50.71887597443840434, -34.77269723932290191 ) ) ;
#17671 = CARTESIAN_POINT ( 'NONE',  ( 47.00221226121089302, -54.26108178918599378, -75.51940560377390455 ) ) ;
#17672 = CYLINDRICAL_SURFACE ( 'NONE', #29539, 7.910999999999997812 ) ;
#17673 = VECTOR ( 'NONE', #2903, 1000.000000000000000 ) ;
#17674 = CARTESIAN_POINT ( 'NONE',  ( 54.85251692984100202, 13.88381105524550030, -14.10626792861419965 ) ) ;
#17675 = ADVANCED_FACE ( 'NONE', ( #45143 ), #49549, .T. ) ;
#17676 = DIRECTION ( 'NONE',  ( 7.719205000000000365E-17, 1.062456999999999985E-16, 1.000000000000000000 ) ) ;
#17677 = FACE_OUTER_BOUND ( 'NONE', #19578, .T. ) ;
#17678 = CARTESIAN_POINT ( 'NONE',  ( 61.42166429544719364, 13.88661517629680020, -27.30521883883519862 ) ) ;
#17679 = CARTESIAN_POINT ( 'NONE',  ( 21.07505574528920178, -9.519296485543838671, -69.00429683512300016 ) ) ;
#17680 = ORIENTED_EDGE ( 'NONE', *, *, #45775, .T. ) ;
#17681 = LINE ( 'NONE', #33650, #2923 ) ;
#17682 = CARTESIAN_POINT ( 'NONE',  ( -9.296035807754268632, -42.83485695790410119, -4.399682342286669545 ) ) ;
#17683 = CARTESIAN_POINT ( 'NONE',  ( 76.56552468136949585, -40.98740743049830115, -13.88134112481359850 ) ) ;
#17684 = CARTESIAN_POINT ( 'NONE',  ( 72.80915813965889072, 1.367045641526529964, -68.91833781196129394 ) ) ;
#17685 = CARTESIAN_POINT ( 'NONE',  ( 71.48855272380100701, 0.8936201581567920771, -60.67538646459720297 ) ) ;
#17686 = DIRECTION ( 'NONE',  ( 0.3294064756440934771, -0.9441882088883220003, -3.885780586188049864E-16 ) ) ;
#17687 = CARTESIAN_POINT ( 'NONE',  ( 23.08073416742070094, -9.873403152104399894, -35.14999999999999858 ) ) ;
#17689 = ADVANCED_FACE ( 'NONE', ( #33063 ), #33045, .T. ) ;
#17688 = CARTESIAN_POINT ( 'NONE',  ( 10.72256312216934759, -19.77478970487977961, -79.24448622922319885 ) ) ;
#17690 = CARTESIAN_POINT ( 'NONE',  ( 49.22821711787649690, -53.85658415721609771, -55.11852911525630105 ) ) ;
#17691 = CARTESIAN_POINT ( 'NONE',  ( 24.04476951127059792, -15.67185460577278100, -33.50990501219975215 ) ) ;
#17692 = EDGE_CURVE ( 'NONE', #16294, #50249, #20227, .T. ) ;
#17693 = CARTESIAN_POINT ( 'NONE',  ( 54.77086636619779370, -51.21734551792319223, -53.06498560372889983 ) ) ;
#17694 = ORIENTED_EDGE ( 'NONE', *, *, #23122, .F. ) ;
#17695 = CARTESIAN_POINT ( 'NONE',  ( 22.59329360082070437, -11.90358719125920040, -56.90129427292909270 ) ) ;
#17696 =( BOUNDED_CURVE ( )  B_SPLINE_CURVE ( 3, ( #18195, #13252, #45727, #5380 ),
 .UNSPECIFIED., .F., .T. ) 
 B_SPLINE_CURVE_WITH_KNOTS ( ( 4, 4 ),
 ( 3.076739999030396445E-15, 0.7853981633974360665 ),
 .UNSPECIFIED. ) 
 CURVE ( )  GEOMETRIC_REPRESENTATION_ITEM ( )  RATIONAL_B_SPLINE_CURVE ( ( 1.000000000000000000, 0.9492530216741930094, 0.9492530216741930094, 1.000000000000000000 ) ) 
 REPRESENTATION_ITEM ( '' )  );
#17697 = CARTESIAN_POINT ( 'NONE',  ( 64.26020817765768811, 1.338417587229490113, -61.22754019711940288 ) ) ;
#17698 = VERTEX_POINT ( 'NONE', #1569 ) ;
#17699 = CYLINDRICAL_SURFACE ( 'NONE', #17562, 5.499999999999998224 ) ;
#17700 = VECTOR ( 'NONE', #3983, 1000.000000000000000 ) ;
#17701 = CARTESIAN_POINT ( 'NONE',  ( 60.41344223070770170, -45.75562068724720177, -47.56364136414550359 ) ) ;
#17702 = CARTESIAN_POINT ( 'NONE',  ( 15.47860435268529855, -22.63851745982070085, -75.37679910129230620 ) ) ;
#17703 = CARTESIAN_POINT ( 'NONE',  ( 21.73883909943680948, -21.19911057316521052, -61.75703682941048811 ) ) ;
#17705 = CARTESIAN_POINT ( 'NONE',  ( 14.06334888173089759, -7.911065466241970157, -35.20899703272518622 ) ) ;
#17704 = CARTESIAN_POINT ( 'NONE',  ( 44.94429346996862762, 8.794140527020607223, -62.08337702003966996 ) ) ;
#17706 = CARTESIAN_POINT ( 'NONE',  ( 53.35835984455025027, -51.38288689484378580, -75.63635970964975286 ) ) ;
#17707 = FACE_OUTER_BOUND ( 'NONE', #23553, .T. ) ;
#17708 = EDGE_LOOP ( 'NONE', ( #12174, #36909, #39894, #44534 ) ) ;
#17709 = ORIENTED_EDGE ( 'NONE', *, *, #50000, .T. ) ;
#17710 = ORIENTED_EDGE ( 'NONE', *, *, #42591, .T. ) ;
#17711 = VERTEX_POINT ( 'NONE', #20687 ) ;
#17712 = B_SPLINE_CURVE_WITH_KNOTS ( 'NONE', 3,
 ( #50186, #41793, #2225, #17431, #18202, #33401, #49417, #13514, #45473, #46526, #31018, #39424, #31530, #35484, #10615, #39676 ),
 .UNSPECIFIED., .F., .F.,
 ( 4, 2, 2, 2, 2, 2, 2, 4 ),
 ( 0.000000000000000000, 0.1213476983427276695, 0.2731151459108055457, 0.3945291039652654153, 0.5159430620197285045, 0.6842823862752845931, 0.9536253050841766443, 1.000000000000000000 ),
 .UNSPECIFIED. ) ;
#17713 = CARTESIAN_POINT ( 'NONE',  ( -22.84941414684771388, -15.61618224896967355, -54.74986855478772441 ) ) ;
#17714 = FACE_OUTER_BOUND ( 'NONE', #10966, .T. ) ;
#17715 = CARTESIAN_POINT ( 'NONE',  ( 56.04685572940000782, -50.83791839738839968, -53.21420621680360341 ) ) ;
#17716 = ORIENTED_EDGE ( 'NONE', *, *, #20845, .F. ) ;
#17717 = VERTEX_POINT ( 'NONE', #13633 ) ;
#17718 = CARTESIAN_POINT ( 'NONE',  ( 22.90088432124023043, -15.64386971747752675, -72.45412750913828859 ) ) ;
#17719 = DIRECTION ( 'NONE',  ( -1.000000000000000000, 0.000000000000000000, 0.000000000000000000 ) ) ;
#17720 = CARTESIAN_POINT ( 'NONE',  ( 15.24811434726632520, -8.849191943919105796, -53.91115499152626711 ) ) ;
#17721 = ORIENTED_EDGE ( 'NONE', *, *, #36010, .T. ) ;
#17722 = LINE ( 'NONE', #46297, #5769 ) ;
#17723 = CARTESIAN_POINT ( 'NONE',  ( 53.60866176960309559, -50.88321737380339727, -76.14577100024149559 ) ) ;
#17724 = AXIS2_PLACEMENT_3D ( 'NONE', #34548, #47405, #39270 ) ;
#17725 = CARTESIAN_POINT ( 'NONE',  ( 7.433595052712614226, -61.36773602579286546, -19.83583517853760370 ) ) ;
#17726 = CARTESIAN_POINT ( 'NONE',  ( 21.21773088487490000, -21.59463283680559798, -62.28818158525510285 ) ) ;
#17727 = CARTESIAN_POINT ( 'NONE',  ( 16.13393739769620083, -15.61618894467929941, -32.14999999999999858 ) ) ;
#17728 = CARTESIAN_POINT ( 'NONE',  ( 44.59168717410679506, 13.92269748457639977, -7.270472794180020237 ) ) ;
#17729 = EDGE_CURVE ( 'NONE', #19952, #25535, #8037, .T. ) ;
#17730 = CARTESIAN_POINT ( 'NONE',  ( 42.93197233849409855, -42.55807683903029925, -3.307825584507050110 ) ) ;
#17731 = CARTESIAN_POINT ( 'NONE',  ( 68.13393739769841773, -50.61618894467878960, -73.25000000000220268 ) ) ;
#17732 = LINE ( 'NONE', #38172, #39096 ) ;
#17733 = AXIS2_PLACEMENT_3D ( 'NONE', #7011, #41865, #38982 ) ;
#17734 = AXIS2_PLACEMENT_3D ( 'NONE', #14551, #5403, #45494 ) ;
#17735 = CARTESIAN_POINT ( 'NONE',  ( 63.99083253892909084, 1.458411868502019981, -69.65665569611660146 ) ) ;
#17736 = DIRECTION ( 'NONE',  ( 0.000000000000000000, 1.000000000000000000, 0.000000000000000000 ) ) ;
#17737 = CARTESIAN_POINT ( 'NONE',  ( 67.26280899804329749, 1.086883144305099913, -18.54866898292119970 ) ) ;
#17738 = VERTEX_POINT ( 'NONE', #17305 ) ;
#17739 = CARTESIAN_POINT ( 'NONE',  ( 14.67572115279929967, -52.29221104373330320, -75.97756937697440094 ) ) ;
#17740 = CARTESIAN_POINT ( 'NONE',  ( 57.31065200125909342, 19.28726522077679917, -53.29731268387590148 ) ) ;
#17741 = DIRECTION ( 'NONE',  ( 0.1686178020941689615, 0.6660492713794448072, -0.7265992051412127894 ) ) ;
#17742 = CARTESIAN_POINT ( 'NONE',  ( 11.14789759607523401, 32.56083963050009089, -43.84340685703310214 ) ) ;
#17743 = ADVANCED_FACE ( 'NONE', ( #45596 ), #35273, .T. ) ;
#17744 = FACE_OUTER_BOUND ( 'NONE', #38578, .T. ) ;
#17745 = CARTESIAN_POINT ( 'NONE',  ( 63.20250508406000023, 1.096932441169210071, -69.00001114258428458 ) ) ;
#17746 = CARTESIAN_POINT ( 'NONE',  ( 11.92216765568830006, 34.20610614520490600, -17.95790456664920143 ) ) ;
#17747 = CARTESIAN_POINT ( 'NONE',  ( 20.99562869291927569, -21.94234359756718789, -52.08399634476754159 ) ) ;
#17748 = CARTESIAN_POINT ( 'NONE',  ( 24.88393739769619728, -15.61618894467929941, 14.34999999999999964 ) ) ;
#17749 = EDGE_CURVE ( 'NONE', #40473, #15666, #25654, .T. ) ;
#17750 = CARTESIAN_POINT ( 'NONE',  ( 48.26498440238650289, 23.02110959576539884, -55.06465735757110025 ) ) ;
#17751 = ORIENTED_EDGE ( 'NONE', *, *, #27834, .F. ) ;
#17752 = CARTESIAN_POINT ( 'NONE',  ( 9.593587546094811458, -12.97679829661129958, -63.96927302813099203 ) ) ;
#17753 = EDGE_LOOP ( 'NONE', ( #40503, #44680, #20438, #29938 ) ) ;
#17754 = CYLINDRICAL_SURFACE ( 'NONE', #15378, 4.649999999999999467 ) ;
#17755 = CARTESIAN_POINT ( 'NONE',  ( 53.43679795856343873, -49.34287432940195828, -48.83615822498648384 ) ) ;
#17756 = CARTESIAN_POINT ( 'NONE',  ( 57.12444643032910108, -50.61921117833989570, -53.89324253442650559 ) ) ;
#17758 = CARTESIAN_POINT ( 'NONE',  ( 55.91595998539320078, 14.67226890368210057, -25.32542959099430036 ) ) ;
#17757 = CARTESIAN_POINT ( 'NONE',  ( 82.88019469981981047, 13.88961720913030007, -46.94529082815019194 ) ) ;
#17759 = CARTESIAN_POINT ( 'NONE',  ( 13.25862789803809960, -9.176068295359060656, -73.81915773946379034 ) ) ;
#17760 = CARTESIAN_POINT ( 'NONE',  ( -0.007164378094141890356, 19.48649803870589992, -34.77269719633950018 ) ) ;
#17761 = CARTESIAN_POINT ( 'NONE',  ( 72.80768847295010460, 1.384447124000270035, -68.59133994763901399 ) ) ;
#17762 = CARTESIAN_POINT ( 'NONE',  ( 14.36259696023510024, -22.20703816934632968, -41.03609446384544412 ) ) ;
#17763 = DIRECTION ( 'NONE',  ( -1.000000000000000000, 0.000000000000000000, 0.000000000000000000 ) ) ;
#17764 = ORIENTED_EDGE ( 'NONE', *, *, #46084, .T. ) ;
#17765 = ORIENTED_EDGE ( 'NONE', *, *, #15322, .T. ) ;
#17766 = CARTESIAN_POINT ( 'NONE',  ( 12.28455908802260055, -64.73110178338430387, -15.95890976726639998 ) ) ;
#17767 = CARTESIAN_POINT ( 'NONE',  ( 12.07551473733020053, 33.99943997505149440, -46.31242131770569870 ) ) ;
#17768 = CARTESIAN_POINT ( 'NONE',  ( 23.41492785263701748, -12.40909292437391009, -39.37550526180498167 ) ) ;
#17769 = CIRCLE ( 'NONE', #45393, 20.00000000000000355 ) ;
#17770 = CARTESIAN_POINT ( 'NONE',  ( 22.90093739720710531, -16.50198351292171495, -54.49448989795372000 ) ) ;
#17771 = DIRECTION ( 'NONE',  ( 0.000000000000000000, 0.000000000000000000, 1.000000000000000000 ) ) ;
#17772 = AXIS2_PLACEMENT_3D ( 'NONE', #18295, #22735, #34537 ) ;
#17773 = VERTEX_POINT ( 'NONE', #4989 ) ;
#17774 = CARTESIAN_POINT ( 'NONE',  ( -20.84921622758820092, -28.80579560280489915, -53.14778043205649993 ) ) ;
#17775 = CARTESIAN_POINT ( 'NONE',  ( 53.20716069589280295, 18.10213603062282317, -27.47938434864637713 ) ) ;
#17776 = CARTESIAN_POINT ( 'NONE',  ( 53.40992735058819818, 18.17061601739440135, -49.09007107978719375 ) ) ;
#17777 = CARTESIAN_POINT ( 'NONE',  ( 63.04562385509341027, -1.096656852449789943, -16.27512118587200263 ) ) ;
#17778 = CARTESIAN_POINT ( 'NONE',  ( 51.15792108380730241, -50.27113159165210732, -76.23077843503030238 ) ) ;
#17779 = CARTESIAN_POINT ( 'NONE',  ( 56.45552426919280009, -50.53433981852420231, -52.91205187155370027 ) ) ;
#17780 = ORIENTED_EDGE ( 'NONE', *, *, #33050, .F. ) ;
#17781 = CARTESIAN_POINT ( 'NONE',  ( 52.59996064233959601, -49.82480704385319825, -27.82108120899960113 ) ) ;
#17782 = CARTESIAN_POINT ( 'NONE',  ( 68.13393739769810509, 19.38381105532030091, -71.50000000000198952 ) ) ;
#17783 = VERTEX_POINT ( 'NONE', #24871 ) ;
#17784 = CARTESIAN_POINT ( 'NONE',  ( 24.04525281611314824, -15.61618915252426376, -57.50766930885080086 ) ) ;
#17785 = FACE_OUTER_BOUND ( 'NONE', #23737, .T. ) ;
#17786 = CARTESIAN_POINT ( 'NONE',  ( 8.204251278821899973, -17.87512636207440053, -78.70399420596430673 ) ) ;
#17787 = CARTESIAN_POINT ( 'NONE',  ( 13.97463716696829827, -51.18681913482190282, -22.92153293571290007 ) ) ;
#17788 = CARTESIAN_POINT ( 'NONE',  ( 54.52045198098380752, 19.43253422766209937, -76.37641636170799586 ) ) ;
#17789 = EDGE_CURVE ( 'NONE', #18259, #31649, #16886, .T. ) ;
#17790 = CARTESIAN_POINT ( 'NONE',  ( 46.96102864795940235, -53.69224363991650506, -75.90771320283761270 ) ) ;
#17791 = ORIENTED_EDGE ( 'NONE', *, *, #21826, .T. ) ;
#17792 = CARTESIAN_POINT ( 'NONE',  ( 55.74284278219830213, 14.65117925743319915, -16.98778742111269935 ) ) ;
#17793 = CARTESIAN_POINT ( 'NONE',  ( 11.13393739769619906, 32.28996932333459569, -43.76018303787720498 ) ) ;
#17794 = EDGE_CURVE ( 'NONE', #22337, #31736, #48490, .T. ) ;
#17795 = CARTESIAN_POINT ( 'NONE',  ( 56.92789890539140174, -50.64206873198590131, -53.72375501711709944 ) ) ;
#17796 = DIRECTION ( 'NONE',  ( 0.000000000000000000, 1.000000000000000000, 0.000000000000000000 ) ) ;
#17797 = DIRECTION ( 'NONE',  ( -0.8090169943749477843, -0.5877852522924728040, 0.000000000000000000 ) ) ;
#17798 = EDGE_CURVE ( 'NONE', #13741, #29295, #7690, .T. ) ;
#17799 = ORIENTED_EDGE ( 'NONE', *, *, #38602, .T. ) ;
#17800 = CARTESIAN_POINT ( 'NONE',  ( 47.24300521349680082, 22.88509248956220077, -75.51940560377610723 ) ) ;
#17801 = CARTESIAN_POINT ( 'NONE',  ( 65.13423472332449649, 1.371651820402789879, -60.88469507784019896 ) ) ;
#17802 = CARTESIAN_POINT ( 'NONE',  ( 75.39234309038256754, -40.43989336811801394, -12.98456726386316085 ) ) ;
#17803 = TOROIDAL_SURFACE ( 'NONE', #38736, 16.60961179679779676, 0.5000000000000000000 ) ;
#17804 = CARTESIAN_POINT ( 'NONE',  ( 18.20470190565380619, -7.911112859053382351, -57.37566467645442714 ) ) ;
#17805 = VECTOR ( 'NONE', #9372, 1000.000000000000000 ) ;
#17806 = CARTESIAN_POINT ( 'NONE',  ( 64.93393739756689342, 1.883811055192859962, -68.84999999978390406 ) ) ;
#17807 = CARTESIAN_POINT ( 'NONE',  ( -5.174310700386709705, 17.42459025154530039, -39.45610452538490165 ) ) ;
#17809 = CARTESIAN_POINT ( 'NONE',  ( 46.37359821032702456, -40.25881220143922690, -54.56558613226453502 ) ) ;
#17808 = CARTESIAN_POINT ( 'NONE',  ( 10.61751707702059910, -64.82563018155620682, -22.25048313876769868 ) ) ;
#17810 = CARTESIAN_POINT ( 'NONE',  ( 21.79705635832106125, 3.269314289273323126, -84.65000000000000568 ) ) ;
#17811 = DIRECTION ( 'NONE',  ( 0.5765530599821100388, 0.1342272854595110421, 0.8059588108975772602 ) ) ;
#17812 = ADVANCED_FACE ( 'NONE', ( #41141 ), #48757, .T. ) ;
#17813 = CARTESIAN_POINT ( 'NONE',  ( -33.86618693412709291, -10.74011431604400002, -57.52971779843680622 ) ) ;
#17814 = ORIENTED_EDGE ( 'NONE', *, *, #49298, .F. ) ;
#17815 = CARTESIAN_POINT ( 'NONE',  ( 52.91916941891219750, -49.61445646718999569, -48.76921093002629704 ) ) ;
#17816 = ORIENTED_EDGE ( 'NONE', *, *, #31846, .T. ) ;
#17817 = CARTESIAN_POINT ( 'NONE',  ( 41.71914574866418945, 8.547687252698329630, -77.49492017313852443 ) ) ;
#17818 = CARTESIAN_POINT ( 'NONE',  ( 48.88334854381260186, -54.00587892617620156, -55.28861537459440001 ) ) ;
#17819 = CARTESIAN_POINT ( 'NONE',  ( 56.80572106195580773, 14.09462252995199982, -25.70585579729069892 ) ) ;
#17820 = CARTESIAN_POINT ( 'NONE',  ( 20.26879960982470052, -9.902567222571891037, -48.15222407485109812 ) ) ;
#17821 = CARTESIAN_POINT ( 'NONE',  ( 29.11414631625610028, -26.73267003105300077, -35.00928286143069812 ) ) ;
#17822 = CARTESIAN_POINT ( 'NONE',  ( 52.99414826126849931, 18.35427201954029641, -48.92816828239389082 ) ) ;
#17823 = CARTESIAN_POINT ( 'NONE',  ( 64.73018593529980080, 0.9325382164350239922, -60.70884169071130287 ) ) ;
#17824 = CARTESIAN_POINT ( 'NONE',  ( 18.20468603776837924, -23.32126951240223178, -57.92433457871812408 ) ) ;
#17825 = CARTESIAN_POINT ( 'NONE',  ( 10.03393739769619941, -15.61618894467929941, -8.849999999999999645 ) ) ;
#17826 = AXIS2_PLACEMENT_3D ( 'NONE', #9437, #25386, #41387 ) ;
#17827 = VERTEX_POINT ( 'NONE', #8926 ) ;
#17828 = CARTESIAN_POINT ( 'NONE',  ( 8.684550524703789520, -15.50073525340130054, -76.07227559032499187 ) ) ;
#17829 = CARTESIAN_POINT ( 'NONE',  ( 72.76779797359338886, 1.388189907116970101, -68.71367622713330547 ) ) ;
#17830 = CARTESIAN_POINT ( 'NONE',  ( 47.49470543983129289, -54.59752074366780050, -54.79943125224989586 ) ) ;
#17831 = CARTESIAN_POINT ( 'NONE',  ( 23.84737858440118075, -13.78234710530517937, -49.71801685587017516 ) ) ;
#17832 = CARTESIAN_POINT ( 'NONE',  ( 73.20393974370449541, 0.8850831926798630178, -62.44126551166660022 ) ) ;
#17833 = CARTESIAN_POINT ( 'NONE',  ( 11.51841290285589992, -65.37424786629888729, -17.84188021312800387 ) ) ;
#17834 = CARTESIAN_POINT ( 'NONE',  ( 71.58293006479010501, 1.102139304147779830, -60.78391614187979997 ) ) ;
#17835 = CARTESIAN_POINT ( 'NONE',  ( 23.63805141649122277, -18.17389567441268383, -75.89683657592323129 ) ) ;
#17836 = CARTESIAN_POINT ( 'NONE',  ( 22.90053501923144808, -15.53643117899985349, -62.44907673796289060 ) ) ;
#17837 = EDGE_CURVE ( 'NONE', #45267, #17917, #17769, .T. ) ;
#17838 = CARTESIAN_POINT ( 'NONE',  ( 9.366958745649954565, -14.73023443675878141, -57.49448687106261957 ) ) ;
#17839 = CARTESIAN_POINT ( 'NONE',  ( 64.82166782235140090, 0.9254905997697669973, -70.65289529397499280 ) ) ;
#17840 = EDGE_LOOP ( 'NONE', ( #40722, #5861, #10763, #17716, #5908 ) ) ;
#17841 = CARTESIAN_POINT ( 'NONE',  ( 13.61938558678000000, -51.42721352342299923, -23.15000000000000213 ) ) ;
#17842 = FACE_OUTER_BOUND ( 'NONE', #24238, .T. ) ;
#17843 = EDGE_LOOP ( 'NONE', ( #43886, #24716, #19516, #27119 ) ) ;
#17844 = DIRECTION ( 'NONE',  ( 1.000000000000000000, 0.000000000000000000, 0.000000000000000000 ) ) ;
#17845 = CARTESIAN_POINT ( 'NONE',  ( 13.39998208310050032, -51.78678246903520233, -74.14999999999999147 ) ) ;
#17846 = CARTESIAN_POINT ( 'NONE',  ( 22.83615144563630395, -17.18444790103682607, -52.92095170805273341 ) ) ;
#17847 = CARTESIAN_POINT ( 'NONE',  ( 53.50362149015870017, 19.53775296350150370, -76.38491669520200844 ) ) ;
#17848 = AXIS2_PLACEMENT_3D ( 'NONE', #33339, #33852, #49354 ) ;
#17850 = ORIENTED_EDGE ( 'NONE', *, *, #26912, .T. ) ;
#17849 = B_SPLINE_CURVE_WITH_KNOTS ( 'NONE', 3,
 ( #402, #37345, #21084, #9050, #24999, #29468, #8538, #28945, #9322, #1444, #33398, #41273, #8791, #45471, #20557, #16388, #24744, #9572 ),
 .UNSPECIFIED., .F., .F.,
 ( 4, 2, 2, 2, 2, 2, 2, 2, 4 ),
 ( 0.000000000000000000, 0.1774999104124761473, 0.3374998296575247303, 0.4374997791856805596, 0.4999997476407779806, 0.6249996845509727672, 0.7565685563123135671, 0.9670787511304582695, 1.000000000000000000 ),
 .UNSPECIFIED. ) ;
#17851 = AXIS2_PLACEMENT_3D ( 'NONE', #33382, #45457, #9308 ) ;
#17852 = FACE_OUTER_BOUND ( 'NONE', #23415, .T. ) ;
#17853 = CARTESIAN_POINT ( 'NONE',  ( 22.90093739739452516, -15.61117588207490492, -72.45258998807413775 ) ) ;
#17854 = CARTESIAN_POINT ( 'NONE',  ( 24.04492500652006370, -15.60001781178229230, -43.79167453644526375 ) ) ;
#17855 = CARTESIAN_POINT ( 'NONE',  ( 10.95413457039449945, -9.201178209987370238, -49.07611398817059722 ) ) ;
#17856 = CARTESIAN_POINT ( 'NONE',  ( 22.90080294078536483, -15.57010463074422191, -56.45065799404199680 ) ) ;
#17857 = CARTESIAN_POINT ( 'NONE',  ( 43.41780707837584430, -37.83780770426486839, -73.23058605696958523 ) ) ;
#17858 = VERTEX_POINT ( 'NONE', #36677 ) ;
#17859 = ADVANCED_FACE ( 'NONE', ( #49025 ), #13379, .T. ) ;
#17860 = DIRECTION ( 'NONE',  ( 0.000000000000000000, 0.000000000000000000, 1.000000000000000000 ) ) ;
#17861 = CARTESIAN_POINT ( 'NONE',  ( 11.23975427116819858, -21.23345387782550020, -40.96079523860159810 ) ) ;
#17862 = CARTESIAN_POINT ( 'NONE',  ( 9.105463204092400176, -18.18851464184960065, -32.14999999999999858 ) ) ;
#17863 = EDGE_CURVE ( 'NONE', #36314, #6777, #49594, .T. ) ;
#17864 = CIRCLE ( 'NONE', #5350, 0.5000000000000004441 ) ;
#17865 = CARTESIAN_POINT ( 'NONE',  ( 14.30359793617770059, 20.25300558755819935, -75.29799846200430125 ) ) ;
#17866 = CARTESIAN_POINT ( 'NONE',  ( -31.36606260230380272, -62.11618894467930119, 11.84999999999999964 ) ) ;
#17867 = CARTESIAN_POINT ( 'NONE',  ( 41.10495109285060522, -44.90785437222480425, -5.488531188786208936 ) ) ;
#17868 = CARTESIAN_POINT ( 'NONE',  ( 16.13393739769620083, -15.61618894467929941, -28.45282021618999835 ) ) ;
#17869 = CARTESIAN_POINT ( 'NONE',  ( 15.95893776300690092, -23.85949506763950367, -54.01442497355899519 ) ) ;
#17870 = VERTEX_POINT ( 'NONE', #25394 ) ;
#17871 = CARTESIAN_POINT ( 'NONE',  ( 55.49059146526019504, -46.45735698793969704, -25.52441156651820009 ) ) ;
#17872 = CARTESIAN_POINT ( 'NONE',  ( 16.20840964857250199, -51.09324699765929978, -20.73468313311619937 ) ) ;
#17874 = CARTESIAN_POINT ( 'NONE',  ( 46.77956775759329133, -39.16040751821400079, -34.67032516424389854 ) ) ;
#17873 = CARTESIAN_POINT ( 'NONE',  ( 8.283081141223801680, 30.83908974943280157, -14.51842061854859978 ) ) ;
#17875 = DIRECTION ( 'NONE',  ( 1.000000000000000000, 0.000000000000000000, 0.000000000000000000 ) ) ;
#17876 = DIRECTION ( 'NONE',  ( 0.000000000000000000, -1.000000000000000000, 0.000000000000000000 ) ) ;
#17877 = CIRCLE ( 'NONE', #51375, 8.000000000000000000 ) ;
#17878 = ORIENTED_EDGE ( 'NONE', *, *, #50624, .F. ) ;
#17879 = CARTESIAN_POINT ( 'NONE',  ( -5.153449232133100466, -47.10011955755160784, -4.520249556061699536 ) ) ;
#17880 = CIRCLE ( 'NONE', #304, 34.41780050634729804 ) ;
#17881 = CARTESIAN_POINT ( 'NONE',  ( 47.45072472674559805, 23.39242017868889789, -54.80215748663960085 ) ) ;
#17882 = CARTESIAN_POINT ( 'NONE',  ( 56.60951721479818843, -45.32895253404118563, -25.29352247433434187 ) ) ;
#17883 = CARTESIAN_POINT ( 'NONE',  ( 63.15271035305199376, 0.9966178393190270324, -62.31828917185450223 ) ) ;
#17884 = CARTESIAN_POINT ( 'NONE',  ( 61.10824109186599884, 14.10765967360200079, -47.03638507362239807 ) ) ;
#17885 = CARTESIAN_POINT ( 'NONE',  ( 11.54952630610960007, 33.78658844635589276, -16.63601099842679787 ) ) ;
#17886 = CARTESIAN_POINT ( 'NONE',  ( 24.04493739769619864, -15.61618894467929941, -32.14999999999999858 ) ) ;
#17887 = DIRECTION ( 'NONE',  ( 0.6888026391158399431, 0.7071067811865427988, 0.1598465650148944706 ) ) ;
#17888 = CARTESIAN_POINT ( 'NONE',  ( 19.49111017241425969, 24.24266684409263917, -75.60405384317246558 ) ) ;
#17889 = CARTESIAN_POINT ( 'NONE',  ( 6.133937397696199945, -15.61618894467930119, -5.966499999999999915 ) ) ;
#17890 = DIRECTION ( 'NONE',  ( 1.000000000000000000, 0.000000000000000000, 0.000000000000000000 ) ) ;
#17891 = CARTESIAN_POINT ( 'NONE',  ( 55.93394966927949952, 19.54994930437460354, -53.01357101662289750 ) ) ;
#17892 = DIRECTION ( 'NONE',  ( 0.7071067811865473507, 0.7071067811865476838, 0.000000000000000000 ) ) ;
#17893 = CARTESIAN_POINT ( 'NONE',  ( 68.13393739769620083, 16.88381105532069881, -71.50000000000000000 ) ) ;
#17894 = VERTEX_POINT ( 'NONE', #5514 ) ;
#17895 = CARTESIAN_POINT ( 'NONE',  ( 19.86997031299514660, 23.42669132854136294, -17.96412134175789532 ) ) ;
#17896 = CARTESIAN_POINT ( 'NONE',  ( 11.10557753124879987, 32.10104306594170254, -44.25340448499940749 ) ) ;
#17897 = CARTESIAN_POINT ( 'NONE',  ( 72.86285390192669809, 1.309114013480920047, -62.27050734077629812 ) ) ;
#17898 = ADVANCED_FACE ( 'NONE', ( #21470 ), #25090, .T. ) ;
#17899 = CARTESIAN_POINT ( 'NONE',  ( 66.62368884664920188, -33.10221915192529707, -20.10140631842839909 ) ) ;
#17900 = ORIENTED_EDGE ( 'NONE', *, *, #30938, .F. ) ;
#17901 = CARTESIAN_POINT ( 'NONE',  ( 18.66237388380359974, 20.19927249694829996, -74.14993703734479880 ) ) ;
#17902 = VERTEX_POINT ( 'NONE', #14160 ) ;
#17903 = EDGE_CURVE ( 'NONE', #36035, #22762, #41825, .T. ) ;
#17904 = EDGE_LOOP ( 'NONE', ( #12348, #17386, #6687, #23428, #42611 ) ) ;
#17905 = VECTOR ( 'NONE', #21182, 1000.000000000000000 ) ;
#17906 = B_SPLINE_CURVE_WITH_KNOTS ( 'NONE', 3,
 ( #1255, #41338, #26108, #1511, #45798, #34225, #50244, #2280, #21657, #30303, #33967 ),
 .UNSPECIFIED., .F., .F.,
 ( 4, 1, 1, 1, 1, 1, 1, 1, 4 ),
 ( 0.000000000000000000, 0.01056175749839638640, 0.08978068856201353032, 0.1689996196256284000, 0.2482185506892432836, 0.3274374817528581394, 0.4066564128164730230, 0.4858753438800901270, 0.5000037738926587094 ),
 .UNSPECIFIED. ) ;
#17907 = DIRECTION ( 'NONE',  ( -1.000000000000000000, 0.000000000000000000, 0.000000000000000000 ) ) ;
#17908 = CARTESIAN_POINT ( 'NONE',  ( 76.48977085477018534, -3.534982534879841598, -13.18333932634366334 ) ) ;
#17909 = EDGE_LOOP ( 'NONE', ( #46553, #34859, #37899, #46168 ) ) ;
#17910 = CARTESIAN_POINT ( 'NONE',  ( 10.93149295491969930, -63.50462161081620138, -44.89510998098330674 ) ) ;
#17911 = CARTESIAN_POINT ( 'NONE',  ( 57.30237695512850138, -45.45193249669419799, -26.06568594713050047 ) ) ;
#17912 = CARTESIAN_POINT ( 'NONE',  ( 22.04684636386204133, -19.02418517277557442, -44.61949510988410594 ) ) ;
#17913 = EDGE_CURVE ( 'NONE', #23932, #39634, #5219, .T. ) ;
#17914 = CARTESIAN_POINT ( 'NONE',  ( 17.25678305769729803, 12.72875286183739973, -62.64999999999999858 ) ) ;
#17915 = ORIENTED_EDGE ( 'NONE', *, *, #19676, .T. ) ;
#17916 = CARTESIAN_POINT ( 'NONE',  ( 45.41914672974152722, 6.858506551998131862, -63.22389523773885855 ) ) ;
#17917 = VERTEX_POINT ( 'NONE', #30898 ) ;
#17918 = CARTESIAN_POINT ( 'NONE',  ( 55.40394017515929903, -45.11618894460369944, -14.52023579739710080 ) ) ;
#17919 = CARTESIAN_POINT ( 'NONE',  ( -30.36606260230379917, -53.11618894467940066, 16.35000000000000142 ) ) ;
#17920 = CARTESIAN_POINT ( 'NONE',  ( 15.93086454162719789, 19.78639745450599818, -20.59235730855439783 ) ) ;
#17921 = CARTESIAN_POINT ( 'NONE',  ( 22.90093394831552942, -15.62408632508305217, -50.45319058549613089 ) ) ;
#17922 = AXIS2_PLACEMENT_3D ( 'NONE', #33207, #32941, #48435 ) ;
#17923 = ORIENTED_EDGE ( 'NONE', *, *, #27404, .F. ) ;
#17924 = CARTESIAN_POINT ( 'NONE',  ( 46.86866897037879909, -54.05579343596940589, -75.74320899229410031 ) ) ;
#17925 = CARTESIAN_POINT ( 'NONE',  ( 44.89546122686059704, 13.88381105527729886, -7.313136318628219890 ) ) ;
#17926 = ADVANCED_FACE ( 'NONE', ( #51098 ), #2362, .F. ) ;
#17927 = CARTESIAN_POINT ( 'NONE',  ( 50.08385623720359803, -49.23364898979970405, -76.14999999999999147 ) ) ;
#17928 = DIRECTION ( 'NONE',  ( -1.000000000000000000, 0.000000000000000000, 0.000000000000000000 ) ) ;
#17929 = CARTESIAN_POINT ( 'NONE',  ( 51.81953054287640015, 20.00644079818270171, -76.05779033163869940 ) ) ;
#17930 = CARTESIAN_POINT ( 'NONE',  ( 61.44557787504049884, 13.91402711005510007, -27.69105617369679706 ) ) ;
#17931 = CARTESIAN_POINT ( 'NONE',  ( 10.43819401510400091, -10.21755434852080135, -68.52898324874108482 ) ) ;
#17932 = EDGE_LOOP ( 'NONE', ( #28192, #7257 ) ) ;
#17933 = CARTESIAN_POINT ( 'NONE',  ( 38.67452568954060155, 1.883811055320659955, -81.65000000000000568 ) ) ;
#17934 = TOROIDAL_SURFACE ( 'NONE', #47255, 9.000000000000000000, 1.000000000000000000 ) ;
#17935 = CARTESIAN_POINT ( 'NONE',  ( 73.18782247527531126, 0.8859637708054480809, -62.41593972647859800 ) ) ;
#17936 = CARTESIAN_POINT ( 'NONE',  ( 76.60139863843768637, -42.13230907256439650, -14.03747475277350176 ) ) ;
#17937 = CARTESIAN_POINT ( 'NONE',  ( 72.87560783889900051, 1.145379646617900038, -69.26025556182580090 ) ) ;
#17938 = CARTESIAN_POINT ( 'NONE',  ( 7.635415421591214447, 29.62789471496180482, -20.56421356237308729 ) ) ;
#17939 = CARTESIAN_POINT ( 'NONE',  ( 71.83393739770048114, 11.38381105532050164, -69.35000000000411546 ) ) ;
#17940 = CARTESIAN_POINT ( 'NONE',  ( 12.49509346338439997, 19.12609117445460072, -21.18371118359339889 ) ) ;
#17941 = CIRCLE ( 'NONE', #47267, 20.00000000000000355 ) ;
#17942 = CARTESIAN_POINT ( 'NONE',  ( 65.02936113742829605, 1.390208944942409985, -70.27002685503249779 ) ) ;
#17943 = CARTESIAN_POINT ( 'NONE',  ( 9.916610038437418950, -53.65744759104700279, -34.65028073423250277 ) ) ;
#17944 = CARTESIAN_POINT ( 'NONE',  ( 43.75992007188810362, -43.62559376723620375, -5.076600545282080823 ) ) ;
#17945 = CIRCLE ( 'NONE', #47271, 22.00000000000000000 ) ;
#17946 = CARTESIAN_POINT ( 'NONE',  ( 76.51215728517360048, -43.23923739644211395, -14.09245988324813581 ) ) ;
#17947 = CARTESIAN_POINT ( 'NONE',  ( 18.12954643717650072, -51.13035289118570148, -74.36013246830410139 ) ) ;
#17948 = DIRECTION ( 'NONE',  ( 0.3805321250008311118, 0.000000000000000000, -0.9247677015566405645 ) ) ;
#17949 = ORIENTED_EDGE ( 'NONE', *, *, #36399, .T. ) ;
#17950 = CIRCLE ( 'NONE', #17104, 1.000000000000001332 ) ;
#17951 = CARTESIAN_POINT ( 'NONE',  ( 21.78790251819230051, -10.76444979726480078, -54.84160206527499781 ) ) ;
#17952 = CARTESIAN_POINT ( 'NONE',  ( 63.61344205335330315, 1.179532368575769707, -61.75071894376389992 ) ) ;
#17953 = ORIENTED_EDGE ( 'NONE', *, *, #38571, .F. ) ;
#17954 = CARTESIAN_POINT ( 'NONE',  ( 10.64863409883700029, -63.44323389162830296, -23.66469670114080159 ) ) ;
#17955 = CARTESIAN_POINT ( 'NONE',  ( 16.13393739769620083, -15.61618894467929941, -35.12503119152809461 ) ) ;
#17956 = DIRECTION ( 'NONE',  ( 1.000000000000000000, 0.000000000000000000, 0.000000000000000000 ) ) ;
#17957 = CARTESIAN_POINT ( 'NONE',  ( 68.13393739823159478, -1.166188945610419969, -65.65000000186969942 ) ) ;
#17959 = CARTESIAN_POINT ( 'NONE',  ( 8.428882060193004122, -13.54534687768648382, -34.87566461313462440 ) ) ;
#17958 = CARTESIAN_POINT ( 'NONE',  ( 44.53450647839624565, 8.764688726411476338, -64.06879138189025014 ) ) ;
#17960 = CARTESIAN_POINT ( 'NONE',  ( -0.007164427059776000244, 14.47565373231149977, -34.77269723891829756 ) ) ;
#17961 = CARTESIAN_POINT ( 'NONE',  ( 45.11068418564629923, -46.01207058399690197, -8.978235659328069218 ) ) ;
#17962 = VERTEX_POINT ( 'NONE', #18087 ) ;
#17963 = ORIENTED_EDGE ( 'NONE', *, *, #13192, .F. ) ;
#17964 = ADVANCED_FACE ( 'NONE', ( #30645 ), #10753, .T. ) ;
#17965 = ORIENTED_EDGE ( 'NONE', *, *, #41065, .F. ) ;
#17966 = VERTEX_POINT ( 'NONE', #50330 ) ;
#17967 = CARTESIAN_POINT ( 'NONE',  ( -22.81250826063345727, -17.44330766158130785, -54.72902440807905577 ) ) ;
#17968 = ADVANCED_FACE ( 'NONE', ( #46149 ), #5469, .T. ) ;
#17969 = CARTESIAN_POINT ( 'NONE',  ( 52.90377914247349622, -49.66458043520950127, -49.02092677081500227 ) ) ;
#17970 = CARTESIAN_POINT ( 'NONE',  ( 61.14661496961065978, 14.27331964475400561, -47.53223270648921073 ) ) ;
#17971 = CARTESIAN_POINT ( 'NONE',  ( 56.14494575505310081, -50.91271539411779656, -53.77253383582240076 ) ) ;
#17972 = VERTEX_POINT ( 'NONE', #42404 ) ;
#17973 = ORIENTED_EDGE ( 'NONE', *, *, #36378, .F. ) ;
#17974 = CARTESIAN_POINT ( 'NONE',  ( 17.01966384186565051, -22.38319920177791289, -72.91110236449276272 ) ) ;
#17975 = VECTOR ( 'NONE', #22676, 1000.000000000000000 ) ;
#17976 = CARTESIAN_POINT ( 'NONE',  ( 51.13393739769659874, -50.61618894467899565, 16.21999999999999886 ) ) ;
#17977 = ORIENTED_EDGE ( 'NONE', *, *, #42079, .T. ) ;
#17978 = CARTESIAN_POINT ( 'NONE',  ( 23.81444512486869414, -17.55625779023211663, -49.58638733271747157 ) ) ;
#17979 = CARTESIAN_POINT ( 'NONE',  ( 53.33359569267409483, -50.64165965796969715, -76.65020871703400474 ) ) ;
#17980 = CARTESIAN_POINT ( 'NONE',  ( 60.67112978390429845, 14.38394182225979989, -47.47021178863389679 ) ) ;
#17981 = CARTESIAN_POINT ( 'NONE',  ( 9.362418724986730112, -19.58270913960189930, -70.84382614012599788 ) ) ;
#17982 = ADVANCED_FACE ( 'NONE', ( #10170 ), #50270, .T. ) ;
#17983 = CYLINDRICAL_SURFACE ( 'NONE', #33898, 7.910999999999997812 ) ;
#17984 = CARTESIAN_POINT ( 'NONE',  ( 41.24055256048669804, 13.59911224018700082, -5.438976187443009813 ) ) ;
#17985 = AXIS2_PLACEMENT_3D ( 'NONE', #8260, #5377, #396 ) ;
#17986 = ADVANCED_FACE ( 'NONE', ( #46347 ), #51551, .T. ) ;
#17987 = CARTESIAN_POINT ( 'NONE',  ( 41.00922517319189353, -44.50642897861339975, -4.614727984880420131 ) ) ;
#17988 = CARTESIAN_POINT ( 'NONE',  ( 72.85590616764901029, 0.9486745332815759157, -61.94714277540219882 ) ) ;
#17989 = CARTESIAN_POINT ( 'NONE',  ( -6.464119761774720807, 15.22590418212459973, -5.599264135990670077 ) ) ;
#17990 = CARTESIAN_POINT ( 'NONE',  ( 64.83129507992209994, 1.367974574076199934, -70.31116820499129005 ) ) ;
#17991 = DIRECTION ( 'NONE',  ( 1.224646799147353207E-16, 1.000000000000000000, -0.000000000000000000 ) ) ;
#17992 = CARTESIAN_POINT ( 'NONE',  ( -15.63324371469531116, 23.83340452438281076, 11.34999999999999964 ) ) ;
#17993 = VERTEX_POINT ( 'NONE', #51803 ) ;
#17994 = CARTESIAN_POINT ( 'NONE',  ( 15.05440318628160057, -53.11618894467930119, -76.14999999999999147 ) ) ;
#17995 = B_SPLINE_CURVE_WITH_KNOTS ( 'NONE', 3,
 ( #43066, #28013, #39832, #38620, #50413, #19898, #40088, #42288 ),
 .UNSPECIFIED., .F., .F.,
 ( 4, 2, 2, 4 ),
 ( 0.4999999271596955452, 0.6249999999960698105, 0.8117231960751974951, 1.000000000000000000 ),
 .UNSPECIFIED. ) ;
#17996 = DIRECTION ( 'NONE',  ( 0.000000000000000000, 0.000000000000000000, -1.000000000000000000 ) ) ;
#17997 = CARTESIAN_POINT ( 'NONE',  ( 48.82567944589380460, -3.116188925162400203, -15.64999999106299988 ) ) ;
#17998 = CARTESIAN_POINT ( 'NONE',  ( 16.72856488856198354, 6.951788894885693182, 4.943674098299959851 ) ) ;
#17999 =( BOUNDED_CURVE ( )  B_SPLINE_CURVE ( 3, ( #28868, #13181, #21255, #9238 ),
 .UNSPECIFIED., .F., .T. ) 
 B_SPLINE_CURVE_WITH_KNOTS ( ( 4, 4 ),
 ( 5.485850788481889673, 5.497787143782139729 ),
 .UNSPECIFIED. ) 
 CURVE ( )  GEOMETRIC_REPRESENTATION_ITEM ( )  RATIONAL_B_SPLINE_CURVE ( ( 1.000000000000000000, 0.9999881269870877221, 0.9999881269870877221, 1.000000000000000000 ) ) 
 REPRESENTATION_ITEM ( '' )  );
#18000 = CARTESIAN_POINT ( 'NONE',  ( 20.55055518814909732, -10.42440965293470079, -32.14999999999999858 ) ) ;
#18001 = CARTESIAN_POINT ( 'NONE',  ( 63.32918872797849019, 1.327097482837290121, -68.80945595804269033 ) ) ;
#18002 = CARTESIAN_POINT ( 'NONE',  ( 48.22056116383330249, -54.26093726109029802, -54.98805926112070352 ) ) ;
#18003 = CIRCLE ( 'NONE', #28057, 33.97624844042361048 ) ;
#18004 = LINE ( 'NONE', #29779, #21393 ) ;
#18005 = CARTESIAN_POINT ( 'NONE',  ( 56.42319918597290496, 19.43625241695789896, -53.17468697167449676 ) ) ;
#18006 = CARTESIAN_POINT ( 'NONE',  ( 41.93138972908788276, 13.29046345300131016, -5.197897843198316714 ) ) ;
#18007 = CARTESIAN_POINT ( 'NONE',  ( 48.37923893010100329, 22.88832752567240192, -54.71411453344789777 ) ) ;
#18008 = VERTEX_POINT ( 'NONE', #39755 ) ;
#18009 = CARTESIAN_POINT ( 'NONE',  ( 20.75744454082159862, -20.94213870710139958, -77.11961558469170086 ) ) ;
#18010 = ORIENTED_EDGE ( 'NONE', *, *, #3892, .T. ) ;
#18011 = FACE_OUTER_BOUND ( 'NONE', #21320, .T. ) ;
#18012 = DIRECTION ( 'NONE',  ( 0.4042525045258790750, 0.000000000000000000, -0.9146474252872273114 ) ) ;
#18013 = CARTESIAN_POINT ( 'NONE',  ( 14.06336572833587439, -7.911061104356444496, -40.92433462936950406 ) ) ;
#18015 = DIRECTION ( 'NONE',  ( 0.000000000000000000, 1.000000000000000000, 0.000000000000000000 ) ) ;
#18014 = CARTESIAN_POINT ( 'NONE',  ( 84.41203222934960593, 12.28655387197119886, -47.41895602134439969 ) ) ;
#18016 = CARTESIAN_POINT ( 'NONE',  ( 15.81374359445209699, -22.66175738342070289, -70.96727622117349199 ) ) ;
#18017 = PLANE ( 'NONE',  #295 ) ;
#18018 = CARTESIAN_POINT ( 'NONE',  ( 56.96825255358579909, -45.11618894467940066, -16.09511754741749812 ) ) ;
#18019 = FACE_OUTER_BOUND ( 'NONE', #49703, .T. ) ;
#18020 = B_SPLINE_SURFACE_WITH_KNOTS ( 'NONE', 3, 3, ( 
 ( #35737, #2998, #31779, #18968, #39161, #39670, #19231, #34949, #23396, #39419, #50949, #15569, #3778 ),
 ( #35214, #31013, #31263, #51721, #47797, #40952, #13199, #24160, #17370, #40434, #24940, #25208, #37024 ),
 ( #28888, #1122, #29148, #33070, #44626, #40694, #12401, #36749, #17118, #28107, #1383, #49097, #20245 ),
 ( #24681, #48054, #28365, #44115, #12153, #8215, #45149, #28626, #48829, #41214, #44371, #5066, #48567 ),
 ( #4794, #8475, #4527, #44890, #8731, #37285, #9261, #20762, #5328, #24421, #40183, #21279, #36237 ),
 ( #4275, #344, #16330, #20499, #36490, #32283, #48304, #595, #16580, #32534, #12671, #21024, #860 ),
 ( #16855, #32802, #12932, #8995, #34105, #33600, #10022, #2682, #6355, #49614, #13958, #26250, #49353 ),
 ( #37807, #21802, #5836, #1902, #14213, #14467, #9519, #17881, #46202, #29411, #10287, #25465, #21539 ),
 ( #37536, #13706, #30184, #42256, #33850, #22573, #29914, #1642, #2160, #22313, #38321, #29662, #13454 ),
 ( #2410, #49866, #41999, #25986, #26505, #18391, #38590, #50383, #33338, #34370, #45933, #50117, #6098 ),
 ( #22054, #45669, #38065, #18140, #45413, #30439, #46461, #10549, #42521, #6610, #41470, #17632, #5585 ),
 ( #9770, #25722, #41731, #10805, #7649, #11066, #23593, #31461, #39358, #46981, #35149, #51155, #39610 ),
 ( #3714, #47485, #18654, #11580, #27032, #27287, #15250, #22828, #43038, #38849, #7134, #31203, #34628 ),
 ( #43548, #43295, #23086, #11323, #19686, #2937, #35410, #18908, #34891, #39105, #7386, #23335, #47232 ),
 ( #50633, #14729, #42781, #50891, #3460, #30949, #14984, #19430, #3197, #51412, #15507, #30700, #19170 ),
 ( #46721, #27542, #26765, #6878, #14384, #42694, #9933, #42434, #14124, #50548, #22227, #25895, #6008 ) ),
 .UNSPECIFIED., .F., .F., .F.,
 ( 4, 2, 2, 2, 2, 2, 2, 4 ),
 ( 4, 1, 1, 1, 1, 1, 1, 1, 1, 1, 4 ),
 ( -1.194374153756279977, -0.9853586768489350778, -0.7464838460976789269, -0.5971870768781439853, -0.5225386922683770141, -0.4031012768927489942, -0.2120014122917439903, 0.04002625521051070279 ),
 ( -0.04002625527861099902, 0.1000000000000000056, 0.2000000000000000111, 0.2999999999999999889, 0.4000000000000000222, 0.5000000000000000000, 0.5999999999999999778, 0.6999999999999999556, 0.8000000000000000444, 0.9000000000000000222, 1.000000000000000000 ),
 .UNSPECIFIED. ) ;
#18021 = VERTEX_POINT ( 'NONE', #36070 ) ;
#18022 = DIRECTION ( 'NONE',  ( 0.000000000000000000, -1.000000000000000000, 0.000000000000000000 ) ) ;
#18023 = AXIS2_PLACEMENT_3D ( 'NONE', #14838, #10917, #7240 ) ;
#18024 = ORIENTED_EDGE ( 'NONE', *, *, #19714, .F. ) ;
#18025 = EDGE_CURVE ( 'NONE', #12701, #1900, #6905, .T. ) ;
#18026 = ORIENTED_EDGE ( 'NONE', *, *, #19055, .F. ) ;
#18027 = CARTESIAN_POINT ( 'NONE',  ( 12.04070883442799911, -64.81472977847060690, -16.10368401052740239 ) ) ;
#18028 = CARTESIAN_POINT ( 'NONE',  ( 55.55365133010059964, 13.88381105532070059, -14.32025150907159983 ) ) ;
#18029 = FACE_OUTER_BOUND ( 'NONE', #36055, .T. ) ;
#18030 = CARTESIAN_POINT ( 'NONE',  ( 50.96419009180484494, 4.052314248501449612, -76.38154650529611445 ) ) ;
#18031 = ORIENTED_EDGE ( 'NONE', *, *, #45315, .T. ) ;
#18032 = ORIENTED_EDGE ( 'NONE', *, *, #17434, .T. ) ;
#18033 = CARTESIAN_POINT ( 'NONE',  ( -18.91827871269439854, -32.83363571916979851, -51.21716275619940006 ) ) ;
#18034 = CARTESIAN_POINT ( 'NONE',  ( 63.93393739769709327, 11.38381105532164028, -69.84999999999999432 ) ) ;
#18035 = CARTESIAN_POINT ( 'NONE',  ( 49.60427607923370630, 21.56003884501200218, -52.10971779361800316 ) ) ;
#18036 = CARTESIAN_POINT ( 'NONE',  ( 65.43644619362240178, -1.044793625667630010, -16.56989681762950184 ) ) ;
#18037 = CARTESIAN_POINT ( 'NONE',  ( 51.06184044748430040, -49.59582491932100368, -76.32371533191239621 ) ) ;
#18038 = CARTESIAN_POINT ( 'NONE',  ( 56.96982729888789976, -50.41531670947319554, -52.91641933479590421 ) ) ;
#18039 = ORIENTED_EDGE ( 'NONE', *, *, #15945, .F. ) ;
#18040 = CARTESIAN_POINT ( 'NONE',  ( 12.14736671544911673, -8.740801174314317024, -33.12518389567012633 ) ) ;
#18041 = CARTESIAN_POINT ( 'NONE',  ( 68.13393739769819035, 19.47158195952109594, -72.59354914830207406 ) ) ;
#18042 = ORIENTED_EDGE ( 'NONE', *, *, #575, .F. ) ;
#18043 = CARTESIAN_POINT ( 'NONE',  ( 12.13393739769598234, -55.41568642894408470, -74.40623532128907414 ) ) ;
#18044 = CARTESIAN_POINT ( 'NONE',  ( 49.62158364714009195, -46.18327638186429596, -12.18455737752769963 ) ) ;
#18045 = CIRCLE ( 'NONE', #43156, 10.00000000000000711 ) ;
#18046 = B_SPLINE_CURVE_WITH_KNOTS ( 'NONE', 3,
 ( #37602, #13260, #1710, #17693, #33663, #8422, #20448, #38663, #15058, #26842, #10621, #31536, #15321, #19242, #35224, #47307 ),
 .UNSPECIFIED., .F., .F.,
 ( 4, 2, 2, 2, 2, 2, 2, 4 ),
 ( 4.583155019233440007E-09, 1.209577291029928503, 2.421219448687449205, 3.178495797223401365, 3.651793515058360473, 4.598388950728297786, 6.112941647800201217, 7.438175257738109281 ),
 .UNSPECIFIED. ) ;
#18047 = CARTESIAN_POINT ( 'NONE',  ( 15.37953186211669987, -23.42756653633809805, -44.54314102700439548 ) ) ;
#18048 = AXIS2_PLACEMENT_3D ( 'NONE', #43352, #47294, #18459 ) ;
#18049 = CARTESIAN_POINT ( 'NONE',  ( 14.04136291104570056, -51.13553769603730359, -22.40089439151919848 ) ) ;
#18050 = CARTESIAN_POINT ( 'NONE',  ( 53.75469708788489953, 19.75578442515150002, -75.91870210712610856 ) ) ;
#18051 = ADVANCED_FACE ( 'NONE', ( #48132 ), #31348, .T. ) ;
#18052 = CARTESIAN_POINT ( 'NONE',  ( 47.00901173922259346, -53.75426067600269420, -75.86421395400510903 ) ) ;
#18053 = ORIENTED_EDGE ( 'NONE', *, *, #16303, .T. ) ;
#18054 = CARTESIAN_POINT ( 'NONE',  ( 56.18893761250490115, 14.30662584625740053, -17.25705736110630184 ) ) ;
#18055 = CARTESIAN_POINT ( 'NONE',  ( 12.72599142185514509, -9.703251754813100760, -77.78615250370977208 ) ) ;
#18056 = CARTESIAN_POINT ( 'NONE',  ( 57.07649182089729578, -50.45121929360420410, -53.03413606727519891 ) ) ;
#18057 = CARTESIAN_POINT ( 'NONE',  ( 22.43205399602669914, -18.79050564095980036, -40.99578301968129068 ) ) ;
#18058 = CARTESIAN_POINT ( 'NONE',  ( 29.13393739769619728, 1.883811055320659955, -34.64999999999999858 ) ) ;
#18059 = CARTESIAN_POINT ( 'NONE',  ( 47.57073486567139753, 23.21246683545610168, -74.81156575899859718 ) ) ;
#18060 = CARTESIAN_POINT ( 'NONE',  ( 69.63393739769620083, -43.11618894467930119, -73.25000000000000000 ) ) ;
#18061 = CARTESIAN_POINT ( 'NONE',  ( 16.13393739769620083, -15.61618894467929941, -28.45282021618999835 ) ) ;
#18062 = CARTESIAN_POINT ( 'NONE',  ( 9.221494253780836203, -11.63192076660207697, -56.95899812772770332 ) ) ;
#18063 = CARTESIAN_POINT ( 'NONE',  ( 28.98356459125609774, -4.548084906195380306, -34.79124076679859456 ) ) ;
#18064 = CARTESIAN_POINT ( 'NONE',  ( -18.86606260230390220, 19.38381105532060289, 17.35000000000000142 ) ) ;
#18065 = AXIS2_PLACEMENT_3D ( 'NONE', #6607, #45930, #22569 ) ;
#18066 = CARTESIAN_POINT ( 'NONE',  ( -15.88451588308629603, 7.113652344613260681, -48.88624781813099673 ) ) ;
#18068 = CARTESIAN_POINT ( 'NONE',  ( 46.74265266493473092, -40.28841859069392228, -52.72914385014497896 ) ) ;
#18067 = LINE ( 'NONE', #34035, #19083 ) ;
#18069 = CARTESIAN_POINT ( 'NONE',  ( 61.28610426219869112, 13.99802494501810024, -46.37202244447839661 ) ) ;
#18070 = CARTESIAN_POINT ( 'NONE',  ( 6.188526101449100203, 32.65406634132989439, -47.34841622259180127 ) ) ;
#18071 = ORIENTED_EDGE ( 'NONE', *, *, #35446, .F. ) ;
#18072 = CARTESIAN_POINT ( 'NONE',  ( 52.76130783809809799, -49.70603018815580043, -48.70177521040290003 ) ) ;
#18073 = EDGE_LOOP ( 'NONE', ( #16063, #22747, #122, #32063, #27886 ) ) ;
#18074 = CARTESIAN_POINT ( 'NONE',  ( 43.58458626024809490, 8.765430566770698206, -68.35028911638491422 ) ) ;
#18075 = CIRCLE ( 'NONE', #35667, 1.000000000000000888 ) ;
#18076 = CARTESIAN_POINT ( 'NONE',  ( 27.13393739769620083, -38.61618894467930119, -59.64999999999999147 ) ) ;
#18077 = CARTESIAN_POINT ( 'NONE',  ( 55.82532434612180339, 14.80164250910239865, -25.33867224380599836 ) ) ;
#18078 = CARTESIAN_POINT ( 'NONE',  ( 10.00102083869919944, -12.13338932698580130, -45.61721828081540053 ) ) ;
#18079 = CARTESIAN_POINT ( 'NONE',  ( 29.04782745927229826, -26.70812982677800207, -34.86734588637909837 ) ) ;
#18080 = CARTESIAN_POINT ( 'NONE',  ( 52.89023671311360175, 18.40607031815540040, -48.86102654974850168 ) ) ;
#18081 = CARTESIAN_POINT ( 'NONE',  ( 64.72587551647490045, 1.099344084866040072, -60.75649936161010345 ) ) ;
#18082 = CARTESIAN_POINT ( 'NONE',  ( 16.17111167639663094, 19.82470455841618318, -15.66946045147826005 ) ) ;
#18083 = EDGE_LOOP ( 'NONE', ( #23281, #18031, #12363, #26963 ) ) ;
#18084 = EDGE_CURVE ( 'NONE', #31691, #47210, #177, .T. ) ;
#18085 = CARTESIAN_POINT ( 'NONE',  ( 21.98123812872290017, -20.23308925758140120, -75.28008627968870314 ) ) ;
#18086 = EDGE_CURVE ( 'NONE', #9786, #35377, #43180, .T. ) ;
#18087 = CARTESIAN_POINT ( 'NONE',  ( -14.37046249213279658, -15.61618894467929941, 8.349999999999999645 ) ) ;
#18088 = DIRECTION ( 'NONE',  ( 1.000000000000000000, 0.000000000000000000, 0.000000000000000000 ) ) ;
#18089 = CARTESIAN_POINT ( 'NONE',  ( 72.77398937677050128, 1.387412027389909985, -62.60488565353588797 ) ) ;
#18090 = CARTESIAN_POINT ( 'NONE',  ( 10.69832412670059973, -64.89277703499729455, -17.91220997211459931 ) ) ;
#18092 = EDGE_CURVE ( 'NONE', #38448, #41688, #13591, .T. ) ;
#18091 = CARTESIAN_POINT ( 'NONE',  ( 71.39251316048110141, 1.372372808637209785, -60.98718532932910819 ) ) ;
#18093 = CARTESIAN_POINT ( 'NONE',  ( 22.90022923424639600, -16.55435297866762667, -66.89132215244777058 ) ) ;
#18094 = CARTESIAN_POINT ( 'NONE',  ( 11.88511791769077064, 10.47075910136237376, -59.64999999999999147 ) ) ;
#18095 = DIRECTION ( 'NONE',  ( 0.4646601886423053496, 0.000000000000000000, 0.8854890790353641128 ) ) ;
#18096 = EDGE_CURVE ( 'NONE', #12971, #12279, #42887, .T. ) ;
#18097 = ORIENTED_EDGE ( 'NONE', *, *, #36029, .F. ) ;
#18098 = CARTESIAN_POINT ( 'NONE',  ( 65.08882305123219680, 1.387412027389909985, -70.29005197907430613 ) ) ;
#18099 = ORIENTED_EDGE ( 'NONE', *, *, #24991, .F. ) ;
#18100 = CARTESIAN_POINT ( 'NONE',  ( 8.949719927774109962, -63.11543068638779630, -46.63538165998269847 ) ) ;
#18101 = CARTESIAN_POINT ( 'NONE',  ( 0.3209249304026170480, -15.61618894467929941, -35.14999999999999858 ) ) ;
#18102 = ORIENTED_EDGE ( 'NONE', *, *, #80, .F. ) ;
#18103 = FACE_OUTER_BOUND ( 'NONE', #23855, .T. ) ;
#18104 = CARTESIAN_POINT ( 'NONE',  ( 57.02861369184739715, 19.39567887796529888, -53.87746547175619583 ) ) ;
#18105 = CARTESIAN_POINT ( 'NONE',  ( 11.27232994224335627, -21.94240753817051726, -70.21600273294129124 ) ) ;
#18106 = CARTESIAN_POINT ( 'NONE',  ( 54.08403600539600831, 19.39417787207790056, -76.77913599485849261 ) ) ;
#18107 = EDGE_LOOP ( 'NONE', ( #19621, #3230, #34619, #7532, #27177, #47636 ) ) ;
#18108 = CARTESIAN_POINT ( 'NONE',  ( 12.89074585065517731, -65.51103569875144217, -47.72398483027909322 ) ) ;
#18109 = DIRECTION ( 'NONE',  ( 0.000000000000000000, -1.000000000000000000, 0.000000000000000000 ) ) ;
#18110 = CARTESIAN_POINT ( 'NONE',  ( 44.34239523011500239, 12.74369304937430059, -3.187564294433600232 ) ) ;
#18111 = EDGE_CURVE ( 'NONE', #8558, #35579, #50411, .T. ) ;
#18112 = DIRECTION ( 'NONE',  ( 0.000000000000000000, 0.000000000000000000, 1.000000000000000000 ) ) ;
#18113 = CARTESIAN_POINT ( 'NONE',  ( 8.585943987534939481, -18.93439863306510063, -50.66049260944299704 ) ) ;
#18114 = VECTOR ( 'NONE', #35355, 1000.000000000000000 ) ;
#18115 = CARTESIAN_POINT ( 'NONE',  ( 23.04647763113142389, -19.60028853819085981, -47.67433631402742833 ) ) ;
#18116 = CARTESIAN_POINT ( 'NONE',  ( 44.62762076536061784, -37.99767204670846610, -67.18153134414910710 ) ) ;
#18117 = ADVANCED_FACE ( 'NONE', ( #11473 ), #27690, .T. ) ;
#18118 = ORIENTED_EDGE ( 'NONE', *, *, #17441, .F. ) ;
#18119 = CARTESIAN_POINT ( 'NONE',  ( 18.38332385620206111, 20.94377882893676102, -75.56421372420827254 ) ) ;
#18120 = CARTESIAN_POINT ( 'NONE',  ( 21.96630730344370264, -20.25193646667360170, -44.44642820540089900 ) ) ;
#18121 = VECTOR ( 'NONE', #40698, 1000.000000000000114 ) ;
#18122 = CARTESIAN_POINT ( 'NONE',  ( 9.367926042023849931, -13.39941049220499991, -32.14999999999999858 ) ) ;
#18123 = CIRCLE ( 'NONE', #35713, 2.000000000000001332 ) ;
#18124 = CARTESIAN_POINT ( 'NONE',  ( 13.60550091158079944, 20.19927249694839944, -74.14993703734479880 ) ) ;
#18125 = DIRECTION ( 'NONE',  ( 0.000000000000000000, 0.000000000000000000, 1.000000000000000000 ) ) ;
#18126 = CARTESIAN_POINT ( 'NONE',  ( 42.47711269216279817, -45.17107499119040170, -6.396649047033399427 ) ) ;
#18127 = CARTESIAN_POINT ( 'NONE',  ( 24.04493243794458834, -15.60658242780756488, -61.50728973154512147 ) ) ;
#18128 = EDGE_CURVE ( 'NONE', #7094, #50433, #44197, .T. ) ;
#18129 = CARTESIAN_POINT ( 'NONE',  ( 17.96668501577229904, -23.65507922116720252, -61.93631807992090188 ) ) ;
#18130 = ORIENTED_EDGE ( 'NONE', *, *, #28482, .T. ) ;
#18131 = CARTESIAN_POINT ( 'NONE',  ( 55.52353368598859618, -46.44448769124329601, -25.67613055164300206 ) ) ;
#18132 = AXIS2_PLACEMENT_3D ( 'NONE', #2474, #1703, #6417 ) ;
#18133 = CARTESIAN_POINT ( 'NONE',  ( 55.27852839649509065, -50.91660802450510204, -75.28002343649311001 ) ) ;
#18135 = CARTESIAN_POINT ( 'NONE',  ( 46.94631559364366780, -39.21699915129384806, -34.75526898281329835 ) ) ;
#18134 = CARTESIAN_POINT ( 'NONE',  ( 10.54211419205399913, 33.45297732329429863, -17.34131202171619890 ) ) ;
#18136 = CARTESIAN_POINT ( 'NONE',  ( 47.47677450096290386, -54.59520210331019285, -54.66133488802340423 ) ) ;
#18137 = FACE_OUTER_BOUND ( 'NONE', #16881, .T. ) ;
#18138 = ORIENTED_EDGE ( 'NONE', *, *, #6563, .F. ) ;
#18139 = CARTESIAN_POINT ( 'NONE',  ( -6.896489314860550834, -45.87074079319390307, -5.066771418161060581 ) ) ;
#18140 = CARTESIAN_POINT ( 'NONE',  ( 47.55224309786800063, 23.32284541588479954, -54.73177068379369814 ) ) ;
#18141 = AXIS2_PLACEMENT_3D ( 'NONE', #21536, #33335, #32799 ) ;
#18142 = CARTESIAN_POINT ( 'NONE',  ( 14.49513316393093909, -7.853150399841008600, -65.22618568674107564 ) ) ;
#18143 = CARTESIAN_POINT ( 'NONE',  ( 84.09627344016217876, -44.51518917121880037, -47.44643142112443712 ) ) ;
#18144 = CARTESIAN_POINT ( 'NONE',  ( 33.83393739769579867, -15.61618894467939711, -10.44999999999995310 ) ) ;
#18145 = CARTESIAN_POINT ( 'NONE',  ( 11.73811129726390057, 33.93366749707369934, -16.79398347924830048 ) ) ;
#18146 = CARTESIAN_POINT ( 'NONE',  ( 38.67452568954060155, -37.56081407618430035, -81.65000000000000568 ) ) ;
#18147 = CARTESIAN_POINT ( 'NONE',  ( 68.13393739769819035, 19.47158195952289717, -70.40645085170193340 ) ) ;
#18148 = FACE_BOUND ( 'NONE', #20915, .T. ) ;
#18149 = LINE ( 'NONE', #30194, #777 ) ;
#18150 = CARTESIAN_POINT ( 'NONE',  ( 56.49023934083049880, 15.04448206350489947, -26.27690413241280254 ) ) ;
#18151 = CARTESIAN_POINT ( 'NONE',  ( 54.72925936106919664, 20.06372169638630254, -53.17373675974890546 ) ) ;
#18152 = CARTESIAN_POINT ( 'NONE',  ( 63.31827236005010917, 1.034646415858929913, -69.21578891831741487 ) ) ;
#18153 = CARTESIAN_POINT ( 'NONE',  ( 53.59007319875249920, 18.17385789302069554, -49.22505640236219904 ) ) ;
#18154 = FACE_BOUND ( 'NONE', #4785, .T. ) ;
#18155 = CARTESIAN_POINT ( 'NONE',  ( 22.90069280194860113, -15.61618434420927670, -40.45282443214609458 ) ) ;
#18156 = CARTESIAN_POINT ( 'NONE',  ( 10.48948069982380105, 31.98855470695709968, -45.62594161163059425 ) ) ;
#18157 = CARTESIAN_POINT ( 'NONE',  ( 73.01560786460549934, 1.024253516290730026, -62.17688587085479668 ) ) ;
#18158 = AXIS2_PLACEMENT_3D ( 'NONE', #45820, #5724, #41881 ) ;
#18159 = CARTESIAN_POINT ( 'NONE',  ( 65.03565853454030332, -32.24739025123630398, -17.83341341673349945 ) ) ;
#18160 = EDGE_CURVE ( 'NONE', #35235, #24503, #41729, .T. ) ;
#18161 = CARTESIAN_POINT ( 'NONE',  ( 68.13393739769618662, -0.1661889446793515246, -40.64999999999999858 ) ) ;
#18162 = ORIENTED_EDGE ( 'NONE', *, *, #15618, .F. ) ;
#18163 = VERTEX_POINT ( 'NONE', #47122 ) ;
#18164 = LINE ( 'NONE', #41753, #35391 ) ;
#18165 = CARTESIAN_POINT ( 'NONE',  ( 76.55049685366816448, -0.2018179213733399535, -13.44501669363641660 ) ) ;
#18166 = ORIENTED_EDGE ( 'NONE', *, *, #19847, .F. ) ;
#18167 = CARTESIAN_POINT ( 'NONE',  ( 11.35394641258329962, -64.66333705649719832, -45.68067175734550744 ) ) ;
#18168 = CARTESIAN_POINT ( 'NONE',  ( 57.50591362654369476, -45.29938006876010093, -25.92779769412700119 ) ) ;
#18169 = CARTESIAN_POINT ( 'NONE',  ( 24.04493739746428815, -15.61625192653408867, -77.50767849141614363 ) ) ;
#18170 = CARTESIAN_POINT ( 'NONE',  ( 64.63032832047218790, 1.424120032878319897, -61.18002170558170150 ) ) ;
#18171 = EDGE_LOOP ( 'NONE', ( #26239, #37193, #47380, #29042 ) ) ;
#18172 = DIRECTION ( 'NONE',  ( 0.8204012560548787913, -0.5717882292104107256, 0.000000000000000000 ) ) ;
#18173 = CARTESIAN_POINT ( 'NONE',  ( 46.49483455572801915, 6.970689097494132014, -57.84551077717584633 ) ) ;
#18174 = VERTEX_POINT ( 'NONE', #7789 ) ;
#18175 = CARTESIAN_POINT ( 'NONE',  ( 50.22560452902379780, -45.20442735010659874, -11.33119790093519974 ) ) ;
#18176 = VECTOR ( 'NONE', #4639, 1000.000000000000000 ) ;
#18177 = CARTESIAN_POINT ( 'NONE',  ( 68.13393739769618662, -29.66618894467940137, -65.65000000000000568 ) ) ;
#18178 = CARTESIAN_POINT ( 'NONE',  ( 15.24233146012789852, 19.83809465259359683, -21.55962016778659773 ) ) ;
#18179 = DIRECTION ( 'NONE',  ( 0.000000000000000000, 0.000000000000000000, 1.000000000000000000 ) ) ;
#18180 = EDGE_CURVE ( 'NONE', #11866, #42806, #37002, .T. ) ;
#18181 = CARTESIAN_POINT ( 'NONE',  ( 26.52624224310950396, -21.61618894467929763, -22.14999999999999858 ) ) ;
#18182 = CARTESIAN_POINT ( 'NONE',  ( 47.18305862770080239, -54.80685414274160649, -74.19838441418400521 ) ) ;
#18183 = CARTESIAN_POINT ( 'NONE',  ( 57.81379994192599270, 13.88381319346640019, -10.22123296806000070 ) ) ;
#18184 = CARTESIAN_POINT ( 'NONE',  ( 53.38983091223769151, 13.88381105532070059, -12.71718895194310051 ) ) ;
#18185 = LINE ( 'NONE', #45718, #5817 ) ;
#18186 = CARTESIAN_POINT ( 'NONE',  ( 51.03828701151719827, 19.65712598545220047, -76.15016576382599567 ) ) ;
#18187 = AXIS2_PLACEMENT_3D ( 'NONE', #32115, #44198, #40781 ) ;
#18188 = CARTESIAN_POINT ( 'NONE',  ( 57.97678121319430034, 13.89683454802320028, -25.62129778225950005 ) ) ;
#18189 = EDGE_CURVE ( 'NONE', #42080, #13020, #9410, .T. ) ;
#18190 = CARTESIAN_POINT ( 'NONE',  ( 8.146821171731881250, -17.66281912668999965, -36.42782227743549583 ) ) ;
#18191 = ORIENTED_EDGE ( 'NONE', *, *, #38086, .F. ) ;
#18193 = EDGE_CURVE ( 'NONE', #16042, #49834, #51212, .T. ) ;
#18192 = CYLINDRICAL_SURFACE ( 'NONE', #18838, 1.999999999999999112 ) ;
#18194 = CARTESIAN_POINT ( 'NONE',  ( 9.342107117190629140, -63.49215653426838912, -16.98584847438329959 ) ) ;
#18195 = CARTESIAN_POINT ( 'NONE',  ( 28.13393739769619728, -22.54439217495490055, -35.14999999999999858 ) ) ;
#18196 = CARTESIAN_POINT ( 'NONE',  ( 72.94809253479790812, 1.136600705753959994, -69.15465073100889981 ) ) ;
#18197 = EDGE_CURVE ( 'NONE', #4375, #4255, #39503, .T. ) ;
#18198 = CARTESIAN_POINT ( 'NONE',  ( 19.54510609474682070, -55.47047341688053024, -75.55236793428606745 ) ) ;
#18199 = LINE ( 'NONE', #42579, #32321 ) ;
#18200 = CARTESIAN_POINT ( 'NONE',  ( 68.77953295920740118, -5.818188944679350882, -66.11905263132939581 ) ) ;
#18201 = CARTESIAN_POINT ( 'NONE',  ( 42.42181532145059464, 11.95990745222249885, -3.882827786777780066 ) ) ;
#18202 = CARTESIAN_POINT ( 'NONE',  ( 47.41051750051865099, -54.24117355796746409, -75.29851419690288594 ) ) ;
#18203 = DIRECTION ( 'NONE',  ( 0.000000000000000000, -1.000000000000000000, 0.000000000000000000 ) ) ;
#18204 = CARTESIAN_POINT ( 'NONE',  ( 11.27214961228822077, -21.94227111097665883, -56.50067963292104878 ) ) ;
#18205 = CARTESIAN_POINT ( 'NONE',  ( 75.88268604566961528, -43.33643966824376292, -13.56553953253932221 ) ) ;
#18206 = CARTESIAN_POINT ( 'NONE',  ( 18.66092887556369817, -51.71967070378909881, -74.96248001586319276 ) ) ;
#18207 = CARTESIAN_POINT ( 'NONE',  ( 38.67452568954060155, 6.328436186825659782, -81.65000000000000568 ) ) ;
#18208 = ORIENTED_EDGE ( 'NONE', *, *, #17263, .F. ) ;
#18209 = ADVANCED_FACE ( 'NONE', ( #29495 ), #4614, .T. ) ;
#18210 = CARTESIAN_POINT ( 'NONE',  ( 23.28093797997669867, -17.72025097209759892, -55.15847778952939962 ) ) ;
#18211 = CARTESIAN_POINT ( 'NONE',  ( 63.55532107491779215, 1.170697810385689985, -61.82264208582909504 ) ) ;
#18212 = ORIENTED_EDGE ( 'NONE', *, *, #51310, .F. ) ;
#18213 = CARTESIAN_POINT ( 'NONE',  ( 10.72262114908336983, -19.77486415900381900, -69.24448638217960195 ) ) ;
#18214 = CYLINDRICAL_SURFACE ( 'NONE', #10001, 21.19999999999999929 ) ;
#18215 = CARTESIAN_POINT ( 'NONE',  ( 9.367299438200719308, -15.61632798465739924, -73.84717978381010539 ) ) ;
#18216 = CARTESIAN_POINT ( 'NONE',  ( 11.27217523151439948, -21.94228989780888028, -62.21597027386932410 ) ) ;
#18217 = CARTESIAN_POINT ( 'NONE',  ( 22.72481313846669337, -13.84495410388251280, -74.36948689368070120 ) ) ;
#18218 = CARTESIAN_POINT ( 'NONE',  ( 10.34909372178839959, -19.24960104513710135, -81.23899999999999011 ) ) ;
#18219 = FACE_OUTER_BOUND ( 'NONE', #38991, .T. ) ;
#18220 = ADVANCED_FACE ( 'NONE', ( #16671 ), #37114, .T. ) ;
#18221 = ORIENTED_EDGE ( 'NONE', *, *, #30064, .F. ) ;
#18222 = ORIENTED_EDGE ( 'NONE', *, *, #19788, .F. ) ;
#18223 = ORIENTED_EDGE ( 'NONE', *, *, #36959, .T. ) ;
#18224 = CARTESIAN_POINT ( 'NONE',  ( -22.69491836354699288, -19.22720705397727059, -54.67294082763422125 ) ) ;
#18225 = CARTESIAN_POINT ( 'NONE',  ( 9.367243689500000414, -15.61633989587210003, -59.45282021618999835 ) ) ;
#18226 = VECTOR ( 'NONE', #22666, 1000.000000000000000 ) ;
#18227 = ORIENTED_EDGE ( 'NONE', *, *, #51871, .F. ) ;
#18228 = ORIENTED_EDGE ( 'NONE', *, *, #48977, .T. ) ;
#18229 = CARTESIAN_POINT ( 'NONE',  ( 24.04483843941790866, -15.61617050235280679, -77.50767555791956909 ) ) ;
#18230 = CARTESIAN_POINT ( 'NONE',  ( 15.24816392691948508, -22.38319193469252610, -52.99448569864885883 ) ) ;
#18231 = CARTESIAN_POINT ( 'NONE',  ( 20.29256454187332537, -10.20483503270093628, -54.16115577807332215 ) ) ;
#18232 = VERTEX_POINT ( 'NONE', #21112 ) ;
#18233 = CARTESIAN_POINT ( 'NONE',  ( 0.3188172270368339611, -46.24795913321420215, -34.65000333199999716 ) ) ;
#18234 = CARTESIAN_POINT ( 'NONE',  ( 53.05142860133209837, -50.57489361360730129, -76.69950309512469744 ) ) ;
#18235 = CARTESIAN_POINT ( 'NONE',  ( 60.77470318442130548, 14.33787658508280138, -47.45003995119949991 ) ) ;
#18236 = CARTESIAN_POINT ( 'NONE',  ( 23.92239988244430293, -16.57878944086319706, -70.05163682948989390 ) ) ;
#18237 = CARTESIAN_POINT ( 'NONE',  ( 64.43393739769619799, 10.88381105532070059, -64.04999999999999716 ) ) ;
#18238 = CARTESIAN_POINT ( 'NONE',  ( 43.31519929709109817, 13.88514758459549903, -6.625476116054790587 ) ) ;
#18239 = CARTESIAN_POINT ( 'NONE',  ( 41.78486010873790235, -43.67282288760589637, -3.688051967278440202 ) ) ;
#18240 = DIRECTION ( 'NONE',  ( -0.8732394366197182567, 0.4872913772396111343, 0.000000000000000000 ) ) ;
#18241 = DIRECTION ( 'NONE',  ( 0.000000000000000000, 0.000000000000000000, -1.000000000000000000 ) ) ;
#18242 = CARTESIAN_POINT ( 'NONE',  ( 64.87665750633441064, 1.391769041008540153, -70.25462587105869261 ) ) ;
#18243 = CARTESIAN_POINT ( 'NONE',  ( 47.13393657218789912, 8.048130458325550407, -53.76789950451890121 ) ) ;
#18244 = CARTESIAN_POINT ( 'NONE',  ( 8.223454620794861114, -15.61605491354059971, -46.50766849176290663 ) ) ;
#18245 = ORIENTED_EDGE ( 'NONE', *, *, #33822, .T. ) ;
#18247 = ADVANCED_FACE ( 'NONE', ( #28454, #33159 ), #48390, .T. ) ;
#18246 = CARTESIAN_POINT ( 'NONE',  ( 14.94451915430260058, -52.96147345225150360, -76.14999999999999147 ) ) ;
#18248 = CARTESIAN_POINT ( 'NONE',  ( 57.25902743554100027, 19.38381105532069881, -53.91576847614940249 ) ) ;
#18249 = EDGE_CURVE ( 'NONE', #44616, #33500, #26093, .T. ) ;
#18250 = CARTESIAN_POINT ( 'NONE',  ( 45.08270409799413869, -40.03629360808191961, -61.41132920995301703 ) ) ;
#18251 = DIRECTION ( 'NONE',  ( 0.000000000000000000, -1.000000000000000000, 0.000000000000000000 ) ) ;
#18252 = AXIS2_PLACEMENT_3D ( 'NONE', #19334, #11225, #11997 ) ;
#18253 = CARTESIAN_POINT ( 'NONE',  ( 47.18055146300900304, -54.80119377569329941, -74.36335264244719667 ) ) ;
#18254 = CARTESIAN_POINT ( 'NONE',  ( 63.34300561417320807, 1.326324093417220240, -68.83951043167449768 ) ) ;
#18255 = CARTESIAN_POINT ( 'NONE',  ( 48.22131873952969983, -54.24500364010060594, -54.90936548946649509 ) ) ;
#18256 = DIRECTION ( 'NONE',  ( 0.000000000000000000, 0.000000000000000000, 1.000000000000000000 ) ) ;
#18257 = CARTESIAN_POINT ( 'NONE',  ( 56.50529364678479993, 19.52722159213979936, -53.84464738411570295 ) ) ;
#18258 = CARTESIAN_POINT ( 'NONE',  ( 48.06666922905080241, 23.09813023377000007, -54.98957115198240331 ) ) ;
#18259 = VERTEX_POINT ( 'NONE', #20848 ) ;
#18260 = CARTESIAN_POINT ( 'NONE',  ( 13.14827817127709864, -9.226478610231410471, -72.20804185874739289 ) ) ;
#18261 = ORIENTED_EDGE ( 'NONE', *, *, #163, .F. ) ;
#18262 = CARTESIAN_POINT ( 'NONE',  ( 71.35858828687760536, 1.188042061556800144, -70.59681938162209747 ) ) ;
#18263 = CYLINDRICAL_SURFACE ( 'NONE', #8679, 2.999999999999999112 ) ;
#18264 = LINE ( 'NONE', #6229, #27713 ) ;
#18265 = CARTESIAN_POINT ( 'NONE',  ( 73.26121012496899709, 0.8838110553206759423, -68.76625967790960203 ) ) ;
#18267 = CARTESIAN_POINT ( 'NONE',  ( 52.67986940689019804, 18.50721041040169723, -27.55370633776830047 ) ) ;
#18266 = CARTESIAN_POINT ( 'NONE',  ( 83.98295738300248559, 13.34738318005249980, -47.35112499062080360 ) ) ;
#18268 = CARTESIAN_POINT ( 'NONE',  ( 13.68194553784909928, -9.003300359821770016, -79.83979650029878883 ) ) ;
#18269 = FACE_OUTER_BOUND ( 'NONE', #16519, .T. ) ;
#18270 = CARTESIAN_POINT ( 'NONE',  ( 71.40893329644839582, 0.8879664753683499390, -70.67740027405390890 ) ) ;
#18271 = DIRECTION ( 'NONE',  ( 1.000000000000000000, 0.000000000000000000, 0.000000000000000000 ) ) ;
#18272 = ADVANCED_FACE ( 'NONE', ( #25026 ), #37683, .T. ) ;
#18273 = ORIENTED_EDGE ( 'NONE', *, *, #13913, .F. ) ;
#18274 = CARTESIAN_POINT ( 'NONE',  ( 11.51160566532330165, 19.89559162839070083, -21.14999999999999858 ) ) ;
#18275 = EDGE_CURVE ( 'NONE', #44695, #3841, #39331, .T. ) ;
#18276 = ORIENTED_EDGE ( 'NONE', *, *, #40869, .T. ) ;
#18277 = CARTESIAN_POINT ( 'NONE',  ( 12.36320305068320025, -64.54682834576858852, -15.76422791927960176 ) ) ;
#18278 = CARTESIAN_POINT ( 'NONE',  ( 24.04462281140675728, -15.61619016268715399, -39.50767146438039390 ) ) ;
#18279 = CARTESIAN_POINT ( 'NONE',  ( -7.616062602303800055, -62.11618894467930119, 16.35000000000000142 ) ) ;
#18280 = DIRECTION ( 'NONE',  ( -0.5000000000000012212, -0.8660254037844380415, 0.000000000000000000 ) ) ;
#18281 = EDGE_LOOP ( 'NONE', ( #30294, #41182, #41123, #31908 ) ) ;
#18282 = VERTEX_POINT ( 'NONE', #10374 ) ;
#18283 = CARTESIAN_POINT ( 'NONE',  ( -22.72850738805879800, -13.72396512373410005, -54.52996344323300093 ) ) ;
#18284 = CARTESIAN_POINT ( 'NONE',  ( 56.63366319918780079, 14.90690265212999854, -26.25716060252799622 ) ) ;
#18285 = CARTESIAN_POINT ( 'NONE',  ( 52.70796924836110264, 18.47694211103949513, -48.28462455411140297 ) ) ;
#18286 = CARTESIAN_POINT ( 'NONE',  ( 16.13393739769620083, -15.61618894467929941, -5.093415854460129566 ) ) ;
#18287 = CARTESIAN_POINT ( 'NONE',  ( 51.58109477403640852, -50.32311754940320014, -76.34882668000840056 ) ) ;
#18288 = CARTESIAN_POINT ( 'NONE',  ( 57.07871704937310398, -50.59515825109639309, -53.12705742518219409 ) ) ;
#18289 = VERTEX_POINT ( 'NONE', #34977 ) ;
#18290 = CARTESIAN_POINT ( 'NONE',  ( 20.11426146801901993, -8.759875404557478262, -33.45974718993613806 ) ) ;
#18291 = CARTESIAN_POINT ( 'NONE',  ( 67.04038824939814845, 19.47158195952278703, -71.50000000000200373 ) ) ;
#18292 = ORIENTED_EDGE ( 'NONE', *, *, #19288, .T. ) ;
#18293 = CARTESIAN_POINT ( 'NONE',  ( 16.13393739769620083, -15.61618894467929941, -6.649999999999999467 ) ) ;
#18294 = VECTOR ( 'NONE', #26548, 1000.000000000000000 ) ;
#18295 = CARTESIAN_POINT ( 'NONE',  ( 16.13393739769620083, -29.47259540523039689, -47.64999999999999858 ) ) ;
#18296 = VECTOR ( 'NONE', #32239, 1000.000000000000000 ) ;
#18297 = CARTESIAN_POINT ( 'NONE',  ( 13.30304109838990101, -8.296846506033869417, -47.39502254529469383 ) ) ;
#18298 = CARTESIAN_POINT ( 'NONE',  ( 13.86858776757270029, -50.80169362180370030, -21.50776138482320121 ) ) ;
#18299 = CARTESIAN_POINT ( 'NONE',  ( 56.55362051290479997, 19.42426019843370355, -75.00522130597019554 ) ) ;
#18300 = CARTESIAN_POINT ( 'NONE',  ( 47.44035392459380063, -54.31358006272590444, -75.17661032366730467 ) ) ;
#18301 = CARTESIAN_POINT ( 'NONE',  ( 56.79703944736839816, 13.88381105532070059, -15.79381048012069932 ) ) ;
#18302 = CARTESIAN_POINT ( 'NONE',  ( 22.90115736359569354, -15.61618877121331295, -78.84717825834033533 ) ) ;
#18303 =( BOUNDED_CURVE ( )  B_SPLINE_CURVE ( 3, ( #50604, #26733, #42491, #25953 ),
 .UNSPECIFIED., .F., .T. ) 
 B_SPLINE_CURVE_WITH_KNOTS ( ( 4, 4 ),
 ( 1.558720328957954759, 1.570796326794896558 ),
 .UNSPECIFIED. ) 
 CURVE ( )  GEOMETRIC_REPRESENTATION_ITEM ( )  RATIONAL_B_SPLINE_CURVE ( ( 1.000000000000000000, 0.9999878475599406347, 0.9999878475599406347, 1.000000000000000000 ) ) 
 REPRESENTATION_ITEM ( '' )  );
#18304 = CARTESIAN_POINT ( 'NONE',  ( 56.39270784037409356, -50.52750194525590643, -52.86271187285759510 ) ) ;
#18305 = CARTESIAN_POINT ( 'NONE',  ( 20.84741856749390365, -10.36969921949989981, -42.58016164095369760 ) ) ;
#18306 = DIRECTION ( 'NONE',  ( 1.000000000000000000, 0.000000000000000000, 0.000000000000000000 ) ) ;
#18307 = VERTEX_POINT ( 'NONE', #27884 ) ;
#18309 = EDGE_CURVE ( 'NONE', #30599, #48268, #51247, .T. ) ;
#18308 = CARTESIAN_POINT ( 'NONE',  ( 47.61801185651960111, 23.31248621914309993, -74.14999581977218668 ) ) ;
#18310 = CARTESIAN_POINT ( 'NONE',  ( 64.99546124159368787, 0.9209567800143640959, -60.53623002923360730 ) ) ;
#18311 = CARTESIAN_POINT ( 'NONE',  ( 60.41799884498815487, -45.84359652593187917, -47.74079192425801921 ) ) ;
#18312 = CARTESIAN_POINT ( 'NONE',  ( 12.16144474485684768, -65.27546953796887408, -23.67678868528984282 ) ) ;
#18313 = FACE_OUTER_BOUND ( 'NONE', #16343, .T. ) ;
#18314 = CARTESIAN_POINT ( 'NONE',  ( 16.13393739769620083, -38.61618894467930119, -59.64999999999999147 ) ) ;
#18315 = CARTESIAN_POINT ( 'NONE',  ( 82.13853704237929776, 14.37236558661899899, -47.68296857959820301 ) ) ;
#18316 = CARTESIAN_POINT ( 'NONE',  ( 0.2534322734540089828, 19.67561520348110093, -34.54509924001159504 ) ) ;
#18318 = CARTESIAN_POINT ( 'NONE',  ( 43.00218716632829796, -37.73344212960819988, -75.30702696467470503 ) ) ;
#18317 = DIRECTION ( 'NONE',  ( 1.000000000000000000, 0.000000000000000000, 0.000000000000000000 ) ) ;
#18319 = CARTESIAN_POINT ( 'NONE',  ( 15.01656936500493167, -23.47607714972237147, -32.33735170919545254 ) ) ;
#18320 = CARTESIAN_POINT ( 'NONE',  ( -32.51565489538130294, -10.90840876578639929, -55.84912116621229927 ) ) ;
#18321 = ORIENTED_EDGE ( 'NONE', *, *, #2141, .T. ) ;
#18322 = CARTESIAN_POINT ( 'NONE',  ( 53.30562535473109875, -49.43700197435749999, -49.00290876415049723 ) ) ;
#18323 = ORIENTED_EDGE ( 'NONE', *, *, #48316, .F. ) ;
#18324 = CIRCLE ( 'NONE', #25870, 2.000000000005381029 ) ;
#18325 = CARTESIAN_POINT ( 'NONE',  ( 13.61938558678000000, -51.42721352342299923, -23.15000000000000213 ) ) ;
#18326 = CARTESIAN_POINT ( 'NONE',  ( 23.04647607065054160, -19.60029144796367007, -73.95899818474369170 ) ) ;
#18327 = CARTESIAN_POINT ( 'NONE',  ( 14.26125502349160001, 19.88540718429639753, -22.45522374605300087 ) ) ;
#18328 = CARTESIAN_POINT ( 'NONE',  ( 55.88236915028019780, 14.71303907941189948, -25.32898514049750105 ) ) ;
#18329 = VECTOR ( 'NONE', #41395, 1000.000000000000000 ) ;
#18330 = CARTESIAN_POINT ( 'NONE',  ( 19.13110865206880007, -9.231870408720430632, -46.09253186719689666 ) ) ;
#18332 = CARTESIAN_POINT ( 'NONE',  ( 53.29384558423090112, 19.31433099946569953, -38.31189016485890875 ) ) ;
#18331 = AXIS2_PLACEMENT_3D ( 'NONE', #16232, #32188, #16749 ) ;
#18333 = CARTESIAN_POINT ( 'NONE',  ( 52.68730263070079900, 18.52618134853540255, -48.67466845563539835 ) ) ;
#18334 = CARTESIAN_POINT ( 'NONE',  ( 56.08437014463689962, -45.70248814750440403, -17.93020000568909822 ) ) ;
#18335 = EDGE_CURVE ( 'NONE', #44797, #27637, #43049, .T. ) ;
#18336 = DIRECTION ( 'NONE',  ( -0.4640893551880601597, 0.8857883891771953788, 0.000000000000000000 ) ) ;
#18337 = ORIENTED_EDGE ( 'NONE', *, *, #42944, .T. ) ;
#18338 = CARTESIAN_POINT ( 'NONE',  ( 22.05366437006999902, -10.46414267589130098, -39.05954089307479649 ) ) ;
#18339 = ADVANCED_FACE ( 'NONE', ( #373 ), #16354, .T. ) ;
#18340 = DIRECTION ( 'NONE',  ( 0.000000000000000000, 0.000000000000000000, -1.000000000000000000 ) ) ;
#18341 = CARTESIAN_POINT ( 'NONE',  ( 11.42523121492209803, 34.02364939933359977, -47.34553053307450199 ) ) ;
#18342 = CARTESIAN_POINT ( 'NONE',  ( 73.02275056366489991, 1.266538207494809942, -62.46861950876320435 ) ) ;
#18343 = CARTESIAN_POINT ( 'NONE',  ( 10.95445192191350081, -65.05736586563961055, -17.59525104008959673 ) ) ;
#18344 = CARTESIAN_POINT ( 'NONE',  ( 68.13393739769620083, -5.291188944679320549, -65.65000000000000568 ) ) ;
#18345 = CARTESIAN_POINT ( 'NONE',  ( 8.427199782394856342, -17.67924411827841524, -76.70928524612517663 ) ) ;
#18346 = CARTESIAN_POINT ( 'NONE',  ( 22.90088705258820667, -15.61618575905976414, -62.45282818884277276 ) ) ;
#18347 = CYLINDRICAL_SURFACE ( 'NONE', #41047, 7.910999999999997812 ) ;
#18348 = CARTESIAN_POINT ( 'NONE',  ( 65.07026117056300052, 1.388189907116970101, -70.28386057589730740 ) ) ;
#18349 = EDGE_LOOP ( 'NONE', ( #19131, #315, #25592, #31935 ) ) ;
#18350 = CARTESIAN_POINT ( 'NONE',  ( 10.14834886040009998, -63.32547621192500031, -45.99365407406120454 ) ) ;
#18351 = ORIENTED_EDGE ( 'NONE', *, *, #44721, .F. ) ;
#18352 = LINE ( 'NONE', #38029, #51824 ) ;
#18353 = CARTESIAN_POINT ( 'NONE',  ( 56.99190255423440021, 19.40009799747580033, -53.87165542209760360 ) ) ;
#18354 = CARTESIAN_POINT ( 'NONE',  ( 52.94902642261280334, 19.16795121501379739, -76.96923112046120252 ) ) ;
#18355 = EDGE_LOOP ( 'NONE', ( #33561, #16816, #22788, #8834 ) ) ;
#18356 = CARTESIAN_POINT ( 'NONE',  ( 12.39246200372603646, -65.46010474685600400, -47.59569286707705515 ) ) ;
#18357 = CARTESIAN_POINT ( 'NONE',  ( 63.34104417888273986, 21.88381105532059934, 11.14289321881345174 ) ) ;
#18358 = CARTESIAN_POINT ( 'NONE',  ( 22.90088360717968285, -15.58831960617060375, -72.45151510512926052 ) ) ;
#18359 = CARTESIAN_POINT ( 'NONE',  ( 9.221342996571138428, -11.63217922216438005, -42.95902251082229384 ) ) ;
#18360 = CARTESIAN_POINT ( 'NONE',  ( 14.75440393491079938, -23.74512537455679961, -66.34584096003959530 ) ) ;
#18361 = CARTESIAN_POINT ( 'NONE',  ( 61.28398356453099893, 14.37233669519349988, -47.68178229854910199 ) ) ;
#18362 = CARTESIAN_POINT ( 'NONE',  ( 44.36550484164386177, -37.96472317729350721, -68.49216281759998992 ) ) ;
#18363 = VERTEX_POINT ( 'NONE', #25750 ) ;
#18364 = VECTOR ( 'NONE', #46786, 1000.000000000000000 ) ;
#18365 = AXIS2_PLACEMENT_3D ( 'NONE', #30150, #46170, #14695 ) ;
#18366 = CARTESIAN_POINT ( 'NONE',  ( 56.77874227380610250, -46.03157376887470065, -26.24782688674920195 ) ) ;
#18367 = CARTESIAN_POINT ( 'NONE',  ( 9.453537067250739057, -12.31786433510400158, -55.37864069218029073 ) ) ;
#18368 = CIRCLE ( 'NONE', #42669, 2.000990444728826478 ) ;
#18369 = AXIS2_PLACEMENT_3D ( 'NONE', #47804, #31787, #51728 ) ;
#18370 = CARTESIAN_POINT ( 'NONE',  ( 8.821128736879460419, -16.36262873326029776, -32.14999999999999858 ) ) ;
#18371 = AXIS2_PLACEMENT_3D ( 'NONE', #39555, #51608, #15963 ) ;
#18373 = ADVANCED_FACE ( 'NONE', ( #22083 ), #6639, .T. ) ;
#18372 = DIRECTION ( 'NONE',  ( -0.7288689868556628149, -0.6846531968814575375, 0.000000000000000000 ) ) ;
#18374 = AXIS2_PLACEMENT_3D ( 'NONE', #22391, #50707, #50456 ) ;
#18375 = CARTESIAN_POINT ( 'NONE',  ( 13.67086563049960013, 20.77210737664869811, -75.25165125838280744 ) ) ;
#18376 = EDGE_CURVE ( 'NONE', #5505, #6515, #14497, .T. ) ;
#18377 = CARTESIAN_POINT ( 'NONE',  ( 14.06335392814032836, -7.911064159492109837, -51.20899709835300939 ) ) ;
#18378 = EDGE_CURVE ( 'NONE', #27172, #18529, #39516, .T. ) ;
#18379 = CARTESIAN_POINT ( 'NONE',  ( 41.48255094495939233, -45.14737637117200109, -5.927812803735399427 ) ) ;
#18380 = CARTESIAN_POINT ( 'NONE',  ( 24.04460466267867247, -15.53778724920028331, -61.50452191719739403 ) ) ;
#18381 = CARTESIAN_POINT ( 'NONE',  ( 18.61786603712990029, -7.754076046534380318, -65.10507532246559492 ) ) ;
#18382 = ORIENTED_EDGE ( 'NONE', *, *, #680, .T. ) ;
#18383 = CARTESIAN_POINT ( 'NONE',  ( 53.30594783414570514, -49.06367964803780524, -26.83653110996110414 ) ) ;
#18384 = CARTESIAN_POINT ( 'NONE',  ( 55.72320022523830119, -50.85322541441449573, -75.08289664133350527 ) ) ;
#18386 = CARTESIAN_POINT ( 'NONE',  ( 46.89857864678852195, -39.20081467324785507, -34.72191413131642435 ) ) ;
#18385 = CARTESIAN_POINT ( 'NONE',  ( 8.676985760002459358, 30.83576240877370012, -14.06454189394279908 ) ) ;
#18387 = CARTESIAN_POINT ( 'NONE',  ( 15.26098176771331438, -16.25042833492357985, -14.88746750000000141 ) ) ;
#18388 = DIRECTION ( 'NONE',  ( 0.000000000000000000, 1.000000000000000000, 0.000000000000000000 ) ) ;
#18389 = EDGE_LOOP ( 'NONE', ( #15696, #30471, #32984, #39709, #42998, #30911 ) ) ;
#18390 = CARTESIAN_POINT ( 'NONE',  ( 21.39066400359539699, -9.703911137440838885, -81.23899999999999011 ) ) ;
#18391 = CARTESIAN_POINT ( 'NONE',  ( 47.51200636829759816, 23.35279827620210114, -54.77739120475299472 ) ) ;
#18392 = EDGE_CURVE ( 'NONE', #42976, #5735, #31140, .T. ) ;
#18393 = CARTESIAN_POINT ( 'NONE',  ( 10.17245219797972844, -10.37354689578340228, -65.02189718388713402 ) ) ;
#18394 = CARTESIAN_POINT ( 'NONE',  ( 16.65420337943509566, -51.11618894467930119, -15.67544740040250062 ) ) ;
#18395 = CARTESIAN_POINT ( 'NONE',  ( 20.53650276133967267, 10.53025766472739555, -34.79644660940672907 ) ) ;
#18396 = CARTESIAN_POINT ( 'NONE',  ( 12.07292176418630092, 34.00632605457140301, -16.81897063588079888 ) ) ;
#18397 = CARTESIAN_POINT ( 'NONE',  ( 20.11167749483549727, -21.44028912360316497, -57.15644495666281699 ) ) ;
#18398 = CARTESIAN_POINT ( 'NONE',  ( 53.01430328511310108, 18.33235873846370012, -48.82220831118790016 ) ) ;
#18399 = CARTESIAN_POINT ( 'NONE',  ( 19.31281851427826979, 24.25684300136392579, -75.75074683321228974 ) ) ;
#18400 = CARTESIAN_POINT ( 'NONE',  ( 57.45269164222676750, -50.61618894467929408, -53.92796674551637182 ) ) ;
#18401 = CARTESIAN_POINT ( 'NONE',  ( 55.20995175243899666, 16.06746250602089887, -26.39668292074910028 ) ) ;
#18402 = CIRCLE ( 'NONE', #44329, 0.4999999999999982236 ) ;
#18403 = CARTESIAN_POINT ( 'NONE',  ( 50.54226496161154358, 4.781393461198343076, -76.21662484925313663 ) ) ;
#18404 = EDGE_CURVE ( 'NONE', #4073, #2764, #33626, .T. ) ;
#18405 = CIRCLE ( 'NONE', #2512, 18.86180339887500068 ) ;
#18406 = CARTESIAN_POINT ( 'NONE',  ( 63.31878016527869590, 0.9618743906590719872, -69.23017199065189686 ) ) ;
#18407 = CIRCLE ( 'NONE', #51037, 0.4999999999999935052 ) ;
#18408 = CARTESIAN_POINT ( 'NONE',  ( 52.82359344163219816, 18.46824642947949968, -48.95125676800460468 ) ) ;
#18409 = CARTESIAN_POINT ( 'NONE',  ( 20.00021293481310991, 23.80000987844158900, -18.69523849944957661 ) ) ;
#18410 = CARTESIAN_POINT ( 'NONE',  ( 10.49122530401870002, 32.03394370215789877, -45.62557954680809758 ) ) ;
#18411 = CARTESIAN_POINT ( 'NONE',  ( 72.73408845884699758, 1.392490173688170074, -62.38007352545039907 ) ) ;
#18412 = CIRCLE ( 'NONE', #10075, 0.5002499999041537526 ) ;
#18413 = CIRCLE ( 'NONE', #41869, 10.00000000000000888 ) ;
#18414 = CARTESIAN_POINT ( 'NONE',  ( 67.26279129939560164, -32.31925440466879706, -18.54865058075920103 ) ) ;
#18415 = CARTESIAN_POINT ( 'NONE',  ( 22.90148701646199925, -15.69275899496028970, -46.85077873481721156 ) ) ;
#18416 = ORIENTED_EDGE ( 'NONE', *, *, #47019, .T. ) ;
#18417 = EDGE_LOOP ( 'NONE', ( #49287, #38883, #3931, #38213 ) ) ;
#18418 = CARTESIAN_POINT ( 'NONE',  ( 56.83258906378680564, 19.07284248766010393, -52.72698304056530105 ) ) ;
#18419 = CARTESIAN_POINT ( 'NONE',  ( 76.49775090137842426, -3.049984699541625321, -13.21772653487406579 ) ) ;
#18420 = ORIENTED_EDGE ( 'NONE', *, *, #29343, .T. ) ;
#18421 = CARTESIAN_POINT ( 'NONE',  ( 12.71291116475580019, -65.48164264958541025, -47.17968986901090034 ) ) ;
#18422 = CARTESIAN_POINT ( 'NONE',  ( 56.05387567297529472, -45.72969253901850095, -25.37923299446759984 ) ) ;
#18423 = CARTESIAN_POINT ( 'NONE',  ( 23.11602277574511177, -19.35578214976509415, -77.66417765721635647 ) ) ;
#18424 = CARTESIAN_POINT ( 'NONE',  ( 51.67587649748470113, -33.96749857170579645, -77.01363636363508647 ) ) ;
#18425 = CARTESIAN_POINT ( 'NONE',  ( 11.53606103740170674, 24.11867657901759188, -21.73577486392030167 ) ) ;
#18426 = ORIENTED_EDGE ( 'NONE', *, *, #38949, .T. ) ;
#18427 = FACE_BOUND ( 'NONE', #9794, .T. ) ;
#18428 = CARTESIAN_POINT ( 'NONE',  ( 46.71043997899148081, 6.991105343399341088, -56.76743462289293518 ) ) ;
#18429 = CARTESIAN_POINT ( 'NONE',  ( 9.367121035360348458, -15.18956524623389726, -45.86723877108192937 ) ) ;
#18430 = ORIENTED_EDGE ( 'NONE', *, *, #42489, .T. ) ;
#18431 = CARTESIAN_POINT ( 'NONE',  ( 20.06347647389389977, -8.367641317401169232, -35.45045784522799437 ) ) ;
#18432 = DIRECTION ( 'NONE',  ( -1.000000000000000000, 0.000000000000000000, 0.000000000000000000 ) ) ;
#18433 = CARTESIAN_POINT ( 'NONE',  ( 14.61081989482540067, 19.82232334755109804, -21.82083395457759778 ) ) ;
#18434 = CARTESIAN_POINT ( 'NONE',  ( 19.20490796821585278, -21.71094733663775855, -50.80397083643239853 ) ) ;
#18435 = CARTESIAN_POINT ( 'NONE',  ( 12.72589019024139745, -21.52906861929441718, -47.11946018635927658 ) ) ;
#18436 = CARTESIAN_POINT ( 'NONE',  ( 73.11690592692650625, 0.8925687589132609290, -68.99219224778180148 ) ) ;
#18437 = CARTESIAN_POINT ( 'NONE',  ( 46.40846215724359780, -53.01587003390369546, -76.14999999999999147 ) ) ;
#18438 = CARTESIAN_POINT ( 'NONE',  ( 61.43493858089180293, 13.88381322377179927, -11.19371918816710121 ) ) ;
#18439 = ADVANCED_FACE ( 'NONE', ( #5864 ), #38618, .T. ) ;
#18440 = CARTESIAN_POINT ( 'NONE',  ( -0.03447620312153085176, -4.141051901845263394, -34.79644660940673617 ) ) ;
#18441 = AXIS2_PLACEMENT_3D ( 'NONE', #17668, #37847, #33109 ) ;
#18442 = EDGE_CURVE ( 'NONE', #19573, #30462, #8576, .T. ) ;
#18443 = VECTOR ( 'NONE', #13726, 999.9999999999998863 ) ;
#18444 = EDGE_CURVE ( 'NONE', #33168, #50858, #19265, .T. ) ;
#18445 = CIRCLE ( 'NONE', #14301, 38.49999999999998579 ) ;
#18446 = CARTESIAN_POINT ( 'NONE',  ( 53.12919740953070402, 20.11397505193579960, -75.74183034380359913 ) ) ;
#18447 = DIRECTION ( 'NONE',  ( -0.1999849291396485207, 0.9797989733190221040, 0.000000000000000000 ) ) ;
#18448 = AXIS2_PLACEMENT_3D ( 'NONE', #50666, #10837, #30730 ) ;
#18449 = CLOSED_SHELL ( 'NONE', ( #2229, #23551, #27947, #21730, #39611, #9917, #21564, #644, #1892, #27720, #14260, #19685, #14325, #37490, #32690, #44127, #4039, #21202, #31840, #23500, #12765, #5427, #34104, #9817, #30005, #20974, #49485, #29214, #48574, #49005, #26809, #39241, #4491, #51217, #13068, #3371, #31741, #2415, #20693, #30739, #13491, #9430, #22880, #5625, #35527, #45973, #28799, #25397, #16491, #47177, #36480, #7823, #46358, #35193, #44883, #13505, #15656, #33753, #41161, #39680, #44135, #4016, #25209, #51825, #41000, #29516, #5040, #43671, #48339, #46520, #11167, #558, #42587, #43534, #22741, #37429, #19156, #50780, #6797, #47341, #12320, #41204, #21914, #44060, #4363, #49338, #12077, #29427, #17528, #2948, #8265, #15556, #9366, #2784, #22282, #6165, #2760, #3826, #51796, #22111, #44718, #30230, #16782, #3560, #14537, #51475, #50101, #49360, #5228, #3702, #25998, #44715, #33231, #33526, #27142, #39095, #16882, #44358, #1108, #7312, #38643, #38094, #35662, #10963, #17617, #43845, #6281, #39596, #18495, #16096, #48738, #11757, #3481, #12254, #19402, #37911, #35502, #37616, #41706, #42580, #15453, #18774, #20313, #14074, #17968, #38206, #7383, #26524, #10071, #1348, #17439, #9822, #13951, #3321, #38809, #30166, #11405, #14505, #1471, #18834, #17353, #49070, #11444, #12457, #28428, #6014, #46328, #10994, #24279, #28029, #33055, #48500, #5000, #37791, #18339, #22091, #36109, #47282, #46950, #26230, #45399, #25780, #32134, #17640, #27660, #9466, #23218, #2437, #10172, #4111, #24870, #36316, #41929, #34805, #10704, #25431, #18272, #19498, #9751, #47823, #27378, #26114, #47338, #22039, #46631, #37518, #19146, #26488, #42295, #49478, #32262, #42349, #28409, #36856, #23504, #13688, #30803, #10523, #28082, #22502, #12137, #21074, #49935, #26827, #30950, #35893, #25185, #51456, #23685, #44549, #37321, #48565, #41920, #23868, #21936, #7634, #28021, #44470, #31073, #38872, #21960, #23208, #33452, #37050, #31750, #9478, #50231, #7440, #18928, #44353, #11112, #1243, #15193, #1306, #26366, #17689, #49659, #29134, #47285, #3454, #19328, #12449, #32246, #13885, #44660, #15846, #37873, #28498, #40985, #23342, #10422, #4307, #11318, #47587, #2222, #25764, #12453, #39512, #17415, #9167, #14560, #14357, #20986, #9240, #47324, #7121, #46508, #50931, #16153, #17926, #10210, #28008, #37607, #33648, #25459, #19750, #15005, #13430, #1010, #25761, #51190, #28675, #7568, #45838, #32993, #6731, #48547, #27839, #14642, #25636, #4852, #10930, #16794, #24548, #29619, #46468, #50498, #42506, #41626, #36014, #1414, #43780, #5382, #8519, #33272, #19090, #27270, #32182, #34490, #36649, #25362, #25367, #47090, #48615, #24052, #50344, #33506, #29773, #27662, #12173, #3244, #27629, #22537, #9981, #4054, #40939, #25863, #18373, #8336, #40551, #28046, #17986, #19691, #15333, #808, #39737, #26082, #22042, #50191 ) ) ;
#18450 = EDGE_CURVE ( 'NONE', #21295, #27800, #38027, .T. ) ;
#18451 = CARTESIAN_POINT ( 'NONE',  ( 21.26076650159200199, -22.07361444172130049, -35.79407082892649328 ) ) ;
#18452 = B_SPLINE_SURFACE_WITH_KNOTS ( 'NONE', 3, 3, ( 
 ( #27586, #43590, #24860, #7695, #23132, #4972, #20941, #3760, #19727, #35719, #30998, #47025, #47779, #34019, #17034, #38235 ),
 ( #41383, #13363, #22226, #49268, #49012, #37714, #5749, #32985, #1812, #50029, #17792, #1554, #33765, #26158, #1301, #25894 ),
 ( #37202, #17542, #49777, #13870, #21705, #29826, #10199, #14123, #45064, #21195, #29578, #29323, #41132, #2075, #45328, #13117 ),
 ( #29068, #9433, #9166, #25122, #5243, #30088, #49526, #45845, #46113, #25382, #9932, #33513, #18054, #25637, #5500, #21456 ),
 ( #41907, #6007, #37455, #42168, #21966, #41640, #37976, #6267, #17291, #33252, #13617, #45584, #9678, #14894, #14638, #15421 ),
 ( #46890, #10976, #42433, #19341, #27195, #30608, #22742, #10715, #7298, #23249, #11497, #31374, #10460, #42949, #22485, #7558 ),
 ( #50547, #26943, #51061, #35055, #23502, #42693, #26671, #38760, #15160, #35325, #30348, #2855, #31120, #50295, #47145, #46372 ),
 ( #18819, #6523, #18567, #11234, #39266, #43208, #3368, #3113, #38491, #22997, #51324, #47401, #7045, #46629, #6788, #2593 ),
 ( #39018, #34802, #27454, #43456, #19080, #2327, #18301, #34273, #26414, #50806, #14383, #34544, #30861, #51831, #707, #24274 ),
 ( #32137, #27711, #4638, #12516, #15931, #8069, #47905, #44478, #8588, #48681, #16699, #47649, #28219, #7814, #44741, #39779 ) ),
 .UNSPECIFIED., .F., .F., .F.,
 ( 4, 1, 1, 1, 1, 1, 1, 4 ),
 ( 4, 2, 2, 2, 2, 2, 2, 4 ),
 ( -1.660620507699999833E-05, 0.1428571428571430157, 0.2857142857142860315, 0.4285714285714289917, 0.5714285714285709528, 0.7142857142857139685, 0.8571428571428569843, 1.000000000000000000 ),
 ( -4.238744881723909508, -3.233993249338640297, -2.649205172199279978, -2.119364137759419897, -1.854443620539500071, -1.430570792987609918, -0.7523742689045949117, 1.660620507699999833E-05 ),
 .UNSPECIFIED. ) ;
#18453 = VERTEX_POINT ( 'NONE', #2708 ) ;
#18454 = CARTESIAN_POINT ( 'NONE',  ( 50.87608087775580401, 20.94596473442846474, -52.56694610553643798 ) ) ;
#18455 = CARTESIAN_POINT ( 'NONE',  ( -3.169058842316599733, -49.13863347070289933, -5.723027784144280261 ) ) ;
#18456 = CARTESIAN_POINT ( 'NONE',  ( 76.42237218134170007, -8.479666956846260817, -12.89291724745850054 ) ) ;
#18457 = FACE_OUTER_BOUND ( 'NONE', #8496, .T. ) ;
#18458 = CARTESIAN_POINT ( 'NONE',  ( 61.28085240419530066, -45.60177449860450594, -47.67834116410560341 ) ) ;
#18459 = DIRECTION ( 'NONE',  ( -1.000000000000000000, 0.000000000000000000, 0.000000000000000000 ) ) ;
#18460 = CYLINDRICAL_SURFACE ( 'NONE', #28144, 1.999999999999997113 ) ;
#18461 = DIRECTION ( 'NONE',  ( 0.5813178231270340612, 0.8136765871738268485, 0.000000000000000000 ) ) ;
#18462 = CARTESIAN_POINT ( 'NONE',  ( 42.10819013808320221, 12.38958205234360044, -4.221348723159180416 ) ) ;
#18463 = CARTESIAN_POINT ( 'NONE',  ( 83.89200044194980421, -48.61618894467930119, -53.92796738110899923 ) ) ;
#18464 = CARTESIAN_POINT ( 'NONE',  ( 20.08284749614042752, 24.18831317000414316, -74.66536237503798645 ) ) ;
#18465 = CARTESIAN_POINT ( 'NONE',  ( 56.48535462447713229, 19.53533792649655609, -53.84780261153423453 ) ) ;
#18466 = CARTESIAN_POINT ( 'NONE',  ( 76.09582226312808473, -43.31040105692301267, -13.69678534746457998 ) ) ;
#18467 = CARTESIAN_POINT ( 'NONE',  ( 18.17711126944659839, -51.44957460136649274, -75.17186369576970151 ) ) ;
#18469 = EDGE_CURVE ( 'NONE', #29987, #34524, #34163, .T. ) ;
#18468 = DIRECTION ( 'NONE',  ( 0.3294064756440933661, -0.9441882088883217783, -3.885780586188048878E-16 ) ) ;
#18470 = ORIENTED_EDGE ( 'NONE', *, *, #24738, .F. ) ;
#18471 = CARTESIAN_POINT ( 'NONE',  ( 11.73483375864000067, -9.603320950852721083, -54.36628847889309668 ) ) ;
#18472 = CARTESIAN_POINT ( 'NONE',  ( 63.77381348670360950, 1.342503070345590022, -61.69870111945830615 ) ) ;
#18473 = VERTEX_POINT ( 'NONE', #19456 ) ;
#18474 = DIRECTION ( 'NONE',  ( 0.000000000000000000, 0.000000000000000000, -1.000000000000000000 ) ) ;
#18475 = LINE ( 'NONE', #14547, #7540 ) ;
#18476 = DIRECTION ( 'NONE',  ( 0.000000000000000000, 0.000000000000000000, -1.000000000000000000 ) ) ;
#18477 = CARTESIAN_POINT ( 'NONE',  ( 23.10892566284617544, -19.36881467858842498, -61.66477234305963862 ) ) ;
#18478 = FACE_OUTER_BOUND ( 'NONE', #13289, .T. ) ;
#18479 = CARTESIAN_POINT ( 'NONE',  ( 9.157312613638797671, -16.66687816016379742, -81.23899999999999011 ) ) ;
#18480 = CARTESIAN_POINT ( 'NONE',  ( 10.09871813756559966, -54.07211264381389526, -34.88336916441289759 ) ) ;
#18481 = ORIENTED_EDGE ( 'NONE', *, *, #11889, .T. ) ;
#18482 = ORIENTED_EDGE ( 'NONE', *, *, #49978, .F. ) ;
#18483 = VERTEX_POINT ( 'NONE', #30727 ) ;
#18484 = CARTESIAN_POINT ( 'NONE',  ( -8.719958794165998839, 10.48190171173589924, -1.467676683391609949 ) ) ;
#18485 = CARTESIAN_POINT ( 'NONE',  ( 61.37851597766940159, -45.20507541364400339, -46.76684488029780340 ) ) ;
#18486 = DIRECTION ( 'NONE',  ( 0.4743737082415240836, -0.8803235683140521184, 0.000000000000000000 ) ) ;
#18487 = VECTOR ( 'NONE', #31713, 1000.000000000000000 ) ;
#18488 = CARTESIAN_POINT ( 'NONE',  ( 82.61176104757076644, -45.25366171719064567, -47.15273383853318734 ) ) ;
#18489 = CONICAL_SURFACE ( 'NONE', #15989, 3.567506086244481622, 0.04995839572194331335 ) ;
#18490 = EDGE_CURVE ( 'NONE', #17993, #8898, #7723, .T. ) ;
#18491 = VERTEX_POINT ( 'NONE', #50918 ) ;
#18492 = VECTOR ( 'NONE', #39818, 1000.000000000000000 ) ;
#18493 = ORIENTED_EDGE ( 'NONE', *, *, #20845, .T. ) ;
#18494 = CARTESIAN_POINT ( 'NONE',  ( 22.90034292835611751, -15.71307119870275848, -72.45738199783259859 ) ) ;
#18495 = ADVANCED_FACE ( 'NONE', ( #31488, #27060 ), #15535, .T. ) ;
#18496 = CARTESIAN_POINT ( 'NONE',  ( 16.13393739769620083, -15.61618894467929941, -23.15000000000000213 ) ) ;
#18497 = ORIENTED_EDGE ( 'NONE', *, *, #19210, .T. ) ;
#18498 = CARTESIAN_POINT ( 'NONE',  ( 13.53092308830080093, -23.16807188358326641, -50.11355989224952623 ) ) ;
#18499 = CARTESIAN_POINT ( 'NONE',  ( 53.12920058238260168, -51.34635257275360232, -75.74182960172289825 ) ) ;
#18500 = CARTESIAN_POINT ( 'NONE',  ( 60.35981425105420328, 14.50694145909750077, -47.43164998684069644 ) ) ;
#18501 = CARTESIAN_POINT ( 'NONE',  ( 9.119644240547859937, -19.13562627146119866, -76.86446490096111006 ) ) ;
#18502 = DIRECTION ( 'NONE',  ( 1.000000000000000000, 0.000000000000000000, 0.000000000000000000 ) ) ;
#18503 = CARTESIAN_POINT ( 'NONE',  ( 41.26856075654099953, -44.30227235397150309, -4.473876447391639921 ) ) ;
#18504 = CARTESIAN_POINT ( 'NONE',  ( 72.38393739883420608, 11.88381105532070059, -61.34712802272770915 ) ) ;
#18505 = CARTESIAN_POINT ( 'NONE',  ( 53.35699421374690132, 18.69401400300939642, -74.14999999999999147 ) ) ;
#18506 = EDGE_CURVE ( 'NONE', #1848, #41267, #39133, .T. ) ;
#18507 = CARTESIAN_POINT ( 'NONE',  ( 64.68616649449130307, 1.374598250659150089, -70.24664079970339969 ) ) ;
#18508 = DIRECTION ( 'NONE',  ( 0.000000000000000000, 0.000000000000000000, -1.000000000000000000 ) ) ;
#18509 = CARTESIAN_POINT ( 'NONE',  ( 9.205734167420720482, -3.616188944679329165, -24.15000000000000213 ) ) ;
#18510 = EDGE_CURVE ( 'NONE', #6855, #42670, #6110, .T. ) ;
#18511 = CARTESIAN_POINT ( 'NONE',  ( 23.36532317189500318, -12.56761420098369975, -53.16051062239899494 ) ) ;
#18512 = ORIENTED_EDGE ( 'NONE', *, *, #37668, .T. ) ;
#18513 = CARTESIAN_POINT ( 'NONE',  ( 15.05440318628160057, -53.11618894467930119, -76.14999999999999147 ) ) ;
#18514 = CARTESIAN_POINT ( 'NONE',  ( 43.44336167987420083, 14.78804531073750006, -7.898836396374890434 ) ) ;
#18515 = CARTESIAN_POINT ( 'NONE',  ( 71.61827519252990726, 1.134960180547589959, -70.47795848906230276 ) ) ;
#18516 = CARTESIAN_POINT ( 'NONE',  ( 44.35599058648487159, -39.98315081151604744, -64.93502037408133276 ) ) ;
#18517 = CARTESIAN_POINT ( 'NONE',  ( 11.25398292730271699, 32.98847748115480982, -44.13762314148468846 ) ) ;
#18518 = AXIS2_PLACEMENT_3D ( 'NONE', #3654, #8097, #43739 ) ;
#18519 = AXIS2_PLACEMENT_3D ( 'NONE', #42485, #2905, #3163 ) ;
#18520 = CARTESIAN_POINT ( 'NONE',  ( 22.06174470004240007, -11.92280751385899862, -32.14999999999999858 ) ) ;
#18521 = AXIS2_PLACEMENT_3D ( 'NONE', #45376, #12899, #9221 ) ;
#18522 = CARTESIAN_POINT ( 'NONE',  ( 63.19978792402569923, 1.187415670095769871, -68.89659930051639947 ) ) ;
#18523 = CARTESIAN_POINT ( 'NONE',  ( 47.93639096317230042, -54.33238953985980402, -54.72300757058719967 ) ) ;
#18524 = CARTESIAN_POINT ( 'NONE',  ( 22.52295300047549276, -13.38580680388945332, -80.74026669357201058 ) ) ;
#18525 = CARTESIAN_POINT ( 'NONE',  ( 56.51188083447149779, 19.51190917532160185, -53.61551639950400272 ) ) ;
#18526 = CARTESIAN_POINT ( 'NONE',  ( 47.87127561442579804, 23.20009848796649976, -55.10367382876560072 ) ) ;
#18527 = ORIENTED_EDGE ( 'NONE', *, *, #40911, .F. ) ;
#18528 = CARTESIAN_POINT ( 'NONE',  ( 12.20533024450969961, -21.47354372396169708, -75.53523696341939342 ) ) ;
#18529 = VERTEX_POINT ( 'NONE', #48274 ) ;
#18530 = CARTESIAN_POINT ( 'NONE',  ( 71.41482173131041122, 1.096036836948800053, -70.62529907715760658 ) ) ;
#18531 = CARTESIAN_POINT ( 'NONE',  ( 82.68191173840780550, 14.16984533597115892, -47.42735572498546048 ) ) ;
#18532 = CARTESIAN_POINT ( 'NONE',  ( 56.17779366879769753, -45.64891426883350078, -28.15000000000000213 ) ) ;
#18533 = CARTESIAN_POINT ( 'NONE',  ( 16.67840439675140018, -22.64798205764600070, -74.92822277435448086 ) ) ;
#18534 = CARTESIAN_POINT ( 'NONE',  ( 46.63833728752520358, -15.61618894467929586, 8.349999999999999645 ) ) ;
#18535 = CARTESIAN_POINT ( 'NONE',  ( 9.221493846662148997, -11.63192146079378908, -66.95899777436285660 ) ) ;
#18536 = CARTESIAN_POINT ( 'NONE',  ( 19.13393739769620083, -49.61618894467939356, -35.14999999999999858 ) ) ;
#18537 = ORIENTED_EDGE ( 'NONE', *, *, #8832, .F. ) ;
#18538 = DIRECTION ( 'NONE',  ( -0.3863301728269175062, -0.9223605572462019175, 3.330669073875470114E-16 ) ) ;
#18539 = VERTEX_POINT ( 'NONE', #40663 ) ;
#18540 = ORIENTED_EDGE ( 'NONE', *, *, #31136, .F. ) ;
#18541 = CARTESIAN_POINT ( 'NONE',  ( 12.13449217321720042, -64.93994367287498903, -16.24910028839300224 ) ) ;
#18542 = CARTESIAN_POINT ( 'NONE',  ( 55.40394000045360201, 13.88381105524500114, -14.52023566624100148 ) ) ;
#18543 = CARTESIAN_POINT ( 'NONE',  ( 11.96163130524179863, 33.91328095712900392, -45.68067242534929306 ) ) ;
#18544 = CARTESIAN_POINT ( 'NONE',  ( 9.596651609803041438, -63.85482046095769704, -46.54795879700470351 ) ) ;
#18545 = EDGE_LOOP ( 'NONE', ( #40930, #44181, #31379, #48136 ) ) ;
#18546 = ADVANCED_FACE ( 'NONE', ( #40404 ), #11123, .T. ) ;
#18547 = ORIENTED_EDGE ( 'NONE', *, *, #18084, .F. ) ;
#18548 = CARTESIAN_POINT ( 'NONE',  ( 71.65889518049858964, 0.9150552061894319245, -60.79444388203420147 ) ) ;
#18549 = CARTESIAN_POINT ( 'NONE',  ( 56.65715976508769813, 14.88738284562609948, -26.25499670583540279 ) ) ;
#18550 = EDGE_CURVE ( 'NONE', #35503, #1409, #44210, .T. ) ;
#18551 = CARTESIAN_POINT ( 'NONE',  ( 53.24163931742309330, 18.19088059586060169, -48.94155518170179420 ) ) ;
#18552 = CARTESIAN_POINT ( 'NONE',  ( 59.45957930948410564, -2.821832259794109898, -15.69652041387840313 ) ) ;
#18553 = CARTESIAN_POINT ( 'NONE',  ( 50.76151237207749745, -49.57686851637080139, -76.22310723638240404 ) ) ;
#18554 = ADVANCED_FACE ( 'NONE', ( #28594 ), #41225, .T. ) ;
#18555 = CARTESIAN_POINT ( 'NONE',  ( 58.94369020000790726, -48.22803363231889762, -50.52845975241639565 ) ) ;
#18556 = ORIENTED_EDGE ( 'NONE', *, *, #49418, .F. ) ;
#18557 = DIRECTION ( 'NONE',  ( -1.000000000000000000, 0.000000000000000000, 0.000000000000000000 ) ) ;
#18558 = CARTESIAN_POINT ( 'NONE',  ( 68.13393739769810509, 19.38381105532030091, -71.50000000000198952 ) ) ;
#18559 = ORIENTED_EDGE ( 'NONE', *, *, #8212, .F. ) ;
#18560 = DIRECTION ( 'NONE',  ( 0.000000000000000000, 1.000000000000000000, 0.000000000000000000 ) ) ;
#18561 = FACE_OUTER_BOUND ( 'NONE', #20815, .T. ) ;
#18562 = CIRCLE ( 'NONE', #44487, 1.999999999999999556 ) ;
#18563 = CARTESIAN_POINT ( 'NONE',  ( 20.31321962299979944, -8.973874011401631989, -41.69125950871409003 ) ) ;
#18564 = CARTESIAN_POINT ( 'NONE',  ( 13.72445191873659986, -50.97659916996759932, -21.83805850002029914 ) ) ;
#18565 = CARTESIAN_POINT ( 'NONE',  ( 55.08889524890580702, 19.54142126883120056, -75.71946145358849378 ) ) ;
#18566 = CARTESIAN_POINT ( 'NONE',  ( 47.45530976305949622, -54.40699705883139359, -75.00633330157590706 ) ) ;
#18567 = CARTESIAN_POINT ( 'NONE',  ( 55.86383447201379937, 13.89944776690939854, -14.96898266773339969 ) ) ;
#18568 = CARTESIAN_POINT ( 'NONE',  ( 9.366428224829499882, -15.61611423639980067, -77.45282021618989177 ) ) ;
#18569 = DIRECTION ( 'NONE',  ( 0.000000000000000000, 0.000000000000000000, -1.000000000000000000 ) ) ;
#18570 = CARTESIAN_POINT ( 'NONE',  ( 11.26840393093330128, -10.51039387845690065, -42.10484805457209490 ) ) ;
#18571 = DIRECTION ( 'NONE',  ( -0.04100182651872445044, -0.05643417272666771678, -0.9975640502598241977 ) ) ;
#18572 = ADVANCED_FACE ( 'NONE', ( #20732 ), #49063, .T. ) ;
#18573 = ORIENTED_EDGE ( 'NONE', *, *, #17349, .T. ) ;
#18574 = CARTESIAN_POINT ( 'NONE',  ( 47.51796367685790301, 23.14532755365199890, -75.00952367221340467 ) ) ;
#18575 = CARTESIAN_POINT ( 'NONE',  ( 64.95255690645950608, 1.266538207494809942, -60.76118683403129950 ) ) ;
#18576 = CARTESIAN_POINT ( 'NONE',  ( 42.48913188665730445, -45.89176091220130616, -7.200515191634200285 ) ) ;
#18577 = CARTESIAN_POINT ( 'NONE',  ( 105.5832649133809156, -15.41618894467909051, -28.20067248431509199 ) ) ;
#18578 = CARTESIAN_POINT ( 'NONE',  ( 71.33393739769628894, 10.88381105532070059, -69.34999999999999432 ) ) ;
#18579 = DIRECTION ( 'NONE',  ( 1.000000000000000000, 0.000000000000000000, 0.000000000000000000 ) ) ;
#18580 = CARTESIAN_POINT ( 'NONE',  ( 82.31238640809949914, 14.12525339545430114, -47.32928036526049453 ) ) ;
#18581 = DIRECTION ( 'NONE',  ( 0.000000000000000000, 0.000000000000000000, 1.000000000000000000 ) ) ;
#18583 = CARTESIAN_POINT ( 'NONE',  ( 46.38156616808179677, -40.25946647325027783, -54.52593885421595132 ) ) ;
#18582 = CARTESIAN_POINT ( 'NONE',  ( 44.13393739769620083, -36.11618894467930119, -35.14999999999999858 ) ) ;
#18584 = CARTESIAN_POINT ( 'NONE',  ( 24.03648926733799840, -15.22123262239629504, -71.49178105483443346 ) ) ;
#18585 = CARTESIAN_POINT ( 'NONE',  ( -12.40573950840240158, 24.76782207504269806, -51.46982831076010001 ) ) ;
#18586 = ORIENTED_EDGE ( 'NONE', *, *, #47979, .T. ) ;
#18587 = AXIS2_PLACEMENT_3D ( 'NONE', #14243, #13734, #34398 ) ;
#18588 = CARTESIAN_POINT ( 'NONE',  ( 52.79729141543799642, -49.69127189832200031, -48.80671576205540418 ) ) ;
#18589 = CIRCLE ( 'NONE', #33630, 10.00000000000000711 ) ;
#18590 = EDGE_LOOP ( 'NONE', ( #33903, #37064, #2551, #47360 ) ) ;
#18591 = AXIS2_PLACEMENT_3D ( 'NONE', #8462, #40683, #39660 ) ;
#18592 = CARTESIAN_POINT ( 'NONE',  ( 45.46242224712364077, 8.938650005438001145, -59.13099268088515714 ) ) ;
#18593 = CARTESIAN_POINT ( 'NONE',  ( 9.366721379915048828, -15.33582998764832617, -39.86035918413693224 ) ) ;
#18594 = CARTESIAN_POINT ( 'NONE',  ( 13.81672828808540032, 19.99687498807509911, -22.59435085047379843 ) ) ;
#18595 = DIRECTION ( 'NONE',  ( -1.062456999999999985E-16, 7.719205000000000365E-17, 1.000000000000000000 ) ) ;
#18596 = CARTESIAN_POINT ( 'NONE',  ( 14.41393119263600120, -8.776295864288348625, -43.87440179741569324 ) ) ;
#18597 = CARTESIAN_POINT ( 'NONE',  ( 28.88047141014000019, -26.64595108362729903, -34.71367995918279092 ) ) ;
#18598 = CARTESIAN_POINT ( 'NONE',  ( 52.61723362075139931, 18.57919235090369980, -48.56631533107179877 ) ) ;
#18599 = CARTESIAN_POINT ( 'NONE',  ( 54.87171479455280121, -45.91467920100570410, -15.83443052021550201 ) ) ;
#18600 = DIRECTION ( 'NONE',  ( 0.6676418852214537347, -0.2329255526947816568, 0.7071067811863875896 ) ) ;
#18601 = ORIENTED_EDGE ( 'NONE', *, *, #28201, .F. ) ;
#18602 = CARTESIAN_POINT ( 'NONE',  ( 18.39333206953279998, -8.100734545543689435, -32.88046427011239814 ) ) ;
#18603 = CARTESIAN_POINT ( 'NONE',  ( 10.85466582836159866, -64.96696992582000973, -17.55961494274349732 ) ) ;
#18604 = CARTESIAN_POINT ( 'NONE',  ( 12.82693890801849967, 34.27287537764330239, -47.70039286047789773 ) ) ;
#18605 = CARTESIAN_POINT ( 'NONE',  ( 73.15215840802929392, 0.9242073871622918935, -62.36095669330580193 ) ) ;
#18606 = CARTESIAN_POINT ( 'NONE',  ( 11.91450189635219914, -65.43783483100590104, -17.98631677234039827 ) ) ;
#18607 = CARTESIAN_POINT ( 'NONE',  ( 53.41947877929934663, -49.46401953720203437, -49.21225703112888539 ) ) ;
#18608 = CARTESIAN_POINT ( 'NONE',  ( 24.04476267751569551, -15.67298808999131232, -75.79461090121749578 ) ) ;
#18609 = CARTESIAN_POINT ( 'NONE',  ( -22.09888148991248968, 14.93421758625839146, 11.34999999999999964 ) ) ;
#18610 = ORIENTED_EDGE ( 'NONE', *, *, #40800, .F. ) ;
#18611 = CARTESIAN_POINT ( 'NONE',  ( 64.74712693194939561, 0.8966068345641440285, -70.60278586552529134 ) ) ;
#18612 = VERTEX_POINT ( 'NONE', #24652 ) ;
#18613 = CARTESIAN_POINT ( 'NONE',  ( 10.97954134168909945, -63.36237133050840242, -44.74488567032319963 ) ) ;
#18614 = EDGE_CURVE ( 'NONE', #32183, #25882, #45118, .T. ) ;
#18615 = DIRECTION ( 'NONE',  ( -1.000000000000000000, 0.000000000000000000, 0.000000000000000000 ) ) ;
#18616 = EDGE_LOOP ( 'NONE', ( #11177, #24419, #44668, #28710, #11989, #1271, #44719, #28105, #13039, #6763, #4312, #29373, #23362, #44178 ) ) ;
#18617 = CARTESIAN_POINT ( 'NONE',  ( 0.3209249304026170480, -8.218592747557250888, -34.64999999999999858 ) ) ;
#18618 = CARTESIAN_POINT ( 'NONE',  ( 56.94040701897879586, 19.11191676585499977, -52.81451654899269954 ) ) ;
#18619 = CARTESIAN_POINT ( 'NONE',  ( 52.47790439711100419, 19.10383386520929605, -76.75890347663309399 ) ) ;
#18620 =( BOUNDED_CURVE ( )  B_SPLINE_CURVE ( 3, ( #34694, #3002, #18973, #14793 ),
 .UNSPECIFIED., .F., .T. ) 
 B_SPLINE_CURVE_WITH_KNOTS ( ( 4, 4 ),
 ( 4.114144097965610314, 4.712388980384689674 ),
 .UNSPECIFIED. ) 
 CURVE ( )  GEOMETRIC_REPRESENTATION_ITEM ( )  RATIONAL_B_SPLINE_CURVE ( ( 1.000000000000000000, 0.9703969717270918283, 0.9703969717270918283, 1.000000000000000000 ) ) 
 REPRESENTATION_ITEM ( '' )  );
#18621 = EDGE_LOOP ( 'NONE', ( #37891, #41878, #12482, #12264, #40099 ) ) ;
#18622 = CARTESIAN_POINT ( 'NONE',  ( 10.73552253366480791, -65.02568017672894030, -47.16673513639202042 ) ) ;
#18623 = CARTESIAN_POINT ( 'NONE',  ( 73.38393739769610136, 11.88381105532070059, -84.94863984844540994 ) ) ;
#18624 = DIRECTION ( 'NONE',  ( 0.000000000000000000, 0.000000000000000000, 1.000000000000000000 ) ) ;
#18625 = CARTESIAN_POINT ( 'NONE',  ( 23.06214062797170072, -3.616188944679349149, -24.14999999999999858 ) ) ;
#18626 = CARTESIAN_POINT ( 'NONE',  ( 16.24108513978070079, -7.371721744350270278, -67.29646813280308493 ) ) ;
#18627 = FACE_OUTER_BOUND ( 'NONE', #26992, .T. ) ;
#18628 = CARTESIAN_POINT ( 'NONE',  ( 45.23524973664237336, -38.07011267116087794, -64.14340693299787688 ) ) ;
#18629 = B_SPLINE_CURVE_WITH_KNOTS ( 'NONE', 3,
 ( #48620, #21328, #37076, #8780, #33387, #45202, #5120, #29195, #32333, #25258 ),
 .UNSPECIFIED., .F., .F.,
 ( 4, 1, 1, 1, 1, 1, 1, 4 ),
 ( 0.5000017723907246303, 0.5455675515341791293, 0.6247864825977968994, 0.7040054136614146696, 0.7832243447250346602, 0.8624432757886524303, 0.9416622068522703115, 1.000000000000000000 ),
 .UNSPECIFIED. ) ;
#18630 = EDGE_LOOP ( 'NONE', ( #24264, #48523, #37771, #8866 ) ) ;
#18631 = CARTESIAN_POINT ( 'NONE',  ( -22.82535044970985538, -14.17006684274750583, -54.73606930856294639 ) ) ;
#18632 = CARTESIAN_POINT ( 'NONE',  ( 10.55445623026200153, -20.55340310930620262, -53.00207276027180114 ) ) ;
#18633 = CIRCLE ( 'NONE', #32001, 0.5000000000000004441 ) ;
#18634 = CARTESIAN_POINT ( 'NONE',  ( 53.55180673896649779, -49.41892566828619948, -49.22385633645210135 ) ) ;
#18635 = CARTESIAN_POINT ( 'NONE',  ( 8.975904575304079813, -14.67896029866649954, -32.14999999999999858 ) ) ;
#18636 = EDGE_CURVE ( 'NONE', #36069, #25155, #44334, .T. ) ;
#18637 = CYLINDRICAL_SURFACE ( 'NONE', #28171, 7.910999999999997812 ) ;
#18638 = EDGE_CURVE ( 'NONE', #43625, #13682, #40922, .T. ) ;
#18639 = CARTESIAN_POINT ( 'NONE',  ( 45.31002868286061869, -45.55093754943392526, -8.676028226913116370 ) ) ;
#18640 = LINE ( 'NONE', #14714, #51611 ) ;
#18641 = CARTESIAN_POINT ( 'NONE',  ( 45.73972096110129826, -45.13933825624529561, -7.826076092515011240 ) ) ;
#18642 = CARTESIAN_POINT ( 'NONE',  ( 22.63786127318122965, -11.06313073300040095, -61.31321979917446185 ) ) ;
#18643 = CARTESIAN_POINT ( 'NONE',  ( 23.67593780178180296, -18.94799785482829790, -67.64008111650160515 ) ) ;
#18644 = ORIENTED_EDGE ( 'NONE', *, *, #18636, .T. ) ;
#18645 = CARTESIAN_POINT ( 'NONE',  ( 53.67452698258109933, -48.64253627208800168, -26.37822025900080192 ) ) ;
#18646 = CIRCLE ( 'NONE', #34541, 1.000000000000000444 ) ;
#18647 = CARTESIAN_POINT ( 'NONE',  ( 54.67791766314789470, -50.80000226043880218, -75.87478752159950091 ) ) ;
#18649 = CARTESIAN_POINT ( 'NONE',  ( 41.42428665458552928, -39.70010360968180407, -79.11029697435235164 ) ) ;
#18648 = CARTESIAN_POINT ( 'NONE',  ( -2.620161787266110043, 18.79900506017029826, -6.313712515450228935 ) ) ;
#18650 = CARTESIAN_POINT ( 'NONE',  ( 20.53650276133967267, 10.53025766472739555, -34.79644660940672907 ) ) ;
#18651 = DIRECTION ( 'NONE',  ( 0.8090169943749462300, -0.5877852522924749135, 0.000000000000000000 ) ) ;
#18652 = ORIENTED_EDGE ( 'NONE', *, *, #2724, .T. ) ;
#18653 = FACE_OUTER_BOUND ( 'NONE', #46656, .T. ) ;
#18654 = CARTESIAN_POINT ( 'NONE',  ( 47.65224270186909905, 23.25978157783099931, -54.72055524659549519 ) ) ;
#18655 = CARTESIAN_POINT ( 'NONE',  ( 42.44161405036800261, -44.94940367324450392, -5.942266020708489194 ) ) ;
#18656 = CARTESIAN_POINT ( 'NONE',  ( 16.29798161965023340, -51.09008541970372619, -15.67302014731996884 ) ) ;
#18657 = CARTESIAN_POINT ( 'NONE',  ( 12.13393739769600010, -55.41568642894409180, -74.14999999999999147 ) ) ;
#18658 = CARTESIAN_POINT ( 'NONE',  ( 11.98493272671680110, 33.91167211021750205, -16.63579482024520217 ) ) ;
#18659 = DIRECTION ( 'NONE',  ( 0.000000000000000000, 0.000000000000000000, -1.000000000000000000 ) ) ;
#18660 = CARTESIAN_POINT ( 'NONE',  ( 52.92965938904679746, 18.37620054566669836, -48.75165688956650456 ) ) ;
#18661 = CYLINDRICAL_SURFACE ( 'NONE', #22483, 1.000000000000001332 ) ;
#18662 = CARTESIAN_POINT ( 'NONE',  ( 59.53646453344369860, -46.29317990693370177, -47.84962771692820382 ) ) ;
#18663 = CARTESIAN_POINT ( 'NONE',  ( 53.47775468590610615, 17.84057308464530323, -27.23453477576759951 ) ) ;
#18664 = CARTESIAN_POINT ( 'NONE',  ( 50.50438588722870747, 22.08300093761100058, -54.79905802874080223 ) ) ;
#18665 = VECTOR ( 'NONE', #48568, 1000.000000000000000 ) ;
#18666 = CARTESIAN_POINT ( 'NONE',  ( 52.93759153535863504, -49.56812172796623628, -27.78191009280273249 ) ) ;
#18667 = CARTESIAN_POINT ( 'NONE',  ( 12.33251669429900055, -64.64566256145140244, -15.86092359077770020 ) ) ;
#18668 = CARTESIAN_POINT ( 'NONE',  ( 8.428829098684769150, -17.68683844382469061, -76.42434267299502437 ) ) ;
#18669 = CARTESIAN_POINT ( 'NONE',  ( 71.26909468036909345, 1.099973129953850215, -60.58645605602389850 ) ) ;
#18670 = CARTESIAN_POINT ( 'NONE',  ( 11.10533104901869983, 31.90439051286449867, -44.25028207899379851 ) ) ;
#18671 = TOROIDAL_SURFACE ( 'NONE', #21977, 19.30901699437490038, 0.5000000000000000000 ) ;
#18672 = CARTESIAN_POINT ( 'NONE',  ( 72.66369507718221143, 1.405464757956500055, -62.20504966370589983 ) ) ;
#18673 = CARTESIAN_POINT ( 'NONE',  ( 9.366937397696199596, -15.61618894467949836, -28.45282021618999835 ) ) ;
#18674 = CARTESIAN_POINT ( 'NONE',  ( 12.61864224197218753, 24.22902235285175365, -75.44170189642458979 ) ) ;
#18675 = ORIENTED_EDGE ( 'NONE', *, *, #11553, .F. ) ;
#18676 = ORIENTED_EDGE ( 'NONE', *, *, #35058, .T. ) ;
#18677 = CARTESIAN_POINT ( 'NONE',  ( 10.47081843707153581, -34.50169217863195570, -84.65000000000000568 ) ) ;
#18678 = EDGE_CURVE ( 'NONE', #30160, #14876, #22935, .T. ) ;
#18679 = CARTESIAN_POINT ( 'NONE',  ( 49.44253838235640330, -2.211264110977851249, -15.73253926033974004 ) ) ;
#18680 = ORIENTED_EDGE ( 'NONE', *, *, #37362, .T. ) ;
#18681 = CARTESIAN_POINT ( 'NONE',  ( 11.61883035538269837, -64.83086464985760244, -45.15685323010969654 ) ) ;
#18682 = CARTESIAN_POINT ( 'NONE',  ( 57.58585165456680244, -45.11742656075429636, -25.40978046210479846 ) ) ;
#18683 = CARTESIAN_POINT ( 'NONE',  ( 19.14634567751863514, -22.94949537724593824, -77.88358313659429655 ) ) ;
#18684 = CARTESIAN_POINT ( 'NONE',  ( 63.50007682179899149, 1.388189907116970101, -68.71367622713330547 ) ) ;
#18685 = ORIENTED_EDGE ( 'NONE', *, *, #15196, .F. ) ;
#18686 = B_SPLINE_CURVE_WITH_KNOTS ( 'NONE', 3,
 ( #38217, #34257, #50280, #14366, #46356, #31614, #7285, #19584, #23489, #46876, #15918, #43952, #39513, #3613, #51560, #47133, #43442, #19329, #11993, #51812, #3355, #35309, #23235, #39765, #27698, #15661, #8053, #26927, #47632, #38747, #51309, #11739, #7545, #43696, #34785, #7800, #14880, #42933 ),
 .UNSPECIFIED., .F., .F.,
 ( 4, 2, 2, 2, 2, 2, 2, 2, 2, 2, 2, 2, 2, 2, 1, 1, 1, 1, 1, 1, 2, 4 ),
 ( 0.000000000000000000, 0.06250074569407504388, 0.1250014913881500878, 0.1875022370822251316, 0.2500029827763001755, 0.2812533556233377530, 0.3125037284703753304, 0.3437541013174129079, 0.3750044741644504298, 0.4062548470114880628, 0.4375052198585256402, 0.4687555927055632177, 0.4843807791290819509, 0.4921933723408414285, 0.4960996689467210841, 0.4980528172496609396, 0.4990293914011308951, 0.4995176784768657896, 0.4997618220147331813, 0.4998838937836668772, 0.4999449296681337529, 0.5000059655526006841 ),
 .UNSPECIFIED. ) ;
#18687 = CARTESIAN_POINT ( 'NONE',  ( 44.42648819202516108, 6.740347691462509339, -68.18724196164413343 ) ) ;
#18688 = CARTESIAN_POINT ( 'NONE',  ( 11.68627894964089897, 34.01944678469089922, -23.21012450963720042 ) ) ;
#18689 = ORIENTED_EDGE ( 'NONE', *, *, #45476, .F. ) ;
#18690 = CARTESIAN_POINT ( 'NONE',  ( 10.90943883812770032, -9.237527312442798788, -33.07388991331939820 ) ) ;
#18691 = AXIS2_PLACEMENT_3D ( 'NONE', #6738, #39217, #35795 ) ;
#18692 = DIRECTION ( 'NONE',  ( 0.000000000000000000, -1.000000000000000000, 0.000000000000000000 ) ) ;
#18693 = CARTESIAN_POINT ( 'NONE',  ( 71.83393739769618946, 10.88381105532070059, -67.25000000000000000 ) ) ;
#18694 = DIRECTION ( 'NONE',  ( 1.000000000000000000, 0.000000000000000000, 0.000000000000000000 ) ) ;
#18695 = CARTESIAN_POINT ( 'NONE',  ( 11.97524499910796969, -21.02749279390264192, -47.16112356747648704 ) ) ;
#18696 = CARTESIAN_POINT ( 'NONE',  ( 14.53575789044414179, 20.42331746235014123, -75.51793353177379231 ) ) ;
#18697 = CARTESIAN_POINT ( 'NONE',  ( 47.29369706019910780, -54.69301655985149324, -74.50208837960660446 ) ) ;
#18698 = CARTESIAN_POINT ( 'NONE',  ( 56.12350828326769658, 13.88381105527479953, -10.09721077832690028 ) ) ;
#18699 = ADVANCED_FACE ( 'NONE', ( #3099 ), #41965, .T. ) ;
#18700 = DIRECTION ( 'NONE',  ( -1.000000000000000000, 0.000000000000000000, 0.000000000000000000 ) ) ;
#18701 = CIRCLE ( 'NONE', #37116, 20.00000000000001421 ) ;
#18702 = CIRCLE ( 'NONE', #12020, 0.5000000000822003576 ) ;
#18703 = CARTESIAN_POINT ( 'NONE',  ( 52.03944399862420056, 20.14552308598300101, -75.97489327918991364 ) ) ;
#18704 = CARTESIAN_POINT ( 'NONE',  ( 65.44700836391344012, -29.90809997924516495, -16.55186812364802051 ) ) ;
#18705 = CARTESIAN_POINT ( 'NONE',  ( 12.06625306698470013, -8.444253027749869744, -34.84344365616309602 ) ) ;
#18706 = EDGE_LOOP ( 'NONE', ( #40085, #4273, #48137, #50985 ) ) ;
#18707 = CARTESIAN_POINT ( 'NONE',  ( 55.20622393724549681, -47.44937218557269887, -26.50255988908530114 ) ) ;
#18708 = CARTESIAN_POINT ( 'NONE',  ( -0.1141852257953769878, -53.55957259884640109, -9.165264109987230512 ) ) ;
#18709 = CARTESIAN_POINT ( 'NONE',  ( 75.09787083995549040, -5.899466855358239670, -11.55750054373280022 ) ) ;
#18710 = B_SPLINE_CURVE_WITH_KNOTS ( 'NONE', 3,
 ( #13251, #29716, #1441, #1958, #9568, #29200, #45210, #49669, #33393, #42051, #5891, #17935, #13758, #41526, #33651, #21336 ),
 .UNSPECIFIED., .F., .F.,
 ( 4, 2, 2, 2, 2, 2, 2, 4 ),
 ( 6.605827000000000045E-15, 0.07319275283556900269, 0.1391693187718509861, 0.1804046724820269898, 0.2061767685508869852, 0.2577209606886070037, 0.3401916681089580119, 0.4123535371017659767 ),
 .UNSPECIFIED. ) ;
#18711 = CARTESIAN_POINT ( 'NONE',  ( 75.23800589958599971, 13.54856819491975628, -14.24441830867649550 ) ) ;
#18712 = CARTESIAN_POINT ( 'NONE',  ( 61.12479307673544326, -45.49567662917237243, -47.50325115173827584 ) ) ;
#18713 = PLANE ( 'NONE',  #8015 ) ;
#18714 = CARTESIAN_POINT ( 'NONE',  ( 82.13853704237929776, -45.64188066427789892, -47.72348187592570667 ) ) ;
#18715 = CARTESIAN_POINT ( 'NONE',  ( 20.13393739768959634, -55.41568642894479524, -74.14999999999999147 ) ) ;
#18716 = CARTESIAN_POINT ( 'NONE',  ( 41.80294713309100274, 12.64028208340220161, -4.284453812058900191 ) ) ;
#18717 = CARTESIAN_POINT ( 'NONE',  ( 61.50409964634459925, -45.37406455498979341, -47.35437808299670337 ) ) ;
#18718 = DIRECTION ( 'NONE',  ( 0.000000000000000000, -1.000000000000000000, 0.000000000000000000 ) ) ;
#18719 = DIRECTION ( 'NONE',  ( -0.6522074047277899300, 0.2731766849828906607, 0.7071067811865471286 ) ) ;
#18720 = CIRCLE ( 'NONE', #16215, 0.5000000000000045519 ) ;
#18721 = CARTESIAN_POINT ( 'NONE',  ( 76.42619217002265941, -43.25680179181886587, -13.99059237503525921 ) ) ;
#18722 = CARTESIAN_POINT ( 'NONE',  ( 18.19607795909060144, -52.32664520840270228, -75.76244777734170555 ) ) ;
#18723 = CARTESIAN_POINT ( 'NONE',  ( 50.34331689155069967, -43.49784654392259853, -6.583704156889679915 ) ) ;
#18724 = ORIENTED_EDGE ( 'NONE', *, *, #11827, .F. ) ;
#18725 = CARTESIAN_POINT ( 'NONE',  ( 10.69097154885009893, -10.52886969908080061, -52.30659627123909416 ) ) ;
#18726 = CARTESIAN_POINT ( 'NONE',  ( 63.71017317316999851, 1.107037132887370046, -61.60361627704830312 ) ) ;
#18727 = VERTEX_POINT ( 'NONE', #41436 ) ;
#18728 = DIRECTION ( 'NONE',  ( 0.000000000000000000, 0.000000000000000000, -1.000000000000000000 ) ) ;
#18729 = CARTESIAN_POINT ( 'NONE',  ( 61.25261794522180026, -45.60868630189549577, -47.68548325530770882 ) ) ;
#18730 = CARTESIAN_POINT ( 'NONE',  ( 73.24087495431770378, 0.9952464559119579279, -68.78371246661670568 ) ) ;
#18731 = CARTESIAN_POINT ( 'NONE',  ( 9.367206039829609310, -15.61603166621950045, -73.45282021618999124 ) ) ;
#18732 = DIRECTION ( 'NONE',  ( 0.000000000000000000, -1.000000000000000000, 0.000000000000000000 ) ) ;
#18733 = CARTESIAN_POINT ( 'NONE',  ( 40.95781332748470049, -45.40040647908620741, -5.890461096499439719 ) ) ;
#18734 = ORIENTED_EDGE ( 'NONE', *, *, #30208, .T. ) ;
#18735 = ORIENTED_EDGE ( 'NONE', *, *, #28969, .T. ) ;
#18736 = EDGE_CURVE ( 'NONE', #21139, #32383, #35344, .T. ) ;
#18737 = ORIENTED_EDGE ( 'NONE', *, *, #23177, .F. ) ;
#18738 = CYLINDRICAL_SURFACE ( 'NONE', #15164, 2.000000000000000000 ) ;
#18739 = CARTESIAN_POINT ( 'NONE',  ( 61.27165170594810206, -45.24929849883929478, -46.82601857492619501 ) ) ;
#18740 = DIRECTION ( 'NONE',  ( 0.000000000000000000, 0.000000000000000000, -1.000000000000000000 ) ) ;
#18741 = CARTESIAN_POINT ( 'NONE',  ( -22.40543978572512174, -21.82123808744384164, -54.48262838077054226 ) ) ;
#18742 = EDGE_CURVE ( 'NONE', #41285, #31407, #11097, .T. ) ;
#18743 = VECTOR ( 'NONE', #7826, 1000.000000000000000 ) ;
#18744 = EDGE_LOOP ( 'NONE', ( #34485, #44924, #40141, #36865, #28775, #25893 ) ) ;
#18745 = ADVANCED_FACE ( 'NONE', ( #37774 ), #14176, .T. ) ;
#18746 = CARTESIAN_POINT ( 'NONE',  ( 10.45401511118626026, -11.85366287480093561, -79.63887948191079147 ) ) ;
#18747 = ORIENTED_EDGE ( 'NONE', *, *, #46923, .T. ) ;
#18748 = CARTESIAN_POINT ( 'NONE',  ( -10.98165337464593350, -35.31681881277557977, -44.31573110638452562 ) ) ;
#18749 = CARTESIAN_POINT ( 'NONE',  ( 57.24929578595761370, 19.38381105532069881, -75.24227954309296251 ) ) ;
#18750 = ORIENTED_EDGE ( 'NONE', *, *, #40612, .T. ) ;
#18751 = DIRECTION ( 'NONE',  ( 0.000000000000000000, 0.000000000000000000, -1.000000000000000000 ) ) ;
#18752 = CARTESIAN_POINT ( 'NONE',  ( 51.08534762786979400, -51.03566300605200468, -76.14824064460249531 ) ) ;
#18753 = CARTESIAN_POINT ( 'NONE',  ( 60.57311214287879864, 14.37431803774079953, -47.23458252443460026 ) ) ;
#18754 = FACE_OUTER_BOUND ( 'NONE', #36068, .T. ) ;
#18755 = AXIS2_PLACEMENT_3D ( 'NONE', #42936, #7035, #27187 ) ;
#18756 = EDGE_CURVE ( 'NONE', #17858, #46747, #23333, .T. ) ;
#18757 = CARTESIAN_POINT ( 'NONE',  ( 43.01559835719150016, -42.64215176563499909, -3.897419375871189917 ) ) ;
#18758 = CARTESIAN_POINT ( 'NONE',  ( 0.3209249304026240424, 19.48649808507980197, -34.64999999999999858 ) ) ;
#18759 = CARTESIAN_POINT ( 'NONE',  ( -7.075746994739700035, 14.57312359469660201, -5.375837286899690426 ) ) ;
#18760 =( BOUNDED_CURVE ( )  B_SPLINE_CURVE ( 3, ( #36523, #7740, #15847, #40212 ),
 .UNSPECIFIED., .F., .T. ) 
 B_SPLINE_CURVE_WITH_KNOTS ( ( 4, 4 ),
 ( 3.701430267445704914, 3.744786642406928934 ),
 .UNSPECIFIED. ) 
 CURVE ( )  GEOMETRIC_REPRESENTATION_ITEM ( )  RATIONAL_B_SPLINE_CURVE ( ( 1.000000000000000000, 0.9998433581970664896, 0.9998433581970664896, 1.000000000000000000 ) ) 
 REPRESENTATION_ITEM ( '' )  );
#18761 = CARTESIAN_POINT ( 'NONE',  ( 64.65174547131330485, 1.408734182879959995, -70.16322028441409486 ) ) ;
#18762 = CARTESIAN_POINT ( 'NONE',  ( 10.13393739769589885, 22.91950879131600161, -35.14999999999999858 ) ) ;
#18763 = CARTESIAN_POINT ( 'NONE',  ( 27.73905384484250192, -51.70197538230620182, -75.56421356237308373 ) ) ;
#18764 = CARTESIAN_POINT ( 'NONE',  ( 21.69055479405609788, -21.15791713123389783, -55.53707855430759821 ) ) ;
#18765 = VERTEX_POINT ( 'NONE', #47132 ) ;
#18766 = B_SPLINE_CURVE_WITH_KNOTS ( 'NONE', 3,
 ( #50070, #25681, #18345, #21497, #38018, #10503, #21751, #37497, #34586, #13658, #33808, #1597, #30392, #38540, #37761, #17835, #2637, #17585, #29620, #50590, #45622, #46155, #9722, #18608, #14680, #10242, #26201, #22268 ),
 .UNSPECIFIED., .F., .F.,
 ( 4, 2, 2, 2, 2, 2, 2, 2, 2, 2, 1, 1, 1, 1, 2, 4 ),
 ( 0.000000000000000000, 0.06250047608285554113, 0.1250009521657110823, 0.1875014282485666095, 0.2500019043314221645, 0.3125023804142777473, 0.3750028564971332190, 0.4375033325799887463, 0.4687535706214165376, 0.4843786896421304333, 0.4921912491524875199, 0.4960975289076660077, 0.4980506687852552239, 0.4990272387240497487, 0.4995155236934472054, 0.5000038086628445511 ),
 .UNSPECIFIED. ) ;
#18767 = CARTESIAN_POINT ( 'NONE',  ( 14.46581869571789980, -52.64324949044350177, -76.02664804518839503 ) ) ;
#18768 = AXIS2_PLACEMENT_3D ( 'NONE', #25779, #34946, #10607 ) ;
#18769 = CARTESIAN_POINT ( 'NONE',  ( 57.43834588691519372, 18.88596480251339926, -52.60518497626989642 ) ) ;
#18770 = CARTESIAN_POINT ( 'NONE',  ( 71.57888773397908722, 1.405464757955549926, -70.17975767949100430 ) ) ;
#18771 = CARTESIAN_POINT ( 'NONE',  ( 44.72493418209450056, -40.01092346187889603, -63.14659530062845505 ) ) ;
#18772 = CARTESIAN_POINT ( 'NONE',  ( 15.03857555098429977, 19.44687904844289861, -20.69450120486289890 ) ) ;
#18774 = ADVANCED_FACE ( 'NONE', ( #17343 ), #25178, .T. ) ;
#18773 = CARTESIAN_POINT ( 'NONE',  ( 47.18324198357289845, -54.80726809202429450, -74.14999999999999147 ) ) ;
#18775 = DIRECTION ( 'NONE',  ( 1.000000000000000000, 0.000000000000000000, 0.000000000000000000 ) ) ;
#18776 = CARTESIAN_POINT ( 'NONE',  ( 47.88635031718219892, -54.41166180851149647, -54.97299310976289632 ) ) ;
#18777 = CARTESIAN_POINT ( 'NONE',  ( 23.14288469598330167, 17.63186702652449966, -35.14566363178219888 ) ) ;
#18778 = CARTESIAN_POINT ( 'NONE',  ( 56.44265055894529581, 19.46638121170060387, -53.28298866551109114 ) ) ;
#18779 = CIRCLE ( 'NONE', #43896, 1.000000000000000000 ) ;
#18780 = CARTESIAN_POINT ( 'NONE',  ( 47.89164947663859806, 23.14006492512999813, -54.78346000236360425 ) ) ;
#18781 = EDGE_LOOP ( 'NONE', ( #28974, #30819, #36256, #15996 ) ) ;
#18782 = CARTESIAN_POINT ( 'NONE',  ( 9.451921682515308731, -13.35937146058209990, -73.95085834214719966 ) ) ;
#18783 = ORIENTED_EDGE ( 'NONE', *, *, #22457, .T. ) ;
#18784 = CARTESIAN_POINT ( 'NONE',  ( 60.82468473753360172, -45.47215345142849685, -47.02385344690110713 ) ) ;
#18785 = CARTESIAN_POINT ( 'NONE',  ( 82.71778650988362358, 14.26036297868509806, -47.55446714344091674 ) ) ;
#18786 = DIRECTION ( 'NONE',  ( 0.000000000000000000, -1.000000000000000000, 0.000000000000000000 ) ) ;
#18788 = DIRECTION ( 'NONE',  ( 0.000000000000000000, 0.000000000000000000, 1.000000000000000000 ) ) ;
#18787 = CARTESIAN_POINT ( 'NONE',  ( 40.80516388273994721, 8.393954547589055792, -82.09339948163508893 ) ) ;
#18789 = DIRECTION ( 'NONE',  ( 0.000000000000000000, 0.000000000000000000, 1.000000000000000000 ) ) ;
#18790 = CARTESIAN_POINT ( 'NONE',  ( 20.99566010709231634, -9.290059359670648220, -67.50066313927187878 ) ) ;
#18791 = FACE_OUTER_BOUND ( 'NONE', #41507, .T. ) ;
#18792 = VERTEX_POINT ( 'NONE', #10253 ) ;
#18793 = DIRECTION ( 'NONE',  ( 1.000000000000000000, 0.000000000000000000, 0.000000000000000000 ) ) ;
#18794 = EDGE_LOOP ( 'NONE', ( #787, #33061, #30475, #10949 ) ) ;
#18795 = ORIENTED_EDGE ( 'NONE', *, *, #36418, .F. ) ;
#18796 = CARTESIAN_POINT ( 'NONE',  ( 12.21465728043759924, -64.70109133449230399, -15.93455456223260036 ) ) ;
#18797 = CARTESIAN_POINT ( 'NONE',  ( 24.04493739769619864, -15.61618894467929941, -32.14999999999999858 ) ) ;
#18798 = FACE_OUTER_BOUND ( 'NONE', #34594, .T. ) ;
#18799 = CARTESIAN_POINT ( 'NONE',  ( 9.874256513748090214, -64.47111594000269008, -46.84384315240179575 ) ) ;
#18800 = VERTEX_POINT ( 'NONE', #5295 ) ;
#18801 = ORIENTED_EDGE ( 'NONE', *, *, #3732, .T. ) ;
#18802 = EDGE_CURVE ( 'NONE', #26465, #8898, #26133, .T. ) ;
#18803 = CARTESIAN_POINT ( 'NONE',  ( 50.52790554252050015, 22.07298246124559782, -54.91101322106069915 ) ) ;
#18804 = CARTESIAN_POINT ( 'NONE',  ( 56.75395847353610179, 14.81488913387570072, -26.24860350449169744 ) ) ;
#18805 = AXIS2_PLACEMENT_3D ( 'NONE', #22369, #9566, #9825 ) ;
#18806 = CARTESIAN_POINT ( 'NONE',  ( 22.13393739769589885, 22.91950879131610108, -54.64999999999999858 ) ) ;
#18807 = CARTESIAN_POINT ( 'NONE',  ( 62.79356416660980500, 0.07457836432415800021, -16.79771323086600177 ) ) ;
#18808 = CARTESIAN_POINT ( 'NONE',  ( 52.11373191115499992, -49.71238562294659857, -77.07264795032170923 ) ) ;
#18809 = CARTESIAN_POINT ( 'NONE',  ( 57.57137425765949956, -49.32502029382759900, -51.58238510503450414 ) ) ;
#18810 = EDGE_LOOP ( 'NONE', ( #24644, #37099, #18865, #50137 ) ) ;
#18811 = FACE_OUTER_BOUND ( 'NONE', #1922, .T. ) ;
#18812 = DIRECTION ( 'NONE',  ( 0.000000000000000000, 0.000000000000000000, -1.000000000000000000 ) ) ;
#18813 = ORIENTED_EDGE ( 'NONE', *, *, #17544, .T. ) ;
#18814 = DIRECTION ( 'NONE',  ( 0.000000000000000000, 0.000000000000000000, 1.000000000000000000 ) ) ;
#18815 = CARTESIAN_POINT ( 'NONE',  ( 60.34379258661509482, -45.86802437805019395, -47.72732609191810127 ) ) ;
#18816 = CARTESIAN_POINT ( 'NONE',  ( 15.67252115383410072, -7.782043002620109284, -45.49376819976779984 ) ) ;
#18817 = CARTESIAN_POINT ( 'NONE',  ( 13.41567315973499852, -51.08505356990979607, -21.91538238065540156 ) ) ;
#18818 = DIRECTION ( 'NONE',  ( 1.000000000000000000, 0.000000000000000000, 0.000000000000000000 ) ) ;
#18819 = CARTESIAN_POINT ( 'NONE',  ( 55.36114547021439591, 13.90104188525289963, -14.57735786978359904 ) ) ;
#18820 = CARTESIAN_POINT ( 'NONE',  ( 14.36273205168262912, -9.025304815231496747, -77.86948557558969242 ) ) ;
#18821 = CARTESIAN_POINT ( 'NONE',  ( 71.15040120820690106, 1.386342629514219826, -70.29952392096339508 ) ) ;
#18822 = CARTESIAN_POINT ( 'NONE',  ( 20.15227385440210028, -21.41235416792470048, -41.15422088180869054 ) ) ;
#18823 = DIRECTION ( 'NONE',  ( 0.4743737082415271922, 0.8803235683140504531, 0.000000000000000000 ) ) ;
#18824 = ORIENTED_EDGE ( 'NONE', *, *, #34767, .T. ) ;
#18825 = CIRCLE ( 'NONE', #25512, 1.999999999999999556 ) ;
#18826 = CARTESIAN_POINT ( 'NONE',  ( 47.49699394960070009, 23.15488270540389948, -75.00831418912220272 ) ) ;
#18827 = CARTESIAN_POINT ( 'NONE',  ( 65.08882305123219680, 1.387412027389909985, -61.00994802092580471 ) ) ;
#18828 = CARTESIAN_POINT ( 'NONE',  ( 24.04504587474531263, -15.61618895646369687, -51.50767080737492165 ) ) ;
#18829 = LINE ( 'NONE', #10471, #21236 ) ;
#18830 = DIRECTION ( 'NONE',  ( 0.8059588108975762610, 0.1342272854594990239, 0.5765530599821140356 ) ) ;
#18831 = EDGE_CURVE ( 'NONE', #39738, #38090, #12947, .T. ) ;
#18832 = CARTESIAN_POINT ( 'NONE',  ( 52.13393739769620083, -15.61618894467929941, 6.349999999999999645 ) ) ;
#18834 = ADVANCED_FACE ( 'NONE', ( #16165 ), #33481, .T. ) ;
#18833 = CARTESIAN_POINT ( 'NONE',  ( 82.13853704237929776, 14.40950277491920062, -47.72348187592570667 ) ) ;
#18835 = CARTESIAN_POINT ( 'NONE',  ( -0.1226425999238490022, 19.83525116875770067, -35.35669575663299469 ) ) ;
#18837 = CARTESIAN_POINT ( 'NONE',  ( 47.12472940097700302, -38.11604021042080603, -54.67813498204329647 ) ) ;
#18836 = DIRECTION ( 'NONE',  ( 0.000000000000000000, 0.000000000000000000, 1.000000000000000000 ) ) ;
#18838 = AXIS2_PLACEMENT_3D ( 'NONE', #14010, #26039, #10342 ) ;
#18839 = CARTESIAN_POINT ( 'NONE',  ( 23.72997357701965626, -13.35730697104988174, -71.41570937345944969 ) ) ;
#18840 = DIRECTION ( 'NONE',  ( -0.4156269377774487461, -0.5720614028176871368, -0.7071067811865479058 ) ) ;
#18841 = CARTESIAN_POINT ( 'NONE',  ( -33.86618693412709291, -20.49226357331469828, -57.52971779843680622 ) ) ;
#18842 = ADVANCED_FACE ( 'NONE', ( #47385 ), #35827, .T. ) ;
#18843 = VERTEX_POINT ( 'NONE', #11992 ) ;
#18844 = CARTESIAN_POINT ( 'NONE',  ( 52.68891395819000678, -49.75006725190949197, -48.47378032971909789 ) ) ;
#18845 = ORIENTED_EDGE ( 'NONE', *, *, #23318, .T. ) ;
#18846 = CARTESIAN_POINT ( 'NONE',  ( 46.60861704013112217, 9.031941543785155346, -53.45405854682181968 ) ) ;
#18847 = CARTESIAN_POINT ( 'NONE',  ( 22.72481333191009156, -13.84495503856223309, -42.36948635521349615 ) ) ;
#18848 = CARTESIAN_POINT ( 'NONE',  ( 14.07775902432950055, 19.81371361753149785, -22.00375624323179835 ) ) ;
#18849 = CARTESIAN_POINT ( 'NONE',  ( 13.09383361200632123, 24.26765008030419679, -75.86242720135740569 ) ) ;
#18850 = CARTESIAN_POINT ( 'NONE',  ( 22.73127723598420147, -18.10971370989899754, -46.56784545357869121 ) ) ;
#18851 = CARTESIAN_POINT ( 'NONE',  ( 53.12059652019419786, 18.33618219888390044, -49.12440246944070310 ) ) ;
#18852 = CARTESIAN_POINT ( 'NONE',  ( 14.83834572504270000, -8.683358393905999506, -80.28837282723659996 ) ) ;
#18853 = CARTESIAN_POINT ( 'NONE',  ( 16.13393739769620083, -15.61618894467929941, 17.35000000000000142 ) ) ;
#18854 = EDGE_LOOP ( 'NONE', ( #16216, #36740, #40775, #51868, #14765, #1320 ) ) ;
#18855 = CARTESIAN_POINT ( 'NONE',  ( 22.65693326085800052, -19.97936131720339858, -37.47516227180238957 ) ) ;
#18856 = ORIENTED_EDGE ( 'NONE', *, *, #1662, .T. ) ;
#18857 = CARTESIAN_POINT ( 'NONE',  ( 11.22168587317889887, -65.22927114923599845, -17.68872783567509899 ) ) ;
#18858 = CARTESIAN_POINT ( 'NONE',  ( 9.071903935231079075, 32.31445225605110494, -46.64254262187220235 ) ) ;
#18859 = CARTESIAN_POINT ( 'NONE',  ( 72.98101631171969927, 1.187931651339009909, -62.25809267083580778 ) ) ;
#18860 = CARTESIAN_POINT ( 'NONE',  ( 11.27214654185450726, -21.94226878787483415, -40.50067558586400196 ) ) ;
#18861 = CARTESIAN_POINT ( 'NONE',  ( 52.84346301666477785, -49.69122173838943013, -48.96941052353703583 ) ) ;
#18862 = CARTESIAN_POINT ( 'NONE',  ( 9.367504675961500382, -15.61621390379479912, -67.84717978381009118 ) ) ;
#18863 = AXIS2_PLACEMENT_3D ( 'NONE', #14978, #30944, #39099 ) ;
#18864 = CARTESIAN_POINT ( 'NONE',  ( 50.12109376404330163, -53.47864665676989659, -55.01406006385839476 ) ) ;
#18865 = ORIENTED_EDGE ( 'NONE', *, *, #39305, .T. ) ;
#18866 = EDGE_CURVE ( 'NONE', #14297, #5682, #46259, .T. ) ;
#18867 = DIRECTION ( 'NONE',  ( 1.000000000000000000, 0.000000000000000000, 0.000000000000000000 ) ) ;
#18868 = ORIENTED_EDGE ( 'NONE', *, *, #17692, .F. ) ;
#18869 = CONICAL_SURFACE ( 'NONE', #44801, 9.750000000000000000, 0.7853981633974476129 ) ;
#18870 = CARTESIAN_POINT ( 'NONE',  ( 9.736686533375289443, -63.21034557680579979, -46.29811293505660075 ) ) ;
#18871 = FACE_OUTER_BOUND ( 'NONE', #29741, .T. ) ;
#18872 = VERTEX_POINT ( 'NONE', #40279 ) ;
#18873 = CARTESIAN_POINT ( 'NONE',  ( 23.60377752213949876, -48.79579064807929711, -34.96018206680719942 ) ) ;
#18874 = CARTESIAN_POINT ( 'NONE',  ( 57.18371624250119822, 19.38400875315999983, -53.90359198974339705 ) ) ;
#18875 = CARTESIAN_POINT ( 'NONE',  ( 52.93656362771660184, 19.08184182246549909, -77.15175517737969813 ) ) ;
#18876 = ORIENTED_EDGE ( 'NONE', *, *, #16683, .F. ) ;
#18877 = CYLINDRICAL_SURFACE ( 'NONE', #4841, 2.000000000000003553 ) ;
#18878 = CARTESIAN_POINT ( 'NONE',  ( 7.517033938252880354, 30.35161808146150264, -19.14999999999999858 ) ) ;
#18879 = CARTESIAN_POINT ( 'NONE',  ( 14.79003424252982057, 21.13935400224803018, -76.01806011803036256 ) ) ;
#18880 = CARTESIAN_POINT ( 'NONE',  ( 57.36123081458359962, -50.13537923174280309, -52.61896056486340001 ) ) ;
#18881 = B_SPLINE_SURFACE_WITH_KNOTS ( 'NONE', 3, 3, ( 
 ( #38964, #43661, #3831, #46838, #27149, #19028, #31578, #27403, #15108, #47348 ),
 ( #43404, #11183, #7248, #22947, #18772, #43154, #39727, #35538, #35003, #34744 ),
 ( #11698, #31068, #27661, #7505, #38710, #50753, #6993, #39477, #2801, #23196 ),
 ( #51271, #39213, #23452, #3577, #19291, #42898, #23714, #14847, #30810, #3057 ),
 ( #10924, #26889, #35272, #15369, #31323, #1940, #17920, #26808, #30479, #38888 ),
 ( #33636, #42297, #2202, #22094, #46240, #2976, #13996, #13744, #2453, #49653 ),
 ( #14509, #42820, #18433, #18178, #34407, #6916, #33891, #42561, #49902, #29955 ),
 ( #10590, #45971, #38105, #29697, #5871, #10328, #42036, #37845, #26289, #10064 ),
 ( #38628, #26024, #34144, #34668, #6137, #50156, #22867, #45709, #21838, #14252 ),
 ( #50672, #50421, #30221, #46499, #6397, #26545, #22356, #38359, #6652, #9810 ) ),
 .UNSPECIFIED., .F., .F., .F.,
 ( 4, 1, 1, 1, 1, 1, 1, 4 ),
 ( 4, 2, 2, 2, 4 ),
 ( -7.647483580428189077E-05, 0.1428571428571430157, 0.2857142857142860315, 0.4285714285714289917, 0.5714285714285709528, 0.7142857142857139685, 0.8571428571428569843, 1.000068219203180009 ),
 ( -0.8959923838512789951, -0.7377509475120830329, -0.4200977637871100012, -0.1578379958887219936, 7.344577026599998924E-05 ),
 .UNSPECIFIED. ) ;
#18882 = CARTESIAN_POINT ( 'NONE',  ( 19.68986098307310328, -8.177228835168328658, -61.43426723409519496 ) ) ;
#18883 = LINE ( 'NONE', #50356, #10466 ) ;
#18884 = COLOUR_RGB ( '', 0.66274510, 0.83137255, 0.94901961) ;
#18885 = CARTESIAN_POINT ( 'NONE',  ( 68.13393739769620083, 0.8838110553206759423, -65.65000000000000568 ) ) ;
#18886 = ORIENTED_EDGE ( 'NONE', *, *, #25566, .F. ) ;
#18887 = VERTEX_POINT ( 'NONE', #20339 ) ;
#18888 = DIRECTION ( 'NONE',  ( 0.000000000000000000, 0.000000000000000000, -1.000000000000000000 ) ) ;
#18889 = CARTESIAN_POINT ( 'NONE',  ( 10.18556923319409968, -11.13025426117309991, -57.43833289983439272 ) ) ;
#18890 = CARTESIAN_POINT ( 'NONE',  ( 8.867200650584759813, -15.35517633189170006, -32.14999999999999858 ) ) ;
#18891 = VECTOR ( 'NONE', #16135, 1000.000000000000000 ) ;
#18892 = CARTESIAN_POINT ( 'NONE',  ( 59.13393739769620083, -15.61618894467929941, -15.65000000000000036 ) ) ;
#18893 = CARTESIAN_POINT ( 'NONE',  ( 69.63393739769620083, 6.883811055320649963, -71.50000000000000000 ) ) ;
#18894 = FACE_OUTER_BOUND ( 'NONE', #28624, .T. ) ;
#18895 = CARTESIAN_POINT ( 'NONE',  ( 11.88460916116889976, 33.59273172673110963, -16.16716782997540136 ) ) ;
#18896 = CARTESIAN_POINT ( 'NONE',  ( 15.56510543608290043, -7.390670668702870039, -60.98569090715739804 ) ) ;
#18897 = CARTESIAN_POINT ( 'NONE',  ( 53.55220836886790181, -48.78100643530040514, -26.47327747818699706 ) ) ;
#18898 = AXIS2_PLACEMENT_3D ( 'NONE', #24811, #36889, #36615 ) ;
#18899 = EDGE_CURVE ( 'NONE', #46602, #23939, #36326, .T. ) ;
#18900 = CARTESIAN_POINT ( 'NONE',  ( 55.36944056199379816, -50.82556113491280314, -75.41474324147199582 ) ) ;
#18902 = CARTESIAN_POINT ( 'NONE',  ( 44.13393739769620083, -36.11618894467930119, -35.14999999999999858 ) ) ;
#18901 = CARTESIAN_POINT ( 'NONE',  ( -6.745630838839370647, 14.94319942760500020, -5.463640701264131039 ) ) ;
#18903 = CARTESIAN_POINT ( 'NONE',  ( 47.25382592556910311, -54.75228172359690149, -54.62311712267080566 ) ) ;
#18904 = FACE_OUTER_BOUND ( 'NONE', #9677, .T. ) ;
#18905 = EDGE_CURVE ( 'NONE', #2493, #37502, #46502, .T. ) ;
#18906 = ORIENTED_EDGE ( 'NONE', *, *, #44650, .F. ) ;
#18907 = CARTESIAN_POINT ( 'NONE',  ( -11.32734370190460105, -41.88171845330919751, -6.430192534648670133 ) ) ;
#18908 = CARTESIAN_POINT ( 'NONE',  ( 47.65564868057830239, 23.28640233928300063, -54.93645362307179880 ) ) ;
#18909 = DIRECTION ( 'NONE',  ( 0.000000000000000000, 1.000000000000000000, 0.000000000000000000 ) ) ;
#18910 = CARTESIAN_POINT ( 'NONE',  ( 16.46706851333994592, -51.11618894468167440, -15.67516967139586548 ) ) ;
#18911 = CARTESIAN_POINT ( 'NONE',  ( 13.51940423530409952, 19.36859641292999967, -21.33263318241190021 ) ) ;
#18912 = CARTESIAN_POINT ( 'NONE',  ( 60.99063469145590233, 14.41619031400530027, -47.70729047236519449 ) ) ;
#18913 = CARTESIAN_POINT ( 'NONE',  ( 11.22384627824540004, 33.78040140241470368, -16.94931753701080268 ) ) ;
#18914 = CARTESIAN_POINT ( 'NONE',  ( 51.86328208370509429, 18.67428979098259845, -76.68384257635129586 ) ) ;
#18915 = CARTESIAN_POINT ( 'NONE',  ( 52.79481764036179925, 18.44745459499829821, -48.50058864900179856 ) ) ;
#18916 = CARTESIAN_POINT ( 'NONE',  ( 0.1457840807894888180, 19.59951024407514097, -34.68167773519660813 ) ) ;
#18917 = DIRECTION ( 'NONE',  ( -0.9151634328774630456, 0.3898247278254499681, -0.1025308377989340020 ) ) ;
#18918 = CARTESIAN_POINT ( 'NONE',  ( 53.04703063237690230, 18.20237249300480187, -27.50709361416090104 ) ) ;
#18919 = CARTESIAN_POINT ( 'NONE',  ( 12.93740664656254680, 18.01819160635294992, -34.64999999999999858 ) ) ;
#18920 = DIRECTION ( 'NONE',  ( 0.000000000000000000, -1.000000000000000000, 0.000000000000000000 ) ) ;
#18921 = CARTESIAN_POINT ( 'NONE',  ( 52.66149042093859123, 18.55528232251300125, -48.73886901161859697 ) ) ;
#18922 = LINE ( 'NONE', #37822, #21550 ) ;
#18923 = CARTESIAN_POINT ( 'NONE',  ( 71.19443613848248731, 1.370118064600899910, -60.90754237392700077 ) ) ;
#18924 = CARTESIAN_POINT ( 'NONE',  ( 11.13393739769619906, 32.11747391597780421, -43.91739627612010111 ) ) ;
#18925 = CARTESIAN_POINT ( 'NONE',  ( 73.01685589897030582, 0.9479899806831150189, -62.16329186921600325 ) ) ;
#18926 = VECTOR ( 'NONE', #9683, 1000.000000000000000 ) ;
#18927 = CARTESIAN_POINT ( 'NONE',  ( 65.95897347940848476, -32.09849744266369953, -17.73193878851440175 ) ) ;
#18928 = ADVANCED_FACE ( 'NONE', ( #25036 ), #48665, .F. ) ;
#18929 = AXIS2_PLACEMENT_3D ( 'NONE', #30894, #26705, #2105 ) ;
#18930 = CARTESIAN_POINT ( 'NONE',  ( 10.04828159318836001, -12.59815513276911858, -65.59931143651195384 ) ) ;
#18931 = ORIENTED_EDGE ( 'NONE', *, *, #35386, .T. ) ;
#18932 = ORIENTED_EDGE ( 'NONE', *, *, #41775, .F. ) ;
#18933 = CARTESIAN_POINT ( 'NONE',  ( 42.93197233849409855, 11.32569894967160096, -3.187564294433600232 ) ) ;
#18934 = ADVANCED_FACE ( 'NONE', ( #44466 ), #36589, .T. ) ;
#18935 = CARTESIAN_POINT ( 'NONE',  ( 51.06529787577495227, 0.2493625510273632662, -16.95223896232651484 ) ) ;
#18936 = ORIENTED_EDGE ( 'NONE', *, *, #21437, .F. ) ;
#18937 = CARTESIAN_POINT ( 'NONE',  ( 11.42316304585989961, -64.61387295428639277, -45.17482744339589829 ) ) ;
#18938 = CARTESIAN_POINT ( 'NONE',  ( 56.13881711988070577, -45.75862301436319513, -25.71798066937759941 ) ) ;
#18939 = CARTESIAN_POINT ( 'NONE',  ( 9.221374816805001373, -19.60025404329541487, -78.34097178294052810 ) ) ;
#18940 = FACE_OUTER_BOUND ( 'NONE', #8946, .T. ) ;
#18941 = DIRECTION ( 'NONE',  ( 0.000000000000000000, -1.000000000000000000, 0.000000000000000000 ) ) ;
#18942 = ORIENTED_EDGE ( 'NONE', *, *, #6699, .T. ) ;
#18943 = CARTESIAN_POINT ( 'NONE',  ( 11.69795627133467697, 34.16744399712961666, -22.44873498087175179 ) ) ;
#18944 = CARTESIAN_POINT ( 'NONE',  ( 43.26664544300862048, 6.584138943362735752, -73.98639579103669917 ) ) ;
#18945 = CIRCLE ( 'NONE', #26486, 19.56371635397779940 ) ;
#18946 = CARTESIAN_POINT ( 'NONE',  ( 11.82668577431979884, 33.14159547282380203, -24.59829236961180143 ) ) ;
#18947 = ORIENTED_EDGE ( 'NONE', *, *, #31026, .F. ) ;
#18948 = CARTESIAN_POINT ( 'NONE',  ( 20.31028818469260244, -22.72544855982049938, -32.12326274055609332 ) ) ;
#18949 = VECTOR ( 'NONE', #43294, 1000.000000000000000 ) ;
#18950 = DIRECTION ( 'NONE',  ( 0.000000000000000000, 0.000000000000000000, -1.000000000000000000 ) ) ;
#18951 = DIRECTION ( 'NONE',  ( -1.000000000000000000, 0.000000000000000000, 0.000000000000000000 ) ) ;
#18952 = CARTESIAN_POINT ( 'NONE',  ( 11.79147378256356937, -20.83640137970460771, -51.17359023759287595 ) ) ;
#18953 = CARTESIAN_POINT ( 'NONE',  ( 61.47160170490100484, -29.95828558899940219, -16.07879158819200072 ) ) ;
#18954 = CARTESIAN_POINT ( 'NONE',  ( 36.13393739769620083, -15.61618894467929941, -15.18999999999999950 ) ) ;
#18955 = CARTESIAN_POINT ( 'NONE',  ( 47.24443041864720527, -54.45681227993460283, -75.11586948118589646 ) ) ;
#18956 = CARTESIAN_POINT ( 'NONE',  ( 43.44710262568360548, 12.61051141539170040, -5.048133889203059610 ) ) ;
#18957 = PLANE ( 'NONE',  #30930 ) ;
#18958 = AXIS2_PLACEMENT_3D ( 'NONE', #24418, #19484, #35477 ) ;
#18959 = DIRECTION ( 'NONE',  ( 0.000000000000000000, 0.000000000000000000, 1.000000000000000000 ) ) ;
#18960 = CARTESIAN_POINT ( 'NONE',  ( 18.64396758981110125, -22.71517679829500125, -81.67932580530198550 ) ) ;
#18961 = ORIENTED_EDGE ( 'NONE', *, *, #11553, .T. ) ;
#18962 = EDGE_CURVE ( 'NONE', #45208, #16752, #24785, .T. ) ;
#18963 = CARTESIAN_POINT ( 'NONE',  ( 4.835529188070480267, -58.78041738421249818, -12.99353756526149972 ) ) ;
#18964 = CARTESIAN_POINT ( 'NONE',  ( 75.04668702423900584, -18.75119728547959852, -11.30405884009489981 ) ) ;
#18965 = CARTESIAN_POINT ( 'NONE',  ( 75.41376673900958849, 12.86054230907423879, -13.63390496164747567 ) ) ;
#18966 = CARTESIAN_POINT ( 'NONE',  ( 19.53780474230963193, -55.47109714356856358, -75.55954122747178303 ) ) ;
#18967 = CARTESIAN_POINT ( 'NONE',  ( 14.84957949698884683, -16.54932958072287263, -11.23251175440650051 ) ) ;
#18968 = CARTESIAN_POINT ( 'NONE',  ( 47.18324198357279897, 23.57489020266570279, -54.61058319554400242 ) ) ;
#18969 = CARTESIAN_POINT ( 'NONE',  ( 82.34851808037059584, -45.64188066427789892, -47.72348187592570667 ) ) ;
#18970 = CARTESIAN_POINT ( 'NONE',  ( 12.94455701826820082, 19.08483511945829747, -21.18967814235449865 ) ) ;
#18971 = CARTESIAN_POINT ( 'NONE',  ( 57.48892408827569511, -50.38497325094370183, -52.98966502147489877 ) ) ;
#18972 = CARTESIAN_POINT ( 'NONE',  ( 41.57697698334229841, 12.60893760990930090, -3.558127426236100010 ) ) ;
#18973 = CARTESIAN_POINT ( 'NONE',  ( 67.78236843376265597, -30.11618894467929763, -17.74895402404430911 ) ) ;
#18974 = LINE ( 'NONE', #34955, #19911 ) ;
#18975 = DIRECTION ( 'NONE',  ( 0.000000000000000000, 0.000000000000000000, -1.000000000000000000 ) ) ;
#18976 = CIRCLE ( 'NONE', #12292, 17.39999999999999503 ) ;
#18977 = CARTESIAN_POINT ( 'NONE',  ( 30.13393739769619728, -38.61618894467930119, -72.14999999999999147 ) ) ;
#18978 = DIRECTION ( 'NONE',  ( 0.000000000000000000, -1.000000000000000000, 0.000000000000000000 ) ) ;
#18980 = CARTESIAN_POINT ( 'NONE',  ( 17.92442291492480066, -51.57142019855179882, -75.41551559479479749 ) ) ;
#18979 = B_SPLINE_CURVE_WITH_KNOTS ( 'NONE', 3,
 ( #40880, #13632, #21468, #29590, #32998, #33263, #9691, #25651, #41656, #5759, #21721, #20952, #37729, #1051, #32460, #48489, #12593, #28554, #44556, #21206, #36948, #9182, #12860, #29338, #8654 ),
 .UNSPECIFIED., .F., .F.,
 ( 4, 2, 2, 1, 1, 2, 2, 2, 2, 1, 1, 1, 2, 2, 4 ),
 ( 0.000000000000000000, 0.1250000000000096312, 0.1875000000000144329, 0.2187500000000176803, 0.2343750000000193179, 0.2421875000000198452, 0.2500000000000204281, 0.5000000000000174305, 0.6250000000000159872, 0.6875000000000153211, 0.7187500000000150990, 0.7343750000000154321, 0.7421875000000155431, 0.7500000000000156541, 1.000000000000000000 ),
 .UNSPECIFIED. ) ;
#18981 = CARTESIAN_POINT ( 'NONE',  ( 42.99567057238449763, -45.11618894467940066, -6.881716687611570293 ) ) ;
#18982 = CARTESIAN_POINT ( 'NONE',  ( 10.72664991973389981, -10.49096344046840024, -68.30882034609030029 ) ) ;
#18983 = CARTESIAN_POINT ( 'NONE',  ( 63.51813308628860710, 1.318402576461300102, -62.06494149197789767 ) ) ;
#18984 = ORIENTED_EDGE ( 'NONE', *, *, #30459, .F. ) ;
#18985 = CARTESIAN_POINT ( 'NONE',  ( 22.90103018812914115, -15.61618888866172483, -50.84718209631233066 ) ) ;
#18986 = CARTESIAN_POINT ( 'NONE',  ( 46.68434392863400717, 22.61662994292931117, 11.34999999999999964 ) ) ;
#18987 = CARTESIAN_POINT ( 'NONE',  ( 72.95819590288708412, 1.328674444234379859, -68.76626720283900340 ) ) ;
#18988 = CARTESIAN_POINT ( 'NONE',  ( 45.35172597471413525, 8.821878553838054415, -60.10595750932078118 ) ) ;
#18989 = CARTESIAN_POINT ( 'NONE',  ( 19.16157989668684891, 18.33238584480854527, -34.89146800830132378 ) ) ;
#18990 = CARTESIAN_POINT ( 'NONE',  ( 42.22416898896209858, -45.44812850840609997, -6.646931848296280698 ) ) ;
#18991 = ORIENTED_EDGE ( 'NONE', *, *, #7236, .T. ) ;
#18992 = CARTESIAN_POINT ( 'NONE',  ( 17.30738868478190184, 21.72103359751309881, -76.14999999999999147 ) ) ;
#18993 = VERTEX_POINT ( 'NONE', #41055 ) ;
#18994 = ORIENTED_EDGE ( 'NONE', *, *, #12133, .F. ) ;
#18995 = AXIS2_PLACEMENT_3D ( 'NONE', #27016, #22556, #43023 ) ;
#18996 = ADVANCED_FACE ( 'NONE', ( #29241 ), #17803, .T. ) ;
#18997 = ORIENTED_EDGE ( 'NONE', *, *, #26844, .F. ) ;
#18998 = CARTESIAN_POINT ( 'NONE',  ( 8.815605938724019097, -63.28267558148569094, -46.67186391142220003 ) ) ;
#18999 = CARTESIAN_POINT ( 'NONE',  ( 23.15496243216929884, -12.51723427498050079, -81.23899999999999011 ) ) ;
#19000 = DIRECTION ( 'NONE',  ( -0.9304380493636940086, -0.3664492274467011645, 0.000000000000000000 ) ) ;
#19001 = CARTESIAN_POINT ( 'NONE',  ( -13.34911547993528025, -41.36128161159584238, -46.70844658446259956 ) ) ;
#19002 = CIRCLE ( 'NONE', #25683, 2.000000000000001776 ) ;
#19003 = VERTEX_POINT ( 'NONE', #5167 ) ;
#19004 = CARTESIAN_POINT ( 'NONE',  ( 14.06324288281645352, -7.911092913131379412, -52.92433643171475666 ) ) ;
#19005 = ORIENTED_EDGE ( 'NONE', *, *, #5966, .T. ) ;
#19006 = DIRECTION ( 'NONE',  ( 0.000000000000000000, 0.000000000000000000, 1.000000000000000000 ) ) ;
#19007 = B_SPLINE_CURVE_WITH_KNOTS ( 'NONE', 3,
 ( #21018, #4522, #28359, #44363, #37017, #8726 ),
 .UNSPECIFIED., .F., .F.,
 ( 4, 1, 1, 4 ),
 ( 0.000000000000000000, 0.3333333333333329263, 0.6666666666666669627, 1.000000000000000000 ),
 .UNSPECIFIED. ) ;
#19008 = CARTESIAN_POINT ( 'NONE',  ( 45.15332781221579239, -33.30556177572260168, -35.04110570142709946 ) ) ;
#19009 = ORIENTED_EDGE ( 'NONE', *, *, #22944, .F. ) ;
#19010 = CARTESIAN_POINT ( 'NONE',  ( 41.61626771661330082, 4.883811055320659733, -82.23834840541459812 ) ) ;
#19011 = CARTESIAN_POINT ( 'NONE',  ( 51.61430885013370329, -51.17530555596519548, -76.09751502629850961 ) ) ;
#19012 = CARTESIAN_POINT ( 'NONE',  ( 60.53709663307620303, 14.40413707899699958, -47.33107028358159596 ) ) ;
#19013 = AXIS2_PLACEMENT_3D ( 'NONE', #32797, #36230, #32024 ) ;
#19014 = CARTESIAN_POINT ( 'NONE',  ( 22.90046023677898646, -15.52937730499472657, -40.44874214335946760 ) ) ;
#19015 = LINE ( 'NONE', #7753, #46827 ) ;
#19016 = CARTESIAN_POINT ( 'NONE',  ( 65.05986622648850926, 0.9377769643968115743, -17.72011801484886107 ) ) ;
#19017 = CARTESIAN_POINT ( 'NONE',  ( -3.812186623206120117, 16.87714592095479915, -5.022395698517160056 ) ) ;
#19018 = CARTESIAN_POINT ( 'NONE',  ( 1.055648624549950121, -22.58715886189619937, -34.65000333055159842 ) ) ;
#19019 = CYLINDRICAL_SURFACE ( 'NONE', #2990, 31.00000000000000000 ) ;
#19020 = CARTESIAN_POINT ( 'NONE',  ( 11.03937652346400000, -21.58546006282470131, -56.01239214068929329 ) ) ;
#19021 = ORIENTED_EDGE ( 'NONE', *, *, #39841, .F. ) ;
#19022 = FACE_OUTER_BOUND ( 'NONE', #4313, .T. ) ;
#19023 = EDGE_CURVE ( 'NONE', #32963, #1782, #16115, .T. ) ;
#19024 = CARTESIAN_POINT ( 'NONE',  ( 57.39562476827909876, 19.32839297046770000, -53.44831944760920095 ) ) ;
#19025 = CARTESIAN_POINT ( 'NONE',  ( 71.69973440771281048, 1.034647430439950000, -70.46565918721690025 ) ) ;
#19026 = CARTESIAN_POINT ( 'NONE',  ( 45.49125530861236655, -40.06305810151475555, -59.42936724080989563 ) ) ;
#19027 = EDGE_CURVE ( 'NONE', #46513, #18727, #24506, .T. ) ;
#19028 = CARTESIAN_POINT ( 'NONE',  ( 15.41374403315509944, 19.54065027890899842, -20.47798662115040003 ) ) ;
#19029 = ADVANCED_FACE ( 'NONE', ( #37125 ), #17466, .T. ) ;
#19030 = DIRECTION ( 'NONE',  ( 0.000000000000000000, 0.000000000000000000, 1.000000000000000000 ) ) ;
#19031 = CARTESIAN_POINT ( 'NONE',  ( 11.25287529172470080, -20.70714090792739981, -45.59048102137129632 ) ) ;
#19032 = EDGE_CURVE ( 'NONE', #19145, #16544, #11746, .T. ) ;
#19033 = CARTESIAN_POINT ( 'NONE',  ( -2.751565836256447906, -9.953069984054630837, -84.65000000000000568 ) ) ;
#19034 = CARTESIAN_POINT ( 'NONE',  ( 48.20452265730919805, -54.29503287064169825, -55.30665343754630214 ) ) ;
#19035 = DIRECTION ( 'NONE',  ( -0.2201791028874051093, -0.9741803703649114521, 0.04993764759559501942 ) ) ;
#19036 = CARTESIAN_POINT ( 'NONE',  ( 56.40078553072510203, 19.31196876521530115, -52.89577359589869587 ) ) ;
#19037 = CARTESIAN_POINT ( 'NONE',  ( 12.14367607025980789, 22.37708546437701429, -21.73578643762689211 ) ) ;
#19038 = ORIENTED_EDGE ( 'NONE', *, *, #22802, .F. ) ;
#19039 = CARTESIAN_POINT ( 'NONE',  ( 21.51824785155720221, -11.06077896193409948, -70.62366323747509966 ) ) ;
#19040 = VERTEX_POINT ( 'NONE', #43354 ) ;
#19041 = CARTESIAN_POINT ( 'NONE',  ( 71.38053669821270830, 1.187415670095769871, -70.58414947367050729 ) ) ;
#19042 = CARTESIAN_POINT ( 'NONE',  ( 20.11811090880234332, -22.52868689541044489, -57.84100116256885116 ) ) ;
#19043 = CARTESIAN_POINT ( 'NONE',  ( 47.93639096317219384, -54.33238953986003139, -54.72300757058784626 ) ) ;
#19044 = CARTESIAN_POINT ( 'NONE',  ( 83.62685937867283315, 13.30364075603329255, -46.55427984015698684 ) ) ;
#19045 = EDGE_CURVE ( 'NONE', #23591, #50655, #37933, .T. ) ;
#19047 = LINE ( 'NONE', #3594, #44876 ) ;
#19046 = CARTESIAN_POINT ( 'NONE',  ( 82.75388200178990417, 14.36257604166400093, -47.67228907607350408 ) ) ;
#19048 = CARTESIAN_POINT ( 'NONE',  ( 22.16258581960079965, -19.27651095769689604, -79.02086993021860906 ) ) ;
#19049 = CARTESIAN_POINT ( 'NONE',  ( 71.58179376171669617, 0.9036513197889539661, -70.56049771322810216 ) ) ;
#19050 = CARTESIAN_POINT ( 'NONE',  ( 24.04493741561075737, -14.58064863577438075, -67.46599913618511835 ) ) ;
#19051 = ORIENTED_EDGE ( 'NONE', *, *, #19285, .F. ) ;
#19052 = CARTESIAN_POINT ( 'NONE',  ( 0.09524056481075650338, 19.92956581399739946, -35.08026080309999628 ) ) ;
#19053 = ORIENTED_EDGE ( 'NONE', *, *, #4549, .T. ) ;
#19054 = VECTOR ( 'NONE', #12160, 1000.000000000000000 ) ;
#19055 = EDGE_CURVE ( 'NONE', #22521, #11543, #39932, .T. ) ;
#19056 = EDGE_LOOP ( 'NONE', ( #20184, #18537, #294, #33667 ) ) ;
#19057 = DIRECTION ( 'NONE',  ( -1.000000000000000000, 0.000000000000000000, 0.000000000000000000 ) ) ;
#19058 = CARTESIAN_POINT ( 'NONE',  ( 22.46008698234219381, -10.75448952574305395, -39.58399611284257702 ) ) ;
#19059 = CARTESIAN_POINT ( 'NONE',  ( 18.11497263573659922, 5.664030231104960400, -35.14999999999999858 ) ) ;
#19060 = CARTESIAN_POINT ( 'NONE',  ( 12.26489985407230066, -65.41013428201999602, -47.36052460643420403 ) ) ;
#19061 = ORIENTED_EDGE ( 'NONE', *, *, #10372, .F. ) ;
#19062 = ORIENTED_EDGE ( 'NONE', *, *, #31618, .T. ) ;
#19063 = CARTESIAN_POINT ( 'NONE',  ( 65.03603135454920903, 1.015437840524759938, -17.83403478221330118 ) ) ;
#19064 = CARTESIAN_POINT ( 'NONE',  ( 56.61099403853209822, 14.92704628377260079, -26.25969108334859925 ) ) ;
#19065 = CARTESIAN_POINT ( 'NONE',  ( 2.277530937145189949, -15.61618894467929941, -32.14999999999999858 ) ) ;
#19066 = DIRECTION ( 'NONE',  ( -1.000000000000000000, 0.000000000000000000, 0.000000000000000000 ) ) ;
#19067 = CARTESIAN_POINT ( 'NONE',  ( 59.58714391122960308, -1.728360499025269892, -15.83152262783869801 ) ) ;
#19068 = CARTESIAN_POINT ( 'NONE',  ( 51.43375901386550453, -49.25898423961760386, -76.62099598227180763 ) ) ;
#19069 = DIRECTION ( 'NONE',  ( 0.000000000000000000, 0.000000000000000000, 1.000000000000000000 ) ) ;
#19070 = SHAPE_REPRESENTATION ( 'Height Adjustment Lead Screw', ( #20940 ), #10115 ) ;
#19071 = ORIENTED_EDGE ( 'NONE', *, *, #48674, .T. ) ;
#19072 = CARTESIAN_POINT ( 'NONE',  ( 63.19468704395289649, 0.8986939045430389905, -69.05651959838648679 ) ) ;
#19073 = CARTESIAN_POINT ( 'NONE',  ( 17.16957635348524747, -23.52717588353839773, -48.25066592410423283 ) ) ;
#19074 = CARTESIAN_POINT ( 'NONE',  ( 68.13393739769620083, 1.883811055320649963, -65.65000000000000568 ) ) ;
#19075 = CARTESIAN_POINT ( 'NONE',  ( 17.16954899286013614, -23.52717978940560073, -53.96600348036692907 ) ) ;
#19076 = ADVANCED_FACE ( 'NONE', ( #47798 ), #6146, .T. ) ;
#19077 = CARTESIAN_POINT ( 'NONE',  ( 8.294557586283641371, -15.97795097143059984, -38.99781585255099259 ) ) ;
#19078 = CARTESIAN_POINT ( 'NONE',  ( 13.21399250059920050, -50.88310479779730144, -21.61005667689260079 ) ) ;
#19079 = CARTESIAN_POINT ( 'NONE',  ( -7.616062602303800055, -62.82329572586585442, 17.05710678118654755 ) ) ;
#19080 = CARTESIAN_POINT ( 'NONE',  ( 56.48652151861699622, 13.88381105532070059, -15.35311052695679912 ) ) ;
#19081 = DIRECTION ( 'NONE',  ( -0.5516667872527333261, 0.8340645993220474619, 0.000000000000000000 ) ) ;
#19082 = DIRECTION ( 'NONE',  ( 1.000000000000000000, 0.000000000000000000, 0.000000000000000000 ) ) ;
#19083 = VECTOR ( 'NONE', #30108, 999.9999999999998863 ) ;
#19084 = CARTESIAN_POINT ( 'NONE',  ( 11.59299064767419907, -21.01270279974499999, -39.56984226053629783 ) ) ;
#19085 = CARTESIAN_POINT ( 'NONE',  ( 46.89353120241150208, -39.59222692223529805, -54.28157613336880161 ) ) ;
#19086 = ORIENTED_EDGE ( 'NONE', *, *, #2134, .F. ) ;
#19087 = CARTESIAN_POINT ( 'NONE',  ( 13.60549529218709885, -51.43164378700710415, -74.36773579016251290 ) ) ;
#19088 = CARTESIAN_POINT ( 'NONE',  ( 64.81454860220658531, 1.096305581841150012, -60.69897858480909747 ) ) ;
#19089 = DIRECTION ( 'NONE',  ( -6.940534999999999567E-13, 3.000959000000000097E-13, -1.000000000000000000 ) ) ;
#19090 = ADVANCED_FACE ( 'NONE', ( #36492 ), #36238, .T. ) ;
#19091 = CARTESIAN_POINT ( 'NONE',  ( 54.63655381128389621, -48.05296878824569973, -26.73577887340519865 ) ) ;
#19092 = EDGE_CURVE ( 'NONE', #24575, #46028, #597, .T. ) ;
#19093 = CARTESIAN_POINT ( 'NONE',  ( 8.731180243531696306, -48.92556967366426335, -34.79644561402096770 ) ) ;
#19094 = CARTESIAN_POINT ( 'NONE',  ( 8.784728771152170879, 23.70287936274029761, -46.67204636145419983 ) ) ;
#19095 = EDGE_CURVE ( 'NONE', #17698, #30160, #37344, .T. ) ;
#19096 = CARTESIAN_POINT ( 'NONE',  ( 82.25807928850851169, 13.89010898168029939, -46.55740818416200000 ) ) ;
#19097 = CARTESIAN_POINT ( 'NONE',  ( 72.71656993463119534, 0.9860880133275228276, -69.52393415259180642 ) ) ;
#19099 = CARTESIAN_POINT ( 'NONE',  ( 9.366937397696199596, -15.61618894467949836, -28.45282021618999835 ) ) ;
#19098 = CARTESIAN_POINT ( 'NONE',  ( 47.57073483231042133, 23.21246685024514633, -74.81156575745629311 ) ) ;
#19100 = CARTESIAN_POINT ( 'NONE',  ( 23.25180567546468779, -12.03939683248547787, -71.35930991703870063 ) ) ;
#19101 = CARTESIAN_POINT ( 'NONE',  ( 49.66352655669150096, 22.42445118933569859, -54.86856413023149770 ) ) ;
#19102 = VERTEX_POINT ( 'NONE', #32032 ) ;
#19103 = CARTESIAN_POINT ( 'NONE',  ( 52.73806811560410068, -49.71908181329310139, -48.65317700872209628 ) ) ;
#19104 = B_SPLINE_CURVE_WITH_KNOTS ( 'NONE', 3,
 ( #32711, #3946, #36398, #8129, #44537, #16240, #35899, #13 ),
 .UNSPECIFIED., .F., .F.,
 ( 4, 2, 2, 4 ),
 ( -0.1350635247397186933, -0.1243669311588919968, -0.1075965482636490056, -0.1052074838081890062 ),
 .UNSPECIFIED. ) ;
#19105 = ORIENTED_EDGE ( 'NONE', *, *, #3724, .T. ) ;
#19106 = CARTESIAN_POINT ( 'NONE',  ( 42.77403168035458236, 6.335355339735892599, -76.42259866880976915 ) ) ;
#19107 = CARTESIAN_POINT ( 'NONE',  ( 9.452223072063393516, -13.93305368010741851, -39.92635120517288527 ) ) ;
#19108 = CARTESIAN_POINT ( 'NONE',  ( 13.79101907244350045, 20.01225008817899820, -22.61438297437780065 ) ) ;
#19109 = CARTESIAN_POINT ( 'NONE',  ( 52.08784026747549945, -49.61362475023040020, -77.13961137824819048 ) ) ;
#19110 = CARTESIAN_POINT ( 'NONE',  ( 9.475322139430359059, -13.29123700130180019, -59.55975014801229861 ) ) ;
#19111 = CARTESIAN_POINT ( 'NONE',  ( 52.85422457117920203, 18.44426668863140151, -48.94261452190229988 ) ) ;
#19112 = CARTESIAN_POINT ( 'NONE',  ( 21.10095754687662861, -10.66581710795787785, -80.59744018890606299 ) ) ;
#19113 = DIRECTION ( 'NONE',  ( 0.000000000000000000, -1.000000000000000000, 0.000000000000000000 ) ) ;
#19114 = ORIENTED_EDGE ( 'NONE', *, *, #36735, .T. ) ;
#19115 = CARTESIAN_POINT ( 'NONE',  ( 21.70740924569160057, -10.09141683809470003, -33.03890213223969141 ) ) ;
#19116 = EDGE_CURVE ( 'NONE', #17025, #6777, #27605, .T. ) ;
#19117 = ORIENTED_EDGE ( 'NONE', *, *, #6498, .T. ) ;
#19118 = CARTESIAN_POINT ( 'NONE',  ( 55.16626882053050451, 17.34692063200439804, -48.76159087390789892 ) ) ;
#19119 = CARTESIAN_POINT ( 'NONE',  ( 10.79909669237359893, 33.81695037855629948, -47.18321592309199985 ) ) ;
#19120 = CARTESIAN_POINT ( 'NONE',  ( 73.04666255914109740, 0.9369374701296400154, -62.20531809130540069 ) ) ;
#19121 = CARTESIAN_POINT ( 'NONE',  ( 9.221330038119877059, -19.60017639455499250, -40.62567196025226934 ) ) ;
#19122 = CARTESIAN_POINT ( 'NONE',  ( 53.36461353568414268, -49.48324289032532164, -49.20419813977648005 ) ) ;
#19123 = DIRECTION ( 'NONE',  ( 0.000000000000000000, 1.000000000000000000, 0.000000000000000000 ) ) ;
#19124 = AXIS2_PLACEMENT_3D ( 'NONE', #14885, #9920, #25883 ) ;
#19125 = CARTESIAN_POINT ( 'NONE',  ( 52.59140206479120394, -52.14549427466430842, -53.43195377655929690 ) ) ;
#19126 = CIRCLE ( 'NONE', #48420, 5.500000000000005329 ) ;
#19127 = VERTEX_POINT ( 'NONE', #39672 ) ;
#19128 = CARTESIAN_POINT ( 'NONE',  ( 63.88393739769619373, -15.61618894467929941, -61.44999999999999574 ) ) ;
#19129 = CARTESIAN_POINT ( 'NONE',  ( 10.77166557288789939, -63.24731521998059947, -45.20467220225359739 ) ) ;
#19130 = CARTESIAN_POINT ( 'NONE',  ( 68.13393739769706769, 17.98087126524489321, -74.20351669811762463 ) ) ;
#19131 = ORIENTED_EDGE ( 'NONE', *, *, #35243, .F. ) ;
#19132 = CARTESIAN_POINT ( 'NONE',  ( 20.49062781741232797, -22.31005579585255560, -44.10890486331368265 ) ) ;
#19133 = CARTESIAN_POINT ( 'NONE',  ( 57.22241557355649633, 19.34714437185240143, -53.44445692377340151 ) ) ;
#19134 = CARTESIAN_POINT ( 'NONE',  ( 52.63065796082889847, 19.00050544084379922, -76.99620446115829964 ) ) ;
#19135 = ORIENTED_EDGE ( 'NONE', *, *, #47691, .F. ) ;
#19136 = CARTESIAN_POINT ( 'NONE',  ( 11.24959019013326689, -65.20486053845806396, -47.30001787599645979 ) ) ;
#19137 = DIRECTION ( 'NONE',  ( 0.000000000000000000, -0.7371541402007413257, 0.6757246285173463818 ) ) ;
#19138 = DIRECTION ( 'NONE',  ( 0.1686178020941689892, 0.6660492713794449182, -0.7265992051412129005 ) ) ;
#19139 = CARTESIAN_POINT ( 'NONE',  ( 17.63604474694280100, -32.15985502643049898, -34.65000333055159842 ) ) ;
#19140 = EDGE_CURVE ( 'NONE', #9837, #18174, #8645, .T. ) ;
#19141 = CARTESIAN_POINT ( 'NONE',  ( 12.82100586541850085, -23.16650050900399904, -58.42394785367758914 ) ) ;
#19142 = EDGE_CURVE ( 'NONE', #23772, #17403, #28714, .T. ) ;
#19143 = CARTESIAN_POINT ( 'NONE',  ( 17.16957815729259806, -23.52717562567822185, -47.96600257623488517 ) ) ;
#19144 = DIRECTION ( 'NONE',  ( 0.000000000000000000, 0.000000000000000000, -1.000000000000000000 ) ) ;
#19145 = VERTEX_POINT ( 'NONE', #4796 ) ;
#19146 = ADVANCED_FACE ( 'NONE', ( #32803 ), #1903, .F. ) ;
#19147 = VERTEX_POINT ( 'NONE', #41732 ) ;
#19148 = FACE_OUTER_BOUND ( 'NONE', #23624, .T. ) ;
#19149 = B_SPLINE_CURVE_WITH_KNOTS ( 'NONE', 3,
 ( #16636, #28679, #44681, #40750, #20816, #916, #32857, #38119 ),
 .UNSPECIFIED., .F., .F.,
 ( 4, 2, 2, 4 ),
 ( 0.05028014561772611163, 0.06097673919850660207, 0.07774712209370319982, 0.08013618654915889705 ),
 .UNSPECIFIED. ) ;
#19150 = CARTESIAN_POINT ( 'NONE',  ( 11.12617520208469912, -10.09993916812369896, -59.49802510748859419 ) ) ;
#19151 = CARTESIAN_POINT ( 'NONE',  ( 50.89984241516300045, 13.88381105524969961, -11.21907654918599917 ) ) ;
#19152 = CARTESIAN_POINT ( 'NONE',  ( 11.92405982532479847, -22.23876938295769889, -32.14999999999999858 ) ) ;
#19153 = CARTESIAN_POINT ( 'NONE',  ( 17.63393739769639978, 10.88381105532070059, -34.64999999999999858 ) ) ;
#19154 = LINE ( 'NONE', #43533, #45165 ) ;
#19155 = CARTESIAN_POINT ( 'NONE',  ( 9.894687805641289913, 22.37488585622680048, -34.64999999999999858 ) ) ;
#19156 = ADVANCED_FACE ( 'NONE', ( #45150 ), #33721, .T. ) ;
#19157 = CARTESIAN_POINT ( 'NONE',  ( 12.00872700126539883, 33.65412506900099743, -16.20508613915610141 ) ) ;
#19158 = CIRCLE ( 'NONE', #12459, 10.00000000000000355 ) ;
#19160 = CIRCLE ( 'NONE', #34213, 2.000000000000002220 ) ;
#19159 = CARTESIAN_POINT ( 'NONE',  ( 23.87596833625310211, -18.45232675081680185, -61.61944235566640060 ) ) ;
#19161 = EDGE_CURVE ( 'NONE', #19396, #1406, #3566, .T. ) ;
#19162 = CARTESIAN_POINT ( 'NONE',  ( 20.10523294086599932, -22.40662673471619826, -32.14999999999999858 ) ) ;
#19163 = CARTESIAN_POINT ( 'NONE',  ( 56.29089617305770332, -50.69853828341889113, -75.05641376200790660 ) ) ;
#19165 = FACE_OUTER_BOUND ( 'NONE', #48715, .T. ) ;
#19164 = CARTESIAN_POINT ( 'NONE',  ( -5.266416193449879657, 16.47668896006809902, -5.857206300276859956 ) ) ;
#19166 = LINE ( 'NONE', #10545, #3754 ) ;
#19167 = DIRECTION ( 'NONE',  ( 0.000000000000000000, 0.000000000000000000, 1.000000000000000000 ) ) ;
#19168 = VERTEX_POINT ( 'NONE', #13201 ) ;
#19169 = CARTESIAN_POINT ( 'NONE',  ( -10.44076365005610008, -42.78597905884220154, -5.977015742479820481 ) ) ;
#19170 = CARTESIAN_POINT ( 'NONE',  ( 47.62315909503939793, 23.31001273183260025, -55.12979940376899890 ) ) ;
#19171 = FACE_OUTER_BOUND ( 'NONE', #22807, .T. ) ;
#19172 = LINE ( 'NONE', #26508, #20978 ) ;
#19173 = DIRECTION ( 'NONE',  ( -1.000000000000000000, 0.000000000000000000, 0.000000000000000000 ) ) ;
#19174 = CARTESIAN_POINT ( 'NONE',  ( 15.79986072486390114, -8.173401390133609112, -77.71837925212089715 ) ) ;
#19175 = CARTESIAN_POINT ( 'NONE',  ( 51.91394611766279610, 18.24433502379679695, -77.01723340761438408 ) ) ;
#19176 = CARTESIAN_POINT ( 'NONE',  ( 52.84630368501289865, 18.42025081107430040, -48.68178166803490114 ) ) ;
#19177 = CARTESIAN_POINT ( 'NONE',  ( 61.13393739769620083, -33.11618894467940066, -84.38499399519520239 ) ) ;
#19178 = CARTESIAN_POINT ( 'NONE',  ( 52.85589391196879916, -49.64722623523429945, -48.63421165633150167 ) ) ;
#19179 = CARTESIAN_POINT ( 'NONE',  ( 53.73157595231050720, 17.54735927887150027, -26.98518945364950383 ) ) ;
#19180 = CARTESIAN_POINT ( 'NONE',  ( 49.70112820465420356, 22.42515808270010069, -55.00786376658820132 ) ) ;
#19181 = CARTESIAN_POINT ( 'NONE',  ( 14.06322880297374489, -7.911096558319137273, -37.20899947889007819 ) ) ;
#19182 = CARTESIAN_POINT ( 'NONE',  ( 65.13393739769620083, 1.383811055320669947, -65.65000000000000568 ) ) ;
#19183 = CARTESIAN_POINT ( 'NONE',  ( 62.59312592420069876, -31.41572991903020196, -16.88303165987050036 ) ) ;
#19184 = CARTESIAN_POINT ( 'NONE',  ( 71.03049636386479904, 1.383411777981069957, -60.92458877361669778 ) ) ;
#19185 = CARTESIAN_POINT ( 'NONE',  ( 11.13393739769619906, 31.97814667466609961, -43.91303247421570433 ) ) ;
#19186 = CARTESIAN_POINT ( 'NONE',  ( 72.31167251984919631, 1.116860450401449878, -61.34995363534049773 ) ) ;
#19187 = CARTESIAN_POINT ( 'NONE',  ( 59.49262858449159808, 19.24776070067098743, -53.20292136905285929 ) ) ;
#19188 = CARTESIAN_POINT ( 'NONE',  ( 16.13393739769620083, -15.61618894467929941, -7.049999999999999822 ) ) ;
#19189 = ORIENTED_EDGE ( 'NONE', *, *, #34405, .F. ) ;
#19190 = ORIENTED_EDGE ( 'NONE', *, *, #17566, .T. ) ;
#19191 = CARTESIAN_POINT ( 'NONE',  ( 9.366584228470589579, -15.61631960056659985, -37.84717978380999881 ) ) ;
#19192 = CARTESIAN_POINT ( 'NONE',  ( 11.97538582446263256, -21.02759958964866982, -59.16115346696501831 ) ) ;
#19193 = ORIENTED_EDGE ( 'NONE', *, *, #40577, .F. ) ;
#19194 = CARTESIAN_POINT ( 'NONE',  ( 55.92590552531359549, -45.91410834023890430, -25.53549666432709842 ) ) ;
#19195 = CARTESIAN_POINT ( 'NONE',  ( 15.48732851072162298, -23.50178174477514403, -78.03370670278647481 ) ) ;
#19196 = AXIS2_PLACEMENT_3D ( 'NONE', #44796, #21185, #48471 ) ;
#19197 = ORIENTED_EDGE ( 'NONE', *, *, #36735, .F. ) ;
#19198 = CARTESIAN_POINT ( 'NONE',  ( 22.73658440641116130, -17.29642323430746131, -80.53196621422273438 ) ) ;
#19199 = AXIS2_PLACEMENT_3D ( 'NONE', #11682, #19279, #27649 ) ;
#19200 = CARTESIAN_POINT ( 'NONE',  ( 45.07403613745758264, 6.819010629880603247, -64.94950603516362264 ) ) ;
#19201 = CARTESIAN_POINT ( 'NONE',  ( 8.428875223629747282, -13.54537173489410762, -34.59100157321395130 ) ) ;
#19202 = AXIS2_PLACEMENT_3D ( 'NONE', #13900, #30823, #3328 ) ;
#19203 = ORIENTED_EDGE ( 'NONE', *, *, #15221, .F. ) ;
#19204 = CARTESIAN_POINT ( 'NONE',  ( 16.40925717896080016, -23.85672821053029935, -32.28170060268320185 ) ) ;
#19205 = EDGE_CURVE ( 'NONE', #36007, #51641, #28606, .T. ) ;
#19206 = B_SPLINE_CURVE_WITH_KNOTS ( 'NONE', 3,
 ( #43472, #39542, #23523, #38512 ),
 .UNSPECIFIED., .F., .F.,
 ( 4, 4 ),
 ( 0.8075652778063105997, 1.000000000000000000 ),
 .UNSPECIFIED. ) ;
#19207 = DIRECTION ( 'NONE',  ( -0.5720614028176829180, -0.4156269377774549634, 0.7071067811865477948 ) ) ;
#19208 = CIRCLE ( 'NONE', #40159, 36.00000000000000000 ) ;
#19209 = CYLINDRICAL_SURFACE ( 'NONE', #4617, 1.999999999999997113 ) ;
#19210 = EDGE_CURVE ( 'NONE', #39784, #26977, #49850, .T. ) ;
#19211 = CARTESIAN_POINT ( 'NONE',  ( 61.11794773234890243, -29.17036088169449926, -15.93336420193230296 ) ) ;
#19212 = CARTESIAN_POINT ( 'NONE',  ( 63.13228119804391270, 0.8904513541338849869, -62.33586013860640662 ) ) ;
#19213 = CARTESIAN_POINT ( 'NONE',  ( 47.13611152337789889, -54.39493520228780454, -75.29258675765889564 ) ) ;
#19214 = CARTESIAN_POINT ( 'NONE',  ( 22.72481099998648091, -17.38743435906051715, -36.53615103672703412 ) ) ;
#19215 = CARTESIAN_POINT ( 'NONE',  ( 44.44825913150810237, 14.59247941183189923, -8.385990530560489375 ) ) ;
#19216 = FACE_OUTER_BOUND ( 'NONE', #35641, .T. ) ;
#19217 = CARTESIAN_POINT ( 'NONE',  ( 83.54413676250719334, -44.84521321811879346, -47.09683803678880309 ) ) ;
#19218 = CARTESIAN_POINT ( 'NONE',  ( 11.78395124410701733, 34.19034018309990586, -17.88069317967955740 ) ) ;
#19219 = CARTESIAN_POINT ( 'NONE',  ( 24.19017502950390153, -17.37111537874790201, -33.57594075914509091 ) ) ;
#19220 = EDGE_CURVE ( 'NONE', #30264, #23002, #21350, .T. ) ;
#19221 = ORIENTED_EDGE ( 'NONE', *, *, #31100, .F. ) ;
#19222 = CARTESIAN_POINT ( 'NONE',  ( 53.40733904913949459, -49.15934302735570327, -27.32642110322520423 ) ) ;
#19223 = CARTESIAN_POINT ( 'NONE',  ( -0.2286426098680529873, -53.48569616968499929, -9.495855095443920035 ) ) ;
#19224 = CARTESIAN_POINT ( 'NONE',  ( 76.27673450680259748, -29.93995206988050128, -12.62359417470960032 ) ) ;
#19225 = CYLINDRICAL_SURFACE ( 'NONE', #1188, 1.999999999999997113 ) ;
#19226 = LINE ( 'NONE', #48051, #5586 ) ;
#19227 = AXIS2_PLACEMENT_3D ( 'NONE', #48144, #8306, #12244 ) ;
#19228 = AXIS2_PLACEMENT_3D ( 'NONE', #35777, #32072, #28931 ) ;
#19229 = CARTESIAN_POINT ( 'NONE',  ( 12.90754703535734826, -55.48555899889392862, -75.71503644607005867 ) ) ;
#19230 = AXIS2_PLACEMENT_3D ( 'NONE', #42831, #23641, #22877 ) ;
#19231 = CARTESIAN_POINT ( 'NONE',  ( 47.18324198357279897, 23.57489020266570279, -54.61058319554400242 ) ) ;
#19232 = CIRCLE ( 'NONE', #16729, 0.4999999999999935052 ) ;
#19233 = CARTESIAN_POINT ( 'NONE',  ( 63.04573361361109818, 1.102581332775290024, -62.55748568903120344 ) ) ;
#19234 = CARTESIAN_POINT ( 'NONE',  ( 57.28635611951199991, -50.59344279636220421, -53.60270239407589798 ) ) ;
#19235 = CARTESIAN_POINT ( 'NONE',  ( 41.57451193271510448, 12.62954792915630087, -3.761783078136979874 ) ) ;
#19236 = DIRECTION ( 'NONE',  ( -1.000000000000000000, 0.000000000000000000, 0.000000000000000000 ) ) ;
#19237 = FACE_OUTER_BOUND ( 'NONE', #48849, .T. ) ;
#19238 = CARTESIAN_POINT ( 'NONE',  ( 57.09844697708260242, -47.42443381619079901, -47.88085270719169273 ) ) ;
#19239 = FACE_OUTER_BOUND ( 'NONE', #42289, .T. ) ;
#19240 = CARTESIAN_POINT ( 'NONE',  ( 68.16820805406568695, -1.116429576517300015, -18.00618044202539991 ) ) ;
#19241 = CARTESIAN_POINT ( 'NONE',  ( 18.43783208065170243, -51.93606027628250388, -75.41551559479479749 ) ) ;
#19242 = CARTESIAN_POINT ( 'NONE',  ( 50.21208614976480078, -53.15602288804570463, -53.95043619330500206 ) ) ;
#19243 = CARTESIAN_POINT ( 'NONE',  ( 19.11518129813550004, -22.44399087095360201, -59.43630006696479740 ) ) ;
#19244 = CARTESIAN_POINT ( 'NONE',  ( 9.221499526225441556, -11.63191175217212958, -40.67433494680559392 ) ) ;
#19245 = CARTESIAN_POINT ( 'NONE',  ( 63.47253245025149937, 1.367958924391579956, -62.34793560868030227 ) ) ;
#19246 = VERTEX_POINT ( 'NONE', #13455 ) ;
#19247 = CARTESIAN_POINT ( 'NONE',  ( 8.786667189176620596, 31.89283771814190160, -46.67161560189330061 ) ) ;
#19248 = CARTESIAN_POINT ( 'NONE',  ( 22.90069508915062002, -15.67807337085623942, -34.45572864665300017 ) ) ;
#19249 = CARTESIAN_POINT ( 'NONE',  ( 73.01236646462280078, 1.336371993404959824, -68.64083569922701145 ) ) ;
#19250 = CARTESIAN_POINT ( 'NONE',  ( 46.47536507427530239, 8.886826513564159313, -54.64999999999999858 ) ) ;
#19251 = CARTESIAN_POINT ( 'NONE',  ( 9.018910532691149839, -15.87964395708210041, -81.23899999999999011 ) ) ;
#19252 = CARTESIAN_POINT ( 'NONE',  ( 44.99427537170129199, -45.82358684235350665, -8.742754287369370658 ) ) ;
#19253 = ORIENTED_EDGE ( 'NONE', *, *, #4651, .F. ) ;
#19254 = CARTESIAN_POINT ( 'NONE',  ( 17.48782757528399756, 21.61970083732919790, -76.12726769927830617 ) ) ;
#19255 = ORIENTED_EDGE ( 'NONE', *, *, #16581, .F. ) ;
#19256 = ORIENTED_EDGE ( 'NONE', *, *, #33822, .F. ) ;
#19257 = CARTESIAN_POINT ( 'NONE',  ( 38.67452568954060155, -37.56081407618430035, -81.65000000000000568 ) ) ;
#19258 = DIRECTION ( 'NONE',  ( 0.000000000000000000, -1.000000000000000000, 0.000000000000000000 ) ) ;
#19259 = DIRECTION ( 'NONE',  ( 0.000000000000000000, 0.000000000000000000, 1.000000000000000000 ) ) ;
#19260 = ORIENTED_EDGE ( 'NONE', *, *, #10787, .F. ) ;
#19261 = CARTESIAN_POINT ( 'NONE',  ( 18.20461993357798036, -7.911089693863461392, -53.09100360769544125 ) ) ;
#19262 = ORIENTED_EDGE ( 'NONE', *, *, #34201, .T. ) ;
#19263 = DIRECTION ( 'NONE',  ( 1.000000000000000000, 0.000000000000000000, 0.000000000000000000 ) ) ;
#19264 = EDGE_CURVE ( 'NONE', #30581, #10936, #27045, .T. ) ;
#19265 = B_SPLINE_CURVE_WITH_KNOTS ( 'NONE', 3,
 ( #29690, #30469, #1931, #17912, #42549, #33881, #46489, #30213, #29946, #42286, #38350, #45700, #6127, #10579, #33367, #45443, #13480, #9800 ),
 .UNSPECIFIED., .F., .F.,
 ( 4, 2, 2, 2, 2, 2, 2, 2, 4 ),
 ( 0.5000000032861632304, 0.5625000028753927017, 0.6250000024646221730, 0.6875000020538517553, 0.7500000016430812266, 0.8125000012323109200, 0.8750000008215406133, 0.9375000004107703067, 1.000000000000000000 ),
 .UNSPECIFIED. ) ;
#19266 = FACE_OUTER_BOUND ( 'NONE', #34793, .T. ) ;
#19267 = AXIS2_PLACEMENT_3D ( 'NONE', #37062, #1160, #13745 ) ;
#19268 = AXIS2_PLACEMENT_3D ( 'NONE', #50595, #26723, #34850 ) ;
#19269 = ORIENTED_EDGE ( 'NONE', *, *, #35181, .T. ) ;
#19270 = LINE ( 'NONE', #36022, #36686 ) ;
#19271 = CARTESIAN_POINT ( 'NONE',  ( 51.90125965379149875, -51.26050537052380207, -76.04050507290840244 ) ) ;
#19272 = AXIS2_PLACEMENT_3D ( 'NONE', #3019, #34711, #46543 ) ;
#19273 = CARTESIAN_POINT ( 'NONE',  ( 60.91201348210339717, 14.41240981587099945, -47.67204987013359840 ) ) ;
#19274 = AXIS2_PLACEMENT_3D ( 'NONE', #47314, #27875, #47561 ) ;
#19275 = AXIS2_PLACEMENT_3D ( 'NONE', #18110, #37259, #49326 ) ;
#19276 = B_SPLINE_CURVE_WITH_KNOTS ( 'NONE', 3,
 ( #3677, #4175, #47699, #20151, #1282, #28528, #16230, #41367, #40340, #40590 ),
 .UNSPECIFIED., .F., .F.,
 ( 4, 2, 2, 2, 4 ),
 ( 0.000000000000000000, 0.1774999999994806010, 0.3374999999985014987, 0.4374999999978896326, 0.5000003605096956516 ),
 .UNSPECIFIED. ) ;
#19277 = CARTESIAN_POINT ( 'NONE',  ( 22.89902617865969958, -15.44245184754445965, -40.44465385252913592 ) ) ;
#19278 = B_SPLINE_CURVE_WITH_KNOTS ( 'NONE', 3,
 ( #51484, #11398, #15584, #14085, #30046, #2556, #35226, #47556, #15324, #11652, #16868, #33082, #37036, #32044, #12684, #44128, #29161, #24173 ),
 .UNSPECIFIED., .F., .F.,
 ( 4, 2, 2, 2, 2, 2, 2, 2, 4 ),
 ( 0.5000015687207624016, 0.5625013726306670181, 0.6250011765405716346, 0.6875009804504761401, 0.7500007843603807567, 0.8125005882702855953, 0.8750003921801903228, 0.9375001960900952724, 1.000000000000000000 ),
 .UNSPECIFIED. ) ;
#19279 = DIRECTION ( 'NONE',  ( 0.000000000000000000, 1.000000000000000000, 0.000000000000000000 ) ) ;
#19280 = CARTESIAN_POINT ( 'NONE',  ( -6.118916323140140001, 15.26694961539969952, -5.118327416809539621 ) ) ;
#19281 = ADVANCED_FACE ( 'NONE', ( #8997 ), #21154, .T. ) ;
#19282 = CARTESIAN_POINT ( 'NONE',  ( 47.13701521578290965, 23.47046883074774470, -74.81156575898371841 ) ) ;
#19283 = DIRECTION ( 'NONE',  ( -0.8090169943749487835, -0.5877852522924713607, 0.000000000000000000 ) ) ;
#19284 = CARTESIAN_POINT ( 'NONE',  ( 23.33437357335099804, -18.73716107904780159, -51.41769413899939423 ) ) ;
#19285 = EDGE_CURVE ( 'NONE', #45555, #1409, #9488, .T. ) ;
#19286 = VERTEX_POINT ( 'NONE', #41471 ) ;
#19287 = DIRECTION ( 'NONE',  ( 0.8535492322677342703, -0.3460892072839221734, 0.3894559907059431669 ) ) ;
#19288 = EDGE_CURVE ( 'NONE', #44094, #30599, #49099, .T. ) ;
#19289 = CARTESIAN_POINT ( 'NONE',  ( 71.85583611592080899, 1.158194067775949909, -70.31019080967980983 ) ) ;
#19290 = CARTESIAN_POINT ( 'NONE',  ( 45.78260039019426131, -40.08104085361300406, -58.01479249339848110 ) ) ;
#19291 = CARTESIAN_POINT ( 'NONE',  ( 15.22027405775829934, 19.63653300932890033, -20.91173439138579937 ) ) ;
#19292 = CARTESIAN_POINT ( 'NONE',  ( 22.23620501646692915, 22.68747772516199035, -34.73809820100316870 ) ) ;
#19293 = SURFACE_STYLE_FILL_AREA ( #19546 ) ;
#19294 = CARTESIAN_POINT ( 'NONE',  ( 61.25723466965784780, 14.07825688653815632, -47.12444968528875222 ) ) ;
#19295 = CARTESIAN_POINT ( 'NONE',  ( 48.31521067748249720, -54.24088337835979701, -55.14618947275539540 ) ) ;
#19296 = CARTESIAN_POINT ( 'NONE',  ( 23.38479371968623255, -12.38874807463486505, -45.37444489943354142 ) ) ;
#19297 = CARTESIAN_POINT ( 'NONE',  ( 22.90101955563642733, -15.61618902498797290, -36.84717743668400658 ) ) ;
#19298 = CARTESIAN_POINT ( 'NONE',  ( 7.853097003783780394, -60.52042854835909935, -20.86915960608759946 ) ) ;
#19299 = ORIENTED_EDGE ( 'NONE', *, *, #2191, .T. ) ;
#19300 = VECTOR ( 'NONE', #3200, 1000.000000000000000 ) ;
#19301 = CARTESIAN_POINT ( 'NONE',  ( 22.97870654863990225, -12.67410981443290119, -36.93812364489689770 ) ) ;
#19302 = EDGE_LOOP ( 'NONE', ( #1141, #51802, #11779, #43389 ) ) ;
#19303 = DIRECTION ( 'NONE',  ( -1.000000000000000000, 0.000000000000000000, 0.000000000000000000 ) ) ;
#19304 = VECTOR ( 'NONE', #19259, 1000.000000000000000 ) ;
#19305 = CARTESIAN_POINT ( 'NONE',  ( 10.10517893431049963, -55.15925497894330931, -21.14999999999999858 ) ) ;
#19306 = CARTESIAN_POINT ( 'NONE',  ( 61.28610861176739633, 13.99802266614350010, -28.15000000000000213 ) ) ;
#19307 = CARTESIAN_POINT ( 'NONE',  ( -13.39236625349549925, -0.8785706602474749882, -54.64999999999999858 ) ) ;
#19309 = DIRECTION ( 'NONE',  ( 0.000000000000000000, 0.000000000000000000, -1.000000000000000000 ) ) ;
#19308 = CARTESIAN_POINT ( 'NONE',  ( 61.75019796695546148, 13.88381105532070059, -26.84765975578291020 ) ) ;
#19310 = VECTOR ( 'NONE', #32130, 1000.000000000000114 ) ;
#19311 = CARTESIAN_POINT ( 'NONE',  ( -0.2277270843104434728, -10.73582424797172585, -34.96449406573682239 ) ) ;
#19312 = CARTESIAN_POINT ( 'NONE',  ( 23.83903846881501210, -13.54551738375433523, -67.70899597192914143 ) ) ;
#19313 = CARTESIAN_POINT ( 'NONE',  ( 56.62432785584509531, 19.48323104975959907, -53.83726655423080132 ) ) ;
#19314 = B_SPLINE_SURFACE_WITH_KNOTS ( 'NONE', 3, 3, ( 
 ( #508, #44803, #32982, #9162, #41128, #32199, #12318, #4705, #1298, #16498, #20673, #28802, #32449, #16760 ),
 ( #24077, #12071, #28025, #5240, #36403, #12577, #40097, #28542, #44540, #4189, #20167, #48219, #8641, #24592 ),
 ( #4969, #40605, #12844, #36661, #20936, #32714, #48740, #36936, #1037, #33762, #38489, #2325, #41637, #45325 ),
 ( #14381, #5745, #50293, #10196, #2590, #13360, #33509, #6264, #49265, #49522, #2072, #45840, #29574, #18050 ),
 ( #13614, #1551, #9929, #45580, #21453, #34270, #9675, #18565, #26410, #29318, #25633, #9429, #25379, #41380 ),
 ( #29823, #50026, #34016, #18299, #21702, #10457, #22224, #30346, #37452, #25891, #37710, #38232, #14119, #1809 ),
 ( #26155, #21963, #30085, #46369, #42431, #5497, #13867, #46110, #42165, #41904, #17788, #6520, #22482, #6004 ),
 ( #17539, #49773, #37972, #35587, #27451, #3882, #31627, #43454, #43708, #47646, #42689, #23247, #34800, #39777 ),
 ( #46887, #51322, #31371, #15418, #34542, #3111, #51574, #15157, #10974, #15673, #6786, #31118, #11495, #46626 ),
 ( #26941, #7043, #7556, #39525, #19596, #11752, #27709, #7812, #50545, #23763, #40034, #40545, #12780, #28737 ) ),
 .UNSPECIFIED., .F., .F., .F.,
 ( 4, 1, 1, 1, 1, 1, 1, 4 ),
 ( 4, 2, 2, 2, 2, 2, 4 ),
 ( -0.0003127823370728670155, 0.1428571428571430157, 0.2857142857142860315, 0.4285714285714289917, 0.5714285714285709528, 0.7142857142857139685, 0.8571428571428569843, 1.000000000000000000 ),
 ( -0.0003008787986270000095, 0.2008536346930439864, 0.4304006457708079991, 0.5738675276944109616, 0.6456009686562129701, 0.7603744741950950736, 0.7973406569620060669 ),
 .UNSPECIFIED. ) ;
#19315 = VERTEX_POINT ( 'NONE', #12933 ) ;
#19316 = CARTESIAN_POINT ( 'NONE',  ( 84.42051485081360340, -43.53095137563540362, -47.44928677006510043 ) ) ;
#19317 = VERTEX_POINT ( 'NONE', #8732 ) ;
#19318 = ORIENTED_EDGE ( 'NONE', *, *, #36916, .F. ) ;
#19319 = CARTESIAN_POINT ( 'NONE',  ( 22.90077909847273219, -15.61618896438501203, -58.84717277627543552 ) ) ;
#19320 = LINE ( 'NONE', #51298, #3092 ) ;
#19321 = CARTESIAN_POINT ( 'NONE',  ( 76.47354785737799432, -26.64541773940327118, -13.11343201606089259 ) ) ;
#19322 = CARTESIAN_POINT ( 'NONE',  ( 9.788883518080631063, -64.09936060989920747, -46.59784358706489371 ) ) ;
#19323 = ORIENTED_EDGE ( 'NONE', *, *, #49237, .F. ) ;
#19324 = VERTEX_POINT ( 'NONE', #20763 ) ;
#19325 = CARTESIAN_POINT ( 'NONE',  ( 71.40227520965750330, 1.367045641526529964, -60.97477925803730159 ) ) ;
#19326 = CARTESIAN_POINT ( 'NONE',  ( 56.90065466210369749, -45.21025265706699514, -25.29837482150149697 ) ) ;
#19327 = CARTESIAN_POINT ( 'NONE',  ( 56.40159924779830192, -50.63276481660309969, -53.06856169275020818 ) ) ;
#19328 = ADVANCED_FACE ( 'NONE', ( #36751 ), #1123, .T. ) ;
#19329 = CARTESIAN_POINT ( 'NONE',  ( 19.71665332066073617, -9.848143450206167770, -46.12982609512481247 ) ) ;
#19330 = CARTESIAN_POINT ( 'NONE',  ( 59.16206914407690221, -2.876195328580839927, -15.65935069007090163 ) ) ;
#19331 = CARTESIAN_POINT ( 'NONE',  ( 51.37477222274990396, -49.09661486018149645, -76.61256277772369572 ) ) ;
#19332 = CARTESIAN_POINT ( 'NONE',  ( 8.222937397696199469, -15.61618894467929941, -32.14999999999999858 ) ) ;
#19333 = EDGE_LOOP ( 'NONE', ( #44933, #14805, #36020, #46548 ) ) ;
#19334 = CARTESIAN_POINT ( 'NONE',  ( 12.06284766121009966, -63.44323389162830296, -22.25048313876769868 ) ) ;
#19335 = LINE ( 'NONE', #35581, #42704 ) ;
#19336 = CARTESIAN_POINT ( 'NONE',  ( 22.90093741645776504, -14.73039735216230284, -52.41115107345247992 ) ) ;
#19337 = CARTESIAN_POINT ( 'NONE',  ( 56.65979965533069418, -47.79656003688090493, -48.39907199131990012 ) ) ;
#19338 = CARTESIAN_POINT ( 'NONE',  ( 13.45295195435610047, -22.99176110175159948, -52.62347199549349597 ) ) ;
#19339 = CARTESIAN_POINT ( 'NONE',  ( 12.16981616251259801, -50.04926267044390187, -21.14999999999999858 ) ) ;
#19340 = CARTESIAN_POINT ( 'NONE',  ( 22.14986259033789651, -18.71508664667078747, -32.60422815991633172 ) ) ;
#19341 = CARTESIAN_POINT ( 'NONE',  ( 55.78258317375759390, 14.07033184101250178, -15.69927152601569631 ) ) ;
#19342 = CARTESIAN_POINT ( 'NONE',  ( 61.18526399883489830, -45.48745254298339802, -47.51713262586719821 ) ) ;
#19343 = CARTESIAN_POINT ( 'NONE',  ( 56.85837508264230422, -50.62728578079150310, -53.45324575303870063 ) ) ;
#19344 = AXIS2_PLACEMENT_3D ( 'NONE', #889, #16884, #16098 ) ;
#19345 = CARTESIAN_POINT ( 'NONE',  ( 19.82873695480079590, -9.608609115224629349, -56.52269350815070226 ) ) ;
#19346 = CARTESIAN_POINT ( 'NONE',  ( 46.66336238603499709, -39.88456775088300077, -54.57128118813670170 ) ) ;
#19347 = AXIS2_PLACEMENT_3D ( 'NONE', #15139, #2833, #30837 ) ;
#19348 = ORIENTED_EDGE ( 'NONE', *, *, #47152, .T. ) ;
#19349 = CARTESIAN_POINT ( 'NONE',  ( 13.44774942451820010, -51.74366499200459657, -74.55381114264599773 ) ) ;
#19350 = CARTESIAN_POINT ( 'NONE',  ( 64.85894149894409111, 0.8879664753683469414, -60.62259972594610247 ) ) ;
#19351 = EDGE_CURVE ( 'NONE', #2360, #10572, #14479, .T. ) ;
#19352 = CARTESIAN_POINT ( 'NONE',  ( 42.03135417276770625, -45.79966294656320258, -6.846959983868809552 ) ) ;
#19353 = DIRECTION ( 'NONE',  ( 0.000000000000000000, 0.000000000000000000, 1.000000000000000000 ) ) ;
#19354 = CARTESIAN_POINT ( 'NONE',  ( 72.74715221972319057, 13.88381105532070059, -14.68167674020449986 ) ) ;
#19355 = CARTESIAN_POINT ( 'NONE',  ( -21.36606260230379917, -53.11618894467930119, 11.84999999999999964 ) ) ;
#19356 = CARTESIAN_POINT ( 'NONE',  ( 82.50626185013108227, 14.19657067018509977, -47.45622494215220399 ) ) ;
#19357 = CARTESIAN_POINT ( 'NONE',  ( 29.46622902366960162, -33.11618894467940066, -54.64999999999999858 ) ) ;
#19359 = CARTESIAN_POINT ( 'NONE',  ( 45.74957564526550158, -38.01398953213499965, -61.56096017950429911 ) ) ;
#19358 = DIRECTION ( 'NONE',  ( 0.000000000000000000, 1.000000000000000000, 0.000000000000000000 ) ) ;
#19360 = CARTESIAN_POINT ( 'NONE',  ( 14.66318557257089950, -52.01452886429046885, -75.82251645564090836 ) ) ;
#19361 = LINE ( 'NONE', #50825, #48870 ) ;
#19362 = DIRECTION ( 'NONE',  ( 0.000000000000000000, 0.000000000000000000, 1.000000000000000000 ) ) ;
#19363 = ORIENTED_EDGE ( 'NONE', *, *, #7026, .T. ) ;
#19364 = CARTESIAN_POINT ( 'NONE',  ( 52.91963055335400412, -49.63709126784409875, -48.95754079928280333 ) ) ;
#19365 = ORIENTED_EDGE ( 'NONE', *, *, #38268, .T. ) ;
#19366 = CARTESIAN_POINT ( 'NONE',  ( 42.54139083816280476, 6.317655820708358405, -77.59090943095287685 ) ) ;
#19367 = CARTESIAN_POINT ( 'NONE',  ( 28.63393739769620083, -15.61618894467929941, -2.149999999999999911 ) ) ;
#19368 = CARTESIAN_POINT ( 'NONE',  ( 13.93400774615080095, 19.94011110403380371, -22.49576377567830221 ) ) ;
#19369 = CARTESIAN_POINT ( 'NONE',  ( 16.13393739769620083, -15.61618894467929941, -6.649999999999999467 ) ) ;
#19370 = CARTESIAN_POINT ( 'NONE',  ( 13.72450424504459932, -22.24470239639139635, -53.06379780079559794 ) ) ;
#19371 = CARTESIAN_POINT ( 'NONE',  ( 52.97667581671070280, 18.39974466412820320, -49.06651679849090186 ) ) ;
#19372 = CARTESIAN_POINT ( 'NONE',  ( 55.91594421088640132, -45.90466751205540419, -17.93019951326149908 ) ) ;
#19373 = DIRECTION ( 'NONE',  ( 0.000000000000000000, -1.000000000000000000, 0.000000000000000000 ) ) ;
#19374 = ORIENTED_EDGE ( 'NONE', *, *, #29278, .T. ) ;
#19375 = CARTESIAN_POINT ( 'NONE',  ( 18.90449655907080029, -22.95858338196050141, -33.67265358074869397 ) ) ;
#19376 = B_SPLINE_CURVE_WITH_KNOTS ( 'NONE', 3,
 ( #20889, #986, #28230, #48168, #9384, #21403, #8332, #24285, #40305, #4397 ),
 .UNSPECIFIED., .F., .F.,
 ( 4, 1, 1, 1, 1, 1, 1, 4 ),
 ( 0.5000039623326250071, 0.5569989693773305106, 0.6362179004408794469, 0.7154368315045867011, 0.7946557625681401893, 0.8738746936316936775, 0.9530936246954009317, 1.000000000000000000 ),
 .UNSPECIFIED. ) ;
#19377 = VERTEX_POINT ( 'NONE', #38066 ) ;
#19378 = CARTESIAN_POINT ( 'NONE',  ( 11.91784411962730061, -65.43085189686328818, -17.65793976188430037 ) ) ;
#19379 = CARTESIAN_POINT ( 'NONE',  ( 13.00893739769619906, 34.28605925116850273, -47.75434321273180416 ) ) ;
#19380 = CARTESIAN_POINT ( 'NONE',  ( 72.75389709491450674, 1.389468113695450091, -62.45014271800210537 ) ) ;
#19381 = VECTOR ( 'NONE', #28701, 1000.000000000000000 ) ;
#19382 =( BOUNDED_CURVE ( )  B_SPLINE_CURVE ( 3, ( #24527, #40544, #4634, #12779 ),
 .UNSPECIFIED., .F., .F. ) 
 B_SPLINE_CURVE_WITH_KNOTS ( ( 4, 4 ),
 ( 4.302261639843196761, 5.087659803240767609 ),
 .UNSPECIFIED. ) 
 CURVE ( )  GEOMETRIC_REPRESENTATION_ITEM ( )  RATIONAL_B_SPLINE_CURVE ( ( 1.000000000000000000, 0.9492530216741755789, 0.9492530216741755789, 1.000000000000000000 ) ) 
 REPRESENTATION_ITEM ( '' )  );
#19383 = FACE_OUTER_BOUND ( 'NONE', #51548, .T. ) ;
#19384 = DIRECTION ( 'NONE',  ( -1.838191881340036742E-22, -1.000000000000000000, 6.470619327693540153E-12 ) ) ;
#19385 = CARTESIAN_POINT ( 'NONE',  ( 12.98614995704637032, -49.83962866466749375, -82.44267625234935792 ) ) ;
#19386 = AXIS2_PLACEMENT_3D ( 'NONE', #29337, #36165, #32211 ) ;
#19387 = ORIENTED_EDGE ( 'NONE', *, *, #29983, .F. ) ;
#19388 = DIRECTION ( 'NONE',  ( 0.000000000000000000, -1.000000000000000000, 0.000000000000000000 ) ) ;
#19389 = CARTESIAN_POINT ( 'NONE',  ( 10.77117107879669966, -63.22212903752630098, -45.20474350506940198 ) ) ;
#19390 = EDGE_CURVE ( 'NONE', #49436, #7343, #11161, .T. ) ;
#19391 = CARTESIAN_POINT ( 'NONE',  ( 68.13393739769814772, 19.38381105532029736, -71.50000000000200373 ) ) ;
#19392 = ORIENTED_EDGE ( 'NONE', *, *, #27435, .T. ) ;
#19393 = CARTESIAN_POINT ( 'NONE',  ( 48.42521416700790127, 25.14253336855949783, -74.14999999999999147 ) ) ;
#19394 = CARTESIAN_POINT ( 'NONE',  ( 12.25210256922130725, -8.645705515954809073, -76.84572645005218305 ) ) ;
#19395 = DIRECTION ( 'NONE',  ( 0.000000000000000000, 0.000000000000000000, 1.000000000000000000 ) ) ;
#19396 = VERTEX_POINT ( 'NONE', #13960 ) ;
#19397 = EDGE_CURVE ( 'NONE', #40665, #40081, #46754, .T. ) ;
#19398 = DIRECTION ( 'NONE',  ( 1.000000000000000000, 0.000000000000000000, 0.000000000000000000 ) ) ;
#19399 = CARTESIAN_POINT ( 'NONE',  ( 53.35835817625017796, 20.15050933124701160, -75.63636005538151608 ) ) ;
#19400 = CARTESIAN_POINT ( 'NONE',  ( 83.63329919740728258, -44.53040215208500996, -46.55718455497714103 ) ) ;
#19401 = DIRECTION ( 'NONE',  ( 0.000000000000000000, -1.000000000000000000, 0.000000000000000000 ) ) ;
#19402 = ADVANCED_FACE ( 'NONE', ( #19171 ), #10550, .T. ) ;
#19403 = CARTESIAN_POINT ( 'NONE',  ( 18.75273301534850034, -7.797964749320120070, -65.39521378727619094 ) ) ;
#19404 = CARTESIAN_POINT ( 'NONE',  ( 52.77888429003910176, -49.71941859661360041, -48.89378112591379733 ) ) ;
#19405 = CARTESIAN_POINT ( 'NONE',  ( 9.829250996703903454, -12.53343974589846788, -37.99218164148856403 ) ) ;
#19406 = CARTESIAN_POINT ( 'NONE',  ( 46.32873999300467460, -38.18646364691427664, -58.67597187213492305 ) ) ;
#19407 = ORIENTED_EDGE ( 'NONE', *, *, #3623, .T. ) ;
#19408 = APPLICATION_CONTEXT ( 'automotive_design' ) ;
#19409 = EDGE_LOOP ( 'NONE', ( #26078, #15607 ) ) ;
#19410 = LINE ( 'NONE', #51133, #32554 ) ;
#19411 = CARTESIAN_POINT ( 'NONE',  ( 22.22458528030719904, -19.90695835996979923, -54.42801351941700005 ) ) ;
#19412 = CARTESIAN_POINT ( 'NONE',  ( 50.12047694534380327, -49.40224992130579551, -76.14999999999999147 ) ) ;
#19413 = FACE_OUTER_BOUND ( 'NONE', #3289, .T. ) ;
#19414 = CARTESIAN_POINT ( 'NONE',  ( 47.36716192977550577, 23.43728642252559879, -74.36069403054010252 ) ) ;
#19415 = DIRECTION ( 'NONE',  ( 6.008901426488883237E-29, 1.000000000000000000, -1.065814103640210074E-14 ) ) ;
#19416 = EDGE_CURVE ( 'NONE', #13604, #9988, #22021, .T. ) ;
#19417 = CARTESIAN_POINT ( 'NONE',  ( 23.13393739769620083, -2.337132753317950229, -62.14999999999999858 ) ) ;
#19418 = B_SPLINE_CURVE_WITH_KNOTS ( 'NONE', 3,
 ( #16317, #51710, #48552, #15804, #50557, #37988, #41653, #17804, #10727, #2084, #46641, #6532, #34812, #9689, #18062, #5757, #33777, #26680 ),
 .UNSPECIFIED., .F., .F.,
 ( 4, 2, 2, 2, 2, 2, 2, 2, 4 ),
 ( 0.5000001415279446970, 0.5625001238369514711, 0.6250001061459582452, 0.6875000884549651303, 0.7500000707639719044, 0.8125000530729789006, 0.8750000353819860077, 0.9375000176909930039, 1.000000000000000000 ),
 .UNSPECIFIED. ) ;
#19419 = AXIS2_PLACEMENT_3D ( 'NONE', #48384, #24499, #40517 ) ;
#19420 = CARTESIAN_POINT ( 'NONE',  ( 12.13696592145019792, 33.93507367045299361, -16.64705455762469910 ) ) ;
#19421 = CARTESIAN_POINT ( 'NONE',  ( 9.092216188204538696, -19.90534773362269760, -70.33352477266458891 ) ) ;
#19422 = CARTESIAN_POINT ( 'NONE',  ( 52.56521993351449851, -49.86179673305689874, -28.06704019101890069 ) ) ;
#19423 = CARTESIAN_POINT ( 'NONE',  ( 54.95770575214509535, -50.62412422504770149, -76.43951288111850317 ) ) ;
#19425 = CARTESIAN_POINT ( 'NONE',  ( 9.366917638880204677, -14.73053537850788075, -59.49448256068535557 ) ) ;
#19424 = CARTESIAN_POINT ( 'NONE',  ( -9.182228926101151600, 12.40783594017670133, -5.100143237003939234 ) ) ;
#19426 = CARTESIAN_POINT ( 'NONE',  ( 63.09706677394889596, 1.198183261254770038, -68.71131498411249083 ) ) ;
#19427 = CARTESIAN_POINT ( 'NONE',  ( 68.13393739769630031, 1.883811055320669947, -70.34999999999999432 ) ) ;
#19428 = ORIENTED_EDGE ( 'NONE', *, *, #22169, .F. ) ;
#19429 = CARTESIAN_POINT ( 'NONE',  ( 53.11047205726560350, -49.51384561212010027, -48.81638560371479940 ) ) ;
#19430 = CARTESIAN_POINT ( 'NONE',  ( 47.69543556716480026, 23.26888818243800117, -54.96140342535039736 ) ) ;
#19431 = ADVANCED_FACE ( 'NONE', ( #50634 ), #30701, .F. ) ;
#19432 = CARTESIAN_POINT ( 'NONE',  ( 61.28592748474870433, -45.23049522091189800, -28.15095074383799911 ) ) ;
#19433 = CARTESIAN_POINT ( 'NONE',  ( 68.88393739769620083, -38.11618894467930119, -73.25000000000000000 ) ) ;
#19434 = CARTESIAN_POINT ( 'NONE',  ( 61.52542916938325135, -45.35171639540813970, -47.31474053514811828 ) ) ;
#19435 = CARTESIAN_POINT ( 'NONE',  ( 12.28329235829779975, -21.99421580145110156, -70.90555118064979467 ) ) ;
#19436 = CARTESIAN_POINT ( 'NONE',  ( 51.43375900340840445, 18.02660632394349705, -76.62099598077431040 ) ) ;
#19437 = CARTESIAN_POINT ( 'NONE',  ( 53.06801998396470310, 18.30370955338970163, -48.81041485190910123 ) ) ;
#19438 = DIRECTION ( 'NONE',  ( -0.8090169943749478954, -0.5877852522924724710, 0.000000000000000000 ) ) ;
#19439 = CARTESIAN_POINT ( 'NONE',  ( 52.82975622904280755, -49.66092049964720445, -48.47378032971909789 ) ) ;
#19440 = LINE ( 'NONE', #27043, #14559 ) ;
#19441 = CARTESIAN_POINT ( 'NONE',  ( 21.94685905566085182, -20.98253927633499671, -61.74495104792147515 ) ) ;
#19442 = CARTESIAN_POINT ( 'NONE',  ( 15.09836989202466384, -7.705191364866749382, -37.25066627595537483 ) ) ;
#19443 = CARTESIAN_POINT ( 'NONE',  ( 19.54194828133133299, -21.52908873155781677, -70.78615563984314463 ) ) ;
#19444 = CARTESIAN_POINT ( 'NONE',  ( 63.70037062081990342, -31.89081416583059436, -17.35709357403409925 ) ) ;
#19445 = CARTESIAN_POINT ( 'NONE',  ( 71.26464087954850868, 1.328073773609220076, -60.83220757462540007 ) ) ;
#19446 = CARTESIAN_POINT ( 'NONE',  ( 11.13393739769619906, 32.27621211514449584, -43.92731420739779225 ) ) ;
#19447 = CARTESIAN_POINT ( 'NONE',  ( 72.80625431757680133, 1.063298638255719908, -61.89539269462630244 ) ) ;
#19448 = CARTESIAN_POINT ( 'NONE',  ( 16.13393752749879795, -15.61618872006030045, -20.64999988453819668 ) ) ;
#19449 = CYLINDRICAL_SURFACE ( 'NONE', #9258, 3.000000000000003997 ) ;
#19450 = VERTEX_POINT ( 'NONE', #22574 ) ;
#19451 = ORIENTED_EDGE ( 'NONE', *, *, #20482, .F. ) ;
#19452 = CYLINDRICAL_SURFACE ( 'NONE', #7006, 3.000000000000000000 ) ;
#19453 = CARTESIAN_POINT ( 'NONE',  ( 22.72481302302869821, -17.38742434606708187, -58.53615329005432244 ) ) ;
#19454 = ORIENTED_EDGE ( 'NONE', *, *, #15882, .F. ) ;
#19455 = CARTESIAN_POINT ( 'NONE',  ( 56.34641762111630214, -45.71298718759459945, -25.89277606233699913 ) ) ;
#19456 = CARTESIAN_POINT ( 'NONE',  ( -30.36606260230379917, -53.11618894467930119, 10.84999999999999964 ) ) ;
#19457 = EDGE_CURVE ( 'NONE', #3287, #25228, #51333, .T. ) ;
#19458 = ORIENTED_EDGE ( 'NONE', *, *, #8212, .T. ) ;
#19459 = CARTESIAN_POINT ( 'NONE',  ( 8.731180243531696306, -48.92556967366426335, -34.79644561402096770 ) ) ;
#19460 = CARTESIAN_POINT ( 'NONE',  ( 42.68436296462748203, 6.498366103123425219, -76.89780545169345771 ) ) ;
#19461 = FACE_OUTER_BOUND ( 'NONE', #45063, .T. ) ;
#19462 = EDGE_CURVE ( 'NONE', #27459, #34702, #7372, .T. ) ;
#19463 = ORIENTED_EDGE ( 'NONE', *, *, #23237, .F. ) ;
#19464 = CARTESIAN_POINT ( 'NONE',  ( 24.37106953178879820, -15.98036188512979727, -31.80638701630159915 ) ) ;
#19465 = B_SPLINE_CURVE_WITH_KNOTS ( 'NONE', 3,
 ( #32780, #16562, #7940, #82, #32263, #20743, #23887, #4007, #16054, #36470, #576, #8976, #32009, #12134, #44605, #8713, #24663, #9998 ),
 .UNSPECIFIED., .F., .F.,
 ( 4, 2, 2, 2, 2, 2, 2, 2, 4 ),
 ( 0.000000000000000000, 0.06250003597552350465, 0.1250000719510470093, 0.1875001079265705139, 0.2500001439020940186, 0.3125001798776175232, 0.3750002158531410279, 0.4375002518286645325, 0.5000002878041880372 ),
 .UNSPECIFIED. ) ;
#19466 = CARTESIAN_POINT ( 'NONE',  ( -30.36606260230379917, 21.88381105532059934, 11.84999999999999964 ) ) ;
#19467 = DIRECTION ( 'NONE',  ( 0.7071067811865475727, -0.7071067811865475727, 0.000000000000000000 ) ) ;
#19468 = B_SPLINE_CURVE_WITH_KNOTS ( 'NONE', 3,
 ( #37555, #18415, #17653, #29682, #38084, #9792, #21821, #38342, #34389, #26008, #30719 ),
 .UNSPECIFIED., .F., .F.,
 ( 4, 1, 1, 1, 1, 1, 1, 1, 4 ),
 ( 0.4999981796106400811, 0.5054020672895994659, 0.5846209983532170140, 0.6638399294168356723, 0.7430588604804532205, 0.8222777915440718788, 0.9014967226076894269, 0.9807156536713079742, 1.000000000000000000 ),
 .UNSPECIFIED. ) ;
#19469 = CARTESIAN_POINT ( 'NONE',  ( 61.73979651615039899, -29.77994616252469839, -16.06604299805859881 ) ) ;
#19470 = CARTESIAN_POINT ( 'NONE',  ( 12.72598990436487298, -9.703252614503353968, -63.78615428896809902 ) ) ;
#19471 = CARTESIAN_POINT ( 'NONE',  ( 46.84762105052649872, -53.84887631677259634, -75.86145147363799879 ) ) ;
#19472 = CARTESIAN_POINT ( 'NONE',  ( 10.89975959942620065, -9.768956234441111164, -75.28008627968870314 ) ) ;
#19473 = DIRECTION ( 'NONE',  ( -0.5516667872527448724, 0.8340645993220398013, 0.000000000000000000 ) ) ;
#19474 = CARTESIAN_POINT ( 'NONE',  ( 44.57981642832929481, 14.36173779840500053, -8.202871819132159459 ) ) ;
#19475 = CARTESIAN_POINT ( 'NONE',  ( 24.04485091158800003, -15.61618876680915236, -45.79233931912149558 ) ) ;
#19476 = CARTESIAN_POINT ( 'NONE',  ( 84.44784216359251161, -43.11618894467930119, -47.47585302082339354 ) ) ;
#19477 = DIRECTION ( 'NONE',  ( -1.000000000000000000, 0.000000000000000000, 0.000000000000000000 ) ) ;
#19478 = CARTESIAN_POINT ( 'NONE',  ( 22.69111796763029787, -10.61757876961529945, -45.30034255656079978 ) ) ;
#19479 = ORIENTED_EDGE ( 'NONE', *, *, #32909, .F. ) ;
#19480 = CARTESIAN_POINT ( 'NONE',  ( 55.48396116477669437, -47.17766655192640002, -26.43082136174480112 ) ) ;
#19481 = CARTESIAN_POINT ( 'NONE',  ( 10.61757787825930066, -64.82569375050010763, -18.17423461342389857 ) ) ;
#19482 = CARTESIAN_POINT ( 'NONE',  ( 75.06396332937768534, -21.88785010825060340, -11.38986195257589884 ) ) ;
#19483 = CARTESIAN_POINT ( 'NONE',  ( 75.41871150549854974, 12.82758396796481470, -13.61662653247154431 ) ) ;
#19484 = DIRECTION ( 'NONE',  ( 0.000000000000000000, 0.000000000000000000, 1.000000000000000000 ) ) ;
#19485 = VECTOR ( 'NONE', #16462, 1000.000000000000000 ) ;
#19486 = CARTESIAN_POINT ( 'NONE',  ( 14.19338055721690139, 1.323206481297250159, -34.90839531524139971 ) ) ;
#19487 = VECTOR ( 'NONE', #13983, 1000.000000000000000 ) ;
#19488 = DIRECTION ( 'NONE',  ( 0.000000000000000000, 0.000000000000000000, -1.000000000000000000 ) ) ;
#19489 = EDGE_CURVE ( 'NONE', #41648, #33306, #3461, .T. ) ;
#19490 = CARTESIAN_POINT ( 'NONE',  ( 30.13393739769619728, 7.383811055320659733, -84.65000000000000568 ) ) ;
#19491 = CARTESIAN_POINT ( 'NONE',  ( 63.40197747243239945, 1.383811055320669947, -62.77400398868049081 ) ) ;
#19492 = CARTESIAN_POINT ( 'NONE',  ( 57.27138006146679317, -50.61618894467930119, -53.91678089496280535 ) ) ;
#19493 = CARTESIAN_POINT ( 'NONE',  ( 41.15934842087519741, 13.27345145488459899, -4.800414586038529663 ) ) ;
#19494 = DIRECTION ( 'NONE',  ( 0.000000000000000000, -0.7071067811865162644, -0.7071067811865786590 ) ) ;
#19495 = CARTESIAN_POINT ( 'NONE',  ( 20.13393739768839552, 24.18330853958629945, -20.65000000000000213 ) ) ;
#19496 = DIRECTION ( 'NONE',  ( 0.4872913772396113563, 0.8732394366197181457, 0.000000000000000000 ) ) ;
#19497 = CARTESIAN_POINT ( 'NONE',  ( 65.43042069957887463, -49.21324915460321137, -75.95351669811965678 ) ) ;
#19498 = ADVANCED_FACE ( 'NONE', ( #3969 ), #29712, .T. ) ;
#19499 = CARTESIAN_POINT ( 'NONE',  ( 68.13393739769658453, -28.80002732851960445, -29.09832030244560741 ) ) ;
#19500 = CARTESIAN_POINT ( 'NONE',  ( 18.01765265267910010, -51.72416169445279621, -75.53980707817230211 ) ) ;
#19501 = CARTESIAN_POINT ( 'NONE',  ( 49.87147262927059899, -45.11618894467940066, -8.489676102032369442 ) ) ;
#19502 = EDGE_CURVE ( 'NONE', #34738, #19, #24621, .T. ) ;
#19503 = CARTESIAN_POINT ( 'NONE',  ( 12.54931810734220043, -9.084941063794440552, -66.40756600056330683 ) ) ;
#19504 = CARTESIAN_POINT ( 'NONE',  ( 68.13393739769618662, -1.166188944679350081, -65.65000000000000568 ) ) ;
#19505 = DIRECTION ( 'NONE',  ( 0.000000000000000000, 0.000000000000000000, -1.000000000000000000 ) ) ;
#19506 = VERTEX_POINT ( 'NONE', #789 ) ;
#19507 = DIRECTION ( 'NONE',  ( 0.000000000000000000, 0.000000000000000000, 1.000000000000000000 ) ) ;
#19508 = CARTESIAN_POINT ( 'NONE',  ( 22.90092240734290385, -15.63158582780186912, -34.45354257009029908 ) ) ;
#19509 = CARTESIAN_POINT ( 'NONE',  ( 72.97487308438059017, 1.330484379554840002, -68.72860478453370092 ) ) ;
#19510 = CARTESIAN_POINT ( 'NONE',  ( 73.24758132965840218, 0.8838110553206759423, -62.51131646858519275 ) ) ;
#19511 = CARTESIAN_POINT ( 'NONE',  ( 12.01177931914589969, -9.122389888939819613, -81.23899999999999011 ) ) ;
#19512 = ORIENTED_EDGE ( 'NONE', *, *, #19095, .F. ) ;
#19513 = CARTESIAN_POINT ( 'NONE',  ( 17.45899407771650047, 21.59920855125570327, -76.12873484255680978 ) ) ;
#19514 = EDGE_LOOP ( 'NONE', ( #41932, #39240, #43954, #48743, #41631, #50269, #16994, #2245 ) ) ;
#19515 = VECTOR ( 'NONE', #267, 1000.000000000000227 ) ;
#19516 = ORIENTED_EDGE ( 'NONE', *, *, #49462, .T. ) ;
#19517 = CARTESIAN_POINT ( 'NONE',  ( 56.66909264166819327, -45.11618894467940066, -15.43624580850259953 ) ) ;
#19518 = CARTESIAN_POINT ( 'NONE',  ( 23.60199757122739683, -15.03637316203499985, -81.23899999999999011 ) ) ;
#19519 = DIRECTION ( 'NONE',  ( 1.000000000000000000, 0.000000000000000000, 0.000000000000000000 ) ) ;
#19520 = ORIENTED_EDGE ( 'NONE', *, *, #28279, .F. ) ;
#19521 = EDGE_CURVE ( 'NONE', #5028, #17403, #21215, .T. ) ;
#19522 = CARTESIAN_POINT ( 'NONE',  ( 24.04500464303940888, -15.61618902416171295, -53.50766607493442706 ) ) ;
#19523 = VERTEX_POINT ( 'NONE', #5001 ) ;
#19524 = CARTESIAN_POINT ( 'NONE',  ( 82.34864690492790373, 14.40950277491920772, -47.72348187592567115 ) ) ;
#19525 = AXIS2_PLACEMENT_3D ( 'NONE', #34510, #5974, #46079 ) ;
#19526 = CARTESIAN_POINT ( 'NONE',  ( 45.25735649856909504, -33.62123980734720163, -34.70630702260449851 ) ) ;
#19527 = VECTOR ( 'NONE', #33924, 1000.000000000000000 ) ;
#19528 = EDGE_LOOP ( 'NONE', ( #38177, #16169, #44196, #25172 ) ) ;
#19529 = CARTESIAN_POINT ( 'NONE',  ( 8.305413682485042415, -16.92329869104723628, -50.45504831420910108 ) ) ;
#19531 = CARTESIAN_POINT ( 'NONE',  ( 52.03944403422909915, -51.37790098174010467, -75.97489327030881157 ) ) ;
#19530 = AXIS2_PLACEMENT_3D ( 'NONE', #26394, #22466, #38475 ) ;
#19532 = CARTESIAN_POINT ( 'NONE',  ( 60.40062465321539520, 14.52871210431360005, -47.56306476889139390 ) ) ;
#19533 = FACE_OUTER_BOUND ( 'NONE', #24226, .T. ) ;
#19534 = CARTESIAN_POINT ( 'NONE',  ( 18.13393739769639978, 10.38381105532070059, -35.14999999999999858 ) ) ;
#19535 = CARTESIAN_POINT ( 'NONE',  ( -6.423395424222389849, 15.09401038596259959, -5.304779371069330729 ) ) ;
#19536 = DIRECTION ( 'NONE',  ( 1.000000000000000000, 0.000000000000000000, 0.000000000000000000 ) ) ;
#19537 = DIRECTION ( 'NONE',  ( 1.062456999999999985E-16, -7.719205000000000365E-17, 1.000000000000000000 ) ) ;
#19538 = CARTESIAN_POINT ( 'NONE',  ( 14.50756117850610138, -23.29353539881530111, -55.85395427856200001 ) ) ;
#19539 = ORIENTED_EDGE ( 'NONE', *, *, #30916, .F. ) ;
#19540 = CARTESIAN_POINT ( 'NONE',  ( 56.53717807884549984, 16.48612042830059821, -47.91220710008310135 ) ) ;
#19541 = CIRCLE ( 'NONE', #9502, 5.499999999999998224 ) ;
#19542 = CARTESIAN_POINT ( 'NONE',  ( 44.00679900668159661, 14.83686777303820037, -8.295979038165928188 ) ) ;
#19543 = FACE_OUTER_BOUND ( 'NONE', #48788, .T. ) ;
#19544 = CARTESIAN_POINT ( 'NONE',  ( 42.57739974420819351, -39.82473145808468473, -73.54253346003443426 ) ) ;
#19545 = FACE_OUTER_BOUND ( 'NONE', #43748, .T. ) ;
#19546 = FILL_AREA_STYLE ('',( #27915 ) ) ;
#19547 = FACE_OUTER_BOUND ( 'NONE', #33427, .T. ) ;
#19548 = DIRECTION ( 'NONE',  ( 0.000000000000000000, 0.000000000000000000, 1.000000000000000000 ) ) ;
#19549 = CARTESIAN_POINT ( 'NONE',  ( 48.58883753202030675, -54.12974218542010618, -55.21967372154079357 ) ) ;
#19550 = CARTESIAN_POINT ( 'NONE',  ( 23.62715585835232091, -12.99531037559654401, -45.40052716342902528 ) ) ;
#19551 = EDGE_CURVE ( 'NONE', #44765, #235, #12848, .T. ) ;
#19552 = CARTESIAN_POINT ( 'NONE',  ( 13.13393739769619906, -49.61618894467939356, -35.14999999999999858 ) ) ;
#19553 = CARTESIAN_POINT ( 'NONE',  ( 9.807847918142682531, -20.47796416623571858, -38.29933577761543262 ) ) ;
#19554 = CARTESIAN_POINT ( 'NONE',  ( 47.87778036368489865, 23.16084776458309946, -54.84373880101900056 ) ) ;
#19555 = EDGE_CURVE ( 'NONE', #29700, #4830, #41059, .T. ) ;
#19556 = ORIENTED_EDGE ( 'NONE', *, *, #25510, .T. ) ;
#19557 = AXIS2_PLACEMENT_3D ( 'NONE', #16935, #49175, #20837 ) ;
#19558 = CARTESIAN_POINT ( 'NONE',  ( 22.32658188330890070, -19.75839229714189926, -37.25499936915149135 ) ) ;
#19559 = CARTESIAN_POINT ( 'NONE',  ( 7.517033938252880354, 30.35161808146150264, -19.14999999999999858 ) ) ;
#19560 = VECTOR ( 'NONE', #19853, 1000.000000000000000 ) ;
#19561 = ORIENTED_EDGE ( 'NONE', *, *, #29835, .F. ) ;
#19562 = CARTESIAN_POINT ( 'NONE',  ( 71.37283554222209148, 1.371509258145880095, -70.32114135108689368 ) ) ;
#19563 = CARTESIAN_POINT ( 'NONE',  ( 60.64942649656659768, -45.57996615352359981, -47.30139731918439594 ) ) ;
#19564 = CARTESIAN_POINT ( 'NONE',  ( 60.23130391296999875, -45.78304229081430066, -47.24246919202539630 ) ) ;
#19565 = DIRECTION ( 'NONE',  ( 1.000000000000000000, 0.000000000000000000, 0.000000000000000000 ) ) ;
#19567 = DIRECTION ( 'NONE',  ( 0.000000000000000000, 0.000000000000000000, -1.000000000000000000 ) ) ;
#19566 = CARTESIAN_POINT ( 'NONE',  ( 83.87142430054399256, 13.62662911754079964, -47.47134017317799959 ) ) ;
#19568 = CARTESIAN_POINT ( 'NONE',  ( 58.16408830537058350, 14.45890994950174147, -26.37137507050323038 ) ) ;
#19569 = CARTESIAN_POINT ( 'NONE',  ( 56.82514454922279867, 19.42926546485919914, -53.84957932253210089 ) ) ;
#19570 = ORIENTED_EDGE ( 'NONE', *, *, #46405, .T. ) ;
#19571 = CARTESIAN_POINT ( 'NONE',  ( 15.29511290902269849, 12.56821928479459949, -59.64999999999999147 ) ) ;
#19572 = ORIENTED_EDGE ( 'NONE', *, *, #4669, .F. ) ;
#19573 = VERTEX_POINT ( 'NONE', #22510 ) ;
#19574 = DIRECTION ( 'NONE',  ( 1.000000000000000000, 0.000000000000000000, 0.000000000000000000 ) ) ;
#19575 = CARTESIAN_POINT ( 'NONE',  ( 24.04460491192063998, -15.61619351124008404, -49.79233069347445451 ) ) ;
#19576 = CARTESIAN_POINT ( 'NONE',  ( 76.42344249101890341, -22.54073511903138183, -12.89752473310971403 ) ) ;
#19577 = CARTESIAN_POINT ( 'NONE',  ( 12.89366548528570000, -65.51121853336410084, -47.72019435537529830 ) ) ;
#19578 = EDGE_LOOP ( 'NONE', ( #25297, #45843, #8118, #7760 ) ) ;
#19579 = ORIENTED_EDGE ( 'NONE', *, *, #14794, .T. ) ;
#19580 = EDGE_CURVE ( 'NONE', #2407, #43345, #2878, .T. ) ;
#19581 = CARTESIAN_POINT ( 'NONE',  ( -19.56713115153528904, 0.1666088194093528763, -52.04600499236246947 ) ) ;
#19582 = CARTESIAN_POINT ( 'NONE',  ( 56.33033006273769416, -50.66288601196639974, -53.07632196026260374 ) ) ;
#19583 = AXIS2_PLACEMENT_3D ( 'NONE', #36650, #9154, #29309 ) ;
#19584 = CARTESIAN_POINT ( 'NONE',  ( 11.90533122472848149, -10.27749421695417986, -45.73977238055704220 ) ) ;
#19585 = EDGE_CURVE ( 'NONE', #28389, #42488, #38258, .T. ) ;
#19586 = CARTESIAN_POINT ( 'NONE',  ( 61.33519241402679967, -0.8007228105548149788, -16.23036785962110073 ) ) ;
#19587 = CARTESIAN_POINT ( 'NONE',  ( 51.78350021394049918, -49.14267277433249603, -77.04630018407770820 ) ) ;
#19588 = DIRECTION ( 'NONE',  ( 0.8133188816852265912, 0.000000000000000000, 0.5818181818182487364 ) ) ;
#19589 = VERTEX_POINT ( 'NONE', #18325 ) ;
#19590 = DIRECTION ( 'NONE',  ( 0.000000000000000000, 0.000000000000000000, -1.000000000000000000 ) ) ;
#19591 = DIRECTION ( 'NONE',  ( 0.000000000000000000, -1.000000000000000000, 0.000000000000000000 ) ) ;
#19592 = CARTESIAN_POINT ( 'NONE',  ( 12.72379725809246587, -9.735079474130024835, -33.78566920041453159 ) ) ;
#19593 = DIRECTION ( 'NONE',  ( 0.5112408204145791890, -0.8594375041513071523, 0.000000000000000000 ) ) ;
#19594 = CARTESIAN_POINT ( 'NONE',  ( 8.572820610417089426, -13.51469887315669993, -53.09878558187529052 ) ) ;
#19595 = CARTESIAN_POINT ( 'NONE',  ( 12.53567562190739970, -49.97757163118789947, -21.12174283171160027 ) ) ;
#19596 = CARTESIAN_POINT ( 'NONE',  ( 56.64426558924419908, 19.38381105532069881, -75.54079041445969267 ) ) ;
#19597 = AXIS2_PLACEMENT_3D ( 'NONE', #45145, #25460, #17875 ) ;
#19598 = LINE ( 'NONE', #22996, #15910 ) ;
#19599 = CARTESIAN_POINT ( 'NONE',  ( -0.03447620312153643757, -27.09132598751343579, -34.79644660940672907 ) ) ;
#19600 = CARTESIAN_POINT ( 'NONE',  ( 8.897806153503289295, 18.01372606128879639, -34.65445009297679491 ) ) ;
#19601 = AXIS2_PLACEMENT_3D ( 'NONE', #4146, #12277, #29277 ) ;
#19602 = CARTESIAN_POINT ( 'NONE',  ( 9.366950684753225786, -16.50208444525215867, -39.41115367992199481 ) ) ;
#19603 = CARTESIAN_POINT ( 'NONE',  ( 16.05499536011179984, -8.563790251386850017, -50.34361688518850286 ) ) ;
#19604 = DIRECTION ( 'NONE',  ( -1.000000000000000000, 0.000000000000000000, 0.000000000000000000 ) ) ;
#19605 = ORIENTED_EDGE ( 'NONE', *, *, #44531, .T. ) ;
#19606 = CARTESIAN_POINT ( 'NONE',  ( 13.94115515399420069, -51.19324711185789312, -74.36773579016251290 ) ) ;
#19607 = CARTESIAN_POINT ( 'NONE',  ( 65.05904174327510248, 1.369885150286779929, -60.91305399111080021 ) ) ;
#19608 = CARTESIAN_POINT ( 'NONE',  ( 42.16682223010890596, -45.82892464120780573, -6.952852404606489678 ) ) ;
#19609 = DIRECTION ( 'NONE',  ( 1.000000000000000000, 2.460964292799963328E-14, 0.000000000000000000 ) ) ;
#19610 = CARTESIAN_POINT ( 'NONE',  ( 24.04461900158476340, -15.61617122039998051, -49.50766513674645353 ) ) ;
#19611 = CARTESIAN_POINT ( 'NONE',  ( 11.97520979020713128, -10.20491147569583923, -75.74446850450661373 ) ) ;
#19612 = CARTESIAN_POINT ( 'NONE',  ( 11.89339496836129939, 34.20366452798109691, -18.15362147985830177 ) ) ;
#19613 = CIRCLE ( 'NONE', #3740, 16.00000000000000000 ) ;
#19614 = CARTESIAN_POINT ( 'NONE',  ( 8.943569970476479725, 18.10127401595480023, -34.64999999999999858 ) ) ;
#19616 = CARTESIAN_POINT ( 'NONE',  ( 43.91162071577659987, -37.84375841978030053, -70.75826489186619028 ) ) ;
#19615 = CARTESIAN_POINT ( 'NONE',  ( 52.38380668138933771, 18.65349054039470644, -77.22917124323686267 ) ) ;
#19617 = ADVANCED_FACE ( 'NONE', ( #14922 ), #51833, .T. ) ;
#19618 = CYLINDRICAL_SURFACE ( 'NONE', #14188, 3.000000000000005773 ) ;
#19619 = DIRECTION ( 'NONE',  ( 1.000000000000000000, 0.000000000000000000, 0.000000000000000000 ) ) ;
#19620 = CARTESIAN_POINT ( 'NONE',  ( 49.42204313923240022, 22.28165337735409679, -54.19389682688740351 ) ) ;
#19621 = ORIENTED_EDGE ( 'NONE', *, *, #2313, .T. ) ;
#19622 = CARTESIAN_POINT ( 'NONE',  ( 53.31858331305709697, -49.44472013427339618, -49.05455764246600125 ) ) ;
#19623 = ORIENTED_EDGE ( 'NONE', *, *, #12966, .T. ) ;
#19624 = CARTESIAN_POINT ( 'NONE',  ( 44.22423880582511657, 7.784288628886946171, -69.62787953467274349 ) ) ;
#19625 = DIRECTION ( 'NONE',  ( 0.000000000000000000, 0.000000000000000000, -1.000000000000000000 ) ) ;
#19626 = CARTESIAN_POINT ( 'NONE',  ( 16.13393739769620083, -45.61618894467940066, -59.64999999999999147 ) ) ;
#19627 = CARTESIAN_POINT ( 'NONE',  ( 51.78349586844800001, -49.14267421975780081, -77.04629326711500426 ) ) ;
#19628 = CARTESIAN_POINT ( 'NONE',  ( 23.05415186443769926, -14.25486957328740090, -56.39099290546759846 ) ) ;
#19629 = CIRCLE ( 'NONE', #48942, 2.999999999999997780 ) ;
#19630 = CARTESIAN_POINT ( 'NONE',  ( 53.41952757764659765, 18.23162460577420063, -49.21226385651820578 ) ) ;
#19631 = CARTESIAN_POINT ( 'NONE',  ( 54.99585155449699414, -45.33621571906800085, -15.06529551545699874 ) ) ;
#19632 = CARTESIAN_POINT ( 'NONE',  ( 53.63393739769619373, 30.88381105532059934, 10.84999999999999964 ) ) ;
#19633 = ORIENTED_EDGE ( 'NONE', *, *, #8583, .T. ) ;
#19634 = AXIS2_PLACEMENT_3D ( 'NONE', #11953, #27908, #23959 ) ;
#19635 = CARTESIAN_POINT ( 'NONE',  ( 8.657171726495921149, -18.00045471869519886, -46.18924468880049972 ) ) ;
#19636 = ORIENTED_EDGE ( 'NONE', *, *, #2822, .T. ) ;
#19637 = CARTESIAN_POINT ( 'NONE',  ( 11.93810467663310071, -65.43945453151620484, -17.87564855520800222 ) ) ;
#19638 = CARTESIAN_POINT ( 'NONE',  ( 10.38317543238860097, 32.50360296011269412, -45.89016348143990598 ) ) ;
#19639 = CARTESIAN_POINT ( 'NONE',  ( 73.07317914023670369, 1.000225705806889964, -62.25573873525459589 ) ) ;
#19640 = CARTESIAN_POINT ( 'NONE',  ( 48.42505861925889832, -54.27772236143609774, -55.06615293675599787 ) ) ;
#19641 = CARTESIAN_POINT ( 'NONE',  ( 11.61157517248314441, -65.37040442588083522, -22.53770969513777800 ) ) ;
#19642 = CARTESIAN_POINT ( 'NONE',  ( -18.86606260230390220, 24.88381105532059934, 11.34999999999999964 ) ) ;
#19643 = VERTEX_POINT ( 'NONE', #45027 ) ;
#19644 = CARTESIAN_POINT ( 'NONE',  ( 64.76223432283450165, 1.187296498006430001, -70.50955232519169158 ) ) ;
#19645 = CARTESIAN_POINT ( 'NONE',  ( 11.13393739769619906, -63.26135015252509675, -43.91418615158710281 ) ) ;
#19646 = DIRECTION ( 'NONE',  ( 1.000000000000000000, 2.460964292799963328E-14, 0.000000000000000000 ) ) ;
#19647 = VERTEX_POINT ( 'NONE', #24822 ) ;
#19648 = EDGE_CURVE ( 'NONE', #29295, #16677, #728, .T. ) ;
#19649 = CARTESIAN_POINT ( 'NONE',  ( 23.62342291817649809, -48.75768716228870403, -35.10565360069929852 ) ) ;
#19650 = CARTESIAN_POINT ( 'NONE',  ( 56.87927060707500004, 19.41808733271159682, -53.72034555577639736 ) ) ;
#19651 = DIRECTION ( 'NONE',  ( 0.000000000000000000, 0.000000000000000000, -1.000000000000000000 ) ) ;
#19652 = EDGE_LOOP ( 'NONE', ( #11098, #8036, #14871, #43507 ) ) ;
#19653 = CARTESIAN_POINT ( 'NONE',  ( 9.807770640268937967, -20.47786500802574849, -36.29933452872364796 ) ) ;
#19654 = DIRECTION ( 'NONE',  ( 0.000000000000000000, 0.000000000000000000, 1.000000000000000000 ) ) ;
#19655 = DIRECTION ( 'NONE',  ( 0.000000000000000000, 0.000000000000000000, -1.000000000000000000 ) ) ;
#19656 = CARTESIAN_POINT ( 'NONE',  ( 9.366931599644679807, -15.61636246440640008, -63.84717978381009118 ) ) ;
#19657 = CARTESIAN_POINT ( 'NONE',  ( 7.988116397819459813, -14.34013240443429993, -72.84179330725640966 ) ) ;
#19658 = TOROIDAL_SURFACE ( 'NONE', #36359, 34.55616290057869833, 2.000000000000000000 ) ;
#19659 = CARTESIAN_POINT ( 'NONE',  ( 68.13393739769620083, 0.8838110553206759423, -65.65000000000000568 ) ) ;
#19660 = CARTESIAN_POINT ( 'NONE',  ( 88.13393739769618662, -1.666188944679350081, -65.65000000000000568 ) ) ;
#19661 = ITEM_DEFINED_TRANSFORMATION ( 'NONE', 'NONE', #23463,  #20940 ) ;
#19662 = EDGE_LOOP ( 'NONE', ( #40608, #32910, #7348, #24645 ) ) ;
#19663 = ORIENTED_EDGE ( 'NONE', *, *, #31561, .T. ) ;
#19664 = CARTESIAN_POINT ( 'NONE',  ( 13.49502580069180091, -8.648919796128959447, -63.61740952279680528 ) ) ;
#19665 = DIRECTION ( 'NONE',  ( 0.5685928097855377228, -0.5944782866685527356, -0.5685928097855347252 ) ) ;
#19666 = DIRECTION ( 'NONE',  ( 0.000000000000000000, 0.000000000000000000, -1.000000000000000000 ) ) ;
#19667 = CARTESIAN_POINT ( 'NONE',  ( 46.37109089150850139, 21.71592500402280024, -76.14999999999999147 ) ) ;
#19668 = CARTESIAN_POINT ( 'NONE',  ( 61.58747524351382197, 14.05432104330237308, -47.18566752083825833 ) ) ;
#19669 = CARTESIAN_POINT ( 'NONE',  ( 68.13393739769649926, -48.11618894468163887, -75.95000000000023022 ) ) ;
#19670 = CARTESIAN_POINT ( 'NONE',  ( 12.12214211478229942, 33.82440024855289806, -16.43788246314790058 ) ) ;
#19671 = CARTESIAN_POINT ( 'NONE',  ( 24.29887580492210120, -14.46879994560240057, -77.46322856839019266 ) ) ;
#19672 = CARTESIAN_POINT ( 'NONE',  ( 53.87584899166630237, -48.41195041224410289, -26.23515327084989934 ) ) ;
#19673 = CARTESIAN_POINT ( 'NONE',  ( 55.96492549803009808, -50.64339188080709420, -75.67011080619238328 ) ) ;
#19675 = FACE_OUTER_BOUND ( 'NONE', #49896, .T. ) ;
#19674 = CARTESIAN_POINT ( 'NONE',  ( -11.30855951853859942, 10.63123909960889968, -5.947173849478319951 ) ) ;
#19676 = EDGE_CURVE ( 'NONE', #45486, #20296, #3604, .T. ) ;
#19677 = CARTESIAN_POINT ( 'NONE',  ( 63.36863247553639411, 1.371651820402789879, -68.64970267437179530 ) ) ;
#19678 = CARTESIAN_POINT ( 'NONE',  ( 61.19582091169579741, 14.04751127219729945, -46.80238762625980087 ) ) ;
#19679 = CARTESIAN_POINT ( 'NONE',  ( 22.37268434111610205, 22.37603658786960281, -34.64999999999999858 ) ) ;
#19680 = CYLINDRICAL_SURFACE ( 'NONE', #43187, 1.999999999999997780 ) ;
#19681 = EDGE_CURVE ( 'NONE', #27937, #7583, #4203, .T. ) ;
#19682 = VERTEX_POINT ( 'NONE', #13078 ) ;
#19683 =( BOUNDED_CURVE ( )  B_SPLINE_CURVE ( 2, ( #23623, #23877, #31739 ),
 .UNSPECIFIED., .F., .T. ) 
 B_SPLINE_CURVE_WITH_KNOTS ( ( 3, 3 ),
 ( 2.734699209162410050, 5.217679283405229462 ),
 .UNSPECIFIED. ) 
 CURVE ( )  GEOMETRIC_REPRESENTATION_ITEM ( )  RATIONAL_B_SPLINE_CURVE ( ( 1.032581180562790024, 1.032237589135679867, 1.004410800606350129 ) ) 
 REPRESENTATION_ITEM ( '' )  );
#19684 = CARTESIAN_POINT ( 'NONE',  ( 52.90228699065409756, -49.62291960146570347, -48.72753553419400419 ) ) ;
#19685 = ADVANCED_FACE ( 'NONE', ( #5205 ), #4930, .T. ) ;
#19686 = CARTESIAN_POINT ( 'NONE',  ( 47.70131400676309852, 23.24817081282549935, -54.82001053506050425 ) ) ;
#19687 = CARTESIAN_POINT ( 'NONE',  ( 57.59318069304929821, -45.71254049200430103, -26.27850964665099909 ) ) ;
#19688 = LINE ( 'NONE', #536, #18487 ) ;
#19689 = CARTESIAN_POINT ( 'NONE',  ( 61.43319361452919480, 14.21598701041570045, -47.47819310727240349 ) ) ;
#19690 = CARTESIAN_POINT ( 'NONE',  ( 8.968719396631879448, -17.65735158387520087, -79.14432001126618843 ) ) ;
#19691 = ADVANCED_FACE ( 'NONE', ( #40831, #41094 ), #25344, .T. ) ;
#19692 = CARTESIAN_POINT ( 'NONE',  ( 51.97623849038839694, 18.77915525888139925, -76.70088623176620501 ) ) ;
#19693 = CARTESIAN_POINT ( 'NONE',  ( 52.91697747311700084, 18.38500394665459936, -48.80601309169850310 ) ) ;
#19694 = CARTESIAN_POINT ( 'NONE',  ( 0.2019507440921959052, -4.548421796940673723, -34.66067286864801389 ) ) ;
#19695 = CARTESIAN_POINT ( 'NONE',  ( 22.90093739769620029, -15.61618894467913243, -28.45282021618999835 ) ) ;
#19696 = AXIS2_PLACEMENT_3D ( 'NONE', #17042, #44815, #28814 ) ;
#19697 = VERTEX_POINT ( 'NONE', #28764 ) ;
#19698 = CARTESIAN_POINT ( 'NONE',  ( 22.90034302961675294, -15.71306413766174614, -40.45738043218361213 ) ) ;
#19699 = CARTESIAN_POINT ( 'NONE',  ( 47.64889676501250193, -54.52888567683150001, -55.03601200310530572 ) ) ;
#19700 = CARTESIAN_POINT ( 'NONE',  ( 28.63393739769619728, -4.678675331415849570, -34.64999999999999858 ) ) ;
#19701 = CARTESIAN_POINT ( 'NONE',  ( 29.13393739769620083, -15.61618894467929941, -6.189999999999999503 ) ) ;
#19702 = CARTESIAN_POINT ( 'NONE',  ( 61.34707231617679923, -30.42972915830750225, -16.23350102184249621 ) ) ;
#19703 = CARTESIAN_POINT ( 'NONE',  ( 71.37757697660960332, 1.096291039689149871, -60.65158056017160249 ) ) ;
#19704 = DIRECTION ( 'NONE',  ( 1.000000000000000000, 2.460964292799963328E-14, 0.000000000000000000 ) ) ;
#19705 = CARTESIAN_POINT ( 'NONE',  ( 72.61824171362239611, 1.332297898505919953, -61.86173543814949483 ) ) ;
#19706 = EDGE_CURVE ( 'NONE', #11854, #1665, #36367, .T. ) ;
#19707 = CARTESIAN_POINT ( 'NONE',  ( 51.49832567296675734, -34.30705569774075059, -76.79133718297113376 ) ) ;
#19708 = CARTESIAN_POINT ( 'NONE',  ( 13.73800010538356453, -9.266389088679069630, -65.83795360124345564 ) ) ;
#19709 = ORIENTED_EDGE ( 'NONE', *, *, #39039, .T. ) ;
#19710 = ORIENTED_EDGE ( 'NONE', *, *, #18831, .T. ) ;
#19711 = CARTESIAN_POINT ( 'NONE',  ( 9.205734167420699166, -27.61618894467930119, -32.14999999999999858 ) ) ;
#19712 = CARTESIAN_POINT ( 'NONE',  ( 49.97510569688304116, -29.81569084455778906, -15.94715247223231458 ) ) ;
#19713 = ORIENTED_EDGE ( 'NONE', *, *, #13849, .F. ) ;
#19714 = EDGE_CURVE ( 'NONE', #4357, #47961, #16999, .T. ) ;
#19715 = DIRECTION ( 'NONE',  ( -0.4999999999999998890, -0.8660254037844387076, 0.000000000000000000 ) ) ;
#19716 = CARTESIAN_POINT ( 'NONE',  ( 16.10561099735067714, -23.52714547073744100, -78.00881095716772506 ) ) ;
#19717 = ORIENTED_EDGE ( 'NONE', *, *, #22457, .F. ) ;
#19718 = CARTESIAN_POINT ( 'NONE',  ( 15.58086402661377257, -22.40678867047189726, -80.97851386839785448 ) ) ;
#19719 = CARTESIAN_POINT ( 'NONE',  ( 45.08397438503814669, 6.820184756207779309, -64.89981427032263639 ) ) ;
#19720 = CARTESIAN_POINT ( 'NONE',  ( 12.91816786240429948, 34.28039554897920027, -23.43576497212680110 ) ) ;
#19721 = CARTESIAN_POINT ( 'NONE',  ( 24.01926528025970242, -18.02540546471280081, -39.88671798479069963 ) ) ;
#19722 = FACE_BOUND ( 'NONE', #50195, .T. ) ;
#19723 = CARTESIAN_POINT ( 'NONE',  ( 11.05733698530690745, -21.71889251823660771, -50.51310250095467325 ) ) ;
#19724 = CARTESIAN_POINT ( 'NONE',  ( 64.62455173613830084, -30.85405543856260024, -16.65869106914230358 ) ) ;
#19725 = DIRECTION ( 'NONE',  ( -1.000000000000000000, 0.000000000000000000, 0.000000000000000000 ) ) ;
#19726 = CARTESIAN_POINT ( 'NONE',  ( 15.77765653362640030, -23.45581977383699979, -70.52695041587149660 ) ) ;
#19727 = CARTESIAN_POINT ( 'NONE',  ( 55.57908331551900005, 14.75265853258540183, -16.80478259867470214 ) ) ;
#19728 = EDGE_CURVE ( 'NONE', #7973, #40265, #1090, .T. ) ;
#19729 = AXIS2_PLACEMENT_3D ( 'NONE', #17489, #38181, #37922 ) ;
#19730 = CARTESIAN_POINT ( 'NONE',  ( 44.12345869187539904, 14.36007666331510002, -7.915795181119260171 ) ) ;
#19731 = CIRCLE ( 'NONE', #4644, 3.076499999999999346 ) ;
#19732 = CARTESIAN_POINT ( 'NONE',  ( 14.98451991090269964, 21.70396400196510100, -76.14999999999999147 ) ) ;
#19733 = CARTESIAN_POINT ( 'NONE',  ( 84.23484834998549786, -43.81302277605040274, -47.06355581890329631 ) ) ;
#19734 = DIRECTION ( 'NONE',  ( 1.000000000000000000, 2.460964292799963328E-14, 0.000000000000000000 ) ) ;
#19735 = CARTESIAN_POINT ( 'NONE',  ( 7.952298879402861509, -14.59466465962590043, -40.54720669274369982 ) ) ;
#19736 = VERTEX_POINT ( 'NONE', #21415 ) ;
#19737 = DIRECTION ( 'NONE',  ( 0.000000000000000000, 0.000000000000000000, -1.000000000000000000 ) ) ;
#19738 = CARTESIAN_POINT ( 'NONE',  ( 11.30323766776139927, -63.48480417437669843, -14.81980353719009891 ) ) ;
#19739 = CARTESIAN_POINT ( 'NONE',  ( 50.69188217665702467, -35.76023418930356002, -76.26103740547989673 ) ) ;
#19740 = CARTESIAN_POINT ( 'NONE',  ( 61.73642047736571925, -45.13062725877497172, -46.64902933540918184 ) ) ;
#19741 = CARTESIAN_POINT ( 'NONE',  ( 13.61751436261749859, -50.16766668102790305, -20.94898426700639860 ) ) ;
#19742 = ORIENTED_EDGE ( 'NONE', *, *, #9163, .T. ) ;
#19743 = CARTESIAN_POINT ( 'NONE',  ( -4.095824978346090717, -48.17436604277430234, -5.432754358006550710 ) ) ;
#19744 = CARTESIAN_POINT ( 'NONE',  ( 9.221463679254590318, -19.60040485680393729, -38.62566536316489874 ) ) ;
#19745 = AXIS2_PLACEMENT_3D ( 'NONE', #7018, #51031, #38990 ) ;
#19746 = CARTESIAN_POINT ( 'NONE',  ( 14.64034768018736798, 18.38379310215821505, -83.19069868277145474 ) ) ;
#19747 = CARTESIAN_POINT ( 'NONE',  ( 63.18711801607420142, 1.188042061556800144, -62.42534911081870064 ) ) ;
#19748 = CARTESIAN_POINT ( 'NONE',  ( 57.55751162060460047, -50.29421797927160043, -52.83558909277360272 ) ) ;
#19749 = CARTESIAN_POINT ( 'NONE',  ( 43.13712996753829998, 11.78398668836219976, -4.491635650878129660 ) ) ;
#19750 = ADVANCED_FACE ( 'NONE', ( #40570 ), #49230, .T. ) ;
#19751 = CARTESIAN_POINT ( 'NONE',  ( 23.83903639717342671, -13.54550718029785905, -61.70899533148040206 ) ) ;
#19752 = CARTESIAN_POINT ( 'NONE',  ( 74.93037156228848517, -45.11618894467250129, -15.31097063366330069 ) ) ;
#19753 = CARTESIAN_POINT ( 'NONE',  ( 59.83314911148339377, -45.99164674684980270, -47.38390679353289414 ) ) ;
#19754 = CONICAL_SURFACE ( 'NONE', #14748, 0.6299999999999942313, 0.7853981633974476129 ) ;
#19755 = CARTESIAN_POINT ( 'NONE',  ( 17.16940049168541549, -7.705176891496546610, -75.33404972303934244 ) ) ;
#19756 = CARTESIAN_POINT ( 'NONE',  ( 10.22099471833763396, -19.02412705075455790, -63.28615105807855201 ) ) ;
#19757 = CARTESIAN_POINT ( 'NONE',  ( 17.21347160910390173, -53.11618894467930119, -76.14999999999999147 ) ) ;
#19758 = B_SPLINE_CURVE_WITH_KNOTS ( 'NONE', 3,
 ( #4335, #36554, #33131, #32344, #48363, #12460, #24480, #16642, #48630, #49157, #26565, #33908, #21858, #34689, #46779, #13761, #42056, #1963 ),
 .UNSPECIFIED., .F., .F.,
 ( 4, 2, 2, 2, 2, 2, 2, 2, 4 ),
 ( 0.000000000000000000, 0.06250017132677161691, 0.1250003426535432338, 0.1875005139803148646, 0.2500006853070864676, 0.3125008566338578486, 0.3750010279606292851, 0.4375011992874006661, 0.5000013706141720471 ),
 .UNSPECIFIED. ) ;
#19759 = CARTESIAN_POINT ( 'NONE',  ( 15.61994416393740082, -8.183658736601330475, -60.54536510185550213 ) ) ;
#19760 = FACE_OUTER_BOUND ( 'NONE', #34366, .T. ) ;
#19761 = PLANE ( 'NONE',  #33304 ) ;
#19762 = VERTEX_POINT ( 'NONE', #29285 ) ;
#19763 = CARTESIAN_POINT ( 'NONE',  ( 45.90333292994009184, 13.88381105525539994, -7.776728755756193046 ) ) ;
#19764 = CARTESIAN_POINT ( 'NONE',  ( 9.447966713677070416, -16.81209814564785177, -35.39653371675596105 ) ) ;
#19765 = CARTESIAN_POINT ( 'NONE',  ( 72.87088340658550578, 1.369885150286800135, -68.72489565442110404 ) ) ;
#19766 = CYLINDRICAL_SURFACE ( 'NONE', #11476, 2.576499999999998902 ) ;
#19767 = VECTOR ( 'NONE', #21408, 999.9999999999998863 ) ;
#19768 = EDGE_CURVE ( 'NONE', #44451, #25228, #1517, .T. ) ;
#19769 = CARTESIAN_POINT ( 'NONE',  ( 9.059951416200188845, -13.96889917543390069, -81.23899999999999011 ) ) ;
#19770 = ORIENTED_EDGE ( 'NONE', *, *, #30369, .F. ) ;
#19771 = CARTESIAN_POINT ( 'NONE',  ( 17.27854763127069759, 21.70054973260339892, -76.14999999999999147 ) ) ;
#19772 = AXIS2_PLACEMENT_3D ( 'NONE', #50188, #6946, #18719 ) ;
#19773 = EDGE_LOOP ( 'NONE', ( #4048, #20695, #39391, #44326 ) ) ;
#19774 = ORIENTED_EDGE ( 'NONE', *, *, #36951, .F. ) ;
#19775 = EDGE_CURVE ( 'NONE', #41037, #5215, #4825, .T. ) ;
#19776 = CARTESIAN_POINT ( 'NONE',  ( 8.643872352928719138, 17.52418497763089889, -35.12503119152809461 ) ) ;
#19777 = CARTESIAN_POINT ( 'NONE',  ( 23.48321685645310097, -16.39228337977660033, -81.23899999999999011 ) ) ;
#19778 = ORIENTED_EDGE ( 'NONE', *, *, #40805, .F. ) ;
#19779 = ORIENTED_EDGE ( 'NONE', *, *, #39396, .T. ) ;
#19780 = DIRECTION ( 'NONE',  ( 0.000000000000000000, 0.000000000000000000, 1.000000000000000000 ) ) ;
#19781 = DIRECTION ( 'NONE',  ( 1.000000000000000000, 0.000000000000000000, -1.224646799147353207E-16 ) ) ;
#19782 = ORIENTED_EDGE ( 'NONE', *, *, #37789, .T. ) ;
#19783 = ORIENTED_EDGE ( 'NONE', *, *, #2141, .F. ) ;
#19784 = CARTESIAN_POINT ( 'NONE',  ( 68.13393739769620083, 18.13381105532069881, -67.99999999999998579 ) ) ;
#19785 = DIRECTION ( 'NONE',  ( 0.1960104533864304444, -0.03282462862514614471, 0.9800522669321607427 ) ) ;
#19786 = CARTESIAN_POINT ( 'NONE',  ( 61.34213663493859769, 14.32983721081379969, -47.63657398781069929 ) ) ;
#19787 = AXIS2_PLACEMENT_3D ( 'NONE', #23518, #30873, #38774 ) ;
#19788 = EDGE_CURVE ( 'NONE', #13020, #11637, #32027, .T. ) ;
#19789 = CONICAL_SURFACE ( 'NONE', #41524, 12.92820323027549989, 0.7481802937784480800 ) ;
#19790 = EDGE_CURVE ( 'NONE', #46911, #49915, #4481, .T. ) ;
#19791 = DIRECTION ( 'NONE',  ( 1.000000000000000000, 0.000000000000000000, 0.000000000000000000 ) ) ;
#19792 = CARTESIAN_POINT ( 'NONE',  ( 42.78018059632909598, -42.70905810753730236, -3.187564294433590462 ) ) ;
#19793 = CARTESIAN_POINT ( 'NONE',  ( -8.872901943480378861, 13.06271670022229969, -5.763478819725060376 ) ) ;
#19794 = DIRECTION ( 'NONE',  ( 0.000000000000000000, -1.000000000000000000, 0.000000000000000000 ) ) ;
#19795 = VECTOR ( 'NONE', #2413, 1000.000000000000114 ) ;
#19796 = CARTESIAN_POINT ( 'NONE',  ( 14.72053854714293664, -22.52595470508762077, -39.41140439840920351 ) ) ;
#19797 = CARTESIAN_POINT ( 'NONE',  ( 9.531576907524980768, -11.37406870345459886, -66.46929104108710362 ) ) ;
#19798 = ORIENTED_EDGE ( 'NONE', *, *, #51230, .T. ) ;
#19799 = CIRCLE ( 'NONE', #49930, 36.00000000000000000 ) ;
#19800 = CARTESIAN_POINT ( 'NONE',  ( 41.04960996913820281, 14.26468518160199928, -6.018009378594939562 ) ) ;
#19801 = CARTESIAN_POINT ( 'NONE',  ( 12.91917450912220033, 34.27891870250100226, -47.58062843003349940 ) ) ;
#19802 = CARTESIAN_POINT ( 'NONE',  ( 72.44676906758759571, 1.345243094457279964, -69.65815164399170101 ) ) ;
#19803 = CARTESIAN_POINT ( 'NONE',  ( 43.76496993594255969, -39.93523117063323014, -67.79702779702520843 ) ) ;
#19804 = ADVANCED_FACE ( 'NONE', ( #46591 ), #17754, .F. ) ;
#19805 = SURFACE_SIDE_STYLE ('',( #19293 ) ) ;
#19806 = CARTESIAN_POINT ( 'NONE',  ( -30.36606260230379917, 21.88381105532059934, 17.35000000000000142 ) ) ;
#19807 = ADVANCED_FACE ( 'NONE', ( #50511 ), #26118, .T. ) ;
#19808 = CARTESIAN_POINT ( 'NONE',  ( 16.13393739769620083, -29.47259540523039689, -47.64999999999999858 ) ) ;
#19809 = CARTESIAN_POINT ( 'NONE',  ( 48.52733106884640080, -54.04267712022559778, -54.66955039445610254 ) ) ;
#19810 = CARTESIAN_POINT ( 'NONE',  ( 51.94631124322077653, -32.86688835305900369, -19.08860917923622935 ) ) ;
#19811 = VECTOR ( 'NONE', #23071, 1000.000000000000000 ) ;
#19812 = DIRECTION ( 'NONE',  ( 1.000000000000000000, 0.000000000000000000, 0.000000000000000000 ) ) ;
#19813 = CARTESIAN_POINT ( 'NONE',  ( 12.14975734981553757, -8.703693278909492292, -71.12565168373707536 ) ) ;
#19814 = ORIENTED_EDGE ( 'NONE', *, *, #4891, .T. ) ;
#19815 = CARTESIAN_POINT ( 'NONE',  ( 21.75386501390569904, -10.72506351928820045, -38.83937799042379879 ) ) ;
#19816 = CARTESIAN_POINT ( 'NONE',  ( 64.69709925250680271, 1.229987811083060212, -60.86278414758729838 ) ) ;
#19817 = ORIENTED_EDGE ( 'NONE', *, *, #46241, .F. ) ;
#19818 = CARTESIAN_POINT ( 'NONE',  ( 8.223295469878840080, -15.61636541503349918, -58.79233150823709764 ) ) ;
#19819 = CARTESIAN_POINT ( 'NONE',  ( 60.55103620144870291, -45.67013093256520051, -47.48780874919079764 ) ) ;
#19820 = AXIS2_PLACEMENT_3D ( 'NONE', #45594, #6533, #1824 ) ;
#19821 = CARTESIAN_POINT ( 'NONE',  ( 0.3188076311095680571, -20.69863068615319790, -34.65000336222090027 ) ) ;
#19822 = CARTESIAN_POINT ( 'NONE',  ( -4.162817235437208829, -15.61618894467929763, 7.530187386896120216 ) ) ;
#19824 = DIRECTION ( 'NONE',  ( 0.000000000000000000, 0.000000000000000000, -1.000000000000000000 ) ) ;
#19823 = CARTESIAN_POINT ( 'NONE',  ( 42.10508499193715437, 8.543310626597461876, -75.82482327354601637 ) ) ;
#19825 = CARTESIAN_POINT ( 'NONE',  ( 61.28610861176739633, 13.99802266614350010, -46.37203261889099792 ) ) ;
#19826 = CARTESIAN_POINT ( 'NONE',  ( 22.46012283054650638, -10.75453872237786612, -67.29933293715515674 ) ) ;
#19827 = VERTEX_POINT ( 'NONE', #5708 ) ;
#19828 = CARTESIAN_POINT ( 'NONE',  ( 0.06051628023451229715, 19.81643162424870042, -34.85735264049939985 ) ) ;
#19829 = ORIENTED_EDGE ( 'NONE', *, *, #29048, .T. ) ;
#19830 = CARTESIAN_POINT ( 'NONE',  ( 9.366553929154591174, -16.71943377812493736, -59.79527010610524940 ) ) ;
#19831 = CARTESIAN_POINT ( 'NONE',  ( 68.13393739769618662, -28.80002732851770020, -65.65000000000000568 ) ) ;
#19832 = DIRECTION ( 'NONE',  ( 0.6522074047277948150, -0.2731766849828846100, 0.7071067811865450192 ) ) ;
#19833 = VECTOR ( 'NONE', #37178, 1000.000000000000000 ) ;
#19834 = VERTEX_POINT ( 'NONE', #21925 ) ;
#19835 = DIRECTION ( 'NONE',  ( -0.8660254037844321573, 0.5000000000000111022, 0.000000000000000000 ) ) ;
#19836 = CARTESIAN_POINT ( 'NONE',  ( 56.85665997422760398, -45.22495964200660268, -25.29717091828119990 ) ) ;
#19837 = CARTESIAN_POINT ( 'NONE',  ( 56.47574211739829764, -50.76931576605299767, -53.73401891104529682 ) ) ;
#19838 = CARTESIAN_POINT ( 'NONE',  ( 47.40322300430479885, 23.42336669154508755, -74.14999999999999147 ) ) ;
#19839 = CARTESIAN_POINT ( 'NONE',  ( 59.27809708943870248, -2.630911221516660348, -15.68030308388919991 ) ) ;
#19840 = CARTESIAN_POINT ( 'NONE',  ( 51.55656801642479792, -49.50504146151539686, -76.63870299401109776 ) ) ;
#19841 = CARTESIAN_POINT ( 'NONE',  ( 29.13393739769619728, -35.78776181993320193, -84.63196841427449613 ) ) ;
#19842 = VERTEX_POINT ( 'NONE', #33725 ) ;
#19843 = CARTESIAN_POINT ( 'NONE',  ( 9.026390854478798076, 16.60930999848670098, -54.64999999999999858 ) ) ;
#19844 = CARTESIAN_POINT ( 'NONE',  ( 22.78876382550086532, -14.33000611521636003, -34.39203900008635628 ) ) ;
#19845 = CARTESIAN_POINT ( 'NONE',  ( 68.13393739769620083, -48.11618894467930119, -73.25000000000000000 ) ) ;
#19846 = CARTESIAN_POINT ( 'NONE',  ( 23.96158271707849963, -15.05519309305950060, -51.98972054698459289 ) ) ;
#19847 = EDGE_CURVE ( 'NONE', #49517, #42477, #1989, .T. ) ;
#19848 = CARTESIAN_POINT ( 'NONE',  ( 17.89246938939492182, -41.85765695298068323, -34.70142521051216988 ) ) ;
#19849 = DIRECTION ( 'NONE',  ( 0.000000000000000000, 0.000000000000000000, -1.000000000000000000 ) ) ;
#19850 = ADVANCED_FACE ( 'NONE', ( #50254 ), #32068, .T. ) ;
#19851 = CARTESIAN_POINT ( 'NONE',  ( 11.12718406851114317, -65.21267171038789456, -18.17421237898564357 ) ) ;
#19852 = CARTESIAN_POINT ( 'NONE',  ( 29.34926776287277761, -6.014689412737906693, 5.856814007409659517 ) ) ;
#19853 = DIRECTION ( 'NONE',  ( 0.000000000000000000, 0.000000000000000000, -1.000000000000000000 ) ) ;
#19854 = CARTESIAN_POINT ( 'NONE',  ( 20.48068097648700103, -21.17032068912790166, -51.13580619582469922 ) ) ;
#19855 = CARTESIAN_POINT ( 'NONE',  ( 46.69650754312519325, -39.84281285528089711, -54.54193493916549329 ) ) ;
#19856 = ORIENTED_EDGE ( 'NONE', *, *, #31369, .T. ) ;
#19857 = CARTESIAN_POINT ( 'NONE',  ( 47.29285256804710258, 22.85955254686820126, -75.52284329973508648 ) ) ;
#19858 = CARTESIAN_POINT ( 'NONE',  ( 47.40880866017789685, -54.64074575612490037, -54.64987641489110359 ) ) ;
#19859 = CARTESIAN_POINT ( 'NONE',  ( 11.28331493930094354, 33.98248205778411801, -47.30875510483342339 ) ) ;
#19860 = CARTESIAN_POINT ( 'NONE',  ( 56.31076453717512464, -46.45614141085656001, -26.30375982980395477 ) ) ;
#19861 = CARTESIAN_POINT ( 'NONE',  ( 9.221470195977161666, -11.63196189502579792, -46.67433538954914241 ) ) ;
#19862 = CIRCLE ( 'NONE', #3988, 15.11955878774480233 ) ;
#19863 = DIRECTION ( 'NONE',  ( -0.1961161351381830731, 0.000000000000000000, -0.9805806756909203337 ) ) ;
#19864 = EDGE_CURVE ( 'NONE', #17657, #1082, #12018, .T. ) ;
#19865 = CARTESIAN_POINT ( 'NONE',  ( 10.75976506916620146, 33.73421398272039795, -18.06526995537059932 ) ) ;
#19866 = CARTESIAN_POINT ( 'NONE',  ( 74.23393739769618094, -30.31618894467939995, -65.65000000000000568 ) ) ;
#19868 = CARTESIAN_POINT ( 'NONE',  ( 11.13393739269939964, 32.53943438258615828, -24.14230604835864114 ) ) ;
#19867 = SPHERICAL_SURFACE ( 'NONE', #50786, 2.000000000000000000 ) ;
#19869 = DIRECTION ( 'NONE',  ( 0.000000000000000000, 0.000000000000000000, 1.000000000000000000 ) ) ;
#19870 = CARTESIAN_POINT ( 'NONE',  ( 49.39892223771079927, 22.40179904714300108, -54.43183785437209821 ) ) ;
#19871 = ORIENTED_EDGE ( 'NONE', *, *, #36167, .F. ) ;
#19872 = CARTESIAN_POINT ( 'NONE',  ( 52.91162675532969928, -49.64972226872590255, -48.98817416027189608 ) ) ;
#19873 = ORIENTED_EDGE ( 'NONE', *, *, #50879, .F. ) ;
#19874 = CARTESIAN_POINT ( 'NONE',  ( 41.91430865176237575, 7.521317205359935087, -81.04388926812714544 ) ) ;
#19875 = CARTESIAN_POINT ( 'NONE',  ( 84.13393739769618662, -0.3411889446793609504, -65.65000000000000568 ) ) ;
#19876 = DIRECTION ( 'NONE',  ( -1.000000000000000000, 5.464378949326942347E-15, 0.000000000000000000 ) ) ;
#19877 = CARTESIAN_POINT ( 'NONE',  ( 83.25003658253979211, 13.60998241570020184, -46.59700837026780107 ) ) ;
#19878 = CARTESIAN_POINT ( 'NONE',  ( 12.06803212418919991, -9.853292710710359614, -55.75724145695859590 ) ) ;
#19879 = CARTESIAN_POINT ( 'NONE',  ( 52.77888422556929982, 18.48704073958080230, -48.89378105638989780 ) ) ;
#19880 = CARTESIAN_POINT ( 'NONE',  ( 55.41258925948719849, -45.63128349684820506, -16.01983445647000082 ) ) ;
#19881 = CARTESIAN_POINT ( 'NONE',  ( 53.87546017034450330, 17.18069085124139761, -26.23270880884989964 ) ) ;
#19882 = ORIENTED_EDGE ( 'NONE', *, *, #20385, .T. ) ;
#19883 = CARTESIAN_POINT ( 'NONE',  ( 8.421582175205850618, -17.06750734713569884, -42.22829813561959611 ) ) ;
#19884 = VERTEX_POINT ( 'NONE', #38194 ) ;
#19885 = CARTESIAN_POINT ( 'NONE',  ( 11.31612280585429886, -65.07844770564609860, -16.97569922736749959 ) ) ;
#19886 = CARTESIAN_POINT ( 'NONE',  ( 10.66704074922019885, 32.15531322180049756, -45.39606957910810081 ) ) ;
#19887 = CARTESIAN_POINT ( 'NONE',  ( 72.99790115655470402, 1.264791438333819906, -62.42094564213650187 ) ) ;
#19888 = CARTESIAN_POINT ( 'NONE',  ( 8.222911740864116581, -16.65154857562174229, -40.75066691665454499 ) ) ;
#19889 = CARTESIAN_POINT ( 'NONE',  ( 11.68864222515470708, -65.39868967919012732, -22.45823848831452096 ) ) ;
#19890 = CARTESIAN_POINT ( 'NONE',  ( 9.367435715182674372, -16.15063196774820398, -67.82204709561700895 ) ) ;
#19891 = ORIENTED_EDGE ( 'NONE', *, *, #22875, .F. ) ;
#19892 = LINE ( 'NONE', #28526, #30147 ) ;
#19893 = CARTESIAN_POINT ( 'NONE',  ( 11.10549195505100073, -63.26330928660971153, -44.25128882018109522 ) ) ;
#19894 = CARTESIAN_POINT ( 'NONE',  ( 65.43393739769578588, 16.88381105532129922, -71.50000000000000000 ) ) ;
#19895 = EDGE_LOOP ( 'NONE', ( #25298, #8498, #34975, #26009 ) ) ;
#19896 = DIRECTION ( 'NONE',  ( 0.000000000000000000, 0.000000000000000000, 1.000000000000000000 ) ) ;
#19897 = CARTESIAN_POINT ( 'NONE',  ( 22.02679469870373552, -10.29530854175601640, -77.27397928379470216 ) ) ;
#19898 = CARTESIAN_POINT ( 'NONE',  ( 13.42427360708462913, -51.80630186999076869, -74.54430098197724419 ) ) ;
#19899 = CARTESIAN_POINT ( 'NONE',  ( 19.53423428272744999, -8.449927945536709117, -49.14865470901539624 ) ) ;
#19900 = VERTEX_POINT ( 'NONE', #13828 ) ;
#19901 = PLANE ( 'NONE',  #43382 ) ;
#19902 = DIRECTION ( 'NONE',  ( -1.000000000000000000, -1.006844464268868150E-16, 0.000000000000000000 ) ) ;
#19903 = FACE_OUTER_BOUND ( 'NONE', #36005, .T. ) ;
#19904 = TOROIDAL_SURFACE ( 'NONE', #26595, 17.69999999999999929, 3.799999999999830180 ) ;
#19905 = CARTESIAN_POINT ( 'NONE',  ( 68.13393739769620083, -42.11618894467930119, -60.14999999999999858 ) ) ;
#19906 = CARTESIAN_POINT ( 'NONE',  ( 23.37973582986149879, -11.68158284795669921, -73.63398261789259891 ) ) ;
#19907 = B_SPLINE_CURVE_WITH_KNOTS ( 'NONE', 3,
 ( #47827, #4302, #11932, #31295, #20273, #12430, #36266, #43381, #20017, #27885, #23687, #11670, #43891, #7984, #11416, #23936, #12179, #51500 ),
 .UNSPECIFIED., .F., .F.,
 ( 4, 2, 2, 2, 2, 2, 2, 2, 4 ),
 ( 0.4999999940960141998, 0.5624999948340123623, 0.6249999955720106914, 0.6874999963100087985, 0.7499999970480071276, 0.8124999977860052347, 0.8749999985240035638, 0.9374999992620016709, 1.000000000000000000 ),
 .UNSPECIFIED. ) ;
#19908 = ADVANCED_FACE ( 'NONE', ( #18011 ), #18263, .F. ) ;
#19909 = FACE_OUTER_BOUND ( 'NONE', #8784, .T. ) ;
#19910 = CARTESIAN_POINT ( 'NONE',  ( 57.36123081079020380, 18.90300135422739913, -52.61896059691729732 ) ) ;
#19911 = VECTOR ( 'NONE', #15052, 1000.000000000000000 ) ;
#19912 = ORIENTED_EDGE ( 'NONE', *, *, #680, .F. ) ;
#19913 = CARTESIAN_POINT ( 'NONE',  ( 23.46275231366020364, -16.95602689483970238, -60.29021441812479765 ) ) ;
#19914 = CARTESIAN_POINT ( 'NONE',  ( 9.367509928541279507, -15.61618483373539767, -35.84717978380999881 ) ) ;
#19915 = CARTESIAN_POINT ( 'NONE',  ( -21.86606260230379917, -15.61618894467929408, -19.14999999999999858 ) ) ;
#19916 = CARTESIAN_POINT ( 'NONE',  ( 47.11383090458340206, 23.12040445463469851, -75.35698732394219235 ) ) ;
#19917 = DIRECTION ( 'NONE',  ( 0.000000000000000000, 0.000000000000000000, -1.000000000000000000 ) ) ;
#19918 = B_SPLINE_CURVE_WITH_KNOTS ( 'NONE', 3,
 ( #47098, #39481, #11700, #39729, #23716, #26894, #38968, #51273, #31836, #23199 ),
 .UNSPECIFIED., .F., .F.,
 ( 4, 2, 2, 2, 4 ),
 ( 0.000000000000000000, 0.2500000000000000000, 0.5000000000000000000, 0.7500000000000000000, 1.000000000000000000 ),
 .UNSPECIFIED. ) ;
#19919 = CARTESIAN_POINT ( 'NONE',  ( 54.20961013379049831, 17.70559848872130360, -48.50941760523620161 ) ) ;
#19920 = CARTESIAN_POINT ( 'NONE',  ( 12.21895752911930089, 33.73857836819860267, -16.28177273607870035 ) ) ;
#19921 = CARTESIAN_POINT ( 'NONE',  ( 22.60509562802760186, -20.72567344578009951, -75.72041208499069853 ) ) ;
#19922 = ADVANCED_FACE ( 'NONE', ( #34231 ), #29785, .T. ) ;
#19923 = CARTESIAN_POINT ( 'NONE',  ( 55.83720749917949888, -50.61618650412209774, -76.10769951055490878 ) ) ;
#19925 = DIRECTION ( 'NONE',  ( 0.000000000000000000, 1.000000000000000000, 0.000000000000000000 ) ) ;
#19924 = CARTESIAN_POINT ( 'NONE',  ( 57.55751162087899786, 19.38381105532069881, -53.92796738110899923 ) ) ;
#19927 = EDGE_CURVE ( 'NONE', #14490, #23688, #41301, .T. ) ;
#19926 = CARTESIAN_POINT ( 'NONE',  ( 63.10820510261260097, 1.196343736543249880, -68.73232403594570883 ) ) ;
#19928 = CARTESIAN_POINT ( 'NONE',  ( 61.55709258699470610, 13.90898581735810069, -46.56616023981329988 ) ) ;
#19929 = CARTESIAN_POINT ( 'NONE',  ( 67.20199456633832824, -1.235504130748810159, -17.36203811242808470 ) ) ;
#19930 = VERTEX_POINT ( 'NONE', #30569 ) ;
#19931 = CARTESIAN_POINT ( 'NONE',  ( 52.79307622657449883, -49.68079306134869455, -48.47378032971909789 ) ) ;
#19932 = AXIS2_PLACEMENT_3D ( 'NONE', #15151, #39518, #22988 ) ;
#19933 = CARTESIAN_POINT ( 'NONE',  ( 60.90224615744529757, -45.28718561006350285, -27.40856525842869829 ) ) ;
#19934 = CARTESIAN_POINT ( 'NONE',  ( 8.222734977135019108, -15.61599928274970139, -66.79233150823698395 ) ) ;
#19935 = CARTESIAN_POINT ( 'NONE',  ( 13.77456432040950141, 19.39060544165389999, -21.29084665975700119 ) ) ;
#19936 = CARTESIAN_POINT ( 'NONE',  ( 60.75158961744540420, 14.30615305676900029, -47.32592388962400776 ) ) ;
#19937 = CARTESIAN_POINT ( 'NONE',  ( 21.28035516724290233, -21.00331043453270397, -72.48992980192200264 ) ) ;
#19938 = CARTESIAN_POINT ( 'NONE',  ( 51.73941885623040093, 18.18506110802390197, -76.84325746863240170 ) ) ;
#19939 = CARTESIAN_POINT ( 'NONE',  ( 52.80965344031350384, 18.44124166929070086, -48.67334067697609612 ) ) ;
#19940 = LINE ( 'NONE', #23343, #16649 ) ;
#19941 = CARTESIAN_POINT ( 'NONE',  ( 53.26660255314480708, -49.43204447085090436, -48.79175800379049832 ) ) ;
#19942 = ORIENTED_EDGE ( 'NONE', *, *, #39986, .F. ) ;
#19943 = CARTESIAN_POINT ( 'NONE',  ( 5.741632552282960766, -9.616188944679340267, -22.14999999999999858 ) ) ;
#19944 = CARTESIAN_POINT ( 'NONE',  ( 47.53978851393139848, -54.55594495545970091, -54.68076641372660163 ) ) ;
#19945 = CARTESIAN_POINT ( 'NONE',  ( 9.367504675961500382, -15.61621390379479912, -67.84717978381009118 ) ) ;
#19946 = CARTESIAN_POINT ( 'NONE',  ( 54.63655771189059607, 16.82059223505549994, -26.73578643762699869 ) ) ;
#19947 = CARTESIAN_POINT ( 'NONE',  ( 61.42640818143939896, -30.97378847031719928, -16.54492983442209919 ) ) ;
#19948 = CARTESIAN_POINT ( 'NONE',  ( 71.48855272380100701, 0.8936201581567889685, -60.67538646459720297 ) ) ;
#19949 = CARTESIAN_POINT ( 'NONE',  ( 11.13393739769619906, 32.25300621514130484, -43.92547639555999694 ) ) ;
#19950 = CARTESIAN_POINT ( 'NONE',  ( 72.06219320706279063, 1.440335647928530083, -61.41002653287189617 ) ) ;
#19951 = FACE_OUTER_BOUND ( 'NONE', #37460, .T. ) ;
#19952 = VERTEX_POINT ( 'NONE', #26372 ) ;
#19953 = ORIENTED_EDGE ( 'NONE', *, *, #49823, .T. ) ;
#19954 = FACE_OUTER_BOUND ( 'NONE', #36488, .T. ) ;
#19955 = CARTESIAN_POINT ( 'NONE',  ( 49.86419038289391636, -29.64908286110574309, -15.89077235228104534 ) ) ;
#19956 = ORIENTED_EDGE ( 'NONE', *, *, #29270, .T. ) ;
#19957 = CARTESIAN_POINT ( 'NONE',  ( 8.223401571539490362, -15.61634053766229968, -58.50766849176299900 ) ) ;
#19958 = CARTESIAN_POINT ( 'NONE',  ( 10.23658038545237758, -12.23234384576881695, -49.61855340168781936 ) ) ;
#19959 = ORIENTED_EDGE ( 'NONE', *, *, #41104, .T. ) ;
#19960 = CARTESIAN_POINT ( 'NONE',  ( 72.18749078828946608, 11.23736444591397543, -67.25000000000000000 ) ) ;
#19961 = CARTESIAN_POINT ( 'NONE',  ( 17.63604474694339785, 0.9274771370723400299, -34.65000333055159842 ) ) ;
#19962 = CARTESIAN_POINT ( 'NONE',  ( 60.65419404070010501, 14.53878550406569836, -47.75595165931559904 ) ) ;
#19963 = EDGE_CURVE ( 'NONE', #29321, #4867, #45805, .T. ) ;
#19964 = DIRECTION ( 'NONE',  ( -1.000000000000000000, 0.000000000000000000, 0.000000000000000000 ) ) ;
#19965 = CARTESIAN_POINT ( 'NONE',  ( 12.65588489087358859, -22.74937664833755591, -50.43664658305362991 ) ) ;
#19966 = ADVANCED_FACE ( 'NONE', ( #37937 ), #26634, .T. ) ;
#19967 = CARTESIAN_POINT ( 'NONE',  ( 64.02385614546949455, -30.35404338245150058, -16.43221122146919910 ) ) ;
#19968 = CARTESIAN_POINT ( 'NONE',  ( 12.45110396332199976, -65.31062155621590648, -23.95537965760280130 ) ) ;
#19969 = CARTESIAN_POINT ( 'NONE',  ( 13.85267124424349916, -8.523762100343390102, -37.63360013392959758 ) ) ;
#19970 = AXIS2_PLACEMENT_3D ( 'NONE', #48609, #36796, #4568 ) ;
#19971 = CARTESIAN_POINT ( 'NONE',  ( 45.12954658315720025, 14.34843193608710088, -8.542182965482949086 ) ) ;
#19972 = CIRCLE ( 'NONE', #49295, 1.000000000000000888 ) ;
#19973 = DIRECTION ( 'NONE',  ( -0.05023550054956103100, 0.000000000000000000, 0.9987374001630935361 ) ) ;
#19974 =( BOUNDED_CURVE ( )  B_SPLINE_CURVE ( 3, ( #2648, #10770, #50079, #14174 ),
 .UNSPECIFIED., .F., .T. ) 
 B_SPLINE_CURVE_WITH_KNOTS ( ( 4, 4 ),
 ( 0.7853981633974705945, 1.570796326794917430 ),
 .UNSPECIFIED. ) 
 CURVE ( )  GEOMETRIC_REPRESENTATION_ITEM ( )  RATIONAL_B_SPLINE_CURVE ( ( 1.000000000000000000, 0.9492530216741912330, 0.9492530216741912330, 1.000000000000000000 ) ) 
 REPRESENTATION_ITEM ( '' )  );
#19975 = CARTESIAN_POINT ( 'NONE',  ( 83.67009235204480433, -44.53553140227840146, -46.70940576878270178 ) ) ;
#19976 = EDGE_CURVE ( 'NONE', #566, #24834, #47349, .T. ) ;
#19977 = DIRECTION ( 'NONE',  ( 0.000000000000000000, 0.000000000000000000, 1.000000000000000000 ) ) ;
#19978 = CARTESIAN_POINT ( 'NONE',  ( 11.63731196220440012, -22.52727282507490258, -44.19127752167019452 ) ) ;
#19979 = EDGE_LOOP ( 'NONE', ( #36021, #38290, #41049, #49667 ) ) ;
#19980 = CARTESIAN_POINT ( 'NONE',  ( 56.12605853786319443, -46.33585505558260564, -26.20103473702469898 ) ) ;
#19981 = CARTESIAN_POINT ( 'NONE',  ( 14.89545651468249865, -50.81498301574369947, -21.03875510983650088 ) ) ;
#19982 = CARTESIAN_POINT ( 'NONE',  ( 20.83810373529012239, -22.00309413542400350, -39.80555329850007240 ) ) ;
#19984 = EDGE_CURVE ( 'NONE', #17403, #40337, #7825, .T. ) ;
#19983 = CARTESIAN_POINT ( 'NONE',  ( 75.45574671126698263, 12.51734667287785996, -13.48816435240556011 ) ) ;
#19985 = CARTESIAN_POINT ( 'NONE',  ( 12.22498025668750010, -50.02555234895769587, -21.14999999999999858 ) ) ;
#19986 = VERTEX_POINT ( 'NONE', #36059 ) ;
#19987 = CARTESIAN_POINT ( 'NONE',  ( -7.439310335423879650, -45.55625616355589358, -5.547491402514559411 ) ) ;
#19988 = CYLINDRICAL_SURFACE ( 'NONE', #23941, 7.910999999999997812 ) ;
#19989 = CARTESIAN_POINT ( 'NONE',  ( 15.13982274958659247, 18.38378545640599171, -83.22692977633533928 ) ) ;
#19990 = CARTESIAN_POINT ( 'NONE',  ( 63.43729419656740731, 1.382840740411490188, -62.66598281567230089 ) ) ;
#19991 = CARTESIAN_POINT ( 'NONE',  ( 57.49763721924109916, -50.14068302088079321, -52.63210796847160822 ) ) ;
#19992 = CARTESIAN_POINT ( 'NONE',  ( 42.69362902231169699, 12.38631381078020155, -4.694965688683719662 ) ) ;
#19993 = CARTESIAN_POINT ( 'NONE',  ( 23.04646698902364221, -11.63206944219079908, -61.62566225664009067 ) ) ;
#19994 = PLANE ( 'NONE',  #7362 ) ;
#19995 = CARTESIAN_POINT ( 'NONE',  ( 60.23130391296999875, -45.78304229081430066, -47.24246919202539630 ) ) ;
#19996 = CARTESIAN_POINT ( 'NONE',  ( -0.3016046179078940015, -20.31737465961040101, -35.02873218748179340 ) ) ;
#19997 = CARTESIAN_POINT ( 'NONE',  ( 68.39017795531430011, -0.8919439843293410775, -18.15414638955719795 ) ) ;
#19998 = CARTESIAN_POINT ( 'NONE',  ( 17.74841177042720020, -52.60116553372549930, -76.03823174343609992 ) ) ;
#19999 = B_SPLINE_CURVE_WITH_KNOTS ( 'NONE', 3,
 ( #50054, #14148, #30117, #46136 ),
 .UNSPECIFIED., .F., .F.,
 ( 4, 4 ),
 ( 0.9850318682126864012, 1.000000000000000000 ),
 .UNSPECIFIED. ) ;
#20000 = B_SPLINE_CURVE_WITH_KNOTS ( 'NONE', 3,
 ( #51222, #31786, #7452, #7718, #7195, #15575, #22895, #27865, #39167, #39425, #43359, #7963, #43865, #35744, #47301, #31269, #27353, #39677, #31531, #51727 ),
 .UNSPECIFIED., .F., .F.,
 ( 4, 2, 2, 2, 2, 2, 2, 2, 2, 4 ),
 ( -1.826192301619919967, -1.710015269418689865, -1.458000257329579830, -1.209852399823200031, -1.027233169661210033, -0.9130961508099619817, -0.6848221131074718748, -0.4130753771390969220, -0.1614840352205790808, 0.000000000000000000 ),
 .UNSPECIFIED. ) ;
#20001 = CARTESIAN_POINT ( 'NONE',  ( 14.06336284780051216, -7.911061850705019438, -72.92433486291146494 ) ) ;
#20002 = AXIS2_PLACEMENT_3D ( 'NONE', #36722, #21249, #44864 ) ;
#20003 = FACE_OUTER_BOUND ( 'NONE', #21176, .T. ) ;
#20004 = ORIENTED_EDGE ( 'NONE', *, *, #4012, .T. ) ;
#20005 = FACE_OUTER_BOUND ( 'NONE', #37338, .T. ) ;
#20006 = CARTESIAN_POINT ( 'NONE',  ( 22.90100569266936148, -15.61618883250986300, -34.84718217067427304 ) ) ;
#20007 = AXIS2_PLACEMENT_3D ( 'NONE', #42042, #38367, #49661 ) ;
#20008 = AXIS2_PLACEMENT_3D ( 'NONE', #31268, #15315, #19494 ) ;
#20009 = CARTESIAN_POINT ( 'NONE',  ( 10.82420443828550027, -10.21340657480750025, -81.23899999999999011 ) ) ;
#20010 = ORIENTED_EDGE ( 'NONE', *, *, #26707, .T. ) ;
#20011 = CARTESIAN_POINT ( 'NONE',  ( 17.21347160910339724, 21.88381105532300097, -76.14999999999999147 ) ) ;
#20012 = ORIENTED_EDGE ( 'NONE', *, *, #51305, .T. ) ;
#20013 = B_SPLINE_CURVE_WITH_KNOTS ( 'NONE', 3,
 ( #29133, #12917, #45133, #4511, #48810, #37269, #28873, #44874, #25448, #1367, #24925, #40937, #5049, #17357, #49336, #22036, #46441, #30164, #46702, #42763, #50614, #45914, #50095, #14708, #38048, #10002, #22812, #34874, #1885, #46182, #41979, #30678, #30418, #2142, #14450, #18122, #10529, #34087, #10269, #25968, #45651, #2921, #18635, #6081, #9749, #37788, #10788, #14194, #26748, #26487, #18890, #29644, #49847, #22554, #13686, #13939, #18370, #26229, #42237, #34351, #38303, #6860, #6591, #25706, #38831, #38568, #41709, #5819, #21782, #50362, #33833, #17862, #29895, #6335, #22296, #42502, #2663, #34611, #39341, #26, #3442, #43529, #23069, #35906, #47975, #15999, #7369, #31952, #27782, #27266, #27522, #3955, #3697, #12076, #7882, #8137, #23829, #51647, #28031, #30934, #23574, #15233, #46963, #44034, #43779, #7630, #19152, #35131, #24082, #47719, #4196, #40102 ),
 .UNSPECIFIED., .F., .F.,
 ( 4, 3, 3, 3, 3, 3, 3, 3, 3, 3, 3, 3, 3, 3, 3, 3, 3, 3, 3, 3, 3, 3, 3, 3, 3, 3, 3, 3, 3, 3, 3, 3, 3, 3, 3, 3, 3, 4 ),
 ( -1.533736992487430006, -1.476288708613070044, -1.420671477261239879, -1.384064776590339996, -1.360357240506639975, -1.351866780710969884, -1.295064170024950112, -1.237933401408560119, -1.182875636651279816, -1.170176689418420013, -1.162728782331990063, -1.127817871893999957, -1.070863257187619988, -1.013122308480070011, -0.9549592363170329445, -0.9075319312463639987, -0.8918603899297049553, -0.8833676294135619500, -0.8240633864161019950, -0.7652500160343579383, -0.7062545595011729960, -0.6468558895549011423, -0.6146511525544209320, -0.6051427578306090016, -0.5954651251075159246, -0.5353212642531580689, -0.4746770572283909306, -0.4139650854173051453, -0.3892179935510600153, -0.3405657443571770138, -0.3192803853348540333, -0.3088845139008700169, -0.2992958171375259546, -0.2386551958669829165, -0.1768310421685470590, -0.1147878079956350383, -0.05320815132276890402, 0.000000000000000000 ),
 .UNSPECIFIED. ) ;
#20014 = ORIENTED_EDGE ( 'NONE', *, *, #2966, .F. ) ;
#20015 = LINE ( 'NONE', #48597, #51154 ) ;
#20016 = CARTESIAN_POINT ( 'NONE',  ( 22.75210022221799733, -11.58476054589980109, -81.23899999999999011 ) ) ;
#20017 = CARTESIAN_POINT ( 'NONE',  ( 17.16956915081890500, -7.705200979555163698, -73.33399818129967684 ) ) ;
#20018 = ORIENTED_EDGE ( 'NONE', *, *, #28477, .T. ) ;
#20019 = LINE ( 'NONE', #32836, #50032 ) ;
#20020 = VERTEX_POINT ( 'NONE', #7779 ) ;
#20021 = CARTESIAN_POINT ( 'NONE',  ( 97.41201884798559263, -0.1661889446793529956, -65.65000000000000568 ) ) ;
#20022 = EDGE_CURVE ( 'NONE', #17902, #23175, #5428, .T. ) ;
#20023 = LINE ( 'NONE', #16896, #8425 ) ;
#20024 = EDGE_LOOP ( 'NONE', ( #24297, #33736, #46436, #6812 ) ) ;
#20025 = EDGE_LOOP ( 'NONE', ( #25752, #5471, #18010, #43687 ) ) ;
#20026 = EDGE_CURVE ( 'NONE', #25535, #39953, #26006, .T. ) ;
#20027 = CARTESIAN_POINT ( 'NONE',  ( 44.47986911915002395, 1.897766893668719312, -48.24899763051212886 ) ) ;
#20028 = CARTESIAN_POINT ( 'NONE',  ( 11.93174526809839975, -65.43929183185349530, -17.93019253464870033 ) ) ;
#20029 = CARTESIAN_POINT ( 'NONE',  ( 60.32681533046309852, 14.53973477817790005, -47.49738862531440731 ) ) ;
#20030 = EDGE_CURVE ( 'NONE', #22337, #51786, #38569, .T. ) ;
#20031 = CARTESIAN_POINT ( 'NONE',  ( 22.61700722620988202, -13.63405001173012288, -40.35842241976454403 ) ) ;
#20032 = CARTESIAN_POINT ( 'NONE',  ( 16.13393739667419879, -15.61618894434099936, -11.12000000014429979 ) ) ;
#20033 = CARTESIAN_POINT ( 'NONE',  ( -6.916656312004059615, 14.59513431219300017, -4.826769747919490428 ) ) ;
#20034 = CIRCLE ( 'NONE', #50177, 9.768249999999998323 ) ;
#20035 = AXIS2_PLACEMENT_3D ( 'NONE', #10776, #26474, #50085 ) ;
#20036 = CIRCLE ( 'NONE', #49374, 5.500000000000000000 ) ;
#20037 = CARTESIAN_POINT ( 'NONE',  ( 46.89723159848931999, 22.92670389814115239, -75.65864031440739268 ) ) ;
#20038 = EDGE_CURVE ( 'NONE', #26643, #13074, #26651, .T. ) ;
#20039 = CARTESIAN_POINT ( 'NONE',  ( 55.38286017496716340, 14.79966023998268732, -16.52948577675217834 ) ) ;
#20040 = AXIS2_PLACEMENT_3D ( 'NONE', #45941, #30958, #43806 ) ;
#20041 = CARTESIAN_POINT ( 'NONE',  ( 21.41930692131999692, -9.815187549925822097, -59.02271152110689911 ) ) ;
#20042 = ORIENTED_EDGE ( 'NONE', *, *, #22675, .T. ) ;
#20043 = CARTESIAN_POINT ( 'NONE',  ( 16.13393739769620083, -15.61618894467929941, -32.14999999999999858 ) ) ;
#20045 = AXIS2_PLACEMENT_3D ( 'NONE', #43370, #15327, #35229 ) ;
#20044 = CARTESIAN_POINT ( 'NONE',  ( 42.30369714865540232, 14.62323136802010026, -7.058027111948209864 ) ) ;
#20046 = CARTESIAN_POINT ( 'NONE',  ( 11.13393739769499824, 32.42518242049779786, -43.78800780971030093 ) ) ;
#20048 = EDGE_CURVE ( 'NONE', #10051, #27800, #27677, .T. ) ;
#20047 = CARTESIAN_POINT ( 'NONE',  ( 72.12133632587820387, 1.039769764133249952, -70.13448369263871029 ) ) ;
#20049 = CARTESIAN_POINT ( 'NONE',  ( 43.05557787259338909, -39.87155913697362308, -71.22985127916425085 ) ) ;
#20050 = B_SPLINE_CURVE_WITH_KNOTS ( 'NONE', 3,
 ( #774, #16003, #31957, #47978 ),
 .UNSPECIFIED., .F., .F.,
 ( 4, 4 ),
 ( 0.1435918933159660016, 0.1514974462201259253 ),
 .UNSPECIFIED. ) ;
#20051 = CARTESIAN_POINT ( 'NONE',  ( 46.40057797168859821, -53.02061573618119894, -76.14999999999999147 ) ) ;
#20052 = CARTESIAN_POINT ( 'NONE',  ( 13.50362949724940087, 18.90074600912790004, -20.96762847177769729 ) ) ;
#20053 = CARTESIAN_POINT ( 'NONE',  ( 46.99011478535390296, 23.09104886575959981, -75.47331634174820181 ) ) ;
#20054 = CARTESIAN_POINT ( 'NONE',  ( 48.44331161791639317, -54.05217057865549890, -54.60670978497749672 ) ) ;
#20055 = CARTESIAN_POINT ( 'NONE',  ( 51.86283645288276034, -32.73404737421963517, -18.73275447517399073 ) ) ;
#20056 = CARTESIAN_POINT ( 'NONE',  ( 64.07670260090860381, 1.019777262794749895, -70.07076857027371375 ) ) ;
#20057 = CARTESIAN_POINT ( 'NONE',  ( 12.73487912048826232, 24.23912916116268690, -75.56421958049274679 ) ) ;
#20058 = CARTESIAN_POINT ( 'NONE',  ( 55.55365133010059964, 13.88381105532070059, -14.32025150907159983 ) ) ;
#20059 = EDGE_LOOP ( 'NONE', ( #39134, #18559, #27487, #9352, #37248, #37127 ) ) ;
#20060 = CARTESIAN_POINT ( 'NONE',  ( 22.94551214130139982, -13.78743987096419943, -80.76368641361828793 ) ) ;
#20061 = DIRECTION ( 'NONE',  ( 0.000000000000000000, -0.8263253571357117577, 0.5631930434180969502 ) ) ;
#20062 = ORIENTED_EDGE ( 'NONE', *, *, #50756, .T. ) ;
#20063 = CARTESIAN_POINT ( 'NONE',  ( 71.58938403497960223, 1.005545696829380109, -70.54702908378739323 ) ) ;
#20064 = CARTESIAN_POINT ( 'NONE',  ( 60.83106467324910227, -45.48877508199960573, -47.24035188271849250 ) ) ;
#20065 = CARTESIAN_POINT ( 'NONE',  ( 0.3209249304026170480, -20.69829881652800196, -34.64999999999999858 ) ) ;
#20066 = CARTESIAN_POINT ( 'NONE',  ( 7.517033938252880354, 30.35161808146150264, -19.14999999999999858 ) ) ;
#20068 = CARTESIAN_POINT ( 'NONE',  ( -0.007164427059776000244, -8.408015226406421405, -34.77269723891829756 ) ) ;
#20067 = CARTESIAN_POINT ( 'NONE',  ( 42.54370938950081182, 8.589020448392009399, -73.70510818031742417 ) ) ;
#20069 = EDGE_CURVE ( 'NONE', #35735, #15737, #3847, .T. ) ;
#20070 = CARTESIAN_POINT ( 'NONE',  ( 30.34915280000618409, 4.391813942490763623, -84.60938206585605315 ) ) ;
#20071 = CARTESIAN_POINT ( 'NONE',  ( 12.13393739769600010, -55.41568642894409180, -23.15000000000000213 ) ) ;
#20072 = ORIENTED_EDGE ( 'NONE', *, *, #41821, .T. ) ;
#20073 = CARTESIAN_POINT ( 'NONE',  ( 71.33393739769628894, 1.383811055320669947, -68.84999999999999432 ) ) ;
#20074 = ORIENTED_EDGE ( 'NONE', *, *, #22738, .T. ) ;
#20075 = CIRCLE ( 'NONE', #38499, 2.000000000000000888 ) ;
#20076 = ORIENTED_EDGE ( 'NONE', *, *, #25037, .F. ) ;
#20077 = CARTESIAN_POINT ( 'NONE',  ( 84.19224659786166853, 13.29802461769379818, -48.96577344625911365 ) ) ;
#20078 = TOROIDAL_SURFACE ( 'NONE', #15906, 25.00000000000000000, 1.000000000000000000 ) ;
#20079 = CARTESIAN_POINT ( 'NONE',  ( 20.99563212089781672, -9.290037028488647763, -79.50066649059343149 ) ) ;
#20080 = AXIS2_PLACEMENT_3D ( 'NONE', #16371, #7750, #39967 ) ;
#20081 = CARTESIAN_POINT ( 'NONE',  ( 76.39919602841192159, -19.31896256756559893, -12.79308182705372054 ) ) ;
#20082 = CARTESIAN_POINT ( 'NONE',  ( 51.58417065388699996, -52.63486567717929177, -53.74111633605280502 ) ) ;
#20083 = TOROIDAL_SURFACE ( 'NONE', #45201, 25.00000000000000000, 3.569999999999939888 ) ;
#20084 = ORIENTED_EDGE ( 'NONE', *, *, #25037, .T. ) ;
#20085 = VERTEX_POINT ( 'NONE', #35019 ) ;
#20086 = CIRCLE ( 'NONE', #30104, 34.47562460986260646 ) ;
#20087 = CARTESIAN_POINT ( 'NONE',  ( 49.21269661613270330, 22.37820248916990096, -54.26152208607290106 ) ) ;
#20088 = CARTESIAN_POINT ( 'NONE',  ( -21.49961078222543520, -5.348885346992251932, -53.70438154331316127 ) ) ;
#20089 = CARTESIAN_POINT ( 'NONE',  ( 56.49779928568679566, -50.76024185320960669, -53.73084170065449428 ) ) ;
#20090 = CARTESIAN_POINT ( 'NONE',  ( 8.786694880862668811, -63.12535539208791135, -46.67160944818530766 ) ) ;
#20091 = CARTESIAN_POINT ( 'NONE',  ( 61.20693769746879553, -0.3648949609556400575, -16.46666462177489976 ) ) ;
#20092 = CARTESIAN_POINT ( 'NONE',  ( 52.23706849658200468, -49.75889047595390480, -77.18592309284780129 ) ) ;
#20093 = EDGE_CURVE ( 'NONE', #19834, #46283, #48825, .T. ) ;
#20094 = VERTEX_POINT ( 'NONE', #12745 ) ;
#20095 = DIRECTION ( 'NONE',  ( -0.000000000000000000, 1.000000000000000000, 0.000000000000000000 ) ) ;
#20096 = CARTESIAN_POINT ( 'NONE',  ( 52.94902644660979973, -50.40032911565540275, -76.96923111675658902 ) ) ;
#20097 = CARTESIAN_POINT ( 'NONE',  ( 21.20676518767113805, -11.08013655934608011, -34.22047514491094233 ) ) ;
#20098 = CARTESIAN_POINT ( 'NONE',  ( 83.30738730474247689, -42.20963518668898473, -44.69194689374966600 ) ) ;
#20099 = ADVANCED_FACE ( 'NONE', ( #32360 ), #26213, .T. ) ;
#20100 = CARTESIAN_POINT ( 'NONE',  ( 21.83940206608119894, -10.22782922122060079, -49.77159047720319762 ) ) ;
#20101 = CARTESIAN_POINT ( 'NONE',  ( 12.76348253639140040, -50.31877257918069546, -21.19734575724999814 ) ) ;
#20102 = CARTESIAN_POINT ( 'NONE',  ( 18.14749711188961001, -51.13605320025961731, -15.68318871053545749 ) ) ;
#20103 = AXIS2_PLACEMENT_3D ( 'NONE', #50034, #22231, #29584 ) ;
#20104 = CARTESIAN_POINT ( 'NONE',  ( 68.13393739769745139, -49.21324915460503036, -70.54648330188275906 ) ) ;
#20105 = CARTESIAN_POINT ( 'NONE',  ( 60.85479269726300089, -45.48099585699259961, -47.26080742266869805 ) ) ;
#20106 = CARTESIAN_POINT ( 'NONE',  ( 71.29447239804829906, 1.393731187554809958, -70.25064478522961053 ) ) ;
#20107 = CARTESIAN_POINT ( 'NONE',  ( 23.01451526111969770, -17.16544923262910061, -48.91767612604338922 ) ) ;
#20108 = CARTESIAN_POINT ( 'NONE',  ( 15.09849613828851389, -7.705176109998896905, -41.25066457774981643 ) ) ;
#20109 = ORIENTED_EDGE ( 'NONE', *, *, #8706, .F. ) ;
#20110 = CARTESIAN_POINT ( 'NONE',  ( 13.94115953405779962, -51.19325459173029458, -74.14992922886710858 ) ) ;
#20111 = CARTESIAN_POINT ( 'NONE',  ( 47.24145533690699494, -54.76228788933499203, -54.65423412537209913 ) ) ;
#20112 = CARTESIAN_POINT ( 'NONE',  ( 8.428840728337423371, -13.54549715867946347, -36.59100207277058558 ) ) ;
#20113 = CYLINDRICAL_SURFACE ( 'NONE', #15425, 6.766999999999998572 ) ;
#20114 = AXIS2_PLACEMENT_3D ( 'NONE', #28947, #7316, #43728 ) ;
#20115 = CARTESIAN_POINT ( 'NONE',  ( 60.87740474328280982, -45.45106909386917948, -47.11566480119547862 ) ) ;
#20116 = AXIS2_PLACEMENT_3D ( 'NONE', #29499, #10896, #50469 ) ;
#20118 = AXIS2_PLACEMENT_3D ( 'NONE', #2654, #18624, #30666 ) ;
#20117 = CARTESIAN_POINT ( 'NONE',  ( 22.90093741582260378, -14.73038773615894215, -76.41114510696804984 ) ) ;
#20119 = DIRECTION ( 'NONE',  ( 0.000000000000000000, 0.000000000000000000, 1.000000000000000000 ) ) ;
#20121 = CARTESIAN_POINT ( 'NONE',  ( 9.807799258745877324, -20.47790172817659737, -52.58399763662833948 ) ) ;
#20120 = CARTESIAN_POINT ( 'NONE',  ( 16.13393739769639623, 7.383811055320659733, -62.64999999999999858 ) ) ;
#20122 = DIRECTION ( 'NONE',  ( 1.000000000000000000, 0.000000000000000000, 0.000000000000000000 ) ) ;
#20123 = CARTESIAN_POINT ( 'NONE',  ( 48.59172395386560339, 22.89772199268099939, -55.28129228068259948 ) ) ;
#20124 = ORIENTED_EDGE ( 'NONE', *, *, #34467, .T. ) ;
#20125 = CARTESIAN_POINT ( 'NONE',  ( 52.62897960803029918, -49.80262906116220023, -48.60272236542579805 ) ) ;
#20126 = ORIENTED_EDGE ( 'NONE', *, *, #46823, .T. ) ;
#20127 = CARTESIAN_POINT ( 'NONE',  ( 45.51548074848881242, 6.624593763210348207, -62.69088906692822860 ) ) ;
#20128 = CARTESIAN_POINT ( 'NONE',  ( 22.90093739792275684, -16.50198059704664999, -74.49448689417269520 ) ) ;
#20129 = FACE_OUTER_BOUND ( 'NONE', #43521, .T. ) ;
#20131 = CARTESIAN_POINT ( 'NONE',  ( 53.13430510201229851, 18.01985497199409991, -27.00377261849559929 ) ) ;
#20130 = CARTESIAN_POINT ( 'NONE',  ( 83.53868183867639630, 13.38921618474499908, -46.56548196350910018 ) ) ;
#20132 = EDGE_CURVE ( 'NONE', #44083, #9344, #18701, .T. ) ;
#20133 = CARTESIAN_POINT ( 'NONE',  ( 19.26073116756969839, -21.93803356609359767, -54.80661428419509917 ) ) ;
#20134 = CARTESIAN_POINT ( 'NONE',  ( 52.90670253716960048, 18.42639719312259672, -49.00842835936489905 ) ) ;
#20135 = CARTESIAN_POINT ( 'NONE',  ( 56.56153180275769898, -45.18625296881599951, -16.30282656199999991 ) ) ;
#20136 = CARTESIAN_POINT ( 'NONE',  ( 20.06281976506910070, -10.10654536788180025, -32.14999999999999858 ) ) ;
#20137 = EDGE_CURVE ( 'NONE', #1216, #17773, #43581, .T. ) ;
#20138 = ORIENTED_EDGE ( 'NONE', *, *, #14117, .F. ) ;
#20139 = CARTESIAN_POINT ( 'NONE',  ( 10.72003978276549852, -9.934951333187338918, -42.54517385987399791 ) ) ;
#20140 = ORIENTED_EDGE ( 'NONE', *, *, #35536, .T. ) ;
#20141 = ADVANCED_FACE ( 'NONE', ( #670 ), #16142, .T. ) ;
#20142 = CARTESIAN_POINT ( 'NONE',  ( 10.97564840259020080, -65.00352292546099875, -17.33480504156820245 ) ) ;
#20143 = CARTESIAN_POINT ( 'NONE',  ( 11.37064335167489837, 33.60134013189160385, -46.20549124663499896 ) ) ;
#20144 = DIRECTION ( 'NONE',  ( -1.000000000000000000, 0.000000000000000000, 0.000000000000000000 ) ) ;
#20145 = CARTESIAN_POINT ( 'NONE',  ( 47.54352022508510345, -54.65002938982319591, -55.12334797975140077 ) ) ;
#20146 = CARTESIAN_POINT ( 'NONE',  ( 11.52000135041339846, -65.33009319714545882, -22.63267478229686347 ) ) ;
#20147 = CARTESIAN_POINT ( 'NONE',  ( 51.40027097486221663, 3.258603514984763638, -76.69281807238613169 ) ) ;
#20148 = ORIENTED_EDGE ( 'NONE', *, *, #50658, .F. ) ;
#20149 = CARTESIAN_POINT ( 'NONE',  ( 49.40539548398250247, -53.49785366680099941, -54.15746054658189479 ) ) ;
#20150 = DIRECTION ( 'NONE',  ( 0.3805321250008311118, 0.000000000000000000, -0.9247677015566405645 ) ) ;
#20151 = CARTESIAN_POINT ( 'NONE',  ( 13.50201805292255308, 20.63639536108878048, -74.86151687916519393 ) ) ;
#20152 = ORIENTED_EDGE ( 'NONE', *, *, #44610, .T. ) ;
#20153 = CARTESIAN_POINT ( 'NONE',  ( 24.04485979958176145, -15.65237997675253467, -43.79378099706513439 ) ) ;
#20154 = CARTESIAN_POINT ( 'NONE',  ( 63.54731047306190561, 1.396834109478129804, -62.44999999999999574 ) ) ;
#20155 =( GEOMETRIC_REPRESENTATION_CONTEXT ( 3 ) GLOBAL_UNCERTAINTY_ASSIGNED_CONTEXT ( ( #43150 ) ) GLOBAL_UNIT_ASSIGNED_CONTEXT ( ( #32260, #4507, #7687 ) ) REPRESENTATION_CONTEXT ( 'NONE', 'WORKASPACE' ) );
#20156 = CARTESIAN_POINT ( 'NONE',  ( 12.76029016835228980, -8.414235847234261101, -48.86834743904469036 ) ) ;
#20157 = VECTOR ( 'NONE', #32739, 1000.000000000000000 ) ;
#20158 = ORIENTED_EDGE ( 'NONE', *, *, #21292, .T. ) ;
#20160 = CARTESIAN_POINT ( 'NONE',  ( 18.07449423817559975, -32.55558437065590027, -34.90839531524139971 ) ) ;
#20159 = CIRCLE ( 'NONE', #21011, 2.999999999999999556 ) ;
#20161 = CARTESIAN_POINT ( 'NONE',  ( 56.53399784783299964, -50.44739419118339896, -52.81205167950179913 ) ) ;
#20162 = CARTESIAN_POINT ( 'NONE',  ( 56.91947791887660202, 18.74135835950649920, -52.25429733693979983 ) ) ;
#20163 = AXIS2_PLACEMENT_3D ( 'NONE', #36930, #39837, #35898 ) ;
#20164 = EDGE_CURVE ( 'NONE', #36469, #26214, #48121, .T. ) ;
#20165 = CARTESIAN_POINT ( 'NONE',  ( 8.367277499166009491, -18.38416908848419951, -72.68335544512909507 ) ) ;
#20166 = DIRECTION ( 'NONE',  ( 0.000000000000000000, 0.000000000000000000, 1.000000000000000000 ) ) ;
#20167 = CARTESIAN_POINT ( 'NONE',  ( 54.14015757560070341, 19.94662053546359815, -75.52143025980080893 ) ) ;
#20168 = APPLICATION_PROTOCOL_DEFINITION ( 'draft international standard', 'automotive_design', 1998, #35476 ) ;
#20169 = ORIENTED_EDGE ( 'NONE', *, *, #16594, .T. ) ;
#20170 = CARTESIAN_POINT ( 'NONE',  ( 10.81560779913390036, -10.39871215161140050, -69.47961042150450339 ) ) ;
#20171 = CARTESIAN_POINT ( 'NONE',  ( 16.13393739769620083, -15.61618894467929941, -35.12503119152809461 ) ) ;
#20172 = CYLINDRICAL_SURFACE ( 'NONE', #28689, 6.766999999999998572 ) ;
#20173 = CARTESIAN_POINT ( 'NONE',  ( 47.06284717455670119, 23.15423693570959784, -75.35927708791611224 ) ) ;
#20174 = CARTESIAN_POINT ( 'NONE',  ( -18.86606260230390220, 19.38381105532060289, 16.85000000000000142 ) ) ;
#20175 = FACE_OUTER_BOUND ( 'NONE', #39706, .T. ) ;
#20176 = CARTESIAN_POINT ( 'NONE',  ( 12.28895731154029924, 33.39433106751570079, -15.84602084848570058 ) ) ;
#20177 = CARTESIAN_POINT ( 'NONE',  ( 8.167756527346648809, -13.48952887549759971, -68.59070828926491004 ) ) ;
#20178 = CARTESIAN_POINT ( 'NONE',  ( 55.31604533750469699, -50.61618591559609825, -76.42157388303350274 ) ) ;
#20180 = CARTESIAN_POINT ( 'NONE',  ( 46.03121886948380137, -45.11618894467940066, -7.582877905987319700 ) ) ;
#20179 = CARTESIAN_POINT ( 'NONE',  ( 15.31199894099709979, -16.87369336301570044, -35.14999999999999858 ) ) ;
#20181 = CARTESIAN_POINT ( 'NONE',  ( 63.35267264707980672, 1.373356196620459935, -68.60593141770759473 ) ) ;
#20182 = CARTESIAN_POINT ( 'NONE',  ( 61.35412202998309539, 13.97118731544910020, -46.63190125567759736 ) ) ;
#20183 = CARTESIAN_POINT ( 'NONE',  ( 24.04507396969289346, -15.61618901627517531, -67.50767071486835391 ) ) ;
#20184 = ORIENTED_EDGE ( 'NONE', *, *, #48527, .F. ) ;
#20185 = VECTOR ( 'NONE', #6034, 1000.000000000000000 ) ;
#20186 = CARTESIAN_POINT ( 'NONE',  ( 52.82122079009729276, -49.66539245525740398, -48.53632958723370194 ) ) ;
#20187 = AXIS2_PLACEMENT_3D ( 'NONE', #14565, #33429, #37900 ) ;
#20188 = CARTESIAN_POINT ( 'NONE',  ( 61.51097123149799728, -45.14411397284619909, -28.15118130352110271 ) ) ;
#20189 = CARTESIAN_POINT ( 'NONE',  ( 23.56462136197711388, -18.43314625579564137, -65.90774450879612800 ) ) ;
#20190 = CARTESIAN_POINT ( 'NONE',  ( 56.61906357297189629, 14.83060900076899991, -26.23212203939170095 ) ) ;
#20191 = CARTESIAN_POINT ( 'NONE',  ( 8.772777754335070455, -16.76511127020750180, -75.18337345808529903 ) ) ;
#20192 = CARTESIAN_POINT ( 'NONE',  ( 50.17499495619189531, 17.98397139427959956, -76.14999999999999147 ) ) ;
#20193 = CARTESIAN_POINT ( 'NONE',  ( 52.80835558948090380, 18.44458679360339559, -48.72774772676130084 ) ) ;
#20194 = CARTESIAN_POINT ( 'NONE',  ( 71.00993340901570150, 1.383811055320669947, -70.38195992526379996 ) ) ;
#20195 = CARTESIAN_POINT ( 'NONE',  ( -0.2865249686166103094, -8.445231654028917845, -35.01561944896767642 ) ) ;
#20196 = B_SPLINE_CURVE_WITH_KNOTS ( 'NONE', 3,
 ( #41120, #32706, #12837, #28794, #1288, #44795, #8899, #29311, #40856, #45316, #25372, #5487, #21445, #37444, #33501, #29567, #41897, #42158, #22215, #22730, #17781, #14372, #38482, #6257 ),
 .UNSPECIFIED., .F., .F.,
 ( 4, 2, 2, 2, 2, 2, 2, 2, 2, 2, 2, 4 ),
 ( 0.000000000000000000, 1.104949632659680159, 2.367749212842169992, 3.156998950456220143, 3.551623819263250326, 4.183023609354489913, 4.647713308159810097, 5.112403006965129393, 5.464321026995399677, 5.816239047025679731, 6.065118473969059565, 6.313997900912440286 ),
 .UNSPECIFIED. ) ;
#20197 = EDGE_CURVE ( 'NONE', #17323, #17172, #45434, .T. ) ;
#20198 = EDGE_LOOP ( 'NONE', ( #41811, #36149, #26503, #5414 ) ) ;
#20199 = CARTESIAN_POINT ( 'NONE',  ( 16.13393739769620083, -15.61618894467929941, -81.23899999999999011 ) ) ;
#20200 = EDGE_CURVE ( 'NONE', #21257, #33273, #24132, .T. ) ;
#20201 = CARTESIAN_POINT ( 'NONE',  ( 47.52872824421969966, -54.58671296295030118, -55.01004339176270008 ) ) ;
#20202 = CARTESIAN_POINT ( 'NONE',  ( 68.13393739769618662, -0.3411889446793609504, -65.65000000000000568 ) ) ;
#20203 = DIRECTION ( 'NONE',  ( 0.000000000000000000, 0.000000000000000000, -1.000000000000000000 ) ) ;
#20204 = CARTESIAN_POINT ( 'NONE',  ( 60.55719807483880146, -30.01614910288270011, -16.03343430148349924 ) ) ;
#20205 = CARTESIAN_POINT ( 'NONE',  ( 71.20900144662560649, 1.388715606738720076, -61.01996879627380110 ) ) ;
#20206 = DIRECTION ( 'NONE',  ( 0.7071067811865457964, 0.000000000000000000, 0.7071067811865492381 ) ) ;
#20207 = CARTESIAN_POINT ( 'NONE',  ( 72.04429487089811346, 1.454949836291180132, -61.42720652002459758 ) ) ;
#20208 = CARTESIAN_POINT ( 'NONE',  ( 82.75389963950340189, -45.59493862562520405, -47.67227237921369465 ) ) ;
#20209 = CARTESIAN_POINT ( 'NONE',  ( 65.21909306016200958, 1.375383258925270136, -70.44587820682191648 ) ) ;
#20210 = ORIENTED_EDGE ( 'NONE', *, *, #8316, .T. ) ;
#20211 = EDGE_LOOP ( 'NONE', ( #5138, #38719, #20675, #22051, #16136, #18984 ) ) ;
#20212 = CARTESIAN_POINT ( 'NONE',  ( 56.93466172174790074, 19.03186587073140146, -52.70269903729370498 ) ) ;
#20213 = CARTESIAN_POINT ( 'NONE',  ( 50.49064792301818727, -30.59810442101372274, -16.30494328501868395 ) ) ;
#20214 = ORIENTED_EDGE ( 'NONE', *, *, #874, .T. ) ;
#20215 = DIRECTION ( 'NONE',  ( 1.000000000000000000, 0.000000000000000000, 0.000000000000000000 ) ) ;
#20216 = CARTESIAN_POINT ( 'NONE',  ( 53.70553476669380188, 20.08271752784780162, -75.56421356237311215 ) ) ;
#20217 = ORIENTED_EDGE ( 'NONE', *, *, #9245, .T. ) ;
#20218 = CARTESIAN_POINT ( 'NONE',  ( 18.70788766945040038, -21.92435149714031439, -80.82966465033948111 ) ) ;
#20219 = CARTESIAN_POINT ( 'NONE',  ( 42.36605831465526251, 6.449731470917973830, -78.48939217686074699 ) ) ;
#20220 = CARTESIAN_POINT ( 'NONE',  ( 24.04369184426532513, -15.76790706435441614, -65.51376952231562711 ) ) ;
#20221 = EDGE_CURVE ( 'NONE', #46925, #11609, #45229, .T. ) ;
#20222 = CARTESIAN_POINT ( 'NONE',  ( 23.43186596475139893, -19.45323972439200233, -41.94641019244489399 ) ) ;
#20223 = CARTESIAN_POINT ( 'NONE',  ( 51.13393739769620083, -15.61618894467929941, 9.349999999999999645 ) ) ;
#20224 = CARTESIAN_POINT ( 'NONE',  ( 42.19548255040618301, -37.65468939562691730, -79.34225115792774830 ) ) ;
#20225 = EDGE_CURVE ( 'NONE', #21835, #9203, #9066, .T. ) ;
#20226 = ORIENTED_EDGE ( 'NONE', *, *, #26644, .F. ) ;
#20227 = CIRCLE ( 'NONE', #11050, 21.72891455324079857 ) ;
#20228 = CARTESIAN_POINT ( 'NONE',  ( 11.47481840896679905, -64.34949529473630037, -24.24805382140619869 ) ) ;
#20229 = CARTESIAN_POINT ( 'NONE',  ( 22.25441655865059687, -19.86429777632060123, -38.42578944456580103 ) ) ;
#20230 = CARTESIAN_POINT ( 'NONE',  ( 45.47878560944119641, 14.14190573372439808, -8.420277138987120935 ) ) ;
#20231 = CARTESIAN_POINT ( 'NONE',  ( 14.72167300019409986, 20.94680560585010198, -75.92929371827810314 ) ) ;
#20232 = CARTESIAN_POINT ( 'NONE',  ( 51.67587649748560352, 17.45826286971839991, -77.01363636363639387 ) ) ;
#20233 = CARTESIAN_POINT ( 'NONE',  ( 83.70962855682149950, -44.61778334324309725, -46.98048264170719790 ) ) ;
#20234 = CARTESIAN_POINT ( 'NONE',  ( 64.42805214825888527, 1.442148388150169991, -70.01405398929449575 ) ) ;
#20235 = CARTESIAN_POINT ( 'NONE',  ( 24.18319539530660123, -13.82952546296830043, -39.43814165785290271 ) ) ;
#20236 = ORIENTED_EDGE ( 'NONE', *, *, #31503, .T. ) ;
#20237 = CARTESIAN_POINT ( 'NONE',  ( 56.36055522987030031, -46.08204502026070770, -26.17081810832250000 ) ) ;
#20238 = CARTESIAN_POINT ( 'NONE',  ( 15.66736729373610260, -50.89670101629940291, -20.45701610577929941 ) ) ;
#20239 = CARTESIAN_POINT ( 'NONE',  ( 23.98346616282663035, -16.73315592963927756, -39.55263113089927884 ) ) ;
#20240 = CARTESIAN_POINT ( 'NONE',  ( -21.36606260230379917, 30.88381105532059934, 16.35000000000000142 ) ) ;
#20241 = FACE_OUTER_BOUND ( 'NONE', #10526, .T. ) ;
#20242 = CARTESIAN_POINT ( 'NONE',  ( 2.414204846871564669, -5.385696586492555227, -35.10658870009159216 ) ) ;
#20243 = VERTEX_POINT ( 'NONE', #25015 ) ;
#20244 = CARTESIAN_POINT ( 'NONE',  ( -3.404429431994520083, -48.49755752188070090, -5.261476749836609734 ) ) ;
#20245 = CARTESIAN_POINT ( 'NONE',  ( 47.23233947733660187, 23.53691302697210119, -54.67407144479440007 ) ) ;
#20246 = DIRECTION ( 'NONE',  ( 0.000000000000000000, 0.000000000000000000, -1.000000000000000000 ) ) ;
#20247 = CARTESIAN_POINT ( 'NONE',  ( 63.26414124932220062, 1.334812829108570131, -62.63859554625260273 ) ) ;
#20248 = CARTESIAN_POINT ( 'NONE',  ( 68.13393739769620083, 0.8838110553206759423, -59.64999999999999858 ) ) ;
#20249 = CARTESIAN_POINT ( 'NONE',  ( 43.37850551145179878, 12.25211561368529978, -4.923475879823000056 ) ) ;
#20250 = CARTESIAN_POINT ( 'NONE',  ( 16.13393739769620083, -15.61618894467929941, -7.049999999999999822 ) ) ;
#20251 = CARTESIAN_POINT ( 'NONE',  ( 19.54197537461858403, -21.52907253456916692, -64.78615502841283558 ) ) ;
#20252 = DIRECTION ( 'NONE',  ( 0.000000000000000000, 0.000000000000000000, -1.000000000000000000 ) ) ;
#20253 = CARTESIAN_POINT ( 'NONE',  ( 7.635415421591214447, 29.62789471496180482, -20.56421356237308729 ) ) ;
#20254 = CARTESIAN_POINT ( 'NONE',  ( -0.2068757739851316280, -20.53916885483576849, -34.94635309924921529 ) ) ;
#20255 = EDGE_CURVE ( 'NONE', #30697, #36299, #21196, .T. ) ;
#20256 = CARTESIAN_POINT ( 'NONE',  ( 64.72196861157989645, 1.188860127980290171, -60.81548205241750082 ) ) ;
#20257 = CARTESIAN_POINT ( 'NONE',  ( 17.35523042653849757, -52.75136490455189886, -76.12493046668770091 ) ) ;
#20258 = AXIS2_PLACEMENT_3D ( 'NONE', #51297, #32113, #3088 ) ;
#20259 = CARTESIAN_POINT ( 'NONE',  ( 20.99566198266418482, -9.290060858646725706, -73.21600132271542805 ) ) ;
#20260 = CARTESIAN_POINT ( 'NONE',  ( 56.94972635783080506, -49.95903273471010664, -52.23813480702960277 ) ) ;
#20261 = ORIENTED_EDGE ( 'NONE', *, *, #28600, .F. ) ;
#20262 = CYLINDRICAL_SURFACE ( 'NONE', #45498, 0.4999999999999982236 ) ;
#20263 = DIRECTION ( 'NONE',  ( 0.000000000000000000, 0.000000000000000000, -1.000000000000000000 ) ) ;
#20264 = CARTESIAN_POINT ( 'NONE',  ( 10.44460050029429965, -10.68230576789959940, -81.23899999999999011 ) ) ;
#20265 = VERTEX_POINT ( 'NONE', #24232 ) ;
#20266 = CARTESIAN_POINT ( 'NONE',  ( 18.26047510295519771, 20.40964180427139851, -75.33373089150879309 ) ) ;
#20267 = ORIENTED_EDGE ( 'NONE', *, *, #19023, .T. ) ;
#20268 = ORIENTED_EDGE ( 'NONE', *, *, #24149, .F. ) ;
#20269 = ORIENTED_EDGE ( 'NONE', *, *, #33185, .F. ) ;
#20270 = CARTESIAN_POINT ( 'NONE',  ( 57.41357375845870337, -45.73808401094120057, -26.25850225888439837 ) ) ;
#20271 = CARTESIAN_POINT ( 'NONE',  ( 18.64696929856319940, -21.92391060386649926, -81.23899999999999011 ) ) ;
#20272 = CARTESIAN_POINT ( 'NONE',  ( 8.223487313465298598, -15.61606829411550024, -62.50766849176299189 ) ) ;
#20273 = CARTESIAN_POINT ( 'NONE',  ( 22.46012461926354220, -10.75454118387916580, -73.58399818425169769 ) ) ;
#20274 = CARTESIAN_POINT ( 'NONE',  ( 9.366420286904855175, -15.72757149194933035, -69.84194449815306882 ) ) ;
#20275 = DIRECTION ( 'NONE',  ( 1.000000000000000000, 0.000000000000000000, 0.000000000000000000 ) ) ;
#20276 = VERTEX_POINT ( 'NONE', #5398 ) ;
#20277 = CARTESIAN_POINT ( 'NONE',  ( 53.93371030420179579, -46.24505842335499750, -15.35643322793939980 ) ) ;
#20278 = EDGE_CURVE ( 'NONE', #32200, #51495, #416, .T. ) ;
#20279 = FACE_OUTER_BOUND ( 'NONE', #6275, .T. ) ;
#20280 = ORIENTED_EDGE ( 'NONE', *, *, #19927, .F. ) ;
#20282 = ORIENTED_EDGE ( 'NONE', *, *, #12554, .F. ) ;
#20281 =( BOUNDED_CURVE ( )  B_SPLINE_CURVE ( 3, ( #5894, #38125, #34164, #2220 ),
 .UNSPECIFIED., .F., .T. ) 
 B_SPLINE_CURVE_WITH_KNOTS ( ( 4, 4 ),
 ( 0.7853981633974498333, 1.570796326794903219 ),
 .UNSPECIFIED. ) 
 CURVE ( )  GEOMETRIC_REPRESENTATION_ITEM ( )  RATIONAL_B_SPLINE_CURVE ( ( 1.000000000000000000, 0.9492530216741903448, 0.9492530216741903448, 1.000000000000000000 ) ) 
 REPRESENTATION_ITEM ( '' )  );
#20283 = CARTESIAN_POINT ( 'NONE',  ( 72.72056432233058842, 1.396834109478129804, -62.44999999999999574 ) ) ;
#20284 = DIRECTION ( 'NONE',  ( 0.000000000000000000, 0.000000000000000000, 1.000000000000000000 ) ) ;
#20285 = CARTESIAN_POINT ( 'NONE',  ( 60.61871271361510338, 14.50847209906229907, -47.69407632338739944 ) ) ;
#20286 = CARTESIAN_POINT ( 'NONE',  ( 49.42599303854620274, 14.94800067427769896, -12.04389119005679909 ) ) ;
#20287 = CARTESIAN_POINT ( 'NONE',  ( 16.65420337941059969, -49.11618894467930829, -20.15000000000000213 ) ) ;
#20288 = B_SPLINE_CURVE_WITH_KNOTS ( 'NONE', 3,
 ( #47109, #21486, #51285, #21741, #7009, #7261, #19042, #17824, #10939, #35018, #11198, #15123, #25926, #21998, #49561, #37485, #23211, #33798 ),
 .UNSPECIFIED., .F., .F.,
 ( 4, 2, 2, 2, 2, 2, 2, 2, 4 ),
 ( 0.4999995031043945604, 0.5624995652163452542, 0.6249996273282960590, 0.6874996894402467529, 0.7499997515521974467, 0.8124998136641481405, 0.8749998757760988344, 0.9374999378880493062, 1.000000000000000000 ),
 .UNSPECIFIED. ) ;
#20289 = CARTESIAN_POINT ( 'NONE',  ( -6.905391680084830064, 14.60833507279039978, -4.924128923718519957 ) ) ;
#20290 = AXIS2_PLACEMENT_3D ( 'NONE', #45899, #9986, #35039 ) ;
#20291 = B_SPLINE_CURVE_WITH_KNOTS ( 'NONE', 3,
 ( #45320, #9426, #2068, #25376, #37969, #49262, #41377, #36931, #18044, #13356, #49519, #8903, #24853, #1034, #40861, #32979 ),
 .UNSPECIFIED., .F., .F.,
 ( 4, 2, 2, 2, 2, 2, 2, 4 ),
 ( 0.000000000000000000, 2.070511893743609999, 3.936888812047710573, 5.103374385987770268, 5.832427869700300249, 7.290534837125381529, 9.623505985005499141, 11.66485573940060050 ),
 .UNSPECIFIED. ) ;
#20292 = AXIS2_PLACEMENT_3D ( 'NONE', #37513, #33572, #26219 ) ;
#20293 = PLANE ( 'NONE',  #34650 ) ;
#20294 = FACE_OUTER_BOUND ( 'NONE', #49229, .T. ) ;
#20295 = CARTESIAN_POINT ( 'NONE',  ( 8.286499081069370831, -15.54940533950840020, -60.29021441812479765 ) ) ;
#20296 = VERTEX_POINT ( 'NONE', #41545 ) ;
#20297 = CARTESIAN_POINT ( 'NONE',  ( 55.07039890521039638, 17.27901299975469840, -48.53535122690350079 ) ) ;
#20298 = CARTESIAN_POINT ( 'NONE',  ( 28.28038400710289935, -8.603434725040973063, -34.79644660940672907 ) ) ;
#20299 = CARTESIAN_POINT ( 'NONE',  ( 11.33958473649649967, 33.18416475853179293, -44.55219422208060109 ) ) ;
#20300 = CARTESIAN_POINT ( 'NONE',  ( 72.49406130868889875, 1.342503070345580030, -69.60129888054170522 ) ) ;
#20301 = CARTESIAN_POINT ( 'NONE',  ( 44.01566611027487141, -39.95595433770805016, -66.58381346753706964 ) ) ;
#20302 = CARTESIAN_POINT ( 'NONE',  ( 46.65228552882730639, 22.34474942460779801, -76.02816657613060158 ) ) ;
#20303 = CARTESIAN_POINT ( 'NONE',  ( 48.45666297591670002, -54.07999444344789453, -54.69197698175730693 ) ) ;
#20304 = CARTESIAN_POINT ( 'NONE',  ( -9.414006712227710238, 12.57454005906549988, -5.942694572982400558 ) ) ;
#20305 = AXIS2_PLACEMENT_3D ( 'NONE', #49413, #1959, #46255 ) ;
#20306 = EDGE_CURVE ( 'NONE', #6210, #885, #17877, .T. ) ;
#20307 = CARTESIAN_POINT ( 'NONE',  ( 12.91854708852280176, -27.61618894467928698, -22.14999999999998792 ) ) ;
#20308 = CARTESIAN_POINT ( 'NONE',  ( 14.43662147174949872, -32.33724466207230108, -34.68801049095930011 ) ) ;
#20309 = DIRECTION ( 'NONE',  ( -0.6561787149247867434, 0.000000000000000000, 0.7546055221635046273 ) ) ;
#20310 = ORIENTED_EDGE ( 'NONE', *, *, #18490, .T. ) ;
#20311 = ADVANCED_FACE ( 'NONE', ( #17446 ), #37358, .T. ) ;
#20312 = CARTESIAN_POINT ( 'NONE',  ( 14.64089083101909949, -22.91533316082380267, -39.63156730105999515 ) ) ;
#20313 = ADVANCED_FACE ( 'NONE', ( #49685 ), #14032, .T. ) ;
#20314 = CARTESIAN_POINT ( 'NONE',  ( 64.61436174452420289, 1.028860820851879909, -60.80092091627260231 ) ) ;
#20315 = CARTESIAN_POINT ( 'NONE',  ( 71.52819866244169589, 1.000225705806889964, -70.58924174254049433 ) ) ;
#20316 = CARTESIAN_POINT ( 'NONE',  ( 60.42880969657360168, -45.68174640767169592, -47.27616847270299871 ) ) ;
#20317 = CARTESIAN_POINT ( 'NONE',  ( 12.13393739769600010, -55.41568642894409180, -23.15000000000000213 ) ) ;
#20318 = CARTESIAN_POINT ( 'NONE',  ( 13.73527022026379996, 18.97497658877130178, -20.93080062776429884 ) ) ;
#20320 = CARTESIAN_POINT ( 'NONE',  ( 45.14832757675640096, -33.29289077328009938, -35.14999999999999858 ) ) ;
#20319 = CARTESIAN_POINT ( 'NONE',  ( 41.23411137459665810, 8.445767796141971928, -80.02631633623509799 ) ) ;
#20321 = EDGE_CURVE ( 'NONE', #33243, #40988, #7279, .T. ) ;
#20322 = CARTESIAN_POINT ( 'NONE',  ( 16.13393739769620083, -15.61618894467929941, -7.349999999999999645 ) ) ;
#20323 = CARTESIAN_POINT ( 'NONE',  ( 8.223605785152290792, -15.61620117245469963, -52.50766849176299900 ) ) ;
#20324 = ORIENTED_EDGE ( 'NONE', *, *, #9172, .T. ) ;
#20325 = CARTESIAN_POINT ( 'NONE',  ( 84.43710458089100257, -43.31157081238789885, -47.42958317885469910 ) ) ;
#20326 = ORIENTED_EDGE ( 'NONE', *, *, #36551, .T. ) ;
#20327 = EDGE_LOOP ( 'NONE', ( #41403, #172, #28087, #6544 ) ) ;
#20328 = EDGE_LOOP ( 'NONE', ( #6027, #39751, #14092, #6810, #35560, #12054 ) ) ;
#20329 = CARTESIAN_POINT ( 'NONE',  ( 16.13393739769620083, -15.61618894467929941, -28.45282021618999835 ) ) ;
#20330 = CARTESIAN_POINT ( 'NONE',  ( 53.59153692561029914, -49.40734274622519706, -49.22791863455219641 ) ) ;
#20331 = CARTESIAN_POINT ( 'NONE',  ( 56.24502371864222283, 14.78143158593881878, -26.06737860630848402 ) ) ;
#20332 = CARTESIAN_POINT ( 'NONE',  ( 76.40835530721405178, -10.60522176584313314, -12.83250761640861626 ) ) ;
#20333 = CARTESIAN_POINT ( 'NONE',  ( 53.26253095931190273, -52.14051419252140107, -54.20764878218570004 ) ) ;
#20334 = AXIS2_PLACEMENT_3D ( 'NONE', #38171, #46305, #10393 ) ;
#20335 = EDGE_LOOP ( 'NONE', ( #15756, #35285 ) ) ;
#20336 = VERTEX_POINT ( 'NONE', #38397 ) ;
#20337 = CARTESIAN_POINT ( 'NONE',  ( 9.221328447382354909, -19.60017377966054397, -56.34096481581358518 ) ) ;
#20338 = CARTESIAN_POINT ( 'NONE',  ( 14.88857959731166503, -8.720501068069950179, -32.29061302249797905 ) ) ;
#20339 = CARTESIAN_POINT ( 'NONE',  ( 73.06894106338337735, -0.5161889446793590519, -69.23549003898403953 ) ) ;
#20340 = DIRECTION ( 'NONE',  ( 0.5685928097855377228, 0.5944782866685497380, -0.5685928097855377228 ) ) ;
#20341 = CARTESIAN_POINT ( 'NONE',  ( 24.01953165718990846, -14.96959786440184104, -59.76628937629125460 ) ) ;
#20342 = EDGE_CURVE ( 'NONE', #24877, #50028, #27078, .T. ) ;
#20343 = CARTESIAN_POINT ( 'NONE',  ( -21.36606260230379917, 31.88381105532059934, 16.35000000000000142 ) ) ;
#20344 = EDGE_LOOP ( 'NONE', ( #43071, #14458, #24280, #51614 ) ) ;
#20345 = CARTESIAN_POINT ( 'NONE',  ( 57.55751162049570269, -50.09049722528730086, -52.57651812429949700 ) ) ;
#20346 = CARTESIAN_POINT ( 'NONE',  ( 53.79479401630810287, -50.60286759701570247, -76.98386069065520587 ) ) ;
#20347 = CARTESIAN_POINT ( 'NONE',  ( 64.66447934098378880, 0.9065823421260920112, -70.54525856488091051 ) ) ;
#20348 = DIRECTION ( 'NONE',  ( -0.1686178020941689615, 0.6660492713794448072, 0.7265992051412127894 ) ) ;
#20349 = CARTESIAN_POINT ( 'NONE',  ( 19.05258302078599897, -8.331392769191539927, -55.63379137591120127 ) ) ;
#20350 = CARTESIAN_POINT ( 'NONE',  ( 13.52884004244890015, -50.22107084656090592, -21.01312649677589661 ) ) ;
#20351 = AXIS2_PLACEMENT_3D ( 'NONE', #15828, #22186, #39434 ) ;
#20352 = DIRECTION ( 'NONE',  ( 0.9200120562340469155, 0.3918900565005459247, 8.326672684688669123E-17 ) ) ;
#20353 = DIRECTION ( 'NONE',  ( 0.4778512656426511240, -0.8513147483649062819, 0.2166134048024561665 ) ) ;
#20354 = CARTESIAN_POINT ( 'NONE',  ( -19.86606260230379917, -15.61618894467929408, 8.349999999999999645 ) ) ;
#20355 = CARTESIAN_POINT ( 'NONE',  ( 53.55347996450810655, 18.14618377272432426, -49.15350056088379205 ) ) ;
#20356 = CARTESIAN_POINT ( 'NONE',  ( 71.31427394968270050, 1.395196698723390138, -70.24366017557039754 ) ) ;
#20357 = EDGE_CURVE ( 'NONE', #17962, #7646, #43005, .T. ) ;
#20358 = CARTESIAN_POINT ( 'NONE',  ( 18.57770503654679928, -22.23212114670179673, -49.23455185029789760 ) ) ;
#20359 = PLANE ( 'NONE',  #8411 ) ;
#20360 = VERTEX_POINT ( 'NONE', #26064 ) ;
#20361 = CARTESIAN_POINT ( 'NONE',  ( 14.59877825211439983, -51.94403353591209793, -75.77396328158880578 ) ) ;
#20362 = CONICAL_SURFACE ( 'NONE', #16187, 0.7980000000000000426, 0.7853981633974476129 ) ;
#20363 = CARTESIAN_POINT ( 'NONE',  ( 47.37100612791930132, -54.67334532463610230, -54.74722572687750244 ) ) ;
#20364 = DIRECTION ( 'NONE',  ( 1.000000000000000000, 0.000000000000000000, 0.000000000000000000 ) ) ;
#20365 = CARTESIAN_POINT ( 'NONE',  ( 15.24812203796652277, -8.849191014885372297, -37.91115498390873739 ) ) ;
#20366 = CARTESIAN_POINT ( 'NONE',  ( 84.12560686116410125, 12.73461969822788653, -46.88422903745967574 ) ) ;
#20367 = AXIS2_PLACEMENT_3D ( 'NONE', #36452, #44328, #27823 ) ;
#20368 = CARTESIAN_POINT ( 'NONE',  ( 60.94144441405484258, -45.44327996998872266, -47.23355084903774070 ) ) ;
#20369 = CARTESIAN_POINT ( 'NONE',  ( 55.91595771132564607, -45.90465035585578590, -17.78184172665631380 ) ) ;
#20370 = CARTESIAN_POINT ( 'NONE',  ( 11.73545769478199929, 34.19022130663289971, -18.15007894723629889 ) ) ;
#20372 = CARTESIAN_POINT ( 'NONE',  ( 18.20469047841077170, -23.32126825782679092, -73.92433474470422539 ) ) ;
#20371 = LINE ( 'NONE', #16455, #31448 ) ;
#20373 = DIRECTION ( 'NONE',  ( 1.000000000000000000, 0.000000000000000000, 0.000000000000000000 ) ) ;
#20374 = CARTESIAN_POINT ( 'NONE',  ( 48.43561012759799667, 22.85868164950310089, -54.69790868973249331 ) ) ;
#20375 = EDGE_LOOP ( 'NONE', ( #36779, #33848, #47064, #10097, #35014 ) ) ;
#20376 = CARTESIAN_POINT ( 'NONE',  ( 52.76221414360290396, -49.72258092212369718, -48.84748662852409495 ) ) ;
#20377 = VERTEX_POINT ( 'NONE', #1457 ) ;
#20378 = DIRECTION ( 'NONE',  ( 0.000000000000000000, 0.000000000000000000, 1.000000000000000000 ) ) ;
#20379 = CARTESIAN_POINT ( 'NONE',  ( 9.366958054073847961, -16.50213838875509609, -75.41115355001534226 ) ) ;
#20380 = CARTESIAN_POINT ( 'NONE',  ( 14.25134538048030031, 19.88704348275010148, -22.60288544069040029 ) ) ;
#20382 = CARTESIAN_POINT ( 'NONE',  ( 52.61201418189830292, 18.58180670245910093, -28.15003492000239760 ) ) ;
#20381 = CARTESIAN_POINT ( 'NONE',  ( 84.14547009360870788, 12.78988100953520046, -47.04794573760770504 ) ) ;
#20383 = CARTESIAN_POINT ( 'NONE',  ( 23.12781470739479772, -14.70611264375299854, -62.41163166630270354 ) ) ;
#20385 = EDGE_CURVE ( 'NONE', #39558, #26710, #6186, .T. ) ;
#20384 = CARTESIAN_POINT ( 'NONE',  ( 53.59007319642049794, 18.17385789206429791, -49.22505640095170065 ) ) ;
#20386 = CARTESIAN_POINT ( 'NONE',  ( 56.50061918389100413, -45.38130610931129638, -17.74550412614280148 ) ) ;
#20387 = DIRECTION ( 'NONE',  ( 0.000000000000000000, -1.000000000000000000, 0.000000000000000000 ) ) ;
#20388 = VECTOR ( 'NONE', #12719, 1000.000000000000000 ) ;
#20389 = B_SPLINE_CURVE_WITH_KNOTS ( 'NONE', 3,
 ( #2025, #14077, #49223, #17495, #5453, #33462, #29533, #38186, #1766, #30038, #46061, #42118, #9633, #25589, #41594, #5703, #33717, #49731, #13820, #19296, #19550, #11189, #51534, #26627, #51276, #10671, #42643, #10929, #42903, #43410, #38443, #47604, #14591, #3062, #50759, #23202 ),
 .UNSPECIFIED., .F., .F.,
 ( 4, 2, 2, 2, 2, 2, 2, 2, 2, 2, 2, 2, 2, 1, 1, 1, 1, 1, 1, 2, 4 ),
 ( 0.000000000000000000, 0.06250066402867544835, 0.1250013280573508967, 0.1875019920860263312, 0.2500026561147017934, 0.3125033201433771723, 0.3437536521577148063, 0.3750039841720524403, 0.4062543161863901298, 0.4375046482007277637, 0.4687549802150655087, 0.4843801462222342979, 0.4921927292258187481, 0.4960990207276109731, 0.4980521664785070857, 0.4990287393539551419, 0.4995170257916792256, 0.4997611690105412396, 0.4998832406199723022, 0.4999442764246878057, 0.5000053122294032537 ),
 .UNSPECIFIED. ) ;
#20390 = EDGE_LOOP ( 'NONE', ( #38615, #8882, #27201, #21362 ) ) ;
#20391 = B_SPLINE_CURVE_WITH_KNOTS ( 'NONE', 3,
 ( #25682, #2638, #22784, #49574, #9976, #29621, #30393, #29869, #30134, #22529, #34323, #45623, #9723, #14424, #46416, #42475, #41684, #5792 ),
 .UNSPECIFIED., .F., .F.,
 ( 4, 2, 2, 2, 2, 2, 2, 2, 4 ),
 ( 0.4999961870157385579, 0.5624966636387712660, 0.6249971402618039740, 0.6874976168848365710, 0.7499980935078692790, 0.8124985701309019870, 0.8749990467539345840, 0.9374995233769672920, 1.000000000000000000 ),
 .UNSPECIFIED. ) ;
#20392 = ORIENTED_EDGE ( 'NONE', *, *, #16748, .T. ) ;
#20393 = CARTESIAN_POINT ( 'NONE',  ( 11.31751865133579926, -65.23669584953859157, -17.44711623494750086 ) ) ;
#20394 = CARTESIAN_POINT ( 'NONE',  ( 11.56529054650530064, 33.93083920818509824, -46.99198115399620690 ) ) ;
#20395 = CARTESIAN_POINT ( 'NONE',  ( 68.13393739769620083, -50.61618894467930119, -76.75000000000000000 ) ) ;
#20396 = CARTESIAN_POINT ( 'NONE',  ( 51.40213405747029896, -51.07147713869009920, -49.97437711432529994 ) ) ;
#20397 = CARTESIAN_POINT ( 'NONE',  ( 10.96685795547830011, -64.79867901642927563, -23.23109294039089789 ) ) ;
#20398 = CYLINDRICAL_SURFACE ( 'NONE', #32598, 7.910999999999997812 ) ;
#20399 = ORIENTED_EDGE ( 'NONE', *, *, #50105, .T. ) ;
#20400 = CARTESIAN_POINT ( 'NONE',  ( 9.807693316221877566, -10.75461209725539469, -74.71598022707215137 ) ) ;
#20401 = CARTESIAN_POINT ( 'NONE',  ( 11.13393739769619906, -63.32855195616750166, -43.91646290072930015 ) ) ;
#20402 = DIRECTION ( 'NONE',  ( 0.000000000000000000, -0.9319748226751467524, 0.3625230060280709155 ) ) ;
#20403 = ADVANCED_FACE ( 'NONE', ( #26326 ), #14290, .T. ) ;
#20404 = CARTESIAN_POINT ( 'NONE',  ( 50.52803994521560327, -50.37895321258069714, -76.14999999999999147 ) ) ;
#20405 = DIRECTION ( 'NONE',  ( 0.000000000000000000, 0.000000000000000000, -1.000000000000000000 ) ) ;
#20406 = ORIENTED_EDGE ( 'NONE', *, *, #42114, .F. ) ;
#20407 = CARTESIAN_POINT ( 'NONE',  ( 8.222936768550598075, -16.65173181358981580, -36.46600169915504353 ) ) ;
#20408 = CARTESIAN_POINT ( 'NONE',  ( 66.53393739769619231, 10.88381105532070059, -69.34999999999999432 ) ) ;
#20409 = CARTESIAN_POINT ( 'NONE',  ( 68.13393739769630031, 1.883811055320669947, -70.34999999999999432 ) ) ;
#20410 = DIRECTION ( 'NONE',  ( 0.000000000000000000, 1.000000000000000000, 0.000000000000000000 ) ) ;
#20411 = CARTESIAN_POINT ( 'NONE',  ( 11.42785662796539903, -8.845995162762550379, -71.09897682385680184 ) ) ;
#20412 = CARTESIAN_POINT ( 'NONE',  ( 16.13393739769620083, -15.61618894467929941, -28.45282021618999835 ) ) ;
#20413 = DIRECTION ( 'NONE',  ( -0.000000000000000000, 1.000000000000000000, 0.000000000000000000 ) ) ;
#20414 =( NAMED_UNIT ( * ) SI_UNIT ( $, .STERADIAN. ) SOLID_ANGLE_UNIT ( ) );
#20415 = CARTESIAN_POINT ( 'NONE',  ( 46.48805971088770406, -53.10800393395699359, -76.13964794981698958 ) ) ;
#20416 = ORIENTED_EDGE ( 'NONE', *, *, #42112, .T. ) ;
#20417 = CARTESIAN_POINT ( 'NONE',  ( 22.87580916398269792, -12.44540688151340113, -64.09272310917850746 ) ) ;
#20418 = EDGE_CURVE ( 'NONE', #23799, #18800, #7004, .T. ) ;
#20419 = FACE_OUTER_BOUND ( 'NONE', #7981, .T. ) ;
#20420 = DIRECTION ( 'NONE',  ( 0.000000000000000000, 0.7071067811865457964, -0.7071067811865492381 ) ) ;
#20421 = EDGE_CURVE ( 'NONE', #12364, #33243, #14199, .T. ) ;
#20422 = AXIS2_PLACEMENT_3D ( 'NONE', #47017, #18950, #22355 ) ;
#20423 = CARTESIAN_POINT ( 'NONE',  ( 46.39225494580800557, 21.75266102372379962, -76.14870948285189911 ) ) ;
#20424 = CARTESIAN_POINT ( 'NONE',  ( 71.01106396815980304, 1.383811055320669947, -60.95624653118409242 ) ) ;
#20425 = EDGE_CURVE ( 'NONE', #12119, #33592, #21875, .T. ) ;
#20426 = CARTESIAN_POINT ( 'NONE',  ( 16.13393739769620083, -15.61618894467929941, 17.35000000000000142 ) ) ;
#20427 =( BOUNDED_CURVE ( )  B_SPLINE_CURVE ( 3, ( #17670, #17411, #22098, #6656 ),
 .UNSPECIFIED., .F., .T. ) 
 B_SPLINE_CURVE_WITH_KNOTS ( ( 4, 4 ),
 ( 5.135640914169340654, 7.430729701136489673 ),
 .UNSPECIFIED. ) 
 CURVE ( )  GEOMETRIC_REPRESENTATION_ITEM ( )  RATIONAL_B_SPLINE_CURVE ( ( 1.000000000000000000, 0.6071517307476801406, 0.6071517307476801406, 1.000000000000000000 ) ) 
 REPRESENTATION_ITEM ( '' )  );
#20428 = DIRECTION ( 'NONE',  ( -1.224646799147353207E-16, 1.000000000000000000, 0.000000000000000000 ) ) ;
#20429 = B_SPLINE_CURVE_WITH_KNOTS ( 'NONE', 3,
 ( #44513, #49497, #41102, #13584, #9403, #44251, #1008, #12818, #32688, #20911, #4420, #24565, #40579, #25091, #20648, #36634, #736, #45294 ),
 .UNSPECIFIED., .F., .F.,
 ( 4, 2, 2, 2, 2, 2, 2, 2, 4 ),
 ( 0.000000000000000000, 0.06249985449796188752, 0.1249997089959237750, 0.1874995634938856626, 0.2499994179918475501, 0.3124992724898094654, 0.3749991269877713251, 0.4374989814857331849, 0.4999988359836951002 ),
 .UNSPECIFIED. ) ;
#20430 = CARTESIAN_POINT ( 'NONE',  ( 16.91175549567909897, -23.82458219277760492, -73.97759560159089176 ) ) ;
#20431 = CARTESIAN_POINT ( 'NONE',  ( 56.79938825701810146, -50.61924877113020216, -75.12131854917910800 ) ) ;
#20433 = CARTESIAN_POINT ( 'NONE',  ( 30.55306054313505371, -35.64636550620694777, -84.61298601366885919 ) ) ;
#20432 = CARTESIAN_POINT ( 'NONE',  ( 57.24929578234380045, 19.38381105828390361, -53.91492796160409284 ) ) ;
#20434 = AXIS2_PLACEMENT_3D ( 'NONE', #591, #8727, #7952 ) ;
#20435 = CARTESIAN_POINT ( 'NONE',  ( 63.26414124932220062, 1.334812829108570131, -68.66140445374750811 ) ) ;
#20436 = CARTESIAN_POINT ( 'NONE',  ( 61.45699444135679812, 13.94749824582279984, -46.72613800703339848 ) ) ;
#20437 = CARTESIAN_POINT ( 'NONE',  ( 12.82281323259240047, -64.96593576180920593, -46.32794539105049836 ) ) ;
#20438 = ORIENTED_EDGE ( 'NONE', *, *, #20048, .F. ) ;
#20439 = CARTESIAN_POINT ( 'NONE',  ( 53.18486246474859769, -49.47487039336269987, -48.80133351323340207 ) ) ;
#20440 = CARTESIAN_POINT ( 'NONE',  ( 60.44012286426450942, -45.18239918516130160, -26.74847066535680185 ) ) ;
#20441 = CARTESIAN_POINT ( 'NONE',  ( 24.04496217889941789, -15.61618911842929869, -37.79232902657031445 ) ) ;
#20442 = CARTESIAN_POINT ( 'NONE',  ( 56.88244700999120340, 14.33082729724810100, -26.04504088914069726 ) ) ;
#20443 = CARTESIAN_POINT ( 'NONE',  ( 9.272726169787338435, -17.24908183236129844, -37.37844945019890019 ) ) ;
#20444 = CARTESIAN_POINT ( 'NONE',  ( 50.40317162242880045, 18.69648349058939729, -76.14999999999999147 ) ) ;
#20446 = ADVANCED_FACE ( 'NONE', ( #42335 ), #45503, .F. ) ;
#20445 = CARTESIAN_POINT ( 'NONE',  ( 53.29392286865769535, 18.19942959119120118, -48.95065426190299718 ) ) ;
#20447 = CARTESIAN_POINT ( 'NONE',  ( 71.13364007206789097, 1.371651820402789879, -70.41530492215990478 ) ) ;
#20448 = CARTESIAN_POINT ( 'NONE',  ( 53.55397377960559879, -51.73583884506710717, -53.25782589811129242 ) ) ;
#20449 = ORIENTED_EDGE ( 'NONE', *, *, #2098, .F. ) ;
#20450 = FACE_OUTER_BOUND ( 'NONE', #11602, .T. ) ;
#20451 = CARTESIAN_POINT ( 'NONE',  ( 47.76739131609710398, -54.44992707061860671, -54.84422872089319156 ) ) ;
#20452 = CARTESIAN_POINT ( 'NONE',  ( -8.924323233577288406, 12.96044049090009942, -5.352796889411019166 ) ) ;
#20453 = FACE_OUTER_BOUND ( 'NONE', #21109, .T. ) ;
#20454 = CARTESIAN_POINT ( 'NONE',  ( 61.33485920126659607, 14.38743525284970026, -47.69940821548620136 ) ) ;
#20455 = CARTESIAN_POINT ( 'NONE',  ( 71.38783905025799470, 1.187237555532410171, -60.72008782705600538 ) ) ;
#20456 = CARTESIAN_POINT ( 'NONE',  ( 18.38332337263111427, -52.17615710686938968, -75.56421430878999956 ) ) ;
#20457 = CARTESIAN_POINT ( 'NONE',  ( 72.07170057178599620, 1.030858001320090089, -61.12206023519150477 ) ) ;
#20458 = LINE ( 'NONE', #1344, #41910 ) ;
#20459 = CARTESIAN_POINT ( 'NONE',  ( 64.92397392854900318, 1.188582381068110205, -70.60520998597918663 ) ) ;
#20460 = ORIENTED_EDGE ( 'NONE', *, *, #5721, .F. ) ;
#20461 = ORIENTED_EDGE ( 'NONE', *, *, #28733, .T. ) ;
#20462 = CIRCLE ( 'NONE', #50643, 6.000000000000005329 ) ;
#20463 = CARTESIAN_POINT ( 'NONE',  ( 14.25092084710789919, -51.11945063272739276, -22.60339915794170196 ) ) ;
#20464 = CARTESIAN_POINT ( 'NONE',  ( 8.222937397696199469, -15.61618894467929941, -32.14999999999999858 ) ) ;
#20465 = B_SPLINE_CURVE_WITH_KNOTS ( 'NONE', 3,
 ( #16751, #1286, #45571, #41117, #17021, #5231, #9664, #32703, #41371, #12835 ),
 .UNSPECIFIED., .F., .F.,
 ( 4, 2, 2, 2, 4 ),
 ( -0.0003767167459391999786, 0.000000000000000000, 0.01529901560024879946, 0.03030530679091670079, 0.04513248637320322471 ),
 .UNSPECIFIED. ) ;
#20466 = ORIENTED_EDGE ( 'NONE', *, *, #29963, .F. ) ;
#20467 = CARTESIAN_POINT ( 'NONE',  ( 16.13393739769620083, -15.61618894467929941, -28.45282021618999835 ) ) ;
#20468 = FACE_OUTER_BOUND ( 'NONE', #43229, .T. ) ;
#20469 = CARTESIAN_POINT ( 'NONE',  ( 20.24159734950449518, -10.16604498721250138, -50.15866389318657070 ) ) ;
#20470 = ORIENTED_EDGE ( 'NONE', *, *, #3756, .T. ) ;
#20471 = CARTESIAN_POINT ( 'NONE',  ( 61.28610861176739633, 13.99802266614350010, -46.37203261889099792 ) ) ;
#20472 = CARTESIAN_POINT ( 'NONE',  ( 14.31997823940066183, -9.037193765400974854, -71.86747918995368423 ) ) ;
#20473 = CARTESIAN_POINT ( 'NONE',  ( 61.13405154998650204, 14.40638383414069956, -47.71032547765840093 ) ) ;
#20474 = CARTESIAN_POINT ( 'NONE',  ( 23.95032869375090101, -12.99192768426819988, -43.68922667584449471 ) ) ;
#20475 = CARTESIAN_POINT ( 'NONE',  ( 45.27534771981950001, 2.448353903276920374, -34.68491900127439465 ) ) ;
#20476 = AXIS2_PLACEMENT_3D ( 'NONE', #35531, #3307, #23448 ) ;
#20477 = CARTESIAN_POINT ( 'NONE',  ( 42.51983742818366352, -37.70581418102509019, -77.72045495091650480 ) ) ;
#20478 = ORIENTED_EDGE ( 'NONE', *, *, #3507, .F. ) ;
#20479 = CARTESIAN_POINT ( 'NONE',  ( 11.07146966777600028, -64.97230528211619571, -23.11170492349029715 ) ) ;
#20480 = CARTESIAN_POINT ( 'NONE',  ( 8.691576068919250275, -15.95962985236369924, -39.21797875520199739 ) ) ;
#20481 = DIRECTION ( 'NONE',  ( -1.000000000000000000, 0.000000000000000000, 0.000000000000000000 ) ) ;
#20482 = EDGE_CURVE ( 'NONE', #33390, #42519, #47199, .T. ) ;
#20483 = B_SPLINE_CURVE_WITH_KNOTS ( 'NONE', 3,
 ( #50920, #46230, #27061, #26280, #38351, #6641, #22347, #30728, #14244, #18684, #10835, #24067, #34658, #50664, #14759, #3938 ),
 .UNSPECIFIED., .F., .F.,
 ( 4, 2, 2, 2, 2, 2, 2, 4 ),
 ( -8.880243999999999390E-15, 0.07216186899280199740, 0.1546325764131560032, 0.2061767685508779924, 0.2319488646197390147, 0.2731842183299159621, 0.3391607842661999994, 0.4123535371017650331 ),
 .UNSPECIFIED. ) ;
#20484 = CARTESIAN_POINT ( 'NONE',  ( 14.47481033283960095, 20.39333564065439930, -75.48537863783369062 ) ) ;
#20485 = EDGE_CURVE ( 'NONE', #37502, #3421, #32853, .T. ) ;
#20486 = CARTESIAN_POINT ( 'NONE',  ( 20.74197122344288502, -22.13452925154505024, -60.09665985822703504 ) ) ;
#20487 = CARTESIAN_POINT ( 'NONE',  ( 83.09574564639500238, -44.89486624088750233, -46.39644155595880193 ) ) ;
#20488 = CARTESIAN_POINT ( 'NONE',  ( 68.13393739769618662, -31.81618894467930403, -65.65000000000000568 ) ) ;
#20489 = CARTESIAN_POINT ( 'NONE',  ( 12.09455160279810038, -22.80410123608560014, -38.17063876083498997 ) ) ;
#20490 = ORIENTED_EDGE ( 'NONE', *, *, #39326, .T. ) ;
#20491 = CARTESIAN_POINT ( 'NONE',  ( 53.14742929986179831, -49.37086717498490174, -27.49438065588160285 ) ) ;
#20492 = CARTESIAN_POINT ( 'NONE',  ( 15.58442563903250111, -50.84470211311809607, -20.41433498000790081 ) ) ;
#20493 = CARTESIAN_POINT ( 'NONE',  ( 23.76540053402172248, -17.76641857869638841, -39.59512095345433380 ) ) ;
#20494 = FACE_OUTER_BOUND ( 'NONE', #38155, .T. ) ;
#20495 = CARTESIAN_POINT ( 'NONE',  ( 19.82873695480376242, -9.608609115219810093, -56.52269350815382154 ) ) ;
#20496 = CARTESIAN_POINT ( 'NONE',  ( 8.222872596472118545, -15.61638977992110000, -80.50766849176289952 ) ) ;
#20497 = VERTEX_POINT ( 'NONE', #7058 ) ;
#20498 = CARTESIAN_POINT ( 'NONE',  ( -4.162343151726740409, -48.30019726062069907, -5.617366207439410175 ) ) ;
#20499 = CARTESIAN_POINT ( 'NONE',  ( 47.42380321553230260, 23.40185720734870145, -54.69111192316769632 ) ) ;
#20500 = CARTESIAN_POINT ( 'NONE',  ( 22.90093741960866325, -16.50197990757633448, -48.49448879811394875 ) ) ;
#20501 = CARTESIAN_POINT ( 'NONE',  ( 63.15706468848460275, 1.190292248953970011, -62.47835652209879953 ) ) ;
#20502 = CARTESIAN_POINT ( 'NONE',  ( 55.35733030022484513, 16.14712512605141725, -26.51179285998376756 ) ) ;
#20503 = FACE_OUTER_BOUND ( 'NONE', #10581, .T. ) ;
#20504 = CARTESIAN_POINT ( 'NONE',  ( 16.13393739769620083, -15.61618894467929941, -28.45282021618999835 ) ) ;
#20506 = EDGE_CURVE ( 'NONE', #51641, #47003, #49788, .T. ) ;
#20505 = CARTESIAN_POINT ( 'NONE',  ( 14.36278465922390701, -22.20708669663512325, -65.03615447382929915 ) ) ;
#20507 = CARTESIAN_POINT ( 'NONE',  ( 72.70504696988909643, 1.400446703427080219, -62.40275391609110756 ) ) ;
#20508 = CARTESIAN_POINT ( 'NONE',  ( 55.20295770280799275, -48.56198109356999737, -48.76073667618629770 ) ) ;
#20509 = CARTESIAN_POINT ( 'NONE',  ( 24.04424242478976836, -15.50292783389250317, -75.78776975939635463 ) ) ;
#20510 = CARTESIAN_POINT ( 'NONE',  ( 64.97340239734420209, 1.393731187554809958, -61.04935521477050031 ) ) ;
#20511 = CARTESIAN_POINT ( 'NONE',  ( 17.36235827195499937, -52.98917440366089693, -76.14999999999999147 ) ) ;
#20512 = ADVANCED_FACE ( 'NONE', ( #11319 ), #39623, .F. ) ;
#20513 = CARTESIAN_POINT ( 'NONE',  ( 23.83903859056454522, -13.54551801267896671, -73.42433450828966102 ) ) ;
#20514 = CARTESIAN_POINT ( 'NONE',  ( 9.367442997458502063, -15.61610373232760018, -47.45282021618999835 ) ) ;
#20515 = ORIENTED_EDGE ( 'NONE', *, *, #27902, .F. ) ;
#20516 = DIRECTION ( 'NONE',  ( 0.000000000000000000, 0.000000000000000000, 1.000000000000000000 ) ) ;
#20517 = CARTESIAN_POINT ( 'NONE',  ( 10.48523087532110054, 31.88305279702909800, -45.62962604688630108 ) ) ;
#20518 = CARTESIAN_POINT ( 'NONE',  ( 16.13393739769620083, -15.61618894467929941, -54.64999999999999858 ) ) ;
#20519 = CARTESIAN_POINT ( 'NONE',  ( 68.23802800759220588, -31.42890113106329508, -18.38247165234229996 ) ) ;
#20520 = ORIENTED_EDGE ( 'NONE', *, *, #2718, .T. ) ;
#20521 = CARTESIAN_POINT ( 'NONE',  ( 18.45619610651039721, 20.68589454807339933, -75.38352342698830455 ) ) ;
#20522 = ORIENTED_EDGE ( 'NONE', *, *, #43940, .F. ) ;
#20523 = VERTEX_POINT ( 'NONE', #7644 ) ;
#20524 = VERTEX_POINT ( 'NONE', #35676 ) ;
#20525 = CARTESIAN_POINT ( 'NONE',  ( 11.65161691330369997, -64.97831056663849836, -46.09346701959520232 ) ) ;
#20526 = DIRECTION ( 'NONE',  ( 0.000000000000000000, -1.000000000000000000, 0.000000000000000000 ) ) ;
#20527 = CARTESIAN_POINT ( 'NONE',  ( 21.63843781001559918, -20.05973176279620063, -81.23899999999999011 ) ) ;
#20528 = CARTESIAN_POINT ( 'NONE',  ( 56.83411512905762919, -46.90160822220050818, -26.73578643762690277 ) ) ;
#20529 = CARTESIAN_POINT ( 'NONE',  ( 0.4142048468714032983, -8.849798201630209249, -35.10658870009234533 ) ) ;
#20530 = ORIENTED_EDGE ( 'NONE', *, *, #13335, .F. ) ;
#20531 = CARTESIAN_POINT ( 'NONE',  ( 75.25317828858366909, 3.262240055439041608, -12.30554431910427304 ) ) ;
#20532 = AXIS2_PLACEMENT_3D ( 'NONE', #49021, #8399, #20684 ) ;
#20533 = DIRECTION ( 'NONE',  ( 0.4999999999999998890, -0.8660254037844387076, 0.000000000000000000 ) ) ;
#20534 = VERTEX_POINT ( 'NONE', #24095 ) ;
#20535 = CARTESIAN_POINT ( 'NONE',  ( 22.89998542976507778, -14.84672387926992343, -42.81098146774382940 ) ) ;
#20536 = VECTOR ( 'NONE', #19863, 1000.000000000000114 ) ;
#20537 = CARTESIAN_POINT ( 'NONE',  ( 59.48252993831315649, -45.49665726213240902, -26.72040254028946649 ) ) ;
#20538 = ORIENTED_EDGE ( 'NONE', *, *, #49913, .F. ) ;
#20539 = ORIENTED_EDGE ( 'NONE', *, *, #39154, .T. ) ;
#20540 = CARTESIAN_POINT ( 'NONE',  ( 22.13393739769619728, -54.15188668067469990, -35.14999999999999858 ) ) ;
#20541 = CARTESIAN_POINT ( 'NONE',  ( 38.67452568954050207, -37.56081407618439982, -81.65000000000000568 ) ) ;
#20542 = CARTESIAN_POINT ( 'NONE',  ( 73.01379001973170091, 13.72769019945460123, -13.76114987980459858 ) ) ;
#20543 = CARTESIAN_POINT ( 'NONE',  ( 47.96938416189519216, 13.96888898634079901, -9.741253716576860455 ) ) ;
#20544 = EDGE_CURVE ( 'NONE', #27800, #9084, #44828, .T. ) ;
#20545 = DIRECTION ( 'NONE',  ( 0.000000000000000000, 0.000000000000000000, 1.000000000000000000 ) ) ;
#20546 = CARTESIAN_POINT ( 'NONE',  ( -8.918955708164858720, 12.96516353870340055, -5.380344673046240977 ) ) ;
#20548 = CIRCLE ( 'NONE', #24731, 5.499999999999998224 ) ;
#20547 = CARTESIAN_POINT ( 'NONE',  ( 1.127242003616780508, -53.29999274968538714, -7.495163844720678092 ) ) ;
#20549 = CARTESIAN_POINT ( 'NONE',  ( 61.05354884778520130, 14.03248421730429918, -27.55223363601019670 ) ) ;
#20550 = CARTESIAN_POINT ( 'NONE',  ( 18.00830954542770002, -7.995593348861908645, -58.86427365897959163 ) ) ;
#20551 = ORIENTED_EDGE ( 'NONE', *, *, #7682, .T. ) ;
#20552 = CARTESIAN_POINT ( 'NONE',  ( 60.24058964203619837, 14.54579934782940143, -47.32689780713820227 ) ) ;
#20553 = CARTESIAN_POINT ( 'NONE',  ( 43.05762310336380239, 14.74520815673739982, -7.621878241775270624 ) ) ;
#20554 = LINE ( 'NONE', #36550, #47143 ) ;
#20555 = CARTESIAN_POINT ( 'NONE',  ( 72.36538891291519349, 1.347758125946150187, -69.74822197408450108 ) ) ;
#20556 = CARTESIAN_POINT ( 'NONE',  ( 43.46623457429583226, -39.90877955095767504, -69.24476199280557864 ) ) ;
#20557 = CARTESIAN_POINT ( 'NONE',  ( 10.97564840259020080, -65.00352292546099875, -17.33480504156820245 ) ) ;
#20558 = AXIS2_PLACEMENT_3D ( 'NONE', #18777, #19035, #35543 ) ;
#20559 = CARTESIAN_POINT ( 'NONE',  ( 12.82083315176570082, 18.86661839715909750, -21.11500886439040059 ) ) ;
#20561 = EDGE_CURVE ( 'NONE', #2182, #48970, #10336, .T. ) ;
#20560 = CARTESIAN_POINT ( 'NONE',  ( 46.89722913963129969, 22.92670556637019885, -75.65864051473879215 ) ) ;
#20562 = CARTESIAN_POINT ( 'NONE',  ( 49.39745668169630477, -53.63492652054119958, -54.43253521562210295 ) ) ;
#20563 = CIRCLE ( 'NONE', #31452, 2.999999999999997780 ) ;
#20564 = CYLINDRICAL_SURFACE ( 'NONE', #3018, 20.79999999999999716 ) ;
#20565 = CARTESIAN_POINT ( 'NONE',  ( 11.49584328075813922, -22.05115804159764181, -34.20649648869382276 ) ) ;
#20566 = FACE_OUTER_BOUND ( 'NONE', #30839, .T. ) ;
#20567 = EDGE_CURVE ( 'NONE', #26995, #41285, #42274, .T. ) ;
#20568 = CARTESIAN_POINT ( 'NONE',  ( 56.07568765954189871, 13.88381105532070059, -14.74720511883509921 ) ) ;
#20569 = EDGE_LOOP ( 'NONE', ( #20723, #28972, #14751, #30319, #22341 ) ) ;
#20570 = CARTESIAN_POINT ( 'NONE',  ( 21.11303220515950230, -10.07404953497180067, -42.80032454360480187 ) ) ;
#20571 = CARTESIAN_POINT ( 'NONE',  ( 64.14956774380819127, 1.407740700961959801, -61.39510741658510540 ) ) ;
#20572 = EDGE_LOOP ( 'NONE', ( #22987, #1011, #46922, #32175 ) ) ;
#20573 = DIRECTION ( 'NONE',  ( -1.000000000000000000, 0.000000000000000000, 0.000000000000000000 ) ) ;
#20574 = CARTESIAN_POINT ( 'NONE',  ( 60.54364033361749620, -45.62202010502980443, -47.24421774848470079 ) ) ;
#20575 = CARTESIAN_POINT ( 'NONE',  ( 23.32557412215919967, 18.09884784672449953, -34.65000333295999724 ) ) ;
#20576 = CARTESIAN_POINT ( 'NONE',  ( 50.34328701401641126, -43.49848369320205421, -6.583824542005403124 ) ) ;
#20578 = CARTESIAN_POINT ( 'NONE',  ( 8.428822758898967038, -17.68681539623817400, -78.70899791345021868 ) ) ;
#20577 = CARTESIAN_POINT ( 'NONE',  ( 41.80405099542780789, 8.510870798982260510, -77.27697826269607617 ) ) ;
#20579 = DIRECTION ( 'NONE',  ( -2.565320000000000120E-13, -1.000000000000000000, 8.628712999999999808E-13 ) ) ;
#20580 = DIRECTION ( 'NONE',  ( -0.05023550054956202326, 0.000000000000000000, 0.9987374001630934250 ) ) ;
#20581 = ORIENTED_EDGE ( 'NONE', *, *, #24481, .T. ) ;
#20582 = CARTESIAN_POINT ( 'NONE',  ( 84.20053740572899414, -44.11518990482350233, -47.28523898137510173 ) ) ;
#20583 = VERTEX_POINT ( 'NONE', #2093 ) ;
#20584 = VERTEX_POINT ( 'NONE', #29596 ) ;
#20585 = CARTESIAN_POINT ( 'NONE',  ( 61.67800232651970305, -45.19184251940130537, -46.93943497666659681 ) ) ;
#20586 = CARTESIAN_POINT ( 'NONE',  ( 53.12243681351169755, -49.57385822095360339, -49.13999347672969975 ) ) ;
#20587 = CARTESIAN_POINT ( 'NONE',  ( 17.52154708603973887, -14.60803149382545563, -170.7999095292539948 ) ) ;
#20588 = CARTESIAN_POINT ( 'NONE',  ( 76.44636341052239459, -6.604837239822047401, -12.99629018861355156 ) ) ;
#20589 = CARTESIAN_POINT ( 'NONE',  ( 53.13499564549729826, -52.07858566517519705, -53.65455749828319654 ) ) ;
#20590 = VECTOR ( 'NONE', #22040, 1000.000000000000114 ) ;
#20591 = ORIENTED_EDGE ( 'NONE', *, *, #40865, .F. ) ;
#20592 = ORIENTED_EDGE ( 'NONE', *, *, #50840, .F. ) ;
#20593 = CARTESIAN_POINT ( 'NONE',  ( 12.14969237204626573, -22.52864793124346932, -56.17427643643699042 ) ) ;
#20594 = CIRCLE ( 'NONE', #49916, 1.999999999999999334 ) ;
#20595 = DIRECTION ( 'NONE',  ( 1.000000000000000000, 0.000000000000000000, 0.000000000000000000 ) ) ;
#20596 = CARTESIAN_POINT ( 'NONE',  ( 13.88443978363049069, -50.25762978063119846, -20.90776614285152846 ) ) ;
#20597 = DIRECTION ( 'NONE',  ( 0.000000000000000000, 0.000000000000000000, 1.000000000000000000 ) ) ;
#20598 = FACE_OUTER_BOUND ( 'NONE', #24399, .T. ) ;
#20599 = CARTESIAN_POINT ( 'NONE',  ( 51.99248274614070198, -49.49756876763530045, -77.11023451094040126 ) ) ;
#20600 = ORIENTED_EDGE ( 'NONE', *, *, #37084, .T. ) ;
#20601 = CARTESIAN_POINT ( 'NONE',  ( 52.98832978415040174, -50.41796700477780746, -76.96373676954098642 ) ) ;
#20602 = CARTESIAN_POINT ( 'NONE',  ( 64.85894149894419058, 0.8879664753683389478, -70.67740027405400838 ) ) ;
#20603 = DIRECTION ( 'NONE',  ( 0.000000000000000000, 0.000000000000000000, -1.000000000000000000 ) ) ;
#20604 = VECTOR ( 'NONE', #24943, 999.9999999999998863 ) ;
#20605 = CARTESIAN_POINT ( 'NONE',  ( 14.77119402760449951, -7.887691154108790847, -65.45693882779990247 ) ) ;
#20606 = CIRCLE ( 'NONE', #17304, 2.000000000000001776 ) ;
#20607 = DIRECTION ( 'NONE',  ( 0.000000000000000000, 1.000000000000000000, 0.000000000000000000 ) ) ;
#20608 = DIRECTION ( 'NONE',  ( 0.000000000000000000, -0.9319748226751467524, 0.3625230060280709155 ) ) ;
#20609 = ADVANCED_FACE ( 'NONE', ( #10218 ), #26178, .T. ) ;
#20610 = CARTESIAN_POINT ( 'NONE',  ( 42.60880853662280288, -43.93543342225530068, -4.906336349381930084 ) ) ;
#20611 = DIRECTION ( 'NONE',  ( 0.000000000000000000, 0.000000000000000000, -1.000000000000000000 ) ) ;
#20612 = CARTESIAN_POINT ( 'NONE',  ( -0.02503409344755289437, -27.07639387936528763, -34.78823607925544081 ) ) ;
#20614 = EDGE_CURVE ( 'NONE', #19589, #20020, #39657, .T. ) ;
#20613 = CARTESIAN_POINT ( 'NONE',  ( 61.30653360879629332, -45.38759780313989722, -47.35768905649830174 ) ) ;
#20615 = EDGE_CURVE ( 'NONE', #9229, #23989, #36300, .T. ) ;
#20616 = CARTESIAN_POINT ( 'NONE',  ( 64.07626989212400304, 1.443555451352130037, -69.77608189653500403 ) ) ;
#20617 = CARTESIAN_POINT ( 'NONE',  ( 9.807869143058068673, -10.75438648984616385, -41.00066472165191556 ) ) ;
#20618 = EDGE_CURVE ( 'NONE', #50796, #30215, #19361, .T. ) ;
#20619 = ORIENTED_EDGE ( 'NONE', *, *, #41923, .F. ) ;
#20620 = CARTESIAN_POINT ( 'NONE',  ( 14.07179683629490086, -52.32664520840259570, -75.76244777734170555 ) ) ;
#20621 = CARTESIAN_POINT ( 'NONE',  ( 47.28175591391539712, -54.73378013403499409, -54.73619099792320242 ) ) ;
#20622 = CARTESIAN_POINT ( 'NONE',  ( 13.00893739761190027, 34.28605925116320208, -47.75434321210310173 ) ) ;
#20623 = DIRECTION ( 'NONE',  ( 0.000000000000000000, 0.000000000000000000, -1.000000000000000000 ) ) ;
#20624 = CARTESIAN_POINT ( 'NONE',  ( 61.02432256287157486, -45.45604146479874430, -47.36561844619770767 ) ) ;
#20625 = CIRCLE ( 'NONE', #1384, 20.00000000000000355 ) ;
#20626 = CARTESIAN_POINT ( 'NONE',  ( 22.56027083402119970, -12.69968737826519956, -32.14999999999999858 ) ) ;
#20627 = CARTESIAN_POINT ( 'NONE',  ( 24.58073416742070094, -18.76089852590099838, -35.14999999999999858 ) ) ;
#20628 = B_SPLINE_CURVE_WITH_KNOTS ( 'NONE', 3,
 ( #10728, #19354, #31130, #51074, #23261, #31900, #7059, #42705, #31385, #51336, #26681, #47413, #43725, #11507 ),
 .UNSPECIFIED., .F., .F.,
 ( 4, 2, 2, 2, 2, 2, 4 ),
 ( 11.92140392297045892, 18.73771508492814419, 24.98362011319689202, 28.10657262733126416, 33.10329664994625887, 41.09805508613030867, 41.83711151413364604 ),
 .UNSPECIFIED. ) ;
#20629 = CARTESIAN_POINT ( 'NONE',  ( 11.91450189635799894, 34.20545694164769657, -17.98631677231880133 ) ) ;
#20631 = CARTESIAN_POINT ( 'NONE',  ( 22.46012192026008591, -20.47784040582451226, -73.71600126361178695 ) ) ;
#20630 = FACE_OUTER_BOUND ( 'NONE', #46408, .T. ) ;
#20632 = CARTESIAN_POINT ( 'NONE',  ( 56.46551649800760231, 19.54378829069240098, -53.85224769578630344 ) ) ;
#20633 = CARTESIAN_POINT ( 'NONE',  ( 42.80890084343171509, 12.86785355401084807, -5.063862465213780695 ) ) ;
#20634 = ADVANCED_FACE ( 'NONE', ( #14916 ), #27734, .T. ) ;
#20635 = CARTESIAN_POINT ( 'NONE',  ( 48.59288953467110161, 22.89722549970059617, -55.31247818475549849 ) ) ;
#20636 = EDGE_LOOP ( 'NONE', ( #28262, #4878 ) ) ;
#20637 = CARTESIAN_POINT ( 'NONE',  ( 20.44176770788429920, -21.20055615977860342, -67.13803027067579876 ) ) ;
#20638 = ORIENTED_EDGE ( 'NONE', *, *, #30396, .T. ) ;
#20639 = CARTESIAN_POINT ( 'NONE',  ( 2.543036500622879892, -5.976568861398989796, -34.65032322548090349 ) ) ;
#20640 = AXIS2_PLACEMENT_3D ( 'NONE', #1014, #238, #36382 ) ;
#20641 = CARTESIAN_POINT ( 'NONE',  ( 64.93393739769599904, 1.396834109478129804, -61.06337307536569625 ) ) ;
#20642 = CYLINDRICAL_SURFACE ( 'NONE', #15364, 5.000000000000000000 ) ;
#20644 = CARTESIAN_POINT ( 'NONE',  ( 56.02287817249710145, 14.72004393977189984, -25.81294518235560176 ) ) ;
#20643 = CARTESIAN_POINT ( 'NONE',  ( 83.66401895982369297, 13.28260268565369984, -46.61643406624119734 ) ) ;
#20645 = CARTESIAN_POINT ( 'NONE',  ( 9.852363362552399195, -18.82311681066459741, -61.30256663141189932 ) ) ;
#20646 = CARTESIAN_POINT ( 'NONE',  ( 70.99050876911339003, 1.383811055320669947, -70.34999999999999432 ) ) ;
#20647 = CARTESIAN_POINT ( 'NONE',  ( 54.85121201869780094, -45.70040766398989973, -15.57405995174110025 ) ) ;
#20648 = CARTESIAN_POINT ( 'NONE',  ( 23.04647616065052773, -19.60029129190153441, -79.95900011493084492 ) ) ;
#20649 = ORIENTED_EDGE ( 'NONE', *, *, #31232, .T. ) ;
#20650 = B_SPLINE_CURVE_WITH_KNOTS ( 'NONE', 3,
 ( #14227, #29929, #30199, #30453 ),
 .UNSPECIFIED., .F., .F.,
 ( 4, 4 ),
 ( 0.000000000000000000, 1.000000000000000000 ),
 .UNSPECIFIED. ) ;
#20651 = ORIENTED_EDGE ( 'NONE', *, *, #38931, .T. ) ;
#20652 = CARTESIAN_POINT ( 'NONE',  ( 11.82286116600939962, -65.20082272508568622, -16.82382485989019827 ) ) ;
#20653 = CARTESIAN_POINT ( 'NONE',  ( 10.97424772006000104, 33.59586616593779951, -46.68812779134029967 ) ) ;
#20654 = CARTESIAN_POINT ( 'NONE',  ( 73.01625195241490474, 1.007912009470880221, -62.17370354086050099 ) ) ;
#20655 = CARTESIAN_POINT ( 'NONE',  ( 48.31794077192549963, -54.26005012469399702, -54.97046006864109557 ) ) ;
#20656 = CARTESIAN_POINT ( 'NONE',  ( 11.27237402512278130, -21.94244088919472446, -64.21600230519077002 ) ) ;
#20657 = EDGE_CURVE ( 'NONE', #41343, #48021, #44696, .T. ) ;
#20658 = VERTEX_POINT ( 'NONE', #43732 ) ;
#20659 = FACE_OUTER_BOUND ( 'NONE', #25025, .T. ) ;
#20660 = CARTESIAN_POINT ( 'NONE',  ( 60.70500520956167634, -60.18725675654477669, 11.84999999999999964 ) ) ;
#20661 = FACE_OUTER_BOUND ( 'NONE', #6483, .T. ) ;
#20662 = DIRECTION ( 'NONE',  ( 0.000000000000000000, 1.000000000000000000, 0.000000000000000000 ) ) ;
#20663 = CARTESIAN_POINT ( 'NONE',  ( 50.45186351439279804, -50.03424225457590069, -76.14999999999999147 ) ) ;
#20664 = DIRECTION ( 'NONE',  ( -0.7071067811865476838, -0.7071067811865473507, 0.000000000000000000 ) ) ;
#20665 = ORIENTED_EDGE ( 'NONE', *, *, #11943, .F. ) ;
#20666 = DIRECTION ( 'NONE',  ( 1.000000000000000000, 8.402539340422012971E-12, -1.224645651945156590E-16 ) ) ;
#20667 = DIRECTION ( 'NONE',  ( 0.000000000000000000, 0.7071067811865492381, -0.7071067811865457964 ) ) ;
#20668 = ORIENTED_EDGE ( 'NONE', *, *, #48877, .F. ) ;
#20669 = CARTESIAN_POINT ( 'NONE',  ( 29.63393739769620083, -15.61618894467929941, -8.655000000000001137 ) ) ;
#20670 = CARTESIAN_POINT ( 'NONE',  ( 15.67962062493570130, 19.63028992856250099, -15.65622423491010196 ) ) ;
#20671 = CARTESIAN_POINT ( 'NONE',  ( 22.51625110737120039, -20.83622647014099982, -76.01055054980119507 ) ) ;
#20672 = CARTESIAN_POINT ( 'NONE',  ( 22.71567673004141596, -17.77000726670902253, -64.94847198785556941 ) ) ;
#20673 = CARTESIAN_POINT ( 'NONE',  ( 54.11848747779500002, 20.00241981255700097, -75.47262416762160342 ) ) ;
#20674 = CARTESIAN_POINT ( 'NONE',  ( 47.30205888664269764, -54.42250278362140392, -75.11586948118589646 ) ) ;
#20675 = ORIENTED_EDGE ( 'NONE', *, *, #11084, .F. ) ;
#20676 = CARTESIAN_POINT ( 'NONE',  ( 10.22103832233932863, -19.02420151566214912, -37.28615309265127564 ) ) ;
#20677 = EDGE_CURVE ( 'NONE', #9983, #43315, #41332, .T. ) ;
#20678 = CARTESIAN_POINT ( 'NONE',  ( 19.34704915299079886, -8.894388095715280329, -61.87459303939719746 ) ) ;
#20679 = CARTESIAN_POINT ( 'NONE',  ( 47.13393739769619373, -36.11618894467930119, -35.14999999999999858 ) ) ;
#20680 = CARTESIAN_POINT ( 'NONE',  ( 12.32811467040465203, 34.12052296847067367, -23.60606026631527143 ) ) ;
#20681 = EDGE_CURVE ( 'NONE', #38311, #35304, #35510, .T. ) ;
#20682 = CARTESIAN_POINT ( 'NONE',  ( 46.37388399891210611, 21.71424375792910055, -76.14999999999999147 ) ) ;
#20683 = DIRECTION ( 'NONE',  ( 0.000000000000000000, 0.000000000000000000, 1.000000000000000000 ) ) ;
#20684 = DIRECTION ( 'NONE',  ( 1.000000000000000000, 0.000000000000000000, 0.000000000000000000 ) ) ;
#20685 = CARTESIAN_POINT ( 'NONE',  ( 28.63604668330599878, -4.677882819536359982, -34.65000333679609668 ) ) ;
#20686 = CARTESIAN_POINT ( 'NONE',  ( 24.36963727833509807, -16.01111688394609800, -79.52292077604440124 ) ) ;
#20687 = CARTESIAN_POINT ( 'NONE',  ( 56.27102044028909944, 19.34483705538490028, -52.87264067008490542 ) ) ;
#20689 = CARTESIAN_POINT ( 'NONE',  ( 42.64825840273801560, -39.90276718693228730, -72.90723142289991188 ) ) ;
#20688 = CARTESIAN_POINT ( 'NONE',  ( 16.13393739707289853, -15.61618894541809865, -10.45000000021869901 ) ) ;
#20690 = CARTESIAN_POINT ( 'NONE',  ( 63.13973003289760300, 0.9958340104639701318, -68.96201750760249638 ) ) ;
#20691 = CARTESIAN_POINT ( 'NONE',  ( 61.57009831922090370, 13.89954555936719949, -46.42185750248089704 ) ) ;
#20692 = CARTESIAN_POINT ( 'NONE',  ( 22.46011490975228497, -10.75452786398427918, -79.29933665554652578 ) ) ;
#20693 = ADVANCED_FACE ( 'NONE', ( #43984 ), #8090, .F. ) ;
#20694 = CARTESIAN_POINT ( 'NONE',  ( 12.93945173865840204, -65.41176199011280801, -46.97472070025159496 ) ) ;
#20695 = ORIENTED_EDGE ( 'NONE', *, *, #19092, .F. ) ;
#20696 = CARTESIAN_POINT ( 'NONE',  ( 52.85389961514279378, -49.65025774184390173, -48.74486371238739935 ) ) ;
#20697 = CARTESIAN_POINT ( 'NONE',  ( 61.58984863193099812, -45.12803552000509910, -28.15126211424280100 ) ) ;
#20698 = CARTESIAN_POINT ( 'NONE',  ( 53.63393739769619373, 30.88381105532059934, 11.84999999999999964 ) ) ;
#20699 = CARTESIAN_POINT ( 'NONE',  ( 13.17518462309900151, 19.66209683819560183, -21.60491894709759819 ) ) ;
#20700 = CARTESIAN_POINT ( 'NONE',  ( 56.69484138974510046, 14.42054476167730215, -26.04356117224130074 ) ) ;
#20701 = CARTESIAN_POINT ( 'NONE',  ( 16.12703488906409888, -8.563351852316490209, -35.95250869105369418 ) ) ;
#20702 = CARTESIAN_POINT ( 'NONE',  ( 50.98146089766679978, 18.17698877489110032, -76.31995468916950642 ) ) ;
#20703 = CARTESIAN_POINT ( 'NONE',  ( 53.42160460796090149, 18.12642228866929983, -48.88221542113920037 ) ) ;
#20704 = CARTESIAN_POINT ( 'NONE',  ( 71.19526263826620038, 1.274277262446069869, -70.59881390902160092 ) ) ;
#20705 = DIRECTION ( 'NONE',  ( -0.2260571801428161165, 1.249000902703300368E-16, 0.9741140340359943917 ) ) ;
#20706 = CARTESIAN_POINT ( 'NONE',  ( 68.57574012094990223, -45.11618894467940066, -13.49754435276109987 ) ) ;
#20707 = ORIENTED_EDGE ( 'NONE', *, *, #28926, .F. ) ;
#20708 = CARTESIAN_POINT ( 'NONE',  ( 22.90092414372679386, -15.63002194425144964, -40.45347516367851171 ) ) ;
#20709 = CARTESIAN_POINT ( 'NONE',  ( 9.557636492705340103, -19.11746881714849877, -59.91161365334649958 ) ) ;
#20710 = CARTESIAN_POINT ( 'NONE',  ( 73.08848314165430793, 0.9307121176571799825, -69.03423516236559010 ) ) ;
#20711 = CARTESIAN_POINT ( 'NONE',  ( 47.61217947097659930, -54.50984741584490223, -54.68372563208449577 ) ) ;
#20712 = CARTESIAN_POINT ( 'NONE',  ( 22.90097009252848892, -15.61618913824531418, -68.84717732178738459 ) ) ;
#20713 = CARTESIAN_POINT ( 'NONE',  ( 73.26121012496899709, 0.8838110553206759423, -62.53374032209040223 ) ) ;
#20714 = CARTESIAN_POINT ( 'NONE',  ( 41.72053738002289691, 12.47914145849190071, -3.400228433360679592 ) ) ;
#20715 = CARTESIAN_POINT ( 'NONE',  ( 59.80688163256760248, 15.43365568175059899, -48.65827547727460001 ) ) ;
#20716 = CARTESIAN_POINT ( 'NONE',  ( 71.32344782937069283, 1.326324093417210248, -60.85906821647699871 ) ) ;
#20717 = CYLINDRICAL_SURFACE ( 'NONE', #7432, 0.4999999999999994449 ) ;
#20718 = CARTESIAN_POINT ( 'NONE',  ( 72.00787155028980635, 0.9860880133278678850, -61.06736746306660280 ) ) ;
#20719 = AXIS2_PLACEMENT_3D ( 'NONE', #38940, #51751, #11934 ) ;
#20720 = EDGE_CURVE ( 'NONE', #26662, #6044, #22917, .T. ) ;
#20721 = DIRECTION ( 'NONE',  ( 0.8660254037844379305, -0.5000000000000011102, -2.498001805406606160E-16 ) ) ;
#20722 = CARTESIAN_POINT ( 'NONE',  ( 64.93204900141920177, 0.9940695285616559795, -70.71491496446259362 ) ) ;
#20723 = ORIENTED_EDGE ( 'NONE', *, *, #9104, .T. ) ;
#20724 = EDGE_CURVE ( 'NONE', #42519, #30599, #11236, .T. ) ;
#20725 = VERTEX_POINT ( 'NONE', #25072 ) ;
#20726 = CARTESIAN_POINT ( 'NONE',  ( 8.222373579151801337, -15.61629175287649929, -54.79233150823699816 ) ) ;
#20727 = AXIS2_PLACEMENT_3D ( 'NONE', #32038, #35991, #47549 ) ;
#20728 = CARTESIAN_POINT ( 'NONE',  ( 16.13393739769620083, -15.61618894467929941, -28.45282021618999835 ) ) ;
#20729 = ORIENTED_EDGE ( 'NONE', *, *, #14209, .T. ) ;
#20730 = DIRECTION ( 'NONE',  ( 2.375726999999999900E-16, -1.726067000000000108E-16, 1.000000000000000000 ) ) ;
#20731 = CARTESIAN_POINT ( 'NONE',  ( 56.50435945712200692, -45.38311456362110619, -25.29338994482560210 ) ) ;
#20732 = FACE_OUTER_BOUND ( 'NONE', #23693, .T. ) ;
#20733 = CARTESIAN_POINT ( 'NONE',  ( 52.47362269241929766, 19.31045068696670342, -76.54035590729588989 ) ) ;
#20734 = EDGE_LOOP ( 'NONE', ( #2388, #49319, #22766, #29753, #38740 ) ) ;
#20735 = CARTESIAN_POINT ( 'NONE',  ( 61.04001029137710077, 14.12696047140060074, -46.86320535112459851 ) ) ;
#20736 = CARTESIAN_POINT ( 'NONE',  ( 42.65553098943552612, 6.494013008808203757, -77.04196490166894762 ) ) ;
#20737 = CARTESIAN_POINT ( 'NONE',  ( 24.04486012107927806, -15.65397104612058143, -65.50918627229970070 ) ) ;
#20738 = CARTESIAN_POINT ( 'NONE',  ( 13.82518338685379966, -23.53151426795909984, -46.38267033200749978 ) ) ;
#20739 = CARTESIAN_POINT ( 'NONE',  ( 43.27761160094991766, -37.81795400707816412, -73.93156894824470271 ) ) ;
#20740 = ORIENTED_EDGE ( 'NONE', *, *, #29699, .T. ) ;
#20741 = EDGE_CURVE ( 'NONE', #15227, #14552, #50412, .T. ) ;
#20742 =( BOUNDED_CURVE ( )  B_SPLINE_CURVE ( 3, ( #31349, #7790, #6766, #23742 ),
 .UNSPECIFIED., .F., .T. ) 
 B_SPLINE_CURVE_WITH_KNOTS ( ( 4, 4 ),
 ( 5.964622971501799320, 6.208697808690975428 ),
 .UNSPECIFIED. ) 
 CURVE ( )  GEOMETRIC_REPRESENTATION_ITEM ( )  RATIONAL_B_SPLINE_CURVE ( ( 1.000000000000000000, 0.9950417810232484728, 0.9950417810232484728, 1.000000000000000000 ) ) 
 REPRESENTATION_ITEM ( '' )  );
#20743 = CARTESIAN_POINT ( 'NONE',  ( 11.27235364543490803, -21.94242546894149370, -42.50066467368454681 ) ) ;
#20744 = CARTESIAN_POINT ( 'NONE',  ( 22.93909306572350104, -18.64877037624530232, -36.36609723691169904 ) ) ;
#20745 = CARTESIAN_POINT ( 'NONE',  ( 75.13393739769618662, -33.11618894467940066, -84.38499399519520239 ) ) ;
#20746 = EDGE_CURVE ( 'NONE', #1986, #14340, #30563, .T. ) ;
#20747 = CARTESIAN_POINT ( 'NONE',  ( 14.27929716716409914, 21.26099547410829871, -75.92929371827810314 ) ) ;
#20748 = B_SPLINE_CURVE_WITH_KNOTS ( 'NONE', 3,
 ( #3816, #40739, #4315, #24464, #905, #4062, #16627, #8249, #24725, #32326, #20028 ),
 .UNSPECIFIED., .F., .F.,
 ( 4, 1, 1, 1, 1, 1, 1, 1, 4 ),
 ( 0.000000000000000000, 0.1249999449042852873, 0.2499998898085705745, 0.3749998347128558618, 0.4999997796171411490, 0.6249997245214263808, 0.7499996694257117236, 0.8749996143299969553, 1.000000000000000000 ),
 .UNSPECIFIED. ) ;
#20749 = CARTESIAN_POINT ( 'NONE',  ( 83.92831008986510710, -44.23173406571270050, -46.72264359244280740 ) ) ;
#20750 = AXIS2_PLACEMENT_3D ( 'NONE', #29058, #48732, #9666 ) ;
#20751 = CARTESIAN_POINT ( 'NONE',  ( 11.22168610240190212, 33.99689329125807546, -17.68872724081435521 ) ) ;
#20752 = CARTESIAN_POINT ( 'NONE',  ( 8.153091836570281359, -13.54524113306460009, -52.58848421441390286 ) ) ;
#20753 = ORIENTED_EDGE ( 'NONE', *, *, #17221, .F. ) ;
#20754 = CARTESIAN_POINT ( 'NONE',  ( 53.10146316558890334, -49.38330102694990131, -27.45415746263869750 ) ) ;
#20755 = CARTESIAN_POINT ( 'NONE',  ( 16.65427257814090112, -51.11618894347309805, -20.14977964541890287 ) ) ;
#20756 = CARTESIAN_POINT ( 'NONE',  ( 76.88109033428489170, 11.93863756556099887, -14.86960256363260058 ) ) ;
#20757 = CARTESIAN_POINT ( 'NONE',  ( 43.91474985151640453, 12.31375205243809923, -5.093415854581109237 ) ) ;
#20758 = CARTESIAN_POINT ( 'NONE',  ( -21.36606260230379917, -62.11618894467930119, 17.35000000000000142 ) ) ;
#20759 = LINE ( 'NONE', #9256, #33199 ) ;
#20760 = EDGE_LOOP ( 'NONE', ( #50403, #17665, #13608, #48554 ) ) ;
#20761 = CARTESIAN_POINT ( 'NONE',  ( -2.836119463527300155, -49.03823118242020485, -5.545754996175841001 ) ) ;
#20762 = CARTESIAN_POINT ( 'NONE',  ( 47.33824183327239865, 23.46194572669929812, -54.72426965761560069 ) ) ;
#20763 = CARTESIAN_POINT ( 'NONE',  ( 85.17508943611194638, -49.58715777506750300, -52.74015335379896641 ) ) ;
#20764 = CARTESIAN_POINT ( 'NONE',  ( 63.10653712364238999, 0.8879664753683469414, -62.37500410124779648 ) ) ;
#20765 = CARTESIAN_POINT ( 'NONE',  ( 30.40353819813270064, -5.248717105502837654, 14.62639320225000006 ) ) ;
#20766 = CARTESIAN_POINT ( 'NONE',  ( 11.19833776072039910, 33.93568566053470192, -17.40716472516109903 ) ) ;
#20767 = DIRECTION ( 'NONE',  ( 0.000000000000000000, 1.000000000000000000, 0.000000000000000000 ) ) ;
#20768 = CARTESIAN_POINT ( 'NONE',  ( 8.222313118464692039, -15.61611924975770016, -60.79233150823699816 ) ) ;
#20769 = DIRECTION ( 'NONE',  ( 0.000000000000000000, 0.000000000000000000, 1.000000000000000000 ) ) ;
#20770 = CARTESIAN_POINT ( 'NONE',  ( 57.59063731204929582, -47.30990445082789364, -48.19963584321670425 ) ) ;
#20771 = DIRECTION ( 'NONE',  ( 1.000000000000000000, 0.000000000000000000, 0.000000000000000000 ) ) ;
#20772 = CARTESIAN_POINT ( 'NONE',  ( 64.84535060374940940, 1.263738073398970041, -60.81786852648419028 ) ) ;
#20773 = CARTESIAN_POINT ( 'NONE',  ( 17.51123789366869943, -52.86216653946310373, -76.12493046668770091 ) ) ;
#20774 = CARTESIAN_POINT ( 'NONE',  ( 14.36265541453573924, -22.20705323002841780, -61.03617101396910982 ) ) ;
#20775 = DIRECTION ( 'NONE',  ( 1.898780000000000034E-11, 1.593211000000000006E-12, -1.000000000000000000 ) ) ;
#20776 = ORIENTED_EDGE ( 'NONE', *, *, #7596, .T. ) ;
#20777 = CARTESIAN_POINT ( 'NONE',  ( -0.2828855350156033732, -10.86435776103753881, -35.01245472409725323 ) ) ;
#20778 = CARTESIAN_POINT ( 'NONE',  ( 9.742404792955269954, 32.03540899651829932, -46.29735760005750222 ) ) ;
#20779 = CARTESIAN_POINT ( 'NONE',  ( 68.13393739769618662, -30.31618894467939995, -65.65000000000000568 ) ) ;
#20780 = EDGE_CURVE ( 'NONE', #7094, #47210, #5383, .T. ) ;
#20781 = CARTESIAN_POINT ( 'NONE',  ( 67.52396372158538895, -31.85234974313089751, -18.22675602796779870 ) ) ;
#20782 = VERTEX_POINT ( 'NONE', #34754 ) ;
#20783 = CARTESIAN_POINT ( 'NONE',  ( 18.11571509568589988, 19.92749982851029955, -74.54610039094001195 ) ) ;
#20784 = VERTEX_POINT ( 'NONE', #31584 ) ;
#20785 = EDGE_CURVE ( 'NONE', #11267, #19523, #12247, .T. ) ;
#20786 = ORIENTED_EDGE ( 'NONE', *, *, #16367, .T. ) ;
#20787 = ORIENTED_EDGE ( 'NONE', *, *, #40761, .F. ) ;
#20788 = CARTESIAN_POINT ( 'NONE',  ( 13.00893739769619906, -65.51843714052719747, -47.75434321273180416 ) ) ;
#20789 = CARTESIAN_POINT ( 'NONE',  ( -31.07316938349034885, 21.88381105532059934, 11.14289321881345352 ) ) ;
#20790 = CARTESIAN_POINT ( 'NONE',  ( 20.76034935557600036, -20.84156012990780127, -81.23899999999999011 ) ) ;
#20791 = EDGE_CURVE ( 'NONE', #2233, #6769, #662, .T. ) ;
#20792 = CARTESIAN_POINT ( 'NONE',  ( 61.65531616106190427, 13.91691178440649779, -46.72879703837820387 ) ) ;
#20793 = ORIENTED_EDGE ( 'NONE', *, *, #27247, .T. ) ;
#20794 = VECTOR ( 'NONE', #30482, 1000.000000000000000 ) ;
#20795 = ORIENTED_EDGE ( 'NONE', *, *, #47528, .F. ) ;
#20796 = VECTOR ( 'NONE', #1077, 1000.000000000000000 ) ;
#20797 = CARTESIAN_POINT ( 'NONE',  ( 9.577107432962000289, -17.87109166221290835, -35.74113635354945728 ) ) ;
#20798 = ORIENTED_EDGE ( 'NONE', *, *, #16426, .T. ) ;
#20799 = DIRECTION ( 'NONE',  ( 0.000000000000000000, 0.000000000000000000, 1.000000000000000000 ) ) ;
#20800 = CARTESIAN_POINT ( 'NONE',  ( 52.10267380125439729, 1.883811055320649963, -20.65000000000000213 ) ) ;
#20801 = DIRECTION ( 'NONE',  ( 0.000000000000000000, 0.000000000000000000, -1.000000000000000000 ) ) ;
#20802 = ORIENTED_EDGE ( 'NONE', *, *, #14800, .T. ) ;
#20803 = VERTEX_POINT ( 'NONE', #24224 ) ;
#20804 = B_SPLINE_CURVE_WITH_KNOTS ( 'NONE', 3,
 ( #21266, #40941, #32016, #37271, #5052, #28094, #44100, #40167, #36736, #16314, #8200, #32270, #20486, #21010, #16567, #32521, #36220, #37009, #1107, #24145, #4262, #48291, #12653, #32787, #28611, #44612, #8718, #842 ),
 .UNSPECIFIED., .F., .F.,
 ( 4, 2, 2, 2, 2, 2, 2, 2, 2, 2, 1, 1, 1, 1, 2, 4 ),
 ( 0.000000000000000000, 0.06250045878239399166, 0.1250009175647879833, 0.1875013763471820027, 0.2500018351295759667, 0.3125022939119698195, 0.3750027526943637279, 0.4375032114767576363, 0.4687534408679544518, 0.4843785555635529705, 0.4921911129113520911, 0.4960973915852517346, 0.4980505309222015842, 0.4990271005906765645, 0.4995153854249139713, 0.5000036702591513782 ),
 .UNSPECIFIED. ) ;
#20805 = CARTESIAN_POINT ( 'NONE',  ( 65.03603135424580728, -1.463538230407920082, -19.52361391316370032 ) ) ;
#20806 = DIRECTION ( 'NONE',  ( -0.06538141124691354555, 0.04750237581189065833, -0.9967290481146758863 ) ) ;
#20807 = CARTESIAN_POINT ( 'NONE',  ( 71.02745183554199571, 13.08237462510360061, -12.42623600195140021 ) ) ;
#20808 = EDGE_CURVE ( 'NONE', #23557, #31144, #36826, .T. ) ;
#20809 = CARTESIAN_POINT ( 'NONE',  ( 54.53726782211339952, 14.79465002154760001, -15.67786077975019943 ) ) ;
#20810 = DIRECTION ( 'NONE',  ( 0.3415390592402317571, -0.6017342458922744219, -0.7219882051209377538 ) ) ;
#20811 = CARTESIAN_POINT ( 'NONE',  ( -3.777837492685370169, 16.75613853373169704, -4.322105417705759400 ) ) ;
#20812 = CARTESIAN_POINT ( 'NONE',  ( 10.10517893431099878, 23.92687708958460036, -21.14999999999999858 ) ) ;
#20813 = CARTESIAN_POINT ( 'NONE',  ( 57.33445156889590066, 14.51539213118700111, -26.24906306687159940 ) ) ;
#20814 = CARTESIAN_POINT ( 'NONE',  ( 23.89748173806130183, -14.46983495992219915, -61.24084159088819490 ) ) ;
#20815 = EDGE_LOOP ( 'NONE', ( #30583, #33756, #16203, #12033 ) ) ;
#20816 = CARTESIAN_POINT ( 'NONE',  ( 18.09749211374589706, 1.343694785579789830, -34.95504743437659556 ) ) ;
#20817 = CARTESIAN_POINT ( 'NONE',  ( 28.49955684666384670, -8.476895227121406862, -34.64999999999999858 ) ) ;
#20818 = CARTESIAN_POINT ( 'NONE',  ( 12.64313521576329968, 34.23242425603879724, -47.04313497434819880 ) ) ;
#20819 = CARTESIAN_POINT ( 'NONE',  ( 72.40645806407979990, 1.061268603384970088, -69.86275902853338948 ) ) ;
#20820 = CARTESIAN_POINT ( 'NONE',  ( 41.88138692637217275, -39.75166464432179936, -76.90407068535067481 ) ) ;
#20821 = CARTESIAN_POINT ( 'NONE',  ( 14.49955684666382716, -41.98180839364702166, -34.65000000000001279 ) ) ;
#20822 = AXIS2_PLACEMENT_3D ( 'NONE', #45460, #26232, #42238 ) ;
#20823 = LINE ( 'NONE', #15176, #46900 ) ;
#20824 = VECTOR ( 'NONE', #10437, 1000.000000000000000 ) ;
#20825 = CARTESIAN_POINT ( 'NONE',  ( 46.35275103504439898, 21.67755452994670406, -76.14999999999999147 ) ) ;
#20826 = CARTESIAN_POINT ( 'NONE',  ( 49.72648160330909661, -53.64673639094029767, -55.11972614036100282 ) ) ;
#20827 = DIRECTION ( 'NONE',  ( 0.000000000000000000, 0.000000000000000000, 1.000000000000000000 ) ) ;
#20828 = CARTESIAN_POINT ( 'NONE',  ( 76.72248428439638701, -43.18406392197798027, -14.42532300465747319 ) ) ;
#20829 = CARTESIAN_POINT ( 'NONE',  ( 14.28038030992529528, -32.47778390180254604, -34.79644291222909658 ) ) ;
#20830 = DIRECTION ( 'NONE',  ( -0.3863301728269291635, 0.9223605572461970326, 0.000000000000000000 ) ) ;
#20831 = EDGE_LOOP ( 'NONE', ( #32890, #39436, #32369, #12399 ) ) ;
#20832 = CARTESIAN_POINT ( 'NONE',  ( 23.15495034093260074, -13.12378617039730067, -42.95876240573199567 ) ) ;
#20833 = CARTESIAN_POINT ( 'NONE',  ( 63.94990637464889716, 1.033013263524900083, -61.34874638836240024 ) ) ;
#20834 = ORIENTED_EDGE ( 'NONE', *, *, #45538, .T. ) ;
#20835 = DIRECTION ( 'NONE',  ( -1.000000000000000000, 0.000000000000000000, 0.000000000000000000 ) ) ;
#20836 = CARTESIAN_POINT ( 'NONE',  ( 60.32372535534879887, -45.84468058682939784, -47.67141866289389895 ) ) ;
#20837 = DIRECTION ( 'NONE',  ( 0.7071067811865472397, -0.7071067811865479058, 0.000000000000000000 ) ) ;
#20838 = CARTESIAN_POINT ( 'NONE',  ( 63.88483510052807191, -43.42126949022875948, -10.13989943727382581 ) ) ;
#20840 = CARTESIAN_POINT ( 'NONE',  ( 9.221384164938969619, -19.60026892670780896, -78.62566431866341077 ) ) ;
#20839 = CARTESIAN_POINT ( 'NONE',  ( 42.21804547344670056, 8.555463751753345392, -75.27853559423084562 ) ) ;
#20841 = CARTESIAN_POINT ( 'NONE',  ( 15.64736352786460039, -8.580152770550549590, -60.32520219920449733 ) ) ;
#20842 = DIRECTION ( 'NONE',  ( 0.000000000000000000, 0.000000000000000000, 1.000000000000000000 ) ) ;
#20843 = ORIENTED_EDGE ( 'NONE', *, *, #20780, .F. ) ;
#20844 = CARTESIAN_POINT ( 'NONE',  ( 82.91592277202040862, -45.56282308470729703, -47.63723459745410338 ) ) ;
#20845 = EDGE_CURVE ( 'NONE', #20784, #47321, #11965, .T. ) ;
#20846 = VERTEX_POINT ( 'NONE', #159 ) ;
#20847 = ORIENTED_EDGE ( 'NONE', *, *, #51596, .T. ) ;
#20848 = CARTESIAN_POINT ( 'NONE',  ( 1.633937397696199056, -15.61618894467930119, -6.928362978644219794 ) ) ;
#20849 = CARTESIAN_POINT ( 'NONE',  ( 56.11803403278968005, 14.71426362913575403, -25.91247644177123988 ) ) ;
#20850 = CARTESIAN_POINT ( 'NONE',  ( 76.46866432614550035, -4.873297363397687931, -13.09238815314908244 ) ) ;
#20851 = B_SPLINE_CURVE_WITH_KNOTS ( 'NONE', 3,
 ( #22421, #38424, #34476, #50485, #14575, #6122, #13476, #22078, #33875, #33361, #33622, #10047, #9796, #1407, #26274, #38088, #13730, #5860 ),
 .UNSPECIFIED., .F., .F.,
 ( 4, 2, 2, 2, 2, 2, 2, 2, 4 ),
 ( 0.5000009455475087350, 0.5625008273540701431, 0.6250007091606315512, 0.6875005909671929594, 0.7500004727737543675, 0.8125003545803157756, 0.8750002363868771837, 0.9375001181934385919, 1.000000000000000000 ),
 .UNSPECIFIED. ) ;
#20852 = CARTESIAN_POINT ( 'NONE',  ( 55.71337517921909210, -51.07520708147169586, -53.59468954495790172 ) ) ;
#20853 = EDGE_LOOP ( 'NONE', ( #38611, #174, #28908 ) ) ;
#20854 = ORIENTED_EDGE ( 'NONE', *, *, #6265, .T. ) ;
#20855 = CARTESIAN_POINT ( 'NONE',  ( 8.428790385332487034, -17.68669786356424112, -56.42431456789199018 ) ) ;
#20856 = CARTESIAN_POINT ( 'NONE',  ( 14.21059016770981032, -7.922947056480517780, -76.92968709617039735 ) ) ;
#20857 = CARTESIAN_POINT ( 'NONE',  ( -8.492060748862416020, 14.62552918811035063, -42.53773143905051768 ) ) ;
#20858 = DIRECTION ( 'NONE',  ( 0.000000000000000000, 0.000000000000000000, -1.000000000000000000 ) ) ;
#20859 = CARTESIAN_POINT ( 'NONE',  ( 8.796734227443069543, -63.17759121671350186, -46.67028841929619887 ) ) ;
#20860 = DIRECTION ( 'NONE',  ( 0.000000000000000000, 0.000000000000000000, -1.000000000000000000 ) ) ;
#20861 = CARTESIAN_POINT ( 'NONE',  ( 38.67452568954060155, -36.11618894467930119, -84.65000000000000568 ) ) ;
#20862 = AXIS2_PLACEMENT_3D ( 'NONE', #37876, #46269, #14022 ) ;
#20863 = EDGE_CURVE ( 'NONE', #4176, #29074, #28792, .T. ) ;
#20864 = VERTEX_POINT ( 'NONE', #48903 ) ;
#20865 = CARTESIAN_POINT ( 'NONE',  ( 11.18388210880936562, 32.13318903344607236, -14.72248478078991951 ) ) ;
#20866 = CARTESIAN_POINT ( 'NONE',  ( 53.99792507037630429, -50.61618862432099775, -77.02993420784260081 ) ) ;
#20867 = CARTESIAN_POINT ( 'NONE',  ( 16.13816125998162931, -22.38318796325360438, -46.95262491913606340 ) ) ;
#20868 = CIRCLE ( 'NONE', #46037, 1.999999999999995115 ) ;
#20869 = CARTESIAN_POINT ( 'NONE',  ( 83.49396093869917479, -45.25227168876257622, -47.52772051731956537 ) ) ;
#20870 = VECTOR ( 'NONE', #51478, 1000.000000000000000 ) ;
#20871 = CIRCLE ( 'NONE', #27578, 2.000000000000001776 ) ;
#20872 = CARTESIAN_POINT ( 'NONE',  ( 10.85903228057479986, -9.805670585965609476, -59.27786220483749702 ) ) ;
#20873 = EDGE_CURVE ( 'NONE', #12469, #5062, #48906, .T. ) ;
#20874 = CARTESIAN_POINT ( 'NONE',  ( 68.13393739769620083, -49.36618894467930829, -73.25000000000000000 ) ) ;
#20875 = CARTESIAN_POINT ( 'NONE',  ( 22.90093739769620029, -15.61618894467913243, -28.45282021618999835 ) ) ;
#20876 = VECTOR ( 'NONE', #43626, 1000.000000000000114 ) ;
#20877 = EDGE_CURVE ( 'NONE', #37366, #4162, #11051, .T. ) ;
#20878 = CARTESIAN_POINT ( 'NONE',  ( 43.05690220640799737, -43.67411922962340043, -4.900907769805740166 ) ) ;
#20879 = CARTESIAN_POINT ( 'NONE',  ( 68.13393739806078031, -1.166188944810203409, -89.14999999981660039 ) ) ;
#20880 = CARTESIAN_POINT ( 'NONE',  ( 67.04038824939736685, -50.70395984888217811, -72.15645085170115181 ) ) ;
#20881 = CARTESIAN_POINT ( 'NONE',  ( 61.37892430293329937, -45.32812869357670849, -47.24517423587799669 ) ) ;
#20882 = CARTESIAN_POINT ( 'NONE',  ( 63.95121251289828734, 1.060191874549210045, -69.95192703337309581 ) ) ;
#20883 = CARTESIAN_POINT ( 'NONE',  ( 8.223148984577919762, -15.61599292915740023, -40.79233150823699816 ) ) ;
#20884 = CARTESIAN_POINT ( 'NONE',  ( 66.71085391307920531, -0.3516942507182569955, -17.22176303687090027 ) ) ;
#20885 = ORIENTED_EDGE ( 'NONE', *, *, #35907, .F. ) ;
#20886 = CARTESIAN_POINT ( 'NONE',  ( 14.14442474872529942, -52.06054985064280061, -75.71157996061791096 ) ) ;
#20887 = CARTESIAN_POINT ( 'NONE',  ( 47.35501076093819961, -54.67813530284840340, -54.64069690081250030 ) ) ;
#20888 = CARTESIAN_POINT ( 'NONE',  ( 19.54191788466946633, -9.703270981965982145, -38.11948896923542662 ) ) ;
#20889 = CARTESIAN_POINT ( 'NONE',  ( 22.90085274204890808, -15.61618877333890332, -76.84718755697707593 ) ) ;
#20890 = CARTESIAN_POINT ( 'NONE',  ( 61.04944787454328292, -45.46340257749388769, -47.40250302194245791 ) ) ;
#20891 = CARTESIAN_POINT ( 'NONE',  ( 23.37921890642729750, -15.16088557610839871, -32.14999999999999858 ) ) ;
#20892 = CARTESIAN_POINT ( 'NONE',  ( 57.43837919783884161, 13.96417635576200134, -25.73816349075863741 ) ) ;
#20893 = CARTESIAN_POINT ( 'NONE',  ( 11.17220089305429909, 33.98357240679010260, -17.67193522364469871 ) ) ;
#20895 = CARTESIAN_POINT ( 'NONE',  ( 8.223551834036749497, -15.61610457483330094, -62.79233150823698395 ) ) ;
#20894 = DIRECTION ( 'NONE',  ( 0.000000000000000000, 0.000000000000000000, 1.000000000000000000 ) ) ;
#20896 = CARTESIAN_POINT ( 'NONE',  ( 68.13393739769618662, -1.166188944679350081, -65.65000000000000568 ) ) ;
#20897 = CARTESIAN_POINT ( 'NONE',  ( 48.40744063480869386, 22.97621965999740112, -55.31593188200960043 ) ) ;
#20898 = VERTEX_POINT ( 'NONE', #44693 ) ;
#20899 = AXIS2_PLACEMENT_3D ( 'NONE', #43963, #11496, #46889 ) ;
#20900 = CARTESIAN_POINT ( 'NONE',  ( 9.965766340832269421, -12.19621453136610079, -60.00832647495010264 ) ) ;
#20901 = VERTEX_POINT ( 'NONE', #20057 ) ;
#20902 = CARTESIAN_POINT ( 'NONE',  ( 18.86789271228535725, -51.78678246903497495, -74.34716300800680244 ) ) ;
#20903 = CARTESIAN_POINT ( 'NONE',  ( 65.11747358718548639, 1.386342629514219826, -61.00047607903670155 ) ) ;
#20904 = CARTESIAN_POINT ( 'NONE',  ( 18.63393739769619728, -45.61618894467940066, -35.14999999999999858 ) ) ;
#20906 = CARTESIAN_POINT ( 'NONE',  ( 53.92218800908630527, 17.13899829394239660, -26.37400648228619815 ) ) ;
#20905 = CARTESIAN_POINT ( 'NONE',  ( 82.45627759125980560, 13.86034323648230071, -46.38986626917139233 ) ) ;
#20907 = AXIS2_PLACEMENT_3D ( 'NONE', #10822, #50650, #5854 ) ;
#20908 = CARTESIAN_POINT ( 'NONE',  ( 20.34507489674630065, -21.27382799827049809, -68.74914615139218199 ) ) ;
#20909 = CARTESIAN_POINT ( 'NONE',  ( 57.50723869802200028, -45.11618894467940066, -17.68294118799479975 ) ) ;
#20910 = B_SPLINE_SURFACE_WITH_KNOTS ( 'NONE', 3, 3, ( 
 ( #50202, #14295, #10369, #30520, #5667, #46544, #21613, #37618, #41809, #10631, #21361, #49690, #29739, #45754, #9847, #25803 ),
 ( #17961, #5916, #37890, #33930, #14037, #15332, #35234, #42603, #30776, #22656, #6698, #18733, #51241, #34971, #27115, #31285 ),
 ( #23164, #3020, #19252, #15067, #26853, #42864, #46800, #39181, #47060, #6958, #38677, #3278, #11145, #7210, #2762, #34712 ),
 ( #31035, #50713, #14811, #10890, #43119, #22910, #38927, #18990, #50970, #25709, #2667, #10534, #13943, #6086, #45918, #42509 ),
 ( #46709, #50619, #45654, #26236, #5823, #42767, #37794, #33838, #30170, #34354, #18379, #6866, #25971, #10010, #38053, #50369 ),
 ( #13690, #2146, #14455, #33586, #30423, #29649, #41714, #18126, #21786, #1889, #46449, #6595, #26492, #22559, #38307, #17867 ),
 ( #38575, #18641, #49851, #17619, #34616, #14715, #46187, #29901, #41983, #30686, #10793, #37525, #26753, #1628, #49603, #34090 ),
 ( #50102, #9756, #14200, #10273, #6341, #42243, #22301, #2394, #43283, #43784, #31446, #36415, #12591, #8652, #48232, #30101 ),
 ( #22495, #38505, #2605, #14649, #17553, #41654, #22608, #30988, #35186, #43326, #27065, #26804, #27576, #51189, #7166, #23120 ) ),
 .UNSPECIFIED., .F., .F., .F.,
 ( 4, 1, 1, 1, 1, 1, 4 ),
 ( 4, 2, 2, 2, 2, 2, 2, 4 ),
 ( -1.817263145799999900E-05, 0.1666666666666670182, 0.3333333333333329818, 0.5000000000000000000, 0.6666666666666670737, 0.8333333333333330373, 1.000000000000000000 ),
 ( -1.817262822599999744E-05, 0.3475067738041929810, 1.991082141981049825, 3.418070884026870093, 4.557427845368080099, 5.127106326038690653, 5.582849110575169860, 5.633122992941930640 ),
 .UNSPECIFIED. ) ;
#20911 = CARTESIAN_POINT ( 'NONE',  ( 17.16956960005933297, -23.52717684783756269, -80.25066610258798505 ) ) ;
#20912 = ORIENTED_EDGE ( 'NONE', *, *, #8513, .T. ) ;
#20913 = EDGE_CURVE ( 'NONE', #260, #15485, #46708, .T. ) ;
#20914 = AXIS2_PLACEMENT_3D ( 'NONE', #42407, #17268, #46350 ) ;
#20915 = EDGE_LOOP ( 'NONE', ( #9136, #23116 ) ) ;
#20916 = CARTESIAN_POINT ( 'NONE',  ( 11.70612132433960006, -65.02222053889551034, -16.54010580623710069 ) ) ;
#20917 = CARTESIAN_POINT ( 'NONE',  ( 11.26776687660830056, 33.31889147624380598, -45.55476822783580104 ) ) ;
#20918 = CARTESIAN_POINT ( 'NONE',  ( 22.23393739769620225, -15.61618894467929941, 2.750000000000000000 ) ) ;
#20919 = CARTESIAN_POINT ( 'NONE',  ( 48.63054825335189690, -53.86377910125730040, -54.34287102679169834 ) ) ;
#20920 = DIRECTION ( 'NONE',  ( 1.000000000000000000, 0.000000000000000000, 0.000000000000000000 ) ) ;
#20921 = ORIENTED_EDGE ( 'NONE', *, *, #34201, .F. ) ;
#20922 = CARTESIAN_POINT ( 'NONE',  ( 16.13393739954389972, -15.61618894518879941, 4.350000000321379900 ) ) ;
#20923 = FACE_OUTER_BOUND ( 'NONE', #27592, .T. ) ;
#20924 = CARTESIAN_POINT ( 'NONE',  ( 52.86588932659250162, 18.89687367272220087, -50.05840281104079992 ) ) ;
#20925 = CARTESIAN_POINT ( 'NONE',  ( 84.13393739769618662, -29.66618894467940137, -65.65000000000000568 ) ) ;
#20926 = CARTESIAN_POINT ( 'NONE',  ( 50.50110134946189788, -49.67252027771040446, -76.16336504862310619 ) ) ;
#20927 = DIRECTION ( 'NONE',  ( -2.306135999999999414E-12, 2.429896999999999860E-12, -1.000000000000000000 ) ) ;
#20928 = ORIENTED_EDGE ( 'NONE', *, *, #6582, .F. ) ;
#20929 = CARTESIAN_POINT ( 'NONE',  ( 16.97276188636960015, -43.80059717415329601, -59.64999999999999147 ) ) ;
#20930 = CARTESIAN_POINT ( 'NONE',  ( 15.01109173769499883, -43.96113075119600211, -62.64999999999999858 ) ) ;
#20931 = ORIENTED_EDGE ( 'NONE', *, *, #15557, .F. ) ;
#20932 = PLANE ( 'NONE',  #20163 ) ;
#20933 = CARTESIAN_POINT ( 'NONE',  ( 56.83411512905762919, 15.66923033284180633, -26.73578643762690277 ) ) ;
#20934 = CARTESIAN_POINT ( 'NONE',  ( 8.564672508253739380, -12.34675523859029944, -80.92212427574548883 ) ) ;
#20935 = CARTESIAN_POINT ( 'NONE',  ( 13.59495223564569955, -51.40398734714930384, -22.70120839867610130 ) ) ;
#20936 = CARTESIAN_POINT ( 'NONE',  ( 56.00368918932939266, 19.58097593056960051, -74.93707363489029660 ) ) ;
#20937 = EDGE_CURVE ( 'NONE', #41285, #37252, #4591, .T. ) ;
#20938 = CARTESIAN_POINT ( 'NONE',  ( 46.81730464115280199, -53.59092212908089436, -75.98233228156729524 ) ) ;
#20939 = ORIENTED_EDGE ( 'NONE', *, *, #21719, .F. ) ;
#20940 = AXIS2_PLACEMENT_3D ( 'NONE', #26546, #22357, #18694 ) ;
#20941 = CARTESIAN_POINT ( 'NONE',  ( 55.45319518098449407, 14.78280949324359916, -16.61882359200989967 ) ) ;
#20942 = CIRCLE ( 'NONE', #26817, 0.4999999999562930175 ) ;
#20943 = CARTESIAN_POINT ( 'NONE',  ( 57.03340749225579742, -50.31390957266170005, -52.79504027221379658 ) ) ;
#20944 = CARTESIAN_POINT ( 'NONE',  ( 52.58883999282150512, -49.83940783755189585, -48.57092258697220188 ) ) ;
#20945 = CARTESIAN_POINT ( 'NONE',  ( 18.16448196509429991, -8.861961676679291244, -32.44013846481049512 ) ) ;
#20946 = CARTESIAN_POINT ( 'NONE',  ( 16.13393739769620083, -15.61618894467929941, 14.62639320225000006 ) ) ;
#20947 = CIRCLE ( 'NONE', #17605, 1.000000000000000888 ) ;
#20948 = CARTESIAN_POINT ( 'NONE',  ( 47.43262305882279861, 23.39837035974399981, -74.36069403054010252 ) ) ;
#20949 = PLANE ( 'NONE',  #38469 ) ;
#20950 = DIRECTION ( 'NONE',  ( 0.000000000000000000, 0.000000000000000000, 1.000000000000000000 ) ) ;
#20951 = CARTESIAN_POINT ( 'NONE',  ( 12.27153357072740114, 33.38674963102350546, -15.84005975576420155 ) ) ;
#20952 = CARTESIAN_POINT ( 'NONE',  ( 17.12805204922614877, -49.61616334567082021, -83.22692977624372190 ) ) ;
#20953 = DIRECTION ( 'NONE',  ( 0.000000000000000000, 0.000000000000000000, -1.000000000000000000 ) ) ;
#20955 = CARTESIAN_POINT ( 'NONE',  ( 29.13393739769619728, -35.78776181993320193, -84.63196841427449613 ) ) ;
#20954 = DIRECTION ( 'NONE',  ( 0.000000000000000000, 0.000000000000000000, 1.000000000000000000 ) ) ;
#20956 = CARTESIAN_POINT ( 'NONE',  ( 63.15096886846589541, 0.8925687589132640376, -68.99219224778180148 ) ) ;
#20957 = CARTESIAN_POINT ( 'NONE',  ( 61.25188761286670314, 14.01595200629009952, -46.56130740076640251 ) ) ;
#20958 = CARTESIAN_POINT ( 'NONE',  ( -29.55684472351650172, -35.86170217675510230, -55.62305524083090091 ) ) ;
#20959 = ORIENTED_EDGE ( 'NONE', *, *, #47696, .T. ) ;
#20960 = CARTESIAN_POINT ( 'NONE',  ( 53.31239004767299861, -49.40924252131510030, -48.83993499871439781 ) ) ;
#20961 = CARTESIAN_POINT ( 'NONE',  ( 60.19345682049280555, -45.11617047991499874, -26.22295725826409907 ) ) ;
#20962 = CARTESIAN_POINT ( 'NONE',  ( 48.02939153114380133, -54.36963205275330324, -55.28067537372130147 ) ) ;
#20963 = CARTESIAN_POINT ( 'NONE',  ( 56.76514959097689683, 14.22673106357260053, -25.88737783761489908 ) ) ;
#20964 = CARTESIAN_POINT ( 'NONE',  ( 15.26394330896870244, -8.617212663664730599, -39.91345524423469726 ) ) ;
#20965 = CARTESIAN_POINT ( 'NONE',  ( 50.50110133130939971, 18.44014233979840256, -76.16336504856330691 ) ) ;
#20966 = CARTESIAN_POINT ( 'NONE',  ( 52.68891395819000678, 18.51768936255079723, -48.47378032971769812 ) ) ;
#20967 = CARTESIAN_POINT ( 'NONE',  ( 71.16987874477759135, 1.383357884654609959, -70.32891903079600127 ) ) ;
#20968 = CARTESIAN_POINT ( 'NONE',  ( 41.27829218924360077, -44.10783499397969365, -3.596739496640999789 ) ) ;
#20969 = CARTESIAN_POINT ( 'NONE',  ( 64.61644452598639532, -44.96401322665339961, -11.41031418918720064 ) ) ;
#20970 = EDGE_LOOP ( 'NONE', ( #14564, #51756, #29122, #50714 ) ) ;
#20971 = ADVANCED_FACE ( 'NONE', ( #43923, #12212 ), #32093, .T. ) ;
#20972 = CARTESIAN_POINT ( 'NONE',  ( 17.73920358962980259, -22.89147689717010081, -77.49821634947008420 ) ) ;
#20973 = ORIENTED_EDGE ( 'NONE', *, *, #16127, .T. ) ;
#20974 = ADVANCED_FACE ( 'NONE', ( #40760 ), #48636, .F. ) ;
#20975 = CARTESIAN_POINT ( 'NONE',  ( 73.04666255914109740, 0.9369374701296400154, -69.09468190869459647 ) ) ;
#20976 = CARTESIAN_POINT ( 'NONE',  ( 47.42307040393540518, -54.63294004021819461, -54.67104605768700054 ) ) ;
#20977 = CARTESIAN_POINT ( 'NONE',  ( 72.82137280411760116, 1.383928098097870096, -62.75238677440889035 ) ) ;
#20978 = VECTOR ( 'NONE', #30952, 1000.000000000000000 ) ;
#20979 = CARTESIAN_POINT ( 'NONE',  ( 27.68571409299283914, -36.31111876860410348, -34.79644660940672907 ) ) ;
#20981 = EDGE_CURVE ( 'NONE', #31098, #39196, #1018, .T. ) ;
#20980 = CARTESIAN_POINT ( 'NONE',  ( 71.56838563924230812, 1.003508719580009867, -60.73835207042080242 ) ) ;
#20982 = CARTESIAN_POINT ( 'NONE',  ( 2.501736331312110373, -25.44663551349389863, -34.68801049095939959 ) ) ;
#20983 = CARTESIAN_POINT ( 'NONE',  ( 72.18032112064790340, 1.107037132887370046, -61.22623577547380336 ) ) ;
#20984 = AXIS2_PLACEMENT_3D ( 'NONE', #25044, #1488, #24788 ) ;
#20985 = CARTESIAN_POINT ( 'NONE',  ( 16.13393739769620083, -15.61618894467929941, 7.944363289481099599 ) ) ;
#20986 = ADVANCED_FACE ( 'NONE', ( #20566 ), #30155, .T. ) ;
#20987 = CARTESIAN_POINT ( 'NONE',  ( 64.87536617802101091, 1.096110717717199812, -70.63920630446280313 ) ) ;
#20988 = ORIENTED_EDGE ( 'NONE', *, *, #6203, .T. ) ;
#20989 = ORIENTED_EDGE ( 'NONE', *, *, #8706, .T. ) ;
#20990 = CARTESIAN_POINT ( 'NONE',  ( 9.276735402967759114, -63.13661701015139727, -46.53281877167430025 ) ) ;
#20991 = CARTESIAN_POINT ( 'NONE',  ( 16.10973090867273783, -51.04076668988478360, -15.66788158150958132 ) ) ;
#20992 = EDGE_LOOP ( 'NONE', ( #51486, #19798, #4880, #45112 ) ) ;
#20993 = CARTESIAN_POINT ( 'NONE',  ( 19.87062220799639789, -9.634571621335810576, -72.52491758300199365 ) ) ;
#20994 = CARTESIAN_POINT ( 'NONE',  ( 23.04644962015954235, -11.63203690814193791, -59.34097683662206180 ) ) ;
#20995 = CARTESIAN_POINT ( 'NONE',  ( 16.13393739769620083, -15.61618894467929941, -81.65000000000000568 ) ) ;
#20996 = CARTESIAN_POINT ( 'NONE',  ( 53.99629484646779787, 19.44063541514490012, -76.54982658315300625 ) ) ;
#20997 = ORIENTED_EDGE ( 'NONE', *, *, #33634, .F. ) ;
#20998 = DIRECTION ( 'NONE',  ( 1.000000000000000000, 0.000000000000000000, 0.000000000000000000 ) ) ;
#20999 = CARTESIAN_POINT ( 'NONE',  ( 10.06369629473941352, -53.99262654158863484, -34.79644414665150975 ) ) ;
#21000 = CARTESIAN_POINT ( 'NONE',  ( 23.99755426256392710, -16.50001052160837034, -65.54328182147770576 ) ) ;
#21001 = CARTESIAN_POINT ( 'NONE',  ( 22.12835029666389985, -9.954940491146789583, -49.55142757455229940 ) ) ;
#21002 = CARTESIAN_POINT ( 'NONE',  ( 14.60579227114195788, -8.963325624781994350, -55.88125799276141947 ) ) ;
#21003 = CARTESIAN_POINT ( 'NONE',  ( 16.15069521921704165, -51.05177107958204630, -15.66900421577824254 ) ) ;
#21004 = EDGE_CURVE ( 'NONE', #51178, #1216, #28636, .T. ) ;
#21005 = ORIENTED_EDGE ( 'NONE', *, *, #12966, .F. ) ;
#21006 = CARTESIAN_POINT ( 'NONE',  ( 11.37791593499470011, -63.64622813626678521, -24.39397853729850141 ) ) ;
#21007 = CARTESIAN_POINT ( 'NONE',  ( 8.941982268396820643, -13.67133028058830035, -37.31672440967518867 ) ) ;
#21008 = CARTESIAN_POINT ( 'NONE',  ( 40.71242742815670113, 14.10279950470690125, -5.692218735367429616 ) ) ;
#21009 = CARTESIAN_POINT ( 'NONE',  ( 14.21728741900179926, 20.91286242874570078, -75.79069550273320033 ) ) ;
#21010 = CARTESIAN_POINT ( 'NONE',  ( 22.30441927812678671, -20.68056348242964049, -60.01079243619062709 ) ) ;
#21011 = AXIS2_PLACEMENT_3D ( 'NONE', #19257, #51246, #47825 ) ;
#21012 = CARTESIAN_POINT ( 'NONE',  ( 84.44784216359251161, -43.11618894467930119, -47.47585302082339354 ) ) ;
#21013 = EDGE_CURVE ( 'NONE', #11609, #26529, #15711, .T. ) ;
#21014 = CARTESIAN_POINT ( 'NONE',  ( 11.26548663221610092, -8.961798825887671072, -54.80661428419509917 ) ) ;
#21015 = ORIENTED_EDGE ( 'NONE', *, *, #1408, .F. ) ;
#21016 = CARTESIAN_POINT ( 'NONE',  ( 55.11178888707910062, -47.40156703920949610, -26.42191461600259572 ) ) ;
#21017 = CARTESIAN_POINT ( 'NONE',  ( 53.80404574041880039, -51.29624668929719888, -75.54363968662481454 ) ) ;
#21018 = CARTESIAN_POINT ( 'NONE',  ( 57.36123081079020380, 18.90300135422739913, -52.61896059691729732 ) ) ;
#21019 = B_SPLINE_CURVE_WITH_KNOTS ( 'NONE', 3,
 ( #3616, #8768, #36530, #3358, #898, #635, #15409, #31361, #15665, #31617 ),
 .UNSPECIFIED., .F., .F.,
 ( 4, 2, 2, 2, 4 ),
 ( 0.000000000000000000, 0.1774999999982362353, 0.3374999999966465936, 0.4374999999956565855, 0.4999999271596955452 ),
 .UNSPECIFIED. ) ;
#21020 = DIRECTION ( 'NONE',  ( -1.000000000000000000, 0.000000000000000000, 0.000000000000000000 ) ) ;
#21021 = CARTESIAN_POINT ( 'NONE',  ( 45.63704616078170062, 14.88914480619270186, -9.401569148867338299 ) ) ;
#21022 = ORIENTED_EDGE ( 'NONE', *, *, #10048, .F. ) ;
#21023 = CARTESIAN_POINT ( 'NONE',  ( -6.893020797678770073, -45.90759191447720156, -5.210453294515490441 ) ) ;
#21024 = CARTESIAN_POINT ( 'NONE',  ( 47.36721828898109976, 23.44513434380789718, -54.83101768469499859 ) ) ;
#21025 = CARTESIAN_POINT ( 'NONE',  ( 22.19769533645140314, 22.77497238916379274, -34.80997524099235818 ) ) ;
#21026 = CARTESIAN_POINT ( 'NONE',  ( 63.52011431889719972, 1.391252479931859964, -62.52735703481241103 ) ) ;
#21027 = LINE ( 'NONE', #45152, #20604 ) ;
#21028 = CARTESIAN_POINT ( 'NONE',  ( 11.37397754636229941, 34.06366721452670276, -17.68262826289139866 ) ) ;
#21029 = DIRECTION ( 'NONE',  ( 0.000000000000000000, 0.000000000000000000, 1.000000000000000000 ) ) ;
#21030 = LINE ( 'NONE', #40957, #29253 ) ;
#21031 = LINE ( 'NONE', #40191, #9039 ) ;
#21032 = CARTESIAN_POINT ( 'NONE',  ( 56.37993369902870455, -47.94505858661049302, -48.46713487898719563 ) ) ;
#21033 = CARTESIAN_POINT ( 'NONE',  ( 22.80556477356921263, -16.78781406865223502, -66.50815379053354093 ) ) ;
#21034 = CARTESIAN_POINT ( 'NONE',  ( 54.90250570405320474, 20.20956959306230161, -53.93623998597109903 ) ) ;
#21035 = CARTESIAN_POINT ( 'NONE',  ( 22.04684512462105772, -19.02418749289184063, -60.61949336887142437 ) ) ;
#21036 = ORIENTED_EDGE ( 'NONE', *, *, #37329, .T. ) ;
#21037 = CARTESIAN_POINT ( 'NONE',  ( 68.13393739769620083, 0.8838110553206759423, -65.65000000000000568 ) ) ;
#21038 = CARTESIAN_POINT ( 'NONE',  ( 8.968618095842160187, 31.99037451711150126, -46.63269056292379844 ) ) ;
#21039 = CARTESIAN_POINT ( 'NONE',  ( 62.63393739769619373, -53.11618894467930119, 17.35000000000000142 ) ) ;
#21040 = DIRECTION ( 'NONE',  ( 0.000000000000000000, 0.000000000000000000, -1.000000000000000000 ) ) ;
#21041 = EDGE_CURVE ( 'NONE', #4191, #34457, #50549, .T. ) ;
#21042 = ORIENTED_EDGE ( 'NONE', *, *, #6555, .T. ) ;
#21043 = CARTESIAN_POINT ( 'NONE',  ( 18.71089559737819741, 20.68059730019909992, -75.01675372117850316 ) ) ;
#21044 = ORIENTED_EDGE ( 'NONE', *, *, #27200, .T. ) ;
#21045 = ORIENTED_EDGE ( 'NONE', *, *, #2409, .T. ) ;
#21046 = CARTESIAN_POINT ( 'NONE',  ( 47.83780165944450147, 23.21886414354259998, -55.23279884646720461 ) ) ;
#21047 = ORIENTED_EDGE ( 'NONE', *, *, #28669, .F. ) ;
#21048 = CARTESIAN_POINT ( 'NONE',  ( 10.78709078437059965, -64.43314706647589674, -46.17090595131550401 ) ) ;
#21049 = CARTESIAN_POINT ( 'NONE',  ( 56.76506913988440317, -45.81015338506770718, -26.16735717962830066 ) ) ;
#21050 = CARTESIAN_POINT ( 'NONE',  ( 20.86987029233329949, -20.75753920121769980, -81.23899999999999011 ) ) ;
#21051 = AXIS2_PLACEMENT_3D ( 'NONE', #21100, #29992, #22394 ) ;
#21052 =( BOUNDED_CURVE ( )  B_SPLINE_CURVE ( 2, ( #30832, #39239, #11981 ),
 .UNSPECIFIED., .F., .T. ) 
 B_SPLINE_CURVE_WITH_KNOTS ( ( 3, 3 ),
 ( 0.1321855491173860031, 2.139356573168320175 ),
 .UNSPECIFIED. ) 
 CURVE ( )  GEOMETRIC_REPRESENTATION_ITEM ( )  RATIONAL_B_SPLINE_CURVE ( ( 1.001093714201189977, 1.008874108730310137, 1.000760730674130183 ) ) 
 REPRESENTATION_ITEM ( '' )  );
#21053 = CARTESIAN_POINT ( 'NONE',  ( 61.63685072850250179, 13.93395889737410087, -46.81169383245449467 ) ) ;
#21054 = DIRECTION ( 'NONE',  ( 0.000000000000000000, 0.000000000000000000, 1.000000000000000000 ) ) ;
#21055 = ORIENTED_EDGE ( 'NONE', *, *, #47308, .F. ) ;
#21056 = CIRCLE ( 'NONE', #1800, 3.000000000000000000 ) ;
#21057 = CARTESIAN_POINT ( 'NONE',  ( 16.13393739769620083, -15.61618894467929941, -21.14999999999999858 ) ) ;
#21058 = CONICAL_SURFACE ( 'NONE', #48687, 0.6299999999999977840, 0.7853981633974476129 ) ;
#21059 = CARTESIAN_POINT ( 'NONE',  ( 12.24533239789906780, 33.66790093028144071, -16.17634612495991320 ) ) ;
#21060 = EDGE_LOOP ( 'NONE', ( #5287, #46698, #43179, #51347 ) ) ;
#21061 = CARTESIAN_POINT ( 'NONE',  ( 11.53023960985226282, -64.72036740955095979, -23.95196799016841993 ) ) ;
#21062 = DIRECTION ( 'NONE',  ( -1.000000000000000000, 0.000000000000000000, 0.000000000000000000 ) ) ;
#21063 = CARTESIAN_POINT ( 'NONE',  ( 59.52869410915831594, -45.48984219772450643, -26.73579121603098585 ) ) ;
#21064 = ORIENTED_EDGE ( 'NONE', *, *, #28393, .F. ) ;
#21065 = ORIENTED_EDGE ( 'NONE', *, *, #31917, .F. ) ;
#21066 = CARTESIAN_POINT ( 'NONE',  ( 8.133937397696209715, -59.02534396924340143, -43.74348518090240390 ) ) ;
#21067 = CARTESIAN_POINT ( 'NONE',  ( 46.65865115320059431, -53.59114685036150405, -76.01705645362520158 ) ) ;
#21068 = CARTESIAN_POINT ( 'NONE',  ( 73.21814398186710093, 13.07780085657029900, -13.04737355632260076 ) ) ;
#21069 = CARTESIAN_POINT ( 'NONE',  ( 49.49099539719589558, 14.73512810581040000, -11.95182011558090096 ) ) ;
#21070 = CARTESIAN_POINT ( 'NONE',  ( 8.223569788570660677, -15.61625877447020017, -68.79233150823709764 ) ) ;
#21071 = CARTESIAN_POINT ( 'NONE',  ( -3.774505099339080072, 16.75816115460079914, -4.401388191994590748 ) ) ;
#21072 = CARTESIAN_POINT ( 'NONE',  ( 16.72856488856178458, -39.04821110511426951, 4.943674098299959851 ) ) ;
#21073 = CARTESIAN_POINT ( 'NONE',  ( 61.30969410147389453, 13.98565706813869980, -28.15107826849129680 ) ) ;
#21074 = ADVANCED_FACE ( 'NONE', ( #32296 ), #50265, .T. ) ;
#21075 = CARTESIAN_POINT ( 'NONE',  ( 23.56545591261919981, -13.09442750760010021, -75.18337345808529903 ) ) ;
#21076 = VERTEX_POINT ( 'NONE', #51167 ) ;
#21078 = EDGE_CURVE ( 'NONE', #19127, #14308, #19440, .T. ) ;
#21077 = CARTESIAN_POINT ( 'NONE',  ( 58.46570011688019264, 15.47571369907180028, -47.60876906798830532 ) ) ;
#21079 = CARTESIAN_POINT ( 'NONE',  ( -8.385535285650650650, -44.09170945325140423, -4.751637014762500222 ) ) ;
#21080 = CARTESIAN_POINT ( 'NONE',  ( 72.88570115400611371, 0.9405967369906069742, -69.31454995071659653 ) ) ;
#21081 = ADVANCED_FACE ( 'NONE', ( #26516 ), #6620, .T. ) ;
#21082 = AXIS2_PLACEMENT_3D ( 'NONE', #16779, #32728, #9446 ) ;
#21083 = AXIS2_PLACEMENT_3D ( 'NONE', #17453, #42076, #6179 ) ;
#21084 = CARTESIAN_POINT ( 'NONE',  ( 12.16231664501490073, -64.67747237300790175, -15.91745067707079819 ) ) ;
#21085 = CARTESIAN_POINT ( 'NONE',  ( 11.27206271277036009, 34.04961529007477594, -18.17421237816838087 ) ) ;
#21086 = CARTESIAN_POINT ( 'NONE',  ( 12.94867006626759931, 18.87859900410219893, -21.09868194578459821 ) ) ;
#21087 = CARTESIAN_POINT ( 'NONE',  ( 47.13218220315749818, 23.40331810880470087, -74.95061771218550462 ) ) ;
#21088 = CARTESIAN_POINT ( 'NONE',  ( 49.18118975347450572, -53.84795997730500261, -54.89353827381820139 ) ) ;
#21089 = CARTESIAN_POINT ( 'NONE',  ( 42.26864886252769793, -44.36179212852169940, -5.126484877156399556 ) ) ;
#21090 = CARTESIAN_POINT ( 'NONE',  ( 76.70062604860851252, -43.19086386613712136, -14.38326864798454530 ) ) ;
#21091 = CARTESIAN_POINT ( 'NONE',  ( 14.39116781407879841, -32.37825826146760733, -34.70985242058469566 ) ) ;
#21092 = CARTESIAN_POINT ( 'NONE',  ( 11.27231692120963302, -21.94239768697393700, -54.50066575920858725 ) ) ;
#21093 = ORIENTED_EDGE ( 'NONE', *, *, #43477, .F. ) ;
#21094 = CARTESIAN_POINT ( 'NONE',  ( 8.812167609467170593, -16.99400660551760112, -42.00813523296859842 ) ) ;
#21095 = CARTESIAN_POINT ( 'NONE',  ( 64.02475525337911222, 1.458407608744489936, -61.60944193589799767 ) ) ;
#21096 = ORIENTED_EDGE ( 'NONE', *, *, #913, .T. ) ;
#21097 = CARTESIAN_POINT ( 'NONE',  ( 84.12560686111216057, -43.96699758738883190, -46.88422903683994036 ) ) ;
#21098 = CARTESIAN_POINT ( 'NONE',  ( 60.74931022661039748, -45.65492624904909746, -47.61700330749530252 ) ) ;
#21099 = DIRECTION ( 'NONE',  ( 0.3805321250008310008, 0.000000000000000000, -0.9247677015566404535 ) ) ;
#21100 = CARTESIAN_POINT ( 'NONE',  ( 16.13393739769620083, -15.61618894467929941, -14.65000000000000036 ) ) ;
#21102 = CARTESIAN_POINT ( 'NONE',  ( 20.78393739769619941, -15.61618894467929941, -18.35000000000000142 ) ) ;
#21101 = CARTESIAN_POINT ( 'NONE',  ( 43.68437078864629086, 8.695783843854092865, -68.18794609937623363 ) ) ;
#21103 = FACE_OUTER_BOUND ( 'NONE', #6770, .T. ) ;
#21104 = CARTESIAN_POINT ( 'NONE',  ( 16.13393739769620083, -15.61618894467929941, -32.14999999999999858 ) ) ;
#21105 = EDGE_CURVE ( 'NONE', #11543, #33996, #10395, .T. ) ;
#21106 = ORIENTED_EDGE ( 'NONE', *, *, #18510, .F. ) ;
#21107 = CARTESIAN_POINT ( 'NONE',  ( 83.43488124258610128, -45.15430218069970181, -47.39353206303620425 ) ) ;
#21108 = B_SPLINE_CURVE_WITH_KNOTS ( 'NONE', 3,
 ( #23017, #26177, #50047, #34038, #50567, #39037, #42188, #34300, #30627, #50314, #3131, #2873, #26434, #14399, #19100, #18839, #30367, #42452, #6539, #38514, #18584, #34562, #10734, #26688, #42713, #12534, #43474, #44500, #40565 ),
 .UNSPECIFIED., .F., .F.,
 ( 4, 2, 2, 2, 2, 2, 2, 2, 2, 2, 1, 1, 1, 1, 1, 2, 4 ),
 ( 0.000000000000000000, 0.06250045477388861681, 0.1250009095477772336, 0.1875013643216658643, 0.2500018190955544672, 0.3125022738694428481, 0.3750027286433312290, 0.4375031834172196654, 0.4687534108041638836, 0.4843785244976359650, 0.4921910813443720611, 0.4960973597677399427, 0.4980504989794240500, 0.4990270685852660204, 0.4995153533881869778, 0.4997594957896475121, 0.5000036381911079353 ),
 .UNSPECIFIED. ) ;
#21109 = EDGE_LOOP ( 'NONE', ( #6497, #12755, #2901, #2044 ) ) ;
#21110 = EDGE_LOOP ( 'NONE', ( #44794, #1112, #29558, #39056 ) ) ;
#21111 = ORIENTED_EDGE ( 'NONE', *, *, #24326, .F. ) ;
#21112 = CARTESIAN_POINT ( 'NONE',  ( 19.21265657477716005, 18.23736444591407135, -34.79644660940672907 ) ) ;
#21113 = CARTESIAN_POINT ( 'NONE',  ( 52.57212603780299531, -49.85477880025769792, -48.51322654165320358 ) ) ;
#21114 = DIRECTION ( 'NONE',  ( -0.8660254037844351549, 0.5000000000000061062, 0.000000000000000000 ) ) ;
#21115 = CARTESIAN_POINT ( 'NONE',  ( 56.46551567295650642, 19.54378694285259854, -74.14999999999999147 ) ) ;
#21116 = ORIENTED_EDGE ( 'NONE', *, *, #5369, .T. ) ;
#21117 = VERTEX_POINT ( 'NONE', #47494 ) ;
#21118 = CARTESIAN_POINT ( 'NONE',  ( 11.58469291347408969, 34.12844306514984538, -22.56541115952017051 ) ) ;
#21119 = ORIENTED_EDGE ( 'NONE', *, *, #18376, .F. ) ;
#21120 = B_SPLINE_CURVE_WITH_KNOTS ( 'NONE', 3,
 ( #43182, #51553, #26919, #14616, #3860, #38737, #38995, #30586, #31608, #7792 ),
 .UNSPECIFIED., .F., .F.,
 ( 4, 1, 1, 1, 1, 1, 1, 4 ),
 ( 0.000000000000000000, 0.03120051833342932235, 0.1104194493971391161, 0.1896383804606883161, 0.2688573115242375855, 0.3480762425879473376, 0.4272951736514943311, 0.4999978458836923934 ),
 .UNSPECIFIED. ) ;
#21121 = CARTESIAN_POINT ( 'NONE',  ( 56.89013219823429779, 19.38816751928939652, -53.45144266626400054 ) ) ;
#21122 = DIRECTION ( 'NONE',  ( -0.5685928097855439400, -0.5944782866685399680, 0.5685928097855418306 ) ) ;
#21123 = CARTESIAN_POINT ( 'NONE',  ( 22.90105422030644533, -15.61618894250064571, -66.84718200393152188 ) ) ;
#21124 = CARTESIAN_POINT ( 'NONE',  ( 64.43393739769619799, 10.88381105532070059, -62.44999999999999574 ) ) ;
#21125 = VERTEX_POINT ( 'NONE', #38859 ) ;
#21126 = CARTESIAN_POINT ( 'NONE',  ( -64.19449136036995185, 21.25811091637316252, -62.88965083512582055 ) ) ;
#21128 = CARTESIAN_POINT ( 'NONE',  ( 52.75996719278299452, -50.16875253228529630, -77.25935876431830707 ) ) ;
#21127 = AXIS2_PLACEMENT_3D ( 'NONE', #8971, #12908, #40409 ) ;
#21129 = CARTESIAN_POINT ( 'NONE',  ( 22.53299121009855455, -17.91495151342063252, -46.56247258658390109 ) ) ;
#21130 = CARTESIAN_POINT ( 'NONE',  ( 60.43524540865149675, 14.44381373781700084, -47.22144309172190191 ) ) ;
#21131 = CARTESIAN_POINT ( 'NONE',  ( 19.51845506803190133, -8.535808465441810711, -61.65443013674619976 ) ) ;
#21132 = CARTESIAN_POINT ( 'NONE',  ( 52.63393739643800018, -15.61618894418049841, 9.350000000565845681 ) ) ;
#21133 = CARTESIAN_POINT ( 'NONE',  ( 41.22888721229060138, 13.59583590325410007, -5.431170674539309573 ) ) ;
#21134 = CARTESIAN_POINT ( 'NONE',  ( 41.47267154800490374, -44.68978306873219708, -5.287754256597220426 ) ) ;
#21135 = CARTESIAN_POINT ( 'NONE',  ( 71.65889518049858964, 0.9150552061894319245, -60.79444388203420147 ) ) ;
#21136 = CARTESIAN_POINT ( 'NONE',  ( 68.23750919724679420, 0.1964239558528288465, -18.38207371053462325 ) ) ;
#21137 = CARTESIAN_POINT ( 'NONE',  ( 64.07915002758259959, 1.048864949068049945, -70.07302479646419613 ) ) ;
#21138 = CARTESIAN_POINT ( 'NONE',  ( 66.13282613077339533, -0.2025808033276020048, -17.01779698185609746 ) ) ;
#21139 = VERTEX_POINT ( 'NONE', #2692 ) ;
#21141 = ADVANCED_FACE ( 'NONE', ( #26261 ), #2949, .T. ) ;
#21140 = CARTESIAN_POINT ( 'NONE',  ( 13.83628172507089893, -52.07648608105650112, -75.48775473117470369 ) ) ;
#21142 = CARTESIAN_POINT ( 'NONE',  ( 47.20893740402939898, -54.78691078231059919, -54.64017658907569341 ) ) ;
#21143 = EDGE_CURVE ( 'NONE', #9803, #24151, #32059, .T. ) ;
#21144 = DIRECTION ( 'NONE',  ( 0.000000000000000000, 0.000000000000000000, -1.000000000000000000 ) ) ;
#21145 = DIRECTION ( 'NONE',  ( 0.000000000000000000, 0.000000000000000000, -1.000000000000000000 ) ) ;
#21146 = CARTESIAN_POINT ( 'NONE',  ( 24.04490883580620064, -15.59321700223370044, -55.50674799533643977 ) ) ;
#21147 = CARTESIAN_POINT ( 'NONE',  ( 23.44752169114309837, -16.31888570327519972, -32.14999999999999858 ) ) ;
#21148 = PLANE ( 'NONE',  #18898 ) ;
#21149 = CARTESIAN_POINT ( 'NONE',  ( 47.67992640529440251, -54.51849087148959683, -55.14611402303650323 ) ) ;
#21150 = CARTESIAN_POINT ( 'NONE',  ( 8.222937397696199469, -15.61618894467929941, -32.14999999999999858 ) ) ;
#21151 = LINE ( 'NONE', #4660, #25040 ) ;
#21152 = CARTESIAN_POINT ( 'NONE',  ( 48.72320918298880343, 22.79968469717220358, -54.90669916513539306 ) ) ;
#21153 = ORIENTED_EDGE ( 'NONE', *, *, #40865, .T. ) ;
#21154 = TOROIDAL_SURFACE ( 'NONE', #4450, 34.47562460986249988, 0.5000000000000000000 ) ;
#21155 = CARTESIAN_POINT ( 'NONE',  ( 13.79233564180089999, -22.26896734105170239, -67.45490599493020056 ) ) ;
#21156 = AXIS2_PLACEMENT_3D ( 'NONE', #15669, #24010, #7808 ) ;
#21157 = ORIENTED_EDGE ( 'NONE', *, *, #12022, .F. ) ;
#21158 = DIRECTION ( 'NONE',  ( 0.000000000000000000, -1.000000000000000000, 0.000000000000000000 ) ) ;
#21159 = CARTESIAN_POINT ( 'NONE',  ( 72.13393739769618662, -31.87354825726865570, -20.65000000000000213 ) ) ;
#21160 = CARTESIAN_POINT ( 'NONE',  ( 8.223013028489239318, -15.61598591435789984, -40.50766849176299189 ) ) ;
#21162 = CARTESIAN_POINT ( 'NONE',  ( 54.56756649838740714, 16.38481432401099980, -26.02999983734660105 ) ) ;
#21161 = CARTESIAN_POINT ( 'NONE',  ( 83.25229294592290330, 13.91601796603040064, -47.26064541804080221 ) ) ;
#21163 = CARTESIAN_POINT ( 'NONE',  ( 15.40691027875000074, -22.63145731195810129, -60.98569090715739804 ) ) ;
#21164 = CARTESIAN_POINT ( 'NONE',  ( 63.34104417888273986, -53.11618894467930119, 11.14289321881345174 ) ) ;
#21165 = CARTESIAN_POINT ( 'NONE',  ( 55.55364201925849699, -45.11618894467940066, -14.32024453839470013 ) ) ;
#21166 = EDGE_CURVE ( 'NONE', #33533, #22647, #6255, .T. ) ;
#21167 = DIRECTION ( 'NONE',  ( 0.000000000000000000, 0.000000000000000000, 1.000000000000000000 ) ) ;
#21168 = ORIENTED_EDGE ( 'NONE', *, *, #36257, .F. ) ;
#21169 = ADVANCED_FACE ( 'NONE', ( #27551 ), #47746, .T. ) ;
#21170 = ORIENTED_EDGE ( 'NONE', *, *, #3507, .T. ) ;
#21171 = CARTESIAN_POINT ( 'NONE',  ( 11.49145838456619906, -65.03764954149001198, -16.71591419049050131 ) ) ;
#21172 = CARTESIAN_POINT ( 'NONE',  ( 11.70363152391320050, 33.71475452077960000, -45.68937680901829879 ) ) ;
#21173 = CARTESIAN_POINT ( 'NONE',  ( 18.60924722850695545, 20.15530953838155170, -15.72404377366573947 ) ) ;
#21174 = DIRECTION ( 'NONE',  ( 0.000000000000000000, 0.000000000000000000, -1.000000000000000000 ) ) ;
#21175 = DIRECTION ( 'NONE',  ( 0.000000000000000000, 0.000000000000000000, -1.000000000000000000 ) ) ;
#21176 = EDGE_LOOP ( 'NONE', ( #41282, #44720, #21333, #652 ) ) ;
#21177 = CARTESIAN_POINT ( 'NONE',  ( -10.09487475708679938, -44.93564566225139600, -43.84234880612240204 ) ) ;
#21178 = CIRCLE ( 'NONE', #22819, 14.50000000000000178 ) ;
#21179 = CARTESIAN_POINT ( 'NONE',  ( 30.63393739769620083, -15.61618894467929941, -7.349999999999999645 ) ) ;
#21180 = LINE ( 'NONE', #44790, #29182 ) ;
#21181 = CARTESIAN_POINT ( 'NONE',  ( 50.08385623720359803, -49.23364898979970405, -76.14999999999999147 ) ) ;
#21182 = DIRECTION ( 'NONE',  ( 1.397030999999999991E-10, 0.000000000000000000, -1.000000000000000000 ) ) ;
#21183 = ORIENTED_EDGE ( 'NONE', *, *, #26854, .F. ) ;
#21184 = CARTESIAN_POINT ( 'NONE',  ( 22.04686275369982695, -12.20822338258555639, -68.28615154681510546 ) ) ;
#21185 = DIRECTION ( 'NONE',  ( 0.000000000000000000, 0.000000000000000000, 1.000000000000000000 ) ) ;
#21186 = ORIENTED_EDGE ( 'NONE', *, *, #50472, .T. ) ;
#21187 = CARTESIAN_POINT ( 'NONE',  ( 22.46012685026492761, -10.75454424016532506, -57.29933437167828458 ) ) ;
#21188 = CARTESIAN_POINT ( 'NONE',  ( 29.99034385824719706, -15.61618894467929941, -32.14999999999999858 ) ) ;
#21189 = CARTESIAN_POINT ( 'NONE',  ( 13.50455111243270068, -23.01031332518880035, -36.62124792064238932 ) ) ;
#21190 = CARTESIAN_POINT ( 'NONE',  ( 18.53141933435923860, -22.24903445305599092, -65.23677592515561230 ) ) ;
#21191 = CARTESIAN_POINT ( 'NONE',  ( -8.966062602303800588, -15.61618894467929763, 4.450000000000000178 ) ) ;
#21192 = AXIS2_PLACEMENT_3D ( 'NONE', #32047, #9012, #32819 ) ;
#21193 = CARTESIAN_POINT ( 'NONE',  ( 47.34724033287390199, -54.49456303200130236, -74.94574354657768822 ) ) ;
#21194 = ORIENTED_EDGE ( 'NONE', *, *, #11152, .F. ) ;
#21195 = CARTESIAN_POINT ( 'NONE',  ( 55.80628784892600436, 14.51787704501589893, -16.86082891554699970 ) ) ;
#21196 = CIRCLE ( 'NONE', #37978, 50.00000000000000000 ) ;
#21197 = CARTESIAN_POINT ( 'NONE',  ( 57.24929579703059801, -50.61618895653209904, -53.91492794795339449 ) ) ;
#21198 = CIRCLE ( 'NONE', #46376, 2.999999999999999112 ) ;
#21199 = CARTESIAN_POINT ( 'NONE',  ( 9.301828245743150703, -17.36685844811330171, -35.76733356948250275 ) ) ;
#21200 = CARTESIAN_POINT ( 'NONE',  ( 9.205734167420699166, -27.61618894467930119, -32.14999999999999858 ) ) ;
#21202 = ADVANCED_FACE ( 'NONE', ( #20450 ), #23857, .T. ) ;
#21201 = CARTESIAN_POINT ( 'NONE',  ( 46.91399176935180293, 22.65135599081870055, -75.82172624862269572 ) ) ;
#21203 = CARTESIAN_POINT ( 'NONE',  ( 65.25681082723269810, 1.383811055320669947, -60.95624653118409242 ) ) ;
#21204 = CARTESIAN_POINT ( 'NONE',  ( 75.18413422297084026, -30.89995173026953523, -11.96273407203979211 ) ) ;
#21205 = CARTESIAN_POINT ( 'NONE',  ( 12.36320305067610015, 33.31445045643330616, -15.76422791930239953 ) ) ;
#21206 = CARTESIAN_POINT ( 'NONE',  ( 14.71607358137469213, -49.61616928914560987, -83.19610070255293977 ) ) ;
#21207 = CIRCLE ( 'NONE', #25365, 1.999999999999999112 ) ;
#21208 = DIRECTION ( 'NONE',  ( 0.000000000000000000, 1.000000000000000000, 0.000000000000000000 ) ) ;
#21209 = CARTESIAN_POINT ( 'NONE',  ( 14.13958958331975602, 1.371102756008198975, -35.06583844469734146 ) ) ;
#21210 = FACE_OUTER_BOUND ( 'NONE', #27996, .T. ) ;
#21211 = CARTESIAN_POINT ( 'NONE',  ( 24.04493737213824289, -14.58064571430853995, -79.46600363739567285 ) ) ;
#21212 = CARTESIAN_POINT ( 'NONE',  ( -25.78889119571919863, -40.94810731387600100, -54.35424806255070251 ) ) ;
#21213 = EDGE_LOOP ( 'NONE', ( #30277, #37414 ) ) ;
#21214 = CARTESIAN_POINT ( 'NONE',  ( 52.80965640710000031, -49.67361798074160362, -48.67334656000949877 ) ) ;
#21215 = LINE ( 'NONE', #16790, #27856 ) ;
#21216 = CARTESIAN_POINT ( 'NONE',  ( 24.04491733993996760, -15.63677092532139312, -65.79315946755016853 ) ) ;
#21217 = CARTESIAN_POINT ( 'NONE',  ( 13.40139815547580149, 19.60627775220709879, -21.60243834236359817 ) ) ;
#21218 = CARTESIAN_POINT ( 'NONE',  ( 57.41989411400300014, 14.57099383176320018, -26.28150916840570162 ) ) ;
#21219 = CARTESIAN_POINT ( 'NONE',  ( 50.46752463075389983, 18.34784747648950187, -76.16325466870340222 ) ) ;
#21220 = CARTESIAN_POINT ( 'NONE',  ( 52.78692660382639446, 18.45971159535350026, -48.74514607373690467 ) ) ;
#21221 = CARTESIAN_POINT ( 'NONE',  ( 71.27241355379879906, 0.9209567800143640959, -70.76376997076650355 ) ) ;
#21222 = DIRECTION ( 'NONE',  ( 1.000000000000000000, 0.000000000000000000, 0.000000000000000000 ) ) ;
#21223 = CARTESIAN_POINT ( 'NONE',  ( 63.80692360858208900, -44.33172560060000222, -10.42320585664760024 ) ) ;
#21224 = ORIENTED_EDGE ( 'NONE', *, *, #40410, .F. ) ;
#21225 = CARTESIAN_POINT ( 'NONE',  ( 15.44167508794500066, -23.03423904108869991, -75.59696200394320442 ) ) ;
#21226 = ORIENTED_EDGE ( 'NONE', *, *, #45795, .F. ) ;
#21227 = EDGE_CURVE ( 'NONE', #29784, #23138, #13773, .T. ) ;
#21228 = CARTESIAN_POINT ( 'NONE',  ( 72.88423911510749065, 1.325841671674440114, -68.92527065596381419 ) ) ;
#21229 = CARTESIAN_POINT ( 'NONE',  ( 47.51461438356749767, -54.58063482146310008, -54.74847341959169711 ) ) ;
#21230 = CARTESIAN_POINT ( 'NONE',  ( 16.25075000454472374, -7.683118076734416491, -49.29699827634726006 ) ) ;
#21231 = FACE_OUTER_BOUND ( 'NONE', #28654, .T. ) ;
#21232 = CARTESIAN_POINT ( 'NONE',  ( 60.88462772975219650, 14.97986367131530017, -48.34569376290319553 ) ) ;
#21233 = FACE_BOUND ( 'NONE', #27285, .T. ) ;
#21234 = DIRECTION ( 'NONE',  ( 0.000000000000000000, 0.000000000000000000, -1.000000000000000000 ) ) ;
#21235 = CARTESIAN_POINT ( 'NONE',  ( 71.59408232549860429, 1.419970371292400113, -61.16051820649249748 ) ) ;
#21236 = VECTOR ( 'NONE', #50816, 1000.000000000000000 ) ;
#21237 = CARTESIAN_POINT ( 'NONE',  ( 24.01953174018752435, -16.26277903687216408, -71.53370740282881002 ) ) ;
#21238 = CARTESIAN_POINT ( 'NONE',  ( 64.97332050699269246, 0.9209334348186318797, -70.75011546227260339 ) ) ;
#21239 = EDGE_LOOP ( 'NONE', ( #41846, #22716, #66, #25120, #48394, #13955 ) ) ;
#21240 = CARTESIAN_POINT ( 'NONE',  ( 13.89744741070980005, -51.22086835671689897, -22.99801678904039903 ) ) ;
#21241 = EDGE_CURVE ( 'NONE', #41111, #23933, #17950, .T. ) ;
#21242 = CARTESIAN_POINT ( 'NONE',  ( 53.63393739769619373, -62.11618894467930119, 17.35000000000000142 ) ) ;
#21243 = ORIENTED_EDGE ( 'NONE', *, *, #41104, .F. ) ;
#21244 = DIRECTION ( 'NONE',  ( 0.3863301728269178947, 0.9223605572462016955, 0.000000000000000000 ) ) ;
#21245 = FACE_OUTER_BOUND ( 'NONE', #30589, .T. ) ;
#21246 = CARTESIAN_POINT ( 'NONE',  ( -1.866062602303798723, -15.61618894467929763, -18.58999999999999986 ) ) ;
#21247 = CARTESIAN_POINT ( 'NONE',  ( 52.52866728376119454, 19.54011015037300325, -76.33211554319051118 ) ) ;
#21248 = ORIENTED_EDGE ( 'NONE', *, *, #25179, .F. ) ;
#21249 = DIRECTION ( 'NONE',  ( -1.930570877714250223E-11, -1.000000000000000000, 6.141198660767589922E-12 ) ) ;
#21250 = LINE ( 'NONE', #1357, #26786 ) ;
#21251 = FACE_OUTER_BOUND ( 'NONE', #37446, .T. ) ;
#21252 = CARTESIAN_POINT ( 'NONE',  ( 9.550928694122980289, -10.65164299720190044, -56.99800709453249681 ) ) ;
#21253 = CIRCLE ( 'NONE', #19583, 31.00000000000000000 ) ;
#21254 = LINE ( 'NONE', #24918, #51434 ) ;
#21255 = CARTESIAN_POINT ( 'NONE',  ( 53.67902323473164472, 20.08789433012093539, -75.56984044762756980 ) ) ;
#21256 = PRODUCT_DEFINITION ( 'UNKNOWN', '', #40250, #36814 ) ;
#21257 = VERTEX_POINT ( 'NONE', #27810 ) ;
#21258 = CARTESIAN_POINT ( 'NONE',  ( 56.99379930123120630, -45.91441121812820114, -26.24653336503459755 ) ) ;
#21259 = CARTESIAN_POINT ( 'NONE',  ( 8.723884074801979693, -16.38936651614000084, -49.19956406921809133 ) ) ;
#21260 = CARTESIAN_POINT ( 'NONE',  ( 8.223031589278729570, -15.61632747405269939, -32.50766849176289952 ) ) ;
#21261 = EDGE_CURVE ( 'NONE', #30405, #51582, #10979, .T. ) ;
#21262 = AXIS2_PLACEMENT_3D ( 'NONE', #37532, #25204, #5320 ) ;
#21263 = CARTESIAN_POINT ( 'NONE',  ( 14.04520966608050081, 21.07290090200200083, -75.74020909530109691 ) ) ;
#21264 = EDGE_CURVE ( 'NONE', #40071, #23870, #4998, .T. ) ;
#21265 = VECTOR ( 'NONE', #296, 1000.000000000000000 ) ;
#21266 = CARTESIAN_POINT ( 'NONE',  ( 8.222313118464692039, -15.61611924975770016, -60.79233150823699816 ) ) ;
#21267 = EDGE_CURVE ( 'NONE', #5164, #41828, #34673, .T. ) ;
#21268 = CARTESIAN_POINT ( 'NONE',  ( 8.223201290577328848, -15.61599831009169925, -56.79233150823699816 ) ) ;
#21269 = EDGE_CURVE ( 'NONE', #34347, #15986, #7660, .T. ) ;
#21270 = CARTESIAN_POINT ( 'NONE',  ( 24.04346245338579990, -17.94473658267029847, -55.59880359483129553 ) ) ;
#21271 = ORIENTED_EDGE ( 'NONE', *, *, #4832, .F. ) ;
#21272 = CARTESIAN_POINT ( 'NONE',  ( 54.39377529478350226, -47.82348005630770160, -26.11201681070369673 ) ) ;
#21273 = CARTESIAN_POINT ( 'NONE',  ( 15.49194271725979988, -51.11618894182689843, -21.93290768620759934 ) ) ;
#21274 = DIRECTION ( 'NONE',  ( 0.6888026391158329487, -0.7071067811865494601, 0.1598465650148944150 ) ) ;
#21275 = CARTESIAN_POINT ( 'NONE',  ( 10.98133074358459993, -10.80025665254149914, -52.08643336858800410 ) ) ;
#21276 = DIRECTION ( 'NONE',  ( 0.000000000000000000, 1.000000000000000000, 0.000000000000000000 ) ) ;
#21277 = VERTEX_POINT ( 'NONE', #24109 ) ;
#21278 = CARTESIAN_POINT ( 'NONE',  ( -8.099603983670419893, -44.89123915805890164, -5.203145410111580382 ) ) ;
#21279 = CARTESIAN_POINT ( 'NONE',  ( 47.31777781540550620, 23.47673220148309881, -54.77383212233990406 ) ) ;
#21280 = ADVANCED_FACE ( 'NONE', ( #35933 ), #51, .T. ) ;
#21281 = CARTESIAN_POINT ( 'NONE',  ( -11.39236625349560050, -33.81790884424879806, -54.64999999999999858 ) ) ;
#21282 = CARTESIAN_POINT ( 'NONE',  ( 63.17541640582520301, 1.096153228089719933, -62.34242842016509201 ) ) ;
#21283 = CARTESIAN_POINT ( 'NONE',  ( 68.13393739769630031, -48.11618894467697061, -70.54999999999976978 ) ) ;
#21284 = CARTESIAN_POINT ( 'NONE',  ( 11.01107119607550011, 33.80107206112160156, -17.34607913294370007 ) ) ;
#21285 = DIRECTION ( 'NONE',  ( 1.000000000000000000, 0.000000000000000000, 0.000000000000000000 ) ) ;
#21286 = DIRECTION ( 'NONE',  ( 0.000000000000000000, 0.000000000000000000, -1.000000000000000000 ) ) ;
#21287 = CARTESIAN_POINT ( 'NONE',  ( 72.83393739769620367, 1.883811055320669947, -68.84999999999999432 ) ) ;
#21288 = CARTESIAN_POINT ( 'NONE',  ( 53.55347996444280056, -49.37856166211740572, -49.15350056090500885 ) ) ;
#21289 = CARTESIAN_POINT ( 'NONE',  ( 9.448242879478044642, -16.81408130491302089, -67.39644184705419150 ) ) ;
#21290 = VECTOR ( 'NONE', #43583, 1000.000000000000114 ) ;
#21291 = CARTESIAN_POINT ( 'NONE',  ( 52.25110910887259763, 21.11888751745159709, -53.60439093749319994 ) ) ;
#21292 = EDGE_CURVE ( 'NONE', #24662, #26724, #48080, .T. ) ;
#21293 = CARTESIAN_POINT ( 'NONE',  ( 63.37498668061930829, 1.231980177647109986, -69.13347842061430981 ) ) ;
#21294 = CARTESIAN_POINT ( 'NONE',  ( 11.89321892211240161, 34.20364954171930094, -18.17421237891140251 ) ) ;
#21295 = VERTEX_POINT ( 'NONE', #11591 ) ;
#21296 = CARTESIAN_POINT ( 'NONE',  ( 20.04366315139102284, 23.92455260968660369, -19.04010690988194909 ) ) ;
#21297 = CARTESIAN_POINT ( 'NONE',  ( 8.967661537042060260, 31.98469721247670350, -46.63268446062889439 ) ) ;
#21298 = DIRECTION ( 'NONE',  ( 0.000000000000000000, 0.000000000000000000, -1.000000000000000000 ) ) ;
#21299 = CARTESIAN_POINT ( 'NONE',  ( 68.39016270601220526, -30.11595112179599809, -18.15415021036589849 ) ) ;
#21300 = ORIENTED_EDGE ( 'NONE', *, *, #37088, .T. ) ;
#21301 = CARTESIAN_POINT ( 'NONE',  ( 18.22835651418590430, 20.70615929725470039, -75.58342519351550948 ) ) ;
#21302 = B_SPLINE_CURVE_WITH_KNOTS ( 'NONE', 3,
 ( #25190, #29391, #14190, #41447, #33831, #6333, #38301, #42235, #9746, #2389, #22034, #18366, #34085, #13683, #45394, #50092, #34348, #21258, #1881, #10265, #29642, #37267, #50359, #17355, #21779, #1619, #25966, #25703, #26225, #14447, #9499 ),
 .UNSPECIFIED., .F., .F.,
 ( 4, 3, 3, 3, 3, 3, 3, 3, 3, 3, 4 ),
 ( -0.9179866166508640068, -0.9044986999917590254, -0.7348924114151850207, -0.6321994764267000466, -0.6191523904019210489, -0.4753206641776559493, -0.3314757346574650487, -0.2163403421623650846, -0.1749400520680369775, -0.1011994735390420175, 1.210143096841420629E-14 ),
 .UNSPECIFIED. ) ;
#21303 = ORIENTED_EDGE ( 'NONE', *, *, #26051, .T. ) ;
#21304 = ORIENTED_EDGE ( 'NONE', *, *, #21623, .F. ) ;
#21305 = DIRECTION ( 'NONE',  ( -0.5000000000000003331, -0.8660254037844385966, 0.000000000000000000 ) ) ;
#21306 = B_SPLINE_CURVE_WITH_KNOTS ( 'NONE', 3,
 ( #26790, #7154, #22848, #42801, #18930, #23869, #7407, #27561, #35942, #23107, #19708, #27308, #11864, #35435, #39125, #35172, #23613, #39633, #11342, #16037, #23353, #39893, #6897, #51431 ),
 .UNSPECIFIED., .F., .F.,
 ( 4, 2, 2, 2, 2, 2, 2, 2, 2, 2, 2, 4 ),
 ( 0.000000000000000000, 0.03124999605426864377, 0.06249999210853728754, 0.09374998816280592784, 0.1249999842170745751, 0.1562499802713432084, 0.1874999763256118557, 0.2499999684341491502, 0.3124999605426864169, 0.3749999526512237114, 0.4374999447597610058, 0.4999999368682983003 ),
 .UNSPECIFIED. ) ;
#21307 = ORIENTED_EDGE ( 'NONE', *, *, #12380, .F. ) ;
#21308 = CARTESIAN_POINT ( 'NONE',  ( 12.53104704357910038, -65.45992346937650552, -47.41792381619649888 ) ) ;
#21309 = CARTESIAN_POINT ( 'NONE',  ( 56.20148638111029982, -46.06399181071520132, -26.07311021849060140 ) ) ;
#21310 = CARTESIAN_POINT ( 'NONE',  ( 23.44593531291890187, -16.58422985608489952, -81.23899999999999011 ) ) ;
#21311 = AXIS2_PLACEMENT_3D ( 'NONE', #21037, #24696, #33084 ) ;
#21312 = CARTESIAN_POINT ( 'NONE',  ( 61.50946113848699781, 13.98876303943020005, -46.98789045329460379 ) ) ;
#21313 = CARTESIAN_POINT ( 'NONE',  ( 16.13393739769620083, -15.61618894467929941, -35.02873218748179340 ) ) ;
#21314 = EDGE_LOOP ( 'NONE', ( #17780, #3739, #17270, #17084 ) ) ;
#21315 = EDGE_CURVE ( 'NONE', #46086, #40660, #9413, .T. ) ;
#21316 = CARTESIAN_POINT ( 'NONE',  ( 15.93498023681340037, -22.66622264832809819, -69.35616034045719402 ) ) ;
#21317 = ORIENTED_EDGE ( 'NONE', *, *, #16365, .F. ) ;
#21318 = CARTESIAN_POINT ( 'NONE',  ( 54.86028353996010054, -45.11618894460420393, -14.11209852549220045 ) ) ;
#21319 = CARTESIAN_POINT ( 'NONE',  ( 13.13393739769619906, 32.28996932333459569, -46.39999999999999858 ) ) ;
#21320 = EDGE_LOOP ( 'NONE', ( #12809, #49825, #26538, #47121 ) ) ;
#21321 = CARTESIAN_POINT ( 'NONE',  ( 72.77398937677050128, 1.387412027389909985, -62.60488565353588797 ) ) ;
#21322 = CARTESIAN_POINT ( 'NONE',  ( 46.65068702493330477, -53.59610475534989860, -76.01748491306379663 ) ) ;
#21323 = CARTESIAN_POINT ( 'NONE',  ( 61.06898323382710458, 14.42329441383000166, -47.72188698851990551 ) ) ;
#21324 = CARTESIAN_POINT ( 'NONE',  ( 53.37797796334299250, 15.00503494411220018, -14.93909541112770079 ) ) ;
#21325 = CIRCLE ( 'NONE', #14645, 5.999999999999998224 ) ;
#21326 = DIRECTION ( 'NONE',  ( 1.000000000000000000, 0.000000000000000000, 0.000000000000000000 ) ) ;
#21327 = PLANE ( 'NONE',  #28346 ) ;
#21328 = CARTESIAN_POINT ( 'NONE',  ( 22.90015496201974088, -16.26211237549280852, -54.87756051468720386 ) ) ;
#21329 = CARTESIAN_POINT ( 'NONE',  ( 61.19331679372790234, 13.94935370702680011, -27.45781938327959537 ) ) ;
#21330 = EDGE_CURVE ( 'NONE', #26214, #31550, #47897, .T. ) ;
#21331 = CARTESIAN_POINT ( 'NONE',  ( 23.38644729089550012, -12.61821489005030017, -69.16273469725000211 ) ) ;
#21332 = B_SPLINE_SURFACE_WITH_KNOTS ( 'NONE', 3, 3, ( 
 ( #32733, #45081, #49028, #20437, #20694, #28561, #8931 ),
 ( #24356, #40627, #9191, #1573, #41402, #25399, #1056 ),
 ( #36424, #17309, #28298, #44302, #36683, #17051, #8410 ),
 ( #13134, #44562, #24617, #4996, #532, #49286, #9450 ),
 ( #41145, #40370, #16518, #12867, #32466, #4728, #25142 ),
 ( #37222, #21212, #29084, #48496, #5260, #1319, #33271 ),
 ( #4467, #13385, #29344, #20958, #12599, #786, #5520 ),
 ( #17564, #45346, #12336, #36954, #48763, #16785, #24876 ),
 ( #28823, #44824, #37475, #40886, #33532, #18841, #50568 ),
 ( #34039, #18320, #6809, #33785, #6541, #17813, #49796 ),
 ( #50315, #34302, #38254, #14400, #42714, #46653, #25659 ),
 ( #29597, #2874, #22761, #2616, #29846, #50048, #14658 ),
 ( #45867, #38782, #49547, #37736, #14142, #25915, #9698 ),
 ( #30368, #46393, #10482, #13637, #1833, #6289, #9951 ),
 ( #30112, #45601, #18585, #41928, #41662, #21729, #30628 ),
 ( #10736, #26437, #5765, #13887, #6026, #22504, #21987 ),
 ( #2347, #46131, #18070, #42453, #38515, #37997, #2094 ),
 ( #10219, #22245, #26179, #42190, #34564, #26691, #12030 ) ),
 .UNSPECIFIED., .F., .F., .F.,
 ( 4, 2, 2, 2, 2, 2, 2, 2, 4 ),
 ( 4, 1, 1, 1, 4 ),
 ( -1.510109315586890100, -1.104486737752440106, -0.6746458442922780296, -0.2928561180551860210, 0.000000000000000000, 0.2928561180551860210, 0.6746458442922800280, 1.104486737752599979, 1.510109315586930068 ),
 ( -0.002513234661244860123, 0.2500000000000000000, 0.5000000000000000000, 0.7500000000000000000, 1.000404478440260148 ),
 .UNSPECIFIED. ) ;
#21333 = ORIENTED_EDGE ( 'NONE', *, *, #21623, .T. ) ;
#21334 = CARTESIAN_POINT ( 'NONE',  ( 56.55198054733560298, 16.47836500032180140, -47.99512079638530082 ) ) ;
#21335 = CIRCLE ( 'NONE', #31392, 2.000000000000001776 ) ;
#21336 = CARTESIAN_POINT ( 'NONE',  ( 73.26121012496899709, 0.8838110553206759423, -62.53374032209040223 ) ) ;
#21337 = CARTESIAN_POINT ( 'NONE',  ( 76.10455262750920724, -42.22089123566479429, -13.51974447861309869 ) ) ;
#21338 = CARTESIAN_POINT ( 'NONE',  ( 72.83400132021240836, 0.9897451961558710876, -69.38063463722799895 ) ) ;
#21339 = CARTESIAN_POINT ( 'NONE',  ( 14.63393739769620083, -42.11618894467930119, -34.64999999999999858 ) ) ;
#21340 = CARTESIAN_POINT ( 'NONE',  ( 82.13853704237929776, -45.11618894467940066, -46.42699167578030028 ) ) ;
#21341 = CARTESIAN_POINT ( 'NONE',  ( 17.01970876327451165, -22.38319278097903720, -78.91115185007626565 ) ) ;
#21342 = CARTESIAN_POINT ( 'NONE',  ( 49.33069834983029978, -53.71595991359180289, -54.59303725311939814 ) ) ;
#21343 = CARTESIAN_POINT ( 'NONE',  ( 42.05805429857900180, -44.46257822744319554, -5.167112339002620125 ) ) ;
#21344 = CARTESIAN_POINT ( 'NONE',  ( 24.04492240731919850, -15.63209485227305073, -33.50830522199780859 ) ) ;
#21345 = CARTESIAN_POINT ( 'NONE',  ( 18.39482185675899828, -51.45286096149530408, -74.99552951437290460 ) ) ;
#21347 = EDGE_CURVE ( 'NONE', #45957, #9803, #28315, .T. ) ;
#21346 = CARTESIAN_POINT ( 'NONE',  ( 68.13393739769620083, 19.38381105532069881, -65.65000000000000568 ) ) ;
#21348 = VERTEX_POINT ( 'NONE', #16279 ) ;
#21349 = CARTESIAN_POINT ( 'NONE',  ( 22.04518293870870238, -20.15092934432739824, -43.27563812998649695 ) ) ;
#21350 =( BOUNDED_CURVE ( )  B_SPLINE_CURVE ( 2, ( #21281, #9520, #5837 ),
 .UNSPECIFIED., .F., .T. ) 
 B_SPLINE_CURVE_WITH_KNOTS ( ( 3, 3 ),
 ( 0.1016765273446490064, 1.071465066788269915 ),
 .UNSPECIFIED. ) 
 CURVE ( )  GEOMETRIC_REPRESENTATION_ITEM ( )  RATIONAL_B_SPLINE_CURVE ( ( 1.000011650623809922, 1.000064461280040007, 1.000064793140389874 ) ) 
 REPRESENTATION_ITEM ( '' )  );
#21351 = CARTESIAN_POINT ( 'NONE',  ( 64.63032832047218790, 1.424120032878319897, -61.18002170558170150 ) ) ;
#21352 = ORIENTED_EDGE ( 'NONE', *, *, #27475, .T. ) ;
#21353 = CARTESIAN_POINT ( 'NONE',  ( 16.13393739769620083, -15.61618894467929941, -3.187564294433600232 ) ) ;
#21354 = CARTESIAN_POINT ( 'NONE',  ( 60.67234038688799558, -45.64753983419380035, -47.54984858108749535 ) ) ;
#21355 = CARTESIAN_POINT ( 'NONE',  ( 23.43760361721910002, 17.88421590754850143, -34.68023162149790295 ) ) ;
#21356 = CARTESIAN_POINT ( 'NONE',  ( 50.12047694090430383, 18.16987201063400192, -76.14999999999999147 ) ) ;
#21358 = DIRECTION ( 'NONE',  ( 0.000000000000000000, 0.000000000000000000, 1.000000000000000000 ) ) ;
#21357 = CARTESIAN_POINT ( 'NONE',  ( 43.93192822685114152, 8.716773305526617222, -66.98897554911386010 ) ) ;
#21359 = AXIS2_PLACEMENT_3D ( 'NONE', #16775, #32458, #32210 ) ;
#21360 = CARTESIAN_POINT ( 'NONE',  ( 12.34706755911540021, -9.666216171624100184, -60.16676433707719696 ) ) ;
#21361 = CARTESIAN_POINT ( 'NONE',  ( 41.16399130181100219, -45.54541204712649716, -6.123782152551889624 ) ) ;
#21362 = ORIENTED_EDGE ( 'NONE', *, *, #23152, .T. ) ;
#21363 = ORIENTED_EDGE ( 'NONE', *, *, #2523, .T. ) ;
#21364 = ORIENTED_EDGE ( 'NONE', *, *, #7034, .T. ) ;
#21365 = ORIENTED_EDGE ( 'NONE', *, *, #188, .F. ) ;
#21366 = CARTESIAN_POINT ( 'NONE',  ( 61.67596629463390201, -45.13022690132009984, -46.63288306418059648 ) ) ;
#21367 = CARTESIAN_POINT ( 'NONE',  ( 52.82265541972740408, -49.70184132309329783, -48.95329528328969815 ) ) ;
#21368 = DIRECTION ( 'NONE',  ( -0.6047562208151086027, -0.7964106436916998932, 0.000000000000000000 ) ) ;
#21369 = CARTESIAN_POINT ( 'NONE',  ( 54.57122049157750610, -51.56176576482789642, -53.75487193063269586 ) ) ;
#21370 = VERTEX_POINT ( 'NONE', #48512 ) ;
#21371 = EDGE_CURVE ( 'NONE', #8034, #41415, #48544, .T. ) ;
#21372 = ORIENTED_EDGE ( 'NONE', *, *, #37134, .T. ) ;
#21373 = EDGE_LOOP ( 'NONE', ( #42341, #13305, #42865, #14298, #33158 ) ) ;
#21374 = VECTOR ( 'NONE', #38956, 1000.000000000000114 ) ;
#21375 = PLANE ( 'NONE',  #14518 ) ;
#21376 = ADVANCED_FACE ( 'NONE', ( #13836 ), #21903, .F. ) ;
#21377 = CARTESIAN_POINT ( 'NONE',  ( 9.366491660071980974, -15.45061801826404313, -65.85496231377463516 ) ) ;
#21378 = CARTESIAN_POINT ( 'NONE',  ( 68.13393739769620083, 18.13381105532069881, -71.50000000000000000 ) ) ;
#21379 = ORIENTED_EDGE ( 'NONE', *, *, #1995, .T. ) ;
#21380 = CARTESIAN_POINT ( 'NONE',  ( 63.43393739769620510, 1.883811055320669947, -65.65000000000000568 ) ) ;
#21381 = CARTESIAN_POINT ( 'NONE',  ( 52.38320847335089780, -50.28303243813110157, -76.75839862240199807 ) ) ;
#21382 = CARTESIAN_POINT ( 'NONE',  ( 15.24808072932934522, -22.38318161335044820, -46.99448119687986747 ) ) ;
#21383 = FACE_OUTER_BOUND ( 'NONE', #37096, .T. ) ;
#21384 = CIRCLE ( 'NONE', #28079, 11.00000000000000000 ) ;
#21385 = CARTESIAN_POINT ( 'NONE',  ( 9.605521497733009895, -11.26113057208659995, -67.19975531119949608 ) ) ;
#21386 = LINE ( 'NONE', #41575, #9607 ) ;
#21387 = CARTESIAN_POINT ( 'NONE',  ( 42.17658700080410483, 13.90468392624960003, -6.213782667886099453 ) ) ;
#21388 = CARTESIAN_POINT ( 'NONE',  ( 42.50318722107469682, -43.99659477718180511, -4.913421252495600022 ) ) ;
#21389 = CARTESIAN_POINT ( 'NONE',  ( 72.07540109225739400, 1.000506532484820132, -61.12530190143370135 ) ) ;
#21390 = CARTESIAN_POINT ( 'NONE',  ( -1.266062602303798856, -15.61618894538776736, -7.049999999999999822 ) ) ;
#21391 = EDGE_CURVE ( 'NONE', #33379, #1986, #33985, .T. ) ;
#21392 = CARTESIAN_POINT ( 'NONE',  ( 63.97401018632380243, 1.443559287490330023, -69.67384056315309238 ) ) ;
#21393 = VECTOR ( 'NONE', #13570, 1000.000000000000000 ) ;
#21394 = CARTESIAN_POINT ( 'NONE',  ( 46.53794730597209650, 8.809177800381760903, -54.64300708228900305 ) ) ;
#21395 = CARTESIAN_POINT ( 'NONE',  ( 66.35712187483230196, -0.6058384114035900714, -16.95628796889650047 ) ) ;
#21396 = EDGE_CURVE ( 'NONE', #31436, #16348, #45814, .T. ) ;
#21397 = ORIENTED_EDGE ( 'NONE', *, *, #37789, .F. ) ;
#21398 = CIRCLE ( 'NONE', #18048, 0.9999999999999974465 ) ;
#21399 = CARTESIAN_POINT ( 'NONE',  ( 14.58589179554379989, -51.79680004542600358, -75.65449215554859563 ) ) ;
#21400 = CARTESIAN_POINT ( 'NONE',  ( 57.37350358383859827, 18.90030437368070082, -52.61683795673179986 ) ) ;
#21401 = B_SPLINE_CURVE_WITH_KNOTS ( 'NONE', 3,
 ( #28207, #439, #36592, #44207, #8305, #24261, #16684, #32642, #20341, #12499, #28724, #16428, #44727, #24782, #40791, #9574, #13255, #22118, #25530, #6160, #33659, #37872, #13763, #6422, #46266, #49674, #33911, #29722 ),
 .UNSPECIFIED., .F., .F.,
 ( 4, 2, 1, 1, 1, 1, 2, 2, 2, 2, 2, 2, 2, 2, 2, 4 ),
 ( 0.5000036702591513782, 0.5004919479249139158, 0.5009802255906764534, 0.5019567809222015287, 0.5039098915852517901, 0.5078161129113522021, 0.5156285555635529150, 0.5312534408679545628, 0.5625032114767575253, 0.6250027526943636724, 0.6875022939119698195, 0.7500018351295759667, 0.8125013763471820027, 0.8750009175647879278, 0.9375004587823939639, 1.000000000000000000 ),
 .UNSPECIFIED. ) ;
#21402 = CARTESIAN_POINT ( 'NONE',  ( 46.43766614693377903, -40.11729158708158849, -54.83318600516120966 ) ) ;
#21403 = CARTESIAN_POINT ( 'NONE',  ( 14.18091115246270029, -22.39322721071389921, -77.43649130894630161 ) ) ;
#21404 = CARTESIAN_POINT ( 'NONE',  ( 23.34951741632489686, -14.96832030630810095, -32.14999999999999858 ) ) ;
#21405 = CARTESIAN_POINT ( 'NONE',  ( 55.76693333300482891, -45.94012783645938924, -17.15566813129047219 ) ) ;
#21406 = CARTESIAN_POINT ( 'NONE',  ( 10.91841378338849999, 33.81381314252419656, -17.66395372719320278 ) ) ;
#21408 = DIRECTION ( 'NONE',  ( -0.8660254037844428154, -0.4999999999999928946, 0.000000000000000000 ) ) ;
#21407 = CARTESIAN_POINT ( 'NONE',  ( 13.61938558678000000, 20.19483563406610216, -23.15000000000000213 ) ) ;
#21409 = CARTESIAN_POINT ( 'NONE',  ( 18.06932202639930196, -55.56934008872529773, -76.14999999999999147 ) ) ;
#21410 = CARTESIAN_POINT ( 'NONE',  ( 48.07874646582410350, 23.06343134960649977, -54.84615067176530090 ) ) ;
#21411 = ORIENTED_EDGE ( 'NONE', *, *, #12785, .F. ) ;
#21412 = CARTESIAN_POINT ( 'NONE',  ( 17.70165363224570143, -22.49258516525739893, -61.27582937196799406 ) ) ;
#21413 = ORIENTED_EDGE ( 'NONE', *, *, #33687, .F. ) ;
#21414 = VECTOR ( 'NONE', #25604, 1000.000000000000000 ) ;
#21415 = CARTESIAN_POINT ( 'NONE',  ( 72.38393739883420608, 4.883811055320659733, -61.44999999999999574 ) ) ;
#21416 = CARTESIAN_POINT ( 'NONE',  ( 62.63393739769619373, 21.88381105532059934, 10.84999999999999964 ) ) ;
#21417 = CARTESIAN_POINT ( 'NONE',  ( 78.22251691734010137, -33.11618894467940066, -20.65000000000000213 ) ) ;
#21419 = CARTESIAN_POINT ( 'NONE',  ( 53.87546017034450330, 17.18069085124139761, -26.23270880884989964 ) ) ;
#21418 = CARTESIAN_POINT ( 'NONE',  ( 83.62075525755088279, 13.54933044287569999, -47.10035895585609467 ) ) ;
#21420 = CARTESIAN_POINT ( 'NONE',  ( 9.491729301919979989, -13.24476947334350108, -75.56197422286339815 ) ) ;
#21421 = DIRECTION ( 'NONE',  ( 0.000000000000000000, -1.000000000000000000, 0.000000000000000000 ) ) ;
#21422 = CARTESIAN_POINT ( 'NONE',  ( 55.36114930388180255, -45.13341976228700503, -14.57736059671599804 ) ) ;
#21423 = LINE ( 'NONE', #13086, #8001 ) ;
#21424 = CIRCLE ( 'NONE', #8916, 14.50000000000000178 ) ;
#21425 = ORIENTED_EDGE ( 'NONE', *, *, #34004, .F. ) ;
#21426 = ORIENTED_EDGE ( 'NONE', *, *, #31558, .F. ) ;
#21427 = CARTESIAN_POINT ( 'NONE',  ( 11.70888777236110023, -64.91672506495389428, -16.37375727426629979 ) ) ;
#21428 = CARTESIAN_POINT ( 'NONE',  ( 10.96434002348909864, 32.60498813690350062, -45.01351260974220025 ) ) ;
#21429 = CARTESIAN_POINT ( 'NONE',  ( 12.33464918225277174, -8.580518978903178606, -38.85044401595073538 ) ) ;
#21430 = DIRECTION ( 'NONE',  ( -1.000000000000000000, 0.000000000000000000, 0.000000000000000000 ) ) ;
#21431 = CARTESIAN_POINT ( 'NONE',  ( 17.98749078828956982, -7.616188944679219475, -34.79644660940672907 ) ) ;
#21432 = AXIS2_PLACEMENT_3D ( 'NONE', #41855, #37661, #49984 ) ;
#21433 = VERTEX_POINT ( 'NONE', #10165 ) ;
#21434 = CARTESIAN_POINT ( 'NONE',  ( -10.08776064405109985, -44.63142044503610606, -43.53771261949579952 ) ) ;
#21435 = AXIS2_PLACEMENT_3D ( 'NONE', #18977, #50699, #34957 ) ;
#21436 = DIRECTION ( 'NONE',  ( 1.000000000000000000, 8.701345253104295327E-30, 2.840828347717470042E-11 ) ) ;
#21437 = EDGE_CURVE ( 'NONE', #23493, #28405, #1837, .T. ) ;
#21438 = FACE_OUTER_BOUND ( 'NONE', #27428, .T. ) ;
#21439 = CARTESIAN_POINT ( 'NONE',  ( 9.221403253415356716, -19.60030155675170604, -60.34101711567728188 ) ) ;
#21440 = CARTESIAN_POINT ( 'NONE',  ( 59.32371920583819502, -2.960042943344160182, -15.67710711396670042 ) ) ;
#21441 = CARTESIAN_POINT ( 'NONE',  ( 51.21769384557849492, -49.33082554619760174, -76.45366765177809043 ) ) ;
#21442 = EDGE_CURVE ( 'NONE', #31681, #1406, #42330, .T. ) ;
#21443 = CARTESIAN_POINT ( 'NONE',  ( 24.04477596867337041, -15.61618922203197357, -43.50766101656756746 ) ) ;
#21444 = ORIENTED_EDGE ( 'NONE', *, *, #20720, .T. ) ;
#21445 = CARTESIAN_POINT ( 'NONE',  ( 53.25888871246090162, -49.10877824327840102, -26.73652702851729757 ) ) ;
#21446 = CARTESIAN_POINT ( 'NONE',  ( 68.13393739769810509, 19.38381105532030091, -71.50000000000198952 ) ) ;
#21447 = EDGE_LOOP ( 'NONE', ( #4560, #39023, #13475, #4239 ) ) ;
#21448 = CARTESIAN_POINT ( 'NONE',  ( 9.221390525194372856, -11.63209808988130334, -52.95899869926838477 ) ) ;
#21449 = FACE_OUTER_BOUND ( 'NONE', #3157, .T. ) ;
#21450 = CARTESIAN_POINT ( 'NONE',  ( 12.61940550337589961, -22.63295351940629985, -32.66030136746149992 ) ) ;
#21451 = CARTESIAN_POINT ( 'NONE',  ( 13.61938558664210142, -51.42721352535720314, -23.00040036072969940 ) ) ;
#21452 = AXIS2_PLACEMENT_3D ( 'NONE', #36819, #17178, #44950 ) ;
#21453 = CARTESIAN_POINT ( 'NONE',  ( 56.20907041320840136, 19.47117149094080091, -75.13105742454641245 ) ) ;
#21454 = CARTESIAN_POINT ( 'NONE',  ( 46.93943911961020632, -53.70440791814009884, -75.90649761523269490 ) ) ;
#21455 = EDGE_LOOP ( 'NONE', ( #38411, #3935, #48100, #3338 ) ) ;
#21456 = CARTESIAN_POINT ( 'NONE',  ( 56.28192814615630368, 14.29581962067599932, -17.93020402604240005 ) ) ;
#21457 = CARTESIAN_POINT ( 'NONE',  ( 57.02861371931150103, -50.62805676436050106, -53.87746547617770432 ) ) ;
#21458 = VECTOR ( 'NONE', #12021, 1000.000000000000000 ) ;
#21459 = CARTESIAN_POINT ( 'NONE',  ( 12.65447590535320010, -9.481377877827920742, -34.18295494821010294 ) ) ;
#21460 = CARTESIAN_POINT ( 'NONE',  ( 61.28085239525059791, 14.36939662108470017, -47.67834120296360112 ) ) ;
#21461 = ADVANCED_FACE ( 'NONE', ( #37682 ), #46598, .T. ) ;
#21462 = ORIENTED_EDGE ( 'NONE', *, *, #18086, .F. ) ;
#21463 = CARTESIAN_POINT ( 'NONE',  ( 47.28501908003789822, 23.16294876505000033, -75.17093853428211503 ) ) ;
#21464 = CARTESIAN_POINT ( 'NONE',  ( 65.12253294394879788, 1.334812829108570131, -60.78020385162600547 ) ) ;
#21465 = LINE ( 'NONE', #37465, #50677 ) ;
#21466 = FACE_OUTER_BOUND ( 'NONE', #47879, .T. ) ;
#21467 = VECTOR ( 'NONE', #43729, 1000.000000000000000 ) ;
#21468 = CARTESIAN_POINT ( 'NONE',  ( 18.65038606164732826, -49.61612828316260249, -83.08753104956571178 ) ) ;
#21469 = AXIS2_PLACEMENT_3D ( 'NONE', #45917, #25708, #14198 ) ;
#21470 = FACE_OUTER_BOUND ( 'NONE', #9668, .T. ) ;
#21472 = CARTESIAN_POINT ( 'NONE',  ( 44.74727839785828110, -40.12401933091472728, -62.58727147069981100 ) ) ;
#21471 = DIRECTION ( 'NONE',  ( 1.000000000000000000, 0.000000000000000000, 0.000000000000000000 ) ) ;
#21473 = CARTESIAN_POINT ( 'NONE',  ( 61.30125735803210318, 13.99008570081610081, -46.43541770244350175 ) ) ;
#21474 = CARTESIAN_POINT ( 'NONE',  ( 14.06323322820019683, -7.911095412653208037, -68.92433645535102471 ) ) ;
#21475 = DIRECTION ( 'NONE',  ( 0.7800418122827239564, 0.000000000000000000, -0.6257273935913973961 ) ) ;
#21476 = ORIENTED_EDGE ( 'NONE', *, *, #15076, .F. ) ;
#21477 = CARTESIAN_POINT ( 'NONE',  ( 53.27424401219509775, -49.42912581425869689, -48.84492659952799443 ) ) ;
#21478 = ORIENTED_EDGE ( 'NONE', *, *, #28410, .T. ) ;
#21479 = CARTESIAN_POINT ( 'NONE',  ( 60.08384063771620021, -45.15096763946600333, -26.42493554971499847 ) ) ;
#21480 = LINE ( 'NONE', #33276, #51116 ) ;
#21481 = CARTESIAN_POINT ( 'NONE',  ( 13.34067846651199929, 19.89164641777950138, -21.90730044338819837 ) ) ;
#21482 = CARTESIAN_POINT ( 'NONE',  ( 17.73618694459234391, -14.45208650838193165, -16.68902128623620129 ) ) ;
#21483 = CARTESIAN_POINT ( 'NONE',  ( 14.94185921909920012, -8.567953771208047797, -81.67932580530198550 ) ) ;
#21484 = CARTESIAN_POINT ( 'NONE',  ( 50.08385623533860098, 18.00127108905680018, -76.14999999999999147 ) ) ;
#21485 = CARTESIAN_POINT ( 'NONE',  ( 53.48012894133849926, 18.14102095893770183, -49.05829627934659243 ) ) ;
#21486 = CARTESIAN_POINT ( 'NONE',  ( 24.04493737933958286, -16.65173024076593222, -57.54933420604645278 ) ) ;
#21487 = CARTESIAN_POINT ( 'NONE',  ( 75.02961066429510595, -45.11618894467940066, -15.00607640852310176 ) ) ;
#21488 = CIRCLE ( 'NONE', #46625, 17.70000000000000284 ) ;
#21489 = ORIENTED_EDGE ( 'NONE', *, *, #24452, .T. ) ;
#21490 = CARTESIAN_POINT ( 'NONE',  ( 15.19106124924670098, -8.225811491055798896, -70.52695041587159608 ) ) ;
#21491 = CARTESIAN_POINT ( 'NONE',  ( 73.07318775143950518, 0.8986939045430379913, -69.05651959838648679 ) ) ;
#21492 = CARTESIAN_POINT ( 'NONE',  ( 47.51346078803879891, -54.57248623694759715, -54.67578198258269850 ) ) ;
#21493 = CARTESIAN_POINT ( 'NONE',  ( 11.81035279570149221, -8.951068426379952925, -49.10926437117617382 ) ) ;
#21494 = CARTESIAN_POINT ( 'NONE',  ( 73.18852689059310990, 0.9219904752505979628, -62.41704322431660046 ) ) ;
#21495 = CARTESIAN_POINT ( 'NONE',  ( 11.19961949155312553, 34.01496270439587732, -18.17421237848505911 ) ) ;
#21496 = CARTESIAN_POINT ( 'NONE',  ( 71.62124566564099837, 0.9425424353906030062, -60.76751081460630388 ) ) ;
#21497 = CARTESIAN_POINT ( 'NONE',  ( 9.214865060109733719, -19.58814555416793013, -76.62618144234603790 ) ) ;
#21498 = CARTESIAN_POINT ( 'NONE',  ( 71.58063725038380198, 1.374525224580329885, -61.05282258189939881 ) ) ;
#21499 = DIRECTION ( 'NONE',  ( -1.000000000000000000, 0.000000000000000000, 0.000000000000000000 ) ) ;
#21500 = CARTESIAN_POINT ( 'NONE',  ( 64.89668540611309311, 1.325715844996850024, -70.41854262496009653 ) ) ;
#21501 = ORIENTED_EDGE ( 'NONE', *, *, #4953, .F. ) ;
#21502 = B_SPLINE_CURVE_WITH_KNOTS ( 'NONE', 3,
 ( #49754, #33739, #13845, #2304, #45300, #13590, #29299, #50271, #42144, #21429, #9409, #9908, #29555, #46089, #2570, #14359, #49244, #5982, #17768, #37689, #25866, #45558, #37951, #26387, #42405, #46348, #29802, #22458, #26132, #38466, #38209, #1787, #10171, #18278 ),
 .UNSPECIFIED., .F., .F.,
 ( 4, 2, 2, 2, 2, 2, 2, 2, 2, 2, 2, 2, 1, 1, 1, 1, 1, 1, 2, 4 ),
 ( 0.000000000000000000, 0.03125032255746391235, 0.06250064511492782471, 0.09375096767239174400, 0.1250012902298556494, 0.1875019353447834880, 0.2500025804597112988, 0.3125032255746391097, 0.3750038706895669760, 0.4375045158044947868, 0.4687548383619586922, 0.4843799996406906172, 0.4921925802800565797, 0.4960988705997395609, 0.4980520157595809683, 0.4990285883395016442, 0.4995168746294618711, 0.4997610177744420401, 0.4998830893469320413, 0.5000051609194220426 ),
 .UNSPECIFIED. ) ;
#21503 = CARTESIAN_POINT ( 'NONE',  ( 8.961073636172280032, -63.17872192377240026, -46.63307763104060655 ) ) ;
#21504 = ADVANCED_FACE ( 'NONE', ( #44841 ), #48776, .T. ) ;
#21505 = FACE_OUTER_BOUND ( 'NONE', #38319, .T. ) ;
#21506 = ORIENTED_EDGE ( 'NONE', *, *, #45388, .T. ) ;
#21507 = CARTESIAN_POINT ( 'NONE',  ( 9.026390854479029002, -47.84168788784550230, -54.64999999999999858 ) ) ;
#21509 = B_SPLINE_CURVE_WITH_KNOTS ( 'NONE', 3,
 ( #13724, #28906, #8492, #24698, #13215, #13471, #40453, #24439, #29426, #48588, #45433, #5602, #25485, #16873 ),
 .UNSPECIFIED., .F., .F.,
 ( 4, 2, 2, 2, 2, 2, 4 ),
 ( 0.000000000000000000, 0.07234295340347396408, 0.1754160052195452568, 0.3815621088516880088, 0.6397668613124120052, 0.9371651888848793188, 1.000000000000000000 ),
 .UNSPECIFIED. ) ;
#21508 = CARTESIAN_POINT ( 'NONE',  ( 15.24810682503254711, -8.849192852612759452, -69.91115498661820027 ) ) ;
#21510 = CARTESIAN_POINT ( 'NONE',  ( 14.06332153136815322, -23.32130534079293938, -70.09100312201769611 ) ) ;
#21511 = CARTESIAN_POINT ( 'NONE',  ( 52.95141701711300186, 19.80221096257439939, -76.06582151403830494 ) ) ;
#21512 = EDGE_LOOP ( 'NONE', ( #48034, #27230, #27309, #886 ) ) ;
#21513 = PRODUCT ( 'Foot Base', 'Foot Base', '', ( #36662 ) ) ;
#21514 = CARTESIAN_POINT ( 'NONE',  ( 29.13393739769619728, -35.78776181993320193, -84.65000000000000568 ) ) ;
#21515 = CARTESIAN_POINT ( 'NONE',  ( 68.13393739769618662, -0.1661889446793599900, -65.65000000000000568 ) ) ;
#21516 = AXIS2_PLACEMENT_3D ( 'NONE', #12048, #16740, #4167 ) ;
#21517 = CARTESIAN_POINT ( 'NONE',  ( 12.23782554533866929, -22.52769441490526248, -66.17096938631890168 ) ) ;
#21518 = CARTESIAN_POINT ( 'NONE',  ( 8.386807182601900834, -18.43836779909439727, -56.68113137027810211 ) ) ;
#21519 = CARTESIAN_POINT ( 'NONE',  ( 16.13393739769620083, -15.61618894467929941, -6.649999999999999467 ) ) ;
#21520 = CARTESIAN_POINT ( 'NONE',  ( 44.97398337673284630, -38.03923227423459963, -65.44976038934856888 ) ) ;
#21521 = ORIENTED_EDGE ( 'NONE', *, *, #51754, .F. ) ;
#21522 = CARTESIAN_POINT ( 'NONE',  ( 18.45800985347563739, 20.88376505810182238, -75.46937998430171035 ) ) ;
#21523 = CARTESIAN_POINT ( 'NONE',  ( 15.21491748573319924, -8.222807025248849655, -39.69329234158369957 ) ) ;
#21524 = DIRECTION ( 'NONE',  ( 0.000000000000000000, 0.000000000000000000, 1.000000000000000000 ) ) ;
#21525 = EDGE_CURVE ( 'NONE', #3978, #29027, #3537, .T. ) ;
#21526 = ADVANCED_FACE ( 'NONE', ( #18019 ), #51236, .T. ) ;
#21527 = CARTESIAN_POINT ( 'NONE',  ( 14.27557590264609999, 19.88380863237500051, -74.14994161014911356 ) ) ;
#21528 = CARTESIAN_POINT ( 'NONE',  ( 17.68200514164429293, -51.79680896053663020, -75.65449996341281746 ) ) ;
#21529 = CARTESIAN_POINT ( 'NONE',  ( 83.11128256222379207, -44.91457445506669899, -46.57919617705099569 ) ) ;
#21530 = CARTESIAN_POINT ( 'NONE',  ( 9.418179351659979659, -20.39963065291350119, -48.31066193697829902 ) ) ;
#21531 = ORIENTED_EDGE ( 'NONE', *, *, #8220, .F. ) ;
#21532 = CARTESIAN_POINT ( 'NONE',  ( 53.96734575795409938, -48.30637184247790117, -26.23153061636689998 ) ) ;
#21533 = CARTESIAN_POINT ( 'NONE',  ( 53.62362271036269590, -51.33149816580809954, -75.58100470206619548 ) ) ;
#21534 = CARTESIAN_POINT ( 'NONE',  ( 10.20255366368179928, 33.09845870078689956, -17.03222616606660011 ) ) ;
#21535 = CARTESIAN_POINT ( 'NONE',  ( 11.97520752817116652, -21.02746473356409140, -57.16110635108449856 ) ) ;
#21536 = CARTESIAN_POINT ( 'NONE',  ( 35.63393739769620083, -15.61618894467929941, -15.18999999999999950 ) ) ;
#21537 = EDGE_LOOP ( 'NONE', ( #43429, #50318, #14236, #8592, #34926, #28591 ) ) ;
#21538 = CARTESIAN_POINT ( 'NONE',  ( -10.88064226659390066, -42.34875619867930396, -6.242712440991480705 ) ) ;
#21539 = CARTESIAN_POINT ( 'NONE',  ( 47.41229157644860237, 23.41797196667260295, -54.89345655439770155 ) ) ;
#21540 = CIRCLE ( 'NONE', #23183, 17.63819660112499932 ) ;
#21541 = CARTESIAN_POINT ( 'NONE',  ( -31.36606260230380272, 21.88381105532059934, 11.84999999999999964 ) ) ;
#21542 = CARTESIAN_POINT ( 'NONE',  ( 63.26997363883779713, 1.264791438333809914, -62.42094564213650187 ) ) ;
#21543 = LINE ( 'NONE', #18657, #5603 ) ;
#21544 = CARTESIAN_POINT ( 'NONE',  ( 42.26864913267620238, 13.12941410943280118, -5.126484833154619558 ) ) ;
#21545 = CARTESIAN_POINT ( 'NONE',  ( 9.501539899509779730, -17.54678703817369012, -57.75637824400988052 ) ) ;
#21546 = CARTESIAN_POINT ( 'NONE',  ( 52.90855285609560354, 18.38725884964460278, -48.71990423803699599 ) ) ;
#21547 = DIRECTION ( 'NONE',  ( 0.000000000000000000, 0.000000000000000000, 1.000000000000000000 ) ) ;
#21548 = CARTESIAN_POINT ( 'NONE',  ( 59.53589770979640150, -46.29254236635570408, -47.84815983218079793 ) ) ;
#21549 = CARTESIAN_POINT ( 'NONE',  ( 9.366922913046613175, -16.22029336621082507, -67.42439374615231884 ) ) ;
#21550 = VECTOR ( 'NONE', #22842, 1000.000000000000000 ) ;
#21551 = CARTESIAN_POINT ( 'NONE',  ( 53.57016373187970260, 20.66090427507980110, -53.57659063368220131 ) ) ;
#21552 = CARTESIAN_POINT ( 'NONE',  ( 63.41196002899340556, 0.9486721756287949114, -69.35284629089670716 ) ) ;
#21553 = CARTESIAN_POINT ( 'NONE',  ( 11.96242383438930013, -65.43598681641390158, -17.67418089159339800 ) ) ;
#21554 = CARTESIAN_POINT ( 'NONE',  ( 50.04794199403829680, 13.88381105532070059, -10.32001505436120148 ) ) ;
#21555 = VERTEX_POINT ( 'NONE', #14091 ) ;
#21556 = CARTESIAN_POINT ( 'NONE',  ( 19.90664092702385801, 23.53180147038325742, -18.14526676646603320 ) ) ;
#21557 = CARTESIAN_POINT ( 'NONE',  ( 10.14348297095079943, 32.01596363797860079, -45.99327272258569366 ) ) ;
#21558 = DIRECTION ( 'NONE',  ( 1.000000000000000000, 0.000000000000000000, 0.000000000000000000 ) ) ;
#21559 = CARTESIAN_POINT ( 'NONE',  ( 66.36400972822720234, -30.63155050328590079, -16.96145626638979920 ) ) ;
#21560 = CARTESIAN_POINT ( 'NONE',  ( 12.20262750478389258, -8.709504227742451477, -80.84286210128752259 ) ) ;
#21561 = ORIENTED_EDGE ( 'NONE', *, *, #25928, .T. ) ;
#21562 = ORIENTED_EDGE ( 'NONE', *, *, #2011, .F. ) ;
#21563 = CARTESIAN_POINT ( 'NONE',  ( 15.29511290902269849, 12.56821928479459949, -59.64999999999999147 ) ) ;
#21564 = ADVANCED_FACE ( 'NONE', ( #18791 ), #8537, .T. ) ;
#21565 = ORIENTED_EDGE ( 'NONE', *, *, #50756, .F. ) ;
#21566 = CARTESIAN_POINT ( 'NONE',  ( 12.57686355069400008, -65.46300284260451008, -47.35844541283869802 ) ) ;
#21567 = CARTESIAN_POINT ( 'NONE',  ( 56.46641740571360657, -46.20943712337750497, -26.25094501701900285 ) ) ;
#21568 = DIRECTION ( 'NONE',  ( 0.9987374001630935361, 0.000000000000000000, -0.05023550054956103100 ) ) ;
#21569 = CARTESIAN_POINT ( 'NONE',  ( 61.67741675730779605, 13.93672178322469968, -46.82959687277750049 ) ) ;
#21570 = DIRECTION ( 'NONE',  ( 0.000000000000000000, 0.000000000000000000, -1.000000000000000000 ) ) ;
#21571 = ORIENTED_EDGE ( 'NONE', *, *, #12004, .F. ) ;
#21572 = CARTESIAN_POINT ( 'NONE',  ( 45.77379034717539241, 6.897320639510064133, -61.45073446201022449 ) ) ;
#21573 = B_SPLINE_SURFACE_WITH_KNOTS ( 'NONE', 3, 3, ( 
 ( #32438, #4954, #37186, #29306, #45308, #8630, #36646, #751 ),
 ( #9417, #16747, #48727, #12831, #20924, #34527, #38477, #50014 ),
 ( #21690, #9661, #46613, #5988, #10701, #17776, #42152, #6508 ),
 ( #6773, #26655, #2577, #37960, #30071, #18551, #9914, #49761 ),
 ( #49508, #50533, #34003, #2312, #30592, #13852, #30334, #2057 ),
 ( #10181, #29810, #45827, #6251, #33746, #10443, #13599, #46096 ),
 ( #25877, #1539, #42676, #25620, #41891, #17526, #22467, #22724 ),
 ( #21948, #33495, #29562, #45567, #41623, #5730, #14623, #26396 ),
 ( #37696, #42416, #18035, #1793, #14104, #18285, #26141, #22208 ) ),
 .UNSPECIFIED., .F., .F., .F.,
 ( 4, 1, 1, 1, 1, 1, 4 ),
 ( 4, 2, 2, 4 ),
 ( 0.000000000000000000, 0.1666666666666670182, 0.3333333333333329818, 0.5000000000000000000, 0.6666666666666670737, 0.8333333333333330373, 1.000009836239660110 ),
 ( -17.15520582519389947, -10.97516758816430027, -7.142721168756169803, -6.988377030140479285 ),
 .UNSPECIFIED. ) ;
#21574 = ORIENTED_EDGE ( 'NONE', *, *, #18249, .T. ) ;
#21575 = CARTESIAN_POINT ( 'NONE',  ( 49.19893965675269953, -45.20300092367129707, -10.60212966286649916 ) ) ;
#21576 = CARTESIAN_POINT ( 'NONE',  ( 16.13393739769620083, -15.61618894467929941, -15.65000000000000036 ) ) ;
#21577 = LINE ( 'NONE', #49393, #48560 ) ;
#21578 = ORIENTED_EDGE ( 'NONE', *, *, #51184, .T. ) ;
#21579 = CARTESIAN_POINT ( 'NONE',  ( 47.13216420861670031, -54.63565002646070212, -74.95072482230889932 ) ) ;
#21580 = FACE_OUTER_BOUND ( 'NONE', #51252, .T. ) ;
#21581 = CARTESIAN_POINT ( 'NONE',  ( 45.90332653426600018, 13.88381105525539994, -7.776724520636079774 ) ) ;
#21582 = EDGE_CURVE ( 'NONE', #21743, #27935, #27273, .T. ) ;
#21583 = CARTESIAN_POINT ( 'NONE',  ( -9.882013117715120032, -40.49932216338130075, -21.14999999999999858 ) ) ;
#21584 = CARTESIAN_POINT ( 'NONE',  ( 16.13393739769620083, -15.61618894467929941, -35.14999999999999858 ) ) ;
#21585 = CARTESIAN_POINT ( 'NONE',  ( 61.51097107413969667, 13.91173608902099978, -28.15130629814199992 ) ) ;
#21586 = CARTESIAN_POINT ( 'NONE',  ( 22.96503088535069992, -11.75317070163309907, -73.12368125043110467 ) ) ;
#21587 = VERTEX_POINT ( 'NONE', #31860 ) ;
#21588 = CARTESIAN_POINT ( 'NONE',  ( 24.04493739769619864, -15.61618894467929941, -32.14999999999999858 ) ) ;
#21589 = CARTESIAN_POINT ( 'NONE',  ( -9.818857736406330972, -43.25243607249999656, -5.498528025088970317 ) ) ;
#21590 = CARTESIAN_POINT ( 'NONE',  ( 16.13393739769620083, -15.61618894467929941, 4.450000000000000178 ) ) ;
#21591 = CARTESIAN_POINT ( 'NONE',  ( 72.79534234514369473, 1.367958924391410092, -68.95206439131310105 ) ) ;
#21592 = B_SPLINE_CURVE_WITH_KNOTS ( 'NONE', 3,
 ( #36461, #4503, #32508, #39906, #16827, #20737, #28081, #20220, #8189, #48801, #40926, #21000, #7932, #75, #44087, #24131, #40154, #4250, #36210, #16300, #28337, #48279, #46172, #41971, #17348, #21517, #38037, #45387, #33314, #10260, #6327, #25184, #1613, #13426, #49069 ),
 .UNSPECIFIED., .F., .F.,
 ( 4, 2, 1, 1, 1, 1, 1, 2, 2, 2, 2, 2, 2, 2, 2, 2, 2, 2, 2, 4 ),
 ( 0.4999984552117135994, 0.5002425965910047845, 0.5004867379702959695, 0.5009750207288782287, 0.5019515862460430800, 0.5039047172803724495, 0.5078109793490309665, 0.5156235034863478894, 0.5312485517609818464, 0.5624986483102496493, 0.6249988414087853661, 0.6874990345073210829, 0.7499992276058569107, 0.8124994207043927386, 0.8437495172536605414, 0.8749996138029284554, 0.9062497103521963693, 0.9374998069014641722, 0.9687499034507320861, 1.000000000000000000 ),
 .UNSPECIFIED. ) ;
#21593 = CYLINDRICAL_SURFACE ( 'NONE', #11451, 0.4999999999999980571 ) ;
#21594 = CARTESIAN_POINT ( 'NONE',  ( 71.33393739770049535, 11.38381105532070059, -69.34999999999999432 ) ) ;
#21595 = CARTESIAN_POINT ( 'NONE',  ( 13.75402769379030055, 19.05428965339309855, -20.97890654100300267 ) ) ;
#21596 = CARTESIAN_POINT ( 'NONE',  ( 22.90093740122328825, -16.50198959089620487, -78.49448387614262401 ) ) ;
#21597 = CARTESIAN_POINT ( 'NONE',  ( 49.20592918829389362, -53.85531719945320361, -55.00566101661709695 ) ) ;
#21598 = CARTESIAN_POINT ( 'NONE',  ( 8.222912444960085665, -16.65155373173890396, -56.75066771667979992 ) ) ;
#21599 = CARTESIAN_POINT ( 'NONE',  ( 24.04462826173309153, -15.61618628916268392, -33.50766512250601181 ) ) ;
#21600 = CARTESIAN_POINT ( 'NONE',  ( 18.50686185362269853, -51.29510989453680736, -74.37030622952239867 ) ) ;
#21601 = DIRECTION ( 'NONE',  ( 0.000000000000000000, 0.000000000000000000, 1.000000000000000000 ) ) ;
#21602 = EDGE_LOOP ( 'NONE', ( #20649, #38997, #25403, #3800, #11725 ) ) ;
#21603 = CARTESIAN_POINT ( 'NONE',  ( 22.96971382812329665, -18.57910219544439556, -51.19753123634840364 ) ) ;
#21604 = CARTESIAN_POINT ( 'NONE',  ( 64.60333993882289860, 1.138495779907959804, -60.85329768958769847 ) ) ;
#21605 = ORIENTED_EDGE ( 'NONE', *, *, #41504, .T. ) ;
#21606 = CARTESIAN_POINT ( 'NONE',  ( 9.366446932119513846, -15.48215974695313335, -33.85347959719207722 ) ) ;
#21607 = CARTESIAN_POINT ( 'NONE',  ( 60.95561879329019916, -45.63102361682189922, -47.66564892484940685 ) ) ;
#21608 = DIRECTION ( 'NONE',  ( 0.000000000000000000, 1.000000000000000000, 0.000000000000000000 ) ) ;
#21609 = CARTESIAN_POINT ( 'NONE',  ( 8.223487313465298598, -15.61606829411550024, -62.50766849176299189 ) ) ;
#21611 = DIRECTION ( 'NONE',  ( -2.490868089198564786E-23, -1.000000000000000000, 1.205421602240320019E-11 ) ) ;
#21610 = CARTESIAN_POINT ( 'NONE',  ( 44.69570754105031085, 8.776462964268782585, -63.28808277378300318 ) ) ;
#21612 = CARTESIAN_POINT ( 'NONE',  ( 53.29384558423090112, -50.54670888882439783, -38.31189016485959797 ) ) ;
#21613 = CARTESIAN_POINT ( 'NONE',  ( 42.67454888401100277, -45.92793478434160193, -7.343008119757059582 ) ) ;
#21614 = VERTEX_POINT ( 'NONE', #43175 ) ;
#21615 = ORIENTED_EDGE ( 'NONE', *, *, #8510, .T. ) ;
#21616 = ORIENTED_EDGE ( 'NONE', *, *, #19790, .F. ) ;
#21617 = EDGE_CURVE ( 'NONE', #17172, #50841, #29130, .T. ) ;
#21618 = VERTEX_POINT ( 'NONE', #7268 ) ;
#21619 = CARTESIAN_POINT ( 'NONE',  ( 61.22099285190670059, -45.29906686168950358, -47.03247545010540165 ) ) ;
#21620 = CARTESIAN_POINT ( 'NONE',  ( 52.88322703206500108, -49.67375961844999921, -49.00539243417760105 ) ) ;
#21621 = DIRECTION ( 'NONE',  ( -1.000000000000000000, 0.000000000000000000, 0.000000000000000000 ) ) ;
#21622 = CARTESIAN_POINT ( 'NONE',  ( 56.36239273759079538, -50.53819555927099572, -52.86232647623099723 ) ) ;
#21623 = EDGE_CURVE ( 'NONE', #46423, #47971, #37840, .T. ) ;
#21624 = ORIENTED_EDGE ( 'NONE', *, *, #35597, .T. ) ;
#21625 = ADVANCED_FACE ( 'NONE', ( #23984 ), #15131, .T. ) ;
#21626 = ORIENTED_EDGE ( 'NONE', *, *, #2098, .T. ) ;
#21627 = CARTESIAN_POINT ( 'NONE',  ( 56.27102381480889903, -50.57721995146319927, -52.87265154067429762 ) ) ;
#21628 = LINE ( 'NONE', #49959, #43665 ) ;
#21629 = DIRECTION ( 'NONE',  ( 0.000000000000000000, 1.000000000000000000, 0.000000000000000000 ) ) ;
#21630 = VERTEX_POINT ( 'NONE', #3335 ) ;
#21631 = CARTESIAN_POINT ( 'NONE',  ( 0.3209249304026170480, -8.218592747557250888, -34.64999999999999858 ) ) ;
#21632 = CARTESIAN_POINT ( 'NONE',  ( 52.00136175985360154, -50.03231718876410383, -76.70561731964021135 ) ) ;
#21633 = CARTESIAN_POINT ( 'NONE',  ( 63.93393739769619089, 1.883811055320669947, -68.84999999999999432 ) ) ;
#21634 = ADVANCED_FACE ( 'NONE', ( #31088 ), #40008, .T. ) ;
#21635 = CARTESIAN_POINT ( 'NONE',  ( 20.77912286130639785, -9.290922183486799213, -63.71412234440029465 ) ) ;
#21636 = CARTESIAN_POINT ( 'NONE',  ( 8.664097273252640008, 17.56341275872060237, -34.96018206680729890 ) ) ;
#21637 = CARTESIAN_POINT ( 'NONE',  ( 41.94961043596779149, 13.67826027404730027, -5.752299076171500047 ) ) ;
#21638 = ADVANCED_FACE ( 'NONE', ( #26911 ), #24404, .T. ) ;
#21639 = CARTESIAN_POINT ( 'NONE',  ( 41.87524915382199708, -44.35687246895969338, -5.012953300357450459 ) ) ;
#21640 = CARTESIAN_POINT ( 'NONE',  ( 68.13393739769847457, -50.70395984888145335, -72.15645085170113759 ) ) ;
#21641 = CARTESIAN_POINT ( 'NONE',  ( -10.41557261171689852, 11.58869671994870032, -6.169019698314530231 ) ) ;
#21642 = CIRCLE ( 'NONE', #9955, 1.000000000000000888 ) ;
#21643 = CARTESIAN_POINT ( 'NONE',  ( 63.90184877270480257, 1.348268598598709955, -69.74930279100139785 ) ) ;
#21644 = DIRECTION ( 'NONE',  ( -0.7071067811865475727, -0.7071067811865475727, 0.000000000000000000 ) ) ;
#21645 = VECTOR ( 'NONE', #6861, 1000.000000000000000 ) ;
#21646 = VECTOR ( 'NONE', #6503, 1000.000000000000114 ) ;
#21647 = CARTESIAN_POINT ( 'NONE',  ( 66.72606221067250942, 1.883603582144870003, -20.65075287695389861 ) ) ;
#21648 = EDGE_LOOP ( 'NONE', ( #1682, #11417, #32111, #3682, #42332 ) ) ;
#21649 = CARTESIAN_POINT ( 'NONE',  ( 14.16789401284239958, -52.35976395901120384, -75.83262351151699932 ) ) ;
#21650 = CARTESIAN_POINT ( 'NONE',  ( 57.27629353325620087, 19.36113991157819925, -53.60235154930700219 ) ) ;
#21651 = FACE_OUTER_BOUND ( 'NONE', #31795, .T. ) ;
#21652 = CYLINDRICAL_SURFACE ( 'NONE', #13413, 0.9999999999999988898 ) ;
#21653 =( BOUNDED_CURVE ( )  B_SPLINE_CURVE ( 3, ( #49457, #5938, #17725, #700 ),
 .UNSPECIFIED., .F., .T. ) 
 B_SPLINE_CURVE_WITH_KNOTS ( ( 4, 4 ),
 ( 4.712388980384691450, 5.229612381435808643 ),
 .UNSPECIFIED. ) 
 CURVE ( )  GEOMETRIC_REPRESENTATION_ITEM ( )  RATIONAL_B_SPLINE_CURVE ( ( 1.000000000000000000, 0.9778306343446301341, 0.9778306343446301341, 1.000000000000000000 ) ) 
 REPRESENTATION_ITEM ( '' )  );
#21655 = EDGE_CURVE ( 'NONE', #41542, #44367, #15238, .T. ) ;
#21654 = CARTESIAN_POINT ( 'NONE',  ( 23.09005290148149925, -13.91445552956680132, -32.14999999999999858 ) ) ;
#21656 = CARTESIAN_POINT ( 'NONE',  ( 47.64964229006469765, -54.53139074986410151, -55.13082436213850457 ) ) ;
#21657 = CARTESIAN_POINT ( 'NONE',  ( 22.84381469196726755, -14.09322211363766719, -50.77553680422087723 ) ) ;
#21658 = PLANE ( 'NONE',  #15042 ) ;
#21659 = CARTESIAN_POINT ( 'NONE',  ( 48.02726464836110409, 23.08853929931079918, -54.84894742480889818 ) ) ;
#21660 = ORIENTED_EDGE ( 'NONE', *, *, #5369, .F. ) ;
#21661 = CARTESIAN_POINT ( 'NONE',  ( 18.95614455194280268, -22.07975653177619790, -59.21613716431369312 ) ) ;
#21662 = VERTEX_POINT ( 'NONE', #22966 ) ;
#21663 = AXIS2_PLACEMENT_3D ( 'NONE', #18885, #23568, #34866 ) ;
#21664 = DIRECTION ( 'NONE',  ( 1.000000000000000000, 0.000000000000000000, 0.000000000000000000 ) ) ;
#21665 = CARTESIAN_POINT ( 'NONE',  ( 58.88698566692261238, -48.67252618344199533, -51.02964062410481461 ) ) ;
#21666 = CARTESIAN_POINT ( 'NONE',  ( 74.17629866868290378, 1.883811055320649963, -65.34607522167520699 ) ) ;
#21668 = CARTESIAN_POINT ( 'NONE',  ( 53.73390105979990494, 17.34280763946619786, -26.38585243011049997 ) ) ;
#21667 = CARTESIAN_POINT ( 'NONE',  ( 84.02215818083939780, 13.18587566258590016, -47.25304732090640414 ) ) ;
#21669 = CARTESIAN_POINT ( 'NONE',  ( 19.22002932807319553, -9.274375695040369294, -78.09698001689929470 ) ) ;
#21670 = CARTESIAN_POINT ( 'NONE',  ( 10.85466640524320070, 33.73459223951330443, -17.55961383757199812 ) ) ;
#21671 = CARTESIAN_POINT ( 'NONE',  ( 55.94725819174559689, -45.11618894467940066, -14.63509477631759914 ) ) ;
#21672 = DIRECTION ( 'NONE',  ( 1.000000000000000000, 0.000000000000000000, 0.000000000000000000 ) ) ;
#21673 = DIRECTION ( 'NONE',  ( 0.000000000000000000, 0.000000000000000000, -1.000000000000000000 ) ) ;
#21674 = VERTEX_POINT ( 'NONE', #27684 ) ;
#21675 = EDGE_LOOP ( 'NONE', ( #20406, #20959, #18222, #40587 ) ) ;
#21676 = CARTESIAN_POINT ( 'NONE',  ( 11.98493272671300147, -65.14404999958080111, -16.63579482025560097 ) ) ;
#21677 = CARTESIAN_POINT ( 'NONE',  ( 11.83192124503869991, 33.83054603674280969, -45.91061019192989789 ) ) ;
#21678 = CARTESIAN_POINT ( 'NONE',  ( 12.06284766121009966, -63.44323389162830296, -22.25048313876769868 ) ) ;
#21679 = EDGE_CURVE ( 'NONE', #44397, #7182, #51292, .T. ) ;
#21680 = VECTOR ( 'NONE', #18109, 1000.000000000000000 ) ;
#21681 = CARTESIAN_POINT ( 'NONE',  ( 13.00893739761190027, 34.28605925116320208, -47.75434321210310173 ) ) ;
#21682 = DIRECTION ( 'NONE',  ( -0.8660254037844379305, 0.5000000000000011102, 0.000000000000000000 ) ) ;
#21683 = AXIS2_PLACEMENT_3D ( 'NONE', #10072, #14517, #5635 ) ;
#21684 = CIRCLE ( 'NONE', #6678, 0.5000000000000000000 ) ;
#21685 = ORIENTED_EDGE ( 'NONE', *, *, #46107, .F. ) ;
#21686 = EDGE_CURVE ( 'NONE', #23531, #30985, #45396, .T. ) ;
#21687 = CARTESIAN_POINT ( 'NONE',  ( -3.761964000850550160, -48.86336368874830072, -38.03777212193249824 ) ) ;
#21688 = CARTESIAN_POINT ( 'NONE',  ( 52.82975622904280755, 18.42854261028849905, -28.15000000000000213 ) ) ;
#21689 = AXIS2_PLACEMENT_3D ( 'NONE', #16140, #32100, #36304 ) ;
#21690 = CARTESIAN_POINT ( 'NONE',  ( 47.83902694909610176, 23.41449876227819971, -55.43872205723609881 ) ) ;
#21691 = CARTESIAN_POINT ( 'NONE',  ( 61.12640465316060556, -1.652607533939269846, -15.96805516186100249 ) ) ;
#21692 = CARTESIAN_POINT ( 'NONE',  ( 50.65222755239680197, -50.00564526808049948, -76.16386725643910438 ) ) ;
#21693 = CARTESIAN_POINT ( 'NONE',  ( 60.29219879490389644, -46.03903543506309859, -47.96865620826579857 ) ) ;
#21694 = ORIENTED_EDGE ( 'NONE', *, *, #457, .F. ) ;
#21695 = CARTESIAN_POINT ( 'NONE',  ( 18.01462889419880042, -7.907399074006033146, -33.36857024937042837 ) ) ;
#21696 = CARTESIAN_POINT ( 'NONE',  ( 70.03247032090600044, 18.72622661238320063, -71.50000000000139266 ) ) ;
#21697 = ORIENTED_EDGE ( 'NONE', *, *, #42017, .T. ) ;
#21698 = DIRECTION ( 'NONE',  ( 1.000000000000000000, 0.000000000000000000, 0.000000000000000000 ) ) ;
#21699 = DIRECTION ( 'NONE',  ( 0.000000000000000000, 0.000000000000000000, 1.000000000000000000 ) ) ;
#21700 = CARTESIAN_POINT ( 'NONE',  ( 19.87406119966940210, -8.717042509227168168, -35.67062074787909864 ) ) ;
#21701 = CARTESIAN_POINT ( 'NONE',  ( 14.01766645441900039, -51.16976191506400085, -22.72052346470150397 ) ) ;
#21702 = CARTESIAN_POINT ( 'NONE',  ( 56.31570272895609719, 19.43228892330789748, -75.23156124386549948 ) ) ;
#21703 = CARTESIAN_POINT ( 'NONE',  ( 47.54867620891420188, -54.45453621600920258, -74.81076251056920512 ) ) ;
#21704 = ORIENTED_EDGE ( 'NONE', *, *, #32926, .T. ) ;
#21705 = CARTESIAN_POINT ( 'NONE',  ( 55.35087876542500140, 14.59724106507499997, -16.24598606757869845 ) ) ;
#21706 = CARTESIAN_POINT ( 'NONE',  ( 16.13393739769620083, -15.61618894467929941, -32.14999999999999858 ) ) ;
#21707 = CARTESIAN_POINT ( 'NONE',  ( 57.18371625252699175, -50.61638664230610374, -53.90359199148200275 ) ) ;
#21708 = CARTESIAN_POINT ( 'NONE',  ( 52.77321279212640093, -49.72572936949169531, -48.90236189552150137 ) ) ;
#21709 = CARTESIAN_POINT ( 'NONE',  ( 12.19555056211440203, -21.23241274584290039, -31.54232391275609615 ) ) ;
#21710 = DIRECTION ( 'NONE',  ( 0.000000000000000000, 0.000000000000000000, 1.000000000000000000 ) ) ;
#21711 = CARTESIAN_POINT ( 'NONE',  ( 46.95048156581290044, 22.62954421289450124, -75.82172624862269572 ) ) ;
#21712 = CARTESIAN_POINT ( 'NONE',  ( 64.97332050699269246, 0.9209334348186318797, -60.54988453772739376 ) ) ;
#21713 = CIRCLE ( 'NONE', #31850, 1.000000000000001332 ) ;
#21714 = CARTESIAN_POINT ( 'NONE',  ( 61.09252571675981613, -45.64957244923583346, -47.71760867771691750 ) ) ;
#21715 = CARTESIAN_POINT ( 'NONE',  ( 31.58225770014178835, -2.032350560840699760, -65.65000000000000568 ) ) ;
#21716 = AXIS2_PLACEMENT_3D ( 'NONE', #40478, #4569, #15860 ) ;
#21717 = CARTESIAN_POINT ( 'NONE',  ( 28.96098294488700020, -4.556468692969050771, -34.77057949856879304 ) ) ;
#21718 = AXIS2_PLACEMENT_3D ( 'NONE', #15493, #3184, #31187 ) ;
#21719 = EDGE_CURVE ( 'NONE', #14040, #17592, #11467, .T. ) ;
#21720 = CIRCLE ( 'NONE', #41790, 0.9999999999999991118 ) ;
#21721 = CARTESIAN_POINT ( 'NONE',  ( 17.62752711509774883, -49.61617099151992250, -83.19069868277399848 ) ) ;
#21723 = ADVANCED_FACE ( 'NONE', ( #4874 ), #16665, .T. ) ;
#21722 = CARTESIAN_POINT ( 'NONE',  ( 71.60339545440879760, 0.9065823421260940096, -60.75474143511929981 ) ) ;
#21724 = CARTESIAN_POINT ( 'NONE',  ( 16.13393739769620083, -15.61618894467929941, -28.45282021618999835 ) ) ;
#21726 = CARTESIAN_POINT ( 'NONE',  ( 47.54692373198528088, -39.37158465659037887, -52.87480529148079711 ) ) ;
#21725 = PLANE ( 'NONE',  #24898 ) ;
#21727 = CIRCLE ( 'NONE', #51780, 16.00000000000000000 ) ;
#21728 = CARTESIAN_POINT ( 'NONE',  ( 61.25107916413389830, 14.01637543934619856, -46.61539294923009891 ) ) ;
#21729 = CARTESIAN_POINT ( 'NONE',  ( -12.78066350546449925, 25.79908749870000051, -53.01233286176530157 ) ) ;
#21730 = ADVANCED_FACE ( 'NONE', ( #944 ), #13272, .T. ) ;
#21731 = EDGE_LOOP ( 'NONE', ( #12930, #48854, #50171, #2116 ) ) ;
#21732 = CARTESIAN_POINT ( 'NONE',  ( 53.04305187236489871, -49.55227711057870010, -48.87083722906180583 ) ) ;
#21733 = EDGE_LOOP ( 'NONE', ( #41093, #28191, #12712, #15085 ) ) ;
#21734 = CARTESIAN_POINT ( 'NONE',  ( 47.04924918918376164, 9.060206648678184038, -51.28166297163371468 ) ) ;
#21735 = CARTESIAN_POINT ( 'NONE',  ( 50.03007040746459921, -32.48240620400619605, -78.14999999999999147 ) ) ;
#21736 = CARTESIAN_POINT ( 'NONE',  ( 57.50545812844309523, 13.88245804299080000, -25.40235374574200122 ) ) ;
#21737 = CARTESIAN_POINT ( 'NONE',  ( 14.60189429842830044, -22.50062084851940014, -41.02252027912539489 ) ) ;
#21738 = CARTESIAN_POINT ( 'NONE',  ( 28.78179405415149716, -26.60912525585749933, -34.67096478998279707 ) ) ;
#21739 = CARTESIAN_POINT ( 'NONE',  ( 52.71233980931599916, 18.50598591079160116, -48.66394846760560000 ) ) ;
#21740 = CARTESIAN_POINT ( 'NONE',  ( 64.74970223533068747, 0.9307121176571799825, -60.69545425604199806 ) ) ;
#21741 = CARTESIAN_POINT ( 'NONE',  ( 23.04647341738391830, -19.60029640582816413, -57.67433433027032663 ) ) ;
#21742 = CARTESIAN_POINT ( 'NONE',  ( 16.19514082297589042, 19.83054448556217153, -15.66998203262581413 ) ) ;
#21743 = VERTEX_POINT ( 'NONE', #33153 ) ;
#21744 = CARTESIAN_POINT ( 'NONE',  ( 21.01798797078739867, -21.24226611600790093, -77.33977848734279803 ) ) ;
#21745 = CARTESIAN_POINT ( 'NONE',  ( 73.04596072059979406, 1.186701509386330011, -68.93447492634859941 ) ) ;
#21746 = CARTESIAN_POINT ( 'NONE',  ( 47.49893771375030127, -54.58694222780890470, -54.71508793643310042 ) ) ;
#21747 = CARTESIAN_POINT ( 'NONE',  ( 16.13393739769620083, -15.61618894467929941, -32.14999999999999858 ) ) ;
#21748 = CARTESIAN_POINT ( 'NONE',  ( 73.18334309134580451, 0.9940423591679348192, -62.42346963566990325 ) ) ;
#21749 = CARTESIAN_POINT ( 'NONE',  ( 11.80006687032470047, -65.42818578075079472, -17.88619248980069898 ) ) ;
#21750 = CARTESIAN_POINT ( 'NONE',  ( 71.46077416446640029, 1.263823323415690147, -60.83883010097409993 ) ) ;
#21751 = CARTESIAN_POINT ( 'NONE',  ( 12.13079090422609418, -22.51756641863451236, -76.45982039034187494 ) ) ;
#21752 = CARTESIAN_POINT ( 'NONE',  ( 61.28610861176739633, -45.23040055550220018, -46.37203261889099792 ) ) ;
#21753 = CARTESIAN_POINT ( 'NONE',  ( 23.99010335988727860, -16.68233456288250238, -45.55063181585114762 ) ) ;
#21754 = ORIENTED_EDGE ( 'NONE', *, *, #4383, .T. ) ;
#21755 = ADVANCED_FACE ( 'NONE', ( #12480 ), #7729, .F. ) ;
#21756 = CARTESIAN_POINT ( 'NONE',  ( 64.81979753630270125, 0.8904513541338849869, -70.65165619965239330 ) ) ;
#21757 = ORIENTED_EDGE ( 'NONE', *, *, #32786, .T. ) ;
#21758 = CARTESIAN_POINT ( 'NONE',  ( 8.786694880862668811, -63.12535539208791135, -46.67160944818530766 ) ) ;
#21759 = DIRECTION ( 'NONE',  ( 0.000000000000000000, 0.000000000000000000, 1.000000000000000000 ) ) ;
#21760 = ORIENTED_EDGE ( 'NONE', *, *, #40915, .T. ) ;
#21761 = CARTESIAN_POINT ( 'NONE',  ( 66.72561048563099462, 1.883811055320649963, -20.64999999980150136 ) ) ;
#21762 = CARTESIAN_POINT ( 'NONE',  ( 9.367478339302499180, -15.61624867646989756, -69.45282021618999124 ) ) ;
#21763 = CARTESIAN_POINT ( 'NONE',  ( 22.90093700018227452, -15.31200357956842062, -50.43851515688148623 ) ) ;
#21764 = CARTESIAN_POINT ( 'NONE',  ( 51.62681371164700295, 19.13241760220180154, -76.35210453837470368 ) ) ;
#21765 = AXIS2_PLACEMENT_3D ( 'NONE', #29937, #34647, #5605 ) ;
#21766 = ORIENTED_EDGE ( 'NONE', *, *, #11184, .F. ) ;
#21767 = DIRECTION ( 'NONE',  ( -0.04251717301921600217, 0.000000000000000000, 0.9990957361526742186 ) ) ;
#21768 = AXIS2_PLACEMENT_3D ( 'NONE', #21612, #33674, #2243 ) ;
#21769 = DIRECTION ( 'NONE',  ( -0.3502816565540492477, 0.000000000000000000, 0.9366444154970182678 ) ) ;
#21770 = DIRECTION ( 'NONE',  ( 0.000000000000000000, 1.000000000000000000, 0.000000000000000000 ) ) ;
#21771 = CIRCLE ( 'NONE', #45204, 0.5000000000000004441 ) ;
#21772 = AXIS2_PLACEMENT_3D ( 'NONE', #47204, #19138, #50862 ) ;
#21773 = B_SPLINE_SURFACE_WITH_KNOTS ( 'NONE', 3, 3, ( 
 ( #8429, #15263, #31219, #4747, #40649, #48515, #20714, #24636, #12620, #28580, #549, #8684, #44580, #16535, #32487, #6679 ),
 ( #31017, #29977, #22639, #6942, #15050, #3001, #10088, #18972, #26047, #34952, #26569, #34435, #50445, #7193, #14532, #30760 ),
 ( #46000, #34166, #50952, #46265, #38657, #11129, #47042, #42058, #19235, #42322, #26836, #27097, #38911, #38384, #46782, #43101 ),
 ( #23148, #46525, #42583, #18201, #6159, #39165, #2479, #3258, #14279, #2745, #49927, #22117, #14017, #38127, #2224, #30244 ),
 ( #50185, #6421, #10351, #26310, #22379, #18462, #30502, #10614, #18716, #34693, #14792, #50695, #10871, #42845, #22894, #43863 ),
 ( #15314, #19749, #24425, #40189, #27608, #31266, #7450, #349, #43613, #36241, #48058, #40439, #51220, #19493, #44120, #35217 ),
 ( #39935, #31784, #3781, #16077, #19992, #43357, #7716, #51474, #47801, #7961, #47299, #11643, #32035, #4531, #12405, #48310 ),
 ( #4279, #11389, #20249, #11907, #35742, #51725, #44377, #15819, #12158, #3523, #27351, #35483, #16335, #31529, #23910, #28369 ),
 ( #23401, #39423, #23661, #28113, #8479, #24165, #39675, #8219, #32288, #15573, #47547, #27863, #4032, #35989, #105, #13711 ),
 ( #29665, #36754, #9266, #25469, #600, #25727, #45673, #41474, #866, #5072, #21544, #28892, #16858, #9776, #41735, #8735 ) ),
 .UNSPECIFIED., .F., .F., .F.,
 ( 4, 1, 1, 1, 1, 1, 1, 4 ),
 ( 4, 2, 2, 2, 2, 2, 2, 4 ),
 ( 0.000000000000000000, 0.1428571428571430157, 0.2857142857142860315, 0.4285714285714289917, 0.5714285714285709528, 0.7142857142857139685, 0.8571428571428569843, 1.000000000000000000 ),
 ( -5.401102999999999791E-13, 0.6760851027942610392, 1.448753791702609872, 1.931671722270319913, 2.173130687554179818, 2.549919136921820151, 3.152780655910059959, 3.863343444541179839 ),
 .UNSPECIFIED. ) ;
#21774 = CARTESIAN_POINT ( 'NONE',  ( 19.20039525651199597, -7.962460686108711272, -55.41362847326020358 ) ) ;
#21775 = B_SPLINE_CURVE_WITH_KNOTS ( 'NONE', 3,
 ( #50077, #38547, #14688, #26726, #30657, #42218, #38285, #9982, #1863, #38810, #14172, #50853, #6057, #42743, #6841, #25688, #9728, #41691 ),
 .UNSPECIFIED., .F., .F.,
 ( 4, 2, 2, 2, 2, 2, 2, 2, 4 ),
 ( 0.4999990007379375156, 0.5624991256456953748, 0.6249992505534531784, 0.6874993754612110930, 0.7499995003689690076, 0.8124996252767267002, 0.8749997501844843928, 0.9374998750922421964, 1.000000000000000000 ),
 .UNSPECIFIED. ) ;
#21776 = DIRECTION ( 'NONE',  ( 0.000000000000000000, 0.000000000000000000, -1.000000000000000000 ) ) ;
#21777 = CARTESIAN_POINT ( 'NONE',  ( 45.66390452674965417, -38.11751718055511162, -62.00015498513875656 ) ) ;
#21778 = EDGE_LOOP ( 'NONE', ( #44460, #47180, #51817, #4665 ) ) ;
#21779 = CARTESIAN_POINT ( 'NONE',  ( 57.18457261690709714, -45.84679711968900051, -26.25601685834770294 ) ) ;
#21780 = CARTESIAN_POINT ( 'NONE',  ( 18.18411367297410308, -22.77883308252629746, -40.64391951434709682 ) ) ;
#21781 = CARTESIAN_POINT ( 'NONE',  ( 52.70698372528340059, -49.76075902929100181, -48.81385732385550114 ) ) ;
#21782 = CARTESIAN_POINT ( 'NONE',  ( 9.079715832018310451, -18.09592210593110195, -32.14999999999999858 ) ) ;
#21783 = CARTESIAN_POINT ( 'NONE',  ( 14.28635823141850203, 19.91124285304359987, -74.53071772762450564 ) ) ;
#21784 = VECTOR ( 'NONE', #33956, 1000.000000000000000 ) ;
#21785 = DIRECTION ( 'NONE',  ( 0.6975711590030510001, -0.7165155114351260401, 0.000000000000000000 ) ) ;
#21786 = CARTESIAN_POINT ( 'NONE',  ( 42.17659605538639056, -45.13706293947769410, -6.213788242717720678 ) ) ;
#21787 = DIRECTION ( 'NONE',  ( 1.000000000000000000, 0.000000000000000000, 0.000000000000000000 ) ) ;
#21788 = CARTESIAN_POINT ( 'NONE',  ( 9.122356773365169147, -19.95444410747009911, -54.33130069781350358 ) ) ;
#21789 = ORIENTED_EDGE ( 'NONE', *, *, #49162, .T. ) ;
#21790 = CARTESIAN_POINT ( 'NONE',  ( 53.13843262439830539, -49.24770168678169568, -27.00111715391960132 ) ) ;
#21791 = EDGE_CURVE ( 'NONE', #48268, #33105, #18589, .T. ) ;
#21792 = CARTESIAN_POINT ( 'NONE',  ( 16.48362619534269768, -51.11256221897610175, -20.43421124880940098 ) ) ;
#21794 = CARTESIAN_POINT ( 'NONE',  ( 41.89882026671822501, -39.75356028169188249, -76.81997356724833992 ) ) ;
#21793 = CARTESIAN_POINT ( 'NONE',  ( 11.78901682358320002, 33.45032075383200265, -15.99444886826960044 ) ) ;
#21795 = CARTESIAN_POINT ( 'NONE',  ( 12.72585340994692515, -21.52904809432142486, -57.11943624023800226 ) ) ;
#21796 = CARTESIAN_POINT ( 'NONE',  ( 51.96927444999568735, 19.26340285573088806, -49.26020569436006014 ) ) ;
#21797 = EDGE_CURVE ( 'NONE', #9344, #1848, #48651, .T. ) ;
#21798 = CIRCLE ( 'NONE', #5880, 17.06999999999999673 ) ;
#21799 = EDGE_LOOP ( 'NONE', ( #34713, #9483, #9015, #5242, #32636 ) ) ;
#21800 = CARTESIAN_POINT ( 'NONE',  ( -9.512669577913570151, -43.68334388704730031, -5.840848558116729983 ) ) ;
#21801 = VECTOR ( 'NONE', #50592, 1000.000000000000000 ) ;
#21802 = CARTESIAN_POINT ( 'NONE',  ( 47.50259510985190303, 23.34628208298549978, -54.66723688595389774 ) ) ;
#21803 = CARTESIAN_POINT ( 'NONE',  ( 63.27438507250460020, 1.187296498006449985, -62.27829692513819992 ) ) ;
#21804 = CARTESIAN_POINT ( 'NONE',  ( 60.70258575398039369, 14.30887124488140039, -47.21990423911680068 ) ) ;
#21805 = TOROIDAL_SURFACE ( 'NONE', #7653, 2.500000000000000000, 0.5000000000000000000 ) ;
#21806 = CARTESIAN_POINT ( 'NONE',  ( 12.05299951489699950, 34.04022587130140209, -16.91217736884900091 ) ) ;
#21807 = CARTESIAN_POINT ( 'NONE',  ( 11.13393739768609869, -63.11566452787130288, -48.70428853817739423 ) ) ;
#21808 = CARTESIAN_POINT ( 'NONE',  ( 28.63393739769619728, -12.15208732954159920, -35.14999999999999858 ) ) ;
#21809 = CARTESIAN_POINT ( 'NONE',  ( 24.04468322966528859, -15.61618861995729013, -71.79233702014498419 ) ) ;
#21810 = CARTESIAN_POINT ( 'NONE',  ( 57.81731062816049871, -47.19213156486770089, -48.15547591032719765 ) ) ;
#21811 = CARTESIAN_POINT ( 'NONE',  ( 11.12718406860063958, 33.98029382107211660, -18.17421237808490631 ) ) ;
#21812 = CARTESIAN_POINT ( 'NONE',  ( 52.84479356091129887, 20.96976391392999872, -53.70842335541510693 ) ) ;
#21813 = CARTESIAN_POINT ( 'NONE',  ( 63.67878178145871004, 1.266076204815560047, -69.56702768459580000 ) ) ;
#21814 = DIRECTION ( 'NONE',  ( 0.000000000000000000, 1.000000000000000000, 0.000000000000000000 ) ) ;
#21815 = ORIENTED_EDGE ( 'NONE', *, *, #50717, .F. ) ;
#21816 = PLANE ( 'NONE',  #6212 ) ;
#21817 = CARTESIAN_POINT ( 'NONE',  ( 11.10549763774450049, 32.03550487100480382, -44.25138291837249227 ) ) ;
#21818 = CARTESIAN_POINT ( 'NONE',  ( 72.99206043124139853, 1.132579237369250036, -62.21177178793440277 ) ) ;
#21819 = CARTESIAN_POINT ( 'NONE',  ( 65.14565750857379101, -32.19410384129359670, -17.75424278862539751 ) ) ;
#21820 = EDGE_CURVE ( 'NONE', #40071, #37443, #11052, .T. ) ;
#21822 = B_SPLINE_CURVE_WITH_KNOTS ( 'NONE', 3,
 ( #36717, #17085, #819, #16821, #28856, #5029, #20993, #1086, #33037, #13169, #26210 ),
 .UNSPECIFIED., .F., .F.,
 ( 4, 1, 1, 1, 1, 1, 1, 1, 4 ),
 ( 0.000000000000000000, 0.02199317534151036882, 0.1012121064050618968, 0.1804310374687717322, 0.2596499685323187534, 0.3388688995958658023, 0.4180878306595756100, 0.4973067617231270998, 0.5000009373669883628 ),
 .UNSPECIFIED. ) ;
#21821 = CARTESIAN_POINT ( 'NONE',  ( 13.03996251179858845, -21.95416011689881941, -47.49173536689809794 ) ) ;
#21823 = VERTEX_POINT ( 'NONE', #36064 ) ;
#21824 = ORIENTED_EDGE ( 'NONE', *, *, #21686, .T. ) ;
#21825 = CARTESIAN_POINT ( 'NONE',  ( 52.82975622904280755, -49.66092049964720445, -28.15000000000000213 ) ) ;
#21826 = EDGE_CURVE ( 'NONE', #13022, #46863, #32107, .T. ) ;
#21827 = CARTESIAN_POINT ( 'NONE',  ( 76.44385176486125033, -6.812219962908470983, -12.98546713699449384 ) ) ;
#21828 = ORIENTED_EDGE ( 'NONE', *, *, #31597, .T. ) ;
#21829 = CARTESIAN_POINT ( 'NONE',  ( 56.35466018300130031, -46.14412721853660315, -26.19499711794230024 ) ) ;
#21830 = CARTESIAN_POINT ( 'NONE',  ( 14.34417029198830029, 17.88381105532299742, -22.49240188329279988 ) ) ;
#21831 = CARTESIAN_POINT ( 'NONE',  ( 0.08961746015897842366, -4.353854841787279106, -34.70268271585497644 ) ) ;
#21832 = DIRECTION ( 'NONE',  ( 1.000000000000000000, 0.000000000000000000, 0.000000000000000000 ) ) ;
#21833 = ORIENTED_EDGE ( 'NONE', *, *, #20677, .T. ) ;
#21834 = CARTESIAN_POINT ( 'NONE',  ( 46.46313271365296771, 6.967551557107034554, -58.00402283214241805 ) ) ;
#21835 = VERTEX_POINT ( 'NONE', #20071 ) ;
#21836 = CARTESIAN_POINT ( 'NONE',  ( 45.31002603524360239, -45.55094031840040003, -8.676032240096109405 ) ) ;
#21837 = CARTESIAN_POINT ( 'NONE',  ( 8.931659033063507280, -18.95453092549626817, -34.65421127275790525 ) ) ;
#21838 = CARTESIAN_POINT ( 'NONE',  ( 16.60579442219519919, 19.88381273878740174, -20.30246704093620025 ) ) ;
#21839 = CARTESIAN_POINT ( 'NONE',  ( 85.84022851002180232, -48.61618894467930119, -53.47585302082339354 ) ) ;
#21840 = VECTOR ( 'NONE', #25596, 1000.000000000000000 ) ;
#21841 = ORIENTED_EDGE ( 'NONE', *, *, #38165, .T. ) ;
#21842 = CARTESIAN_POINT ( 'NONE',  ( 28.13393739769620439, -18.83157925385280862, -22.14999999999998792 ) ) ;
#21843 = CARTESIAN_POINT ( 'NONE',  ( 46.94043888554279675, -54.13312419596409342, -75.65761316843601492 ) ) ;
#21844 = VECTOR ( 'NONE', #23170, 1000.000000000000114 ) ;
#21845 = CARTESIAN_POINT ( 'NONE',  ( 58.23988399474049515, 12.21801982902359995, -8.616684570808338606 ) ) ;
#21846 = AXIS2_PLACEMENT_3D ( 'NONE', #16041, #7412, #43573 ) ;
#21847 = CARTESIAN_POINT ( 'NONE',  ( 50.29495137051839748, -49.91812883465070172, -76.14999999999999147 ) ) ;
#21848 = CARTESIAN_POINT ( 'NONE',  ( 52.73680207265829978, 20.85125113597840141, -53.40499982253649591 ) ) ;
#21849 = CARTESIAN_POINT ( 'NONE',  ( 52.71259303052620027, 20.20049112655190271, -75.79898569453669666 ) ) ;
#21850 = CARTESIAN_POINT ( 'NONE',  ( 60.33389456548449914, 13.95383495194499979, -26.69150274143580148 ) ) ;
#21851 = CARTESIAN_POINT ( 'NONE',  ( 9.062045689195219467, -12.21396969154209877, -70.43023759426799302 ) ) ;
#21852 = EDGE_LOOP ( 'NONE', ( #2285, #46418, #11321, #915 ) ) ;
#21853 = DIRECTION ( 'NONE',  ( 0.000000000000000000, 1.000000000000000000, 0.000000000000000000 ) ) ;
#21854 = ADVANCED_FACE ( 'NONE', ( #1204 ), #17197, .T. ) ;
#21855 = CARTESIAN_POINT ( 'NONE',  ( -11.21045583712350080, -42.00392984997720447, -6.268887757048219989 ) ) ;
#21856 = B_SPLINE_CURVE_WITH_KNOTS ( 'NONE', 3,
 ( #19934, #24622, #3462, #31463, #35925, #35412, #15509, #11583, #51666, #15760, #16018, #11845, #27803, #43800, #47994, #12094, #8157, #24101, #40122, #4215, #20189, #49555, #5771, #45606, #790, #24880, #37480, #36962, #33009, #1580, #21216, #29851, #9704 ),
 .UNSPECIFIED., .F., .F.,
 ( 4, 2, 2, 2, 2, 2, 2, 2, 2, 2, 2, 2, 2, 1, 1, 1, 2, 4 ),
 ( 0.000000000000000000, 0.03125000081801168617, 0.06250000163602337233, 0.09375000245403505850, 0.1250000032720467447, 0.1562500040900584308, 0.1875000049080701170, 0.2500000065440936003, 0.3125000081801173057, 0.3750000098161410111, 0.4375000114521647165, 0.4687500122701767080, 0.4843750126791828148, 0.4921875128836860624, 0.4960937629859378251, 0.4980468880370637619, 0.4990234505626266470, 0.5000000130881896432 ),
 .UNSPECIFIED. ) ;
#21857 = CARTESIAN_POINT ( 'NONE',  ( 72.96823525485120854, 0.9577391936075758672, -69.20405718729148248 ) ) ;
#21858 = CARTESIAN_POINT ( 'NONE',  ( 20.99562489116508601, -21.94234663276146691, -36.08399623320025995 ) ) ;
#21859 = CARTESIAN_POINT ( 'NONE',  ( 38.10178428107396797, -15.61618894467929941, 5.729250452415290518 ) ) ;
#21860 = CARTESIAN_POINT ( 'NONE',  ( 12.53340213339009956, 19.11463212377349663, -21.18850784640499896 ) ) ;
#21861 = CARTESIAN_POINT ( 'NONE',  ( 23.13393739769620083, -2.337132753317950229, -39.64999999999999858 ) ) ;
#21862 = B_SPLINE_CURVE_WITH_KNOTS ( 'NONE', 3,
 ( #34012, #41632, #29314, #25375, #5739, #33244, #21958, #25113, #45576, #14112, #5490, #5236, #6260, #1291, #21448, #49260, #37968, #10191 ),
 .UNSPECIFIED., .F., .F.,
 ( 4, 2, 2, 2, 2, 2, 2, 2, 4 ),
 ( 0.4999984269058530550, 0.5624986235426214787, 0.6249988201793900133, 0.6874990168161585480, 0.7499992134529269716, 0.8124994100896951732, 0.8749996067264634858, 0.9374998033632317984, 1.000000000000000000 ),
 .UNSPECIFIED. ) ;
#21863 = CARTESIAN_POINT ( 'NONE',  ( 71.33393739769628894, 10.88381105532070059, -69.34999999999999432 ) ) ;
#21864 = CARTESIAN_POINT ( 'NONE',  ( 59.13340102237120277, -28.11618894467929763, -15.65754737356207116 ) ) ;
#21865 = CARTESIAN_POINT ( 'NONE',  ( 75.73925199613023551, -43.35112943081499282, -13.49699557879452172 ) ) ;
#21866 = B_SPLINE_CURVE_WITH_KNOTS ( 'NONE', 3,
 ( #24806, #5192, #1248, #49216, #17236, #20366, #16451, #40817, #5446, #4918 ),
 .UNSPECIFIED., .F., .F.,
 ( 4, 2, 2, 2, 4 ),
 ( 0.4459052190640770963, 0.5000000000194557703, 0.6250000000145918833, 0.8250000000068096195, 1.000000000000000000 ),
 .UNSPECIFIED. ) ;
#21867 = CARTESIAN_POINT ( 'NONE',  ( 57.50723796702470025, 13.88381105532070059, -17.93019253464870033 ) ) ;
#21868 = ORIENTED_EDGE ( 'NONE', *, *, #24976, .F. ) ;
#21869 = CARTESIAN_POINT ( 'NONE',  ( 22.01335404994659939, -20.19212099919920078, -59.27786220483759649 ) ) ;
#21870 = CARTESIAN_POINT ( 'NONE',  ( 63.81514305365840301, 1.404167647216139958, -61.74627665679799549 ) ) ;
#21871 = EDGE_LOOP ( 'NONE', ( #40013, #21153, #28804, #17977 ) ) ;
#21872 = CARTESIAN_POINT ( 'NONE',  ( 14.36272346516433274, -22.20707084970106138, -69.03615254816922686 ) ) ;
#21873 = CIRCLE ( 'NONE', #51200, 1.000000000000000888 ) ;
#21874 = CARTESIAN_POINT ( 'NONE',  ( 61.07186058100219839, -45.48678447307229789, -47.46853448916699847 ) ) ;
#21875 = LINE ( 'NONE', #46279, #19527 ) ;
#21876 = CARTESIAN_POINT ( 'NONE',  ( 22.52170170608374988, -20.28853306323505734, -61.70867510901859987 ) ) ;
#21878 = CARTESIAN_POINT ( 'NONE',  ( 9.807858107459463071, -10.75440064878946167, -35.00066427048108864 ) ) ;
#21877 = CARTESIAN_POINT ( 'NONE',  ( 44.34077148419982706, 8.749635085101930443, -65.00859125368401692 ) ) ;
#21879 = AXIS2_PLACEMENT_3D ( 'NONE', #36328, #48400, #12767 ) ;
#21880 = CARTESIAN_POINT ( 'NONE',  ( 9.815298770958309049, -18.40745523507650461, -81.23899999999999011 ) ) ;
#21881 = DIRECTION ( 'NONE',  ( 0.000000000000000000, 1.000000000000000000, 0.000000000000000000 ) ) ;
#21882 = EDGE_LOOP ( 'NONE', ( #38159, #29625 ) ) ;
#21883 = ORIENTED_EDGE ( 'NONE', *, *, #32834, .F. ) ;
#21884 = EDGE_CURVE ( 'NONE', #30791, #22140, #36839, .T. ) ;
#21885 = ORIENTED_EDGE ( 'NONE', *, *, #43594, .T. ) ;
#21886 = CARTESIAN_POINT ( 'NONE',  ( 61.32609621975529990, -45.21089685825819515, -46.52851239421509888 ) ) ;
#21887 = CARTESIAN_POINT ( 'NONE',  ( 61.23063308864373511, 14.32779774614108703, -47.62819202780649164 ) ) ;
#21888 = FACE_OUTER_BOUND ( 'NONE', #38992, .T. ) ;
#21889 = VERTEX_POINT ( 'NONE', #16148 ) ;
#21890 = ORIENTED_EDGE ( 'NONE', *, *, #29651, .F. ) ;
#21891 = CARTESIAN_POINT ( 'NONE',  ( 23.13393739769620083, -28.89524513604070322, -62.14999999999999858 ) ) ;
#21892 = DIRECTION ( 'NONE',  ( 0.000000000000000000, 1.000000000000000000, 0.000000000000000000 ) ) ;
#21893 = VERTEX_POINT ( 'NONE', #49181 ) ;
#21894 = CARTESIAN_POINT ( 'NONE',  ( 1.027904703268269992, 11.45423359053189927, -15.65000000000000036 ) ) ;
#21895 = CARTESIAN_POINT ( 'NONE',  ( 53.91131433518199856, -50.74962858781439934, -76.32773059544709326 ) ) ;
#21896 = CARTESIAN_POINT ( 'NONE',  ( 60.91431180673369994, 14.19281742933669932, -47.01365133320219769 ) ) ;
#21897 = CARTESIAN_POINT ( 'NONE',  ( 22.52031032320270043, -11.05537887965270016, -77.81509207372459969 ) ) ;
#21898 = CARTESIAN_POINT ( 'NONE',  ( 16.13393739769620083, -15.61618894467929941, -40.14999999999999858 ) ) ;
#21899 = CARTESIAN_POINT ( 'NONE',  ( 41.84489819291530210, 13.62916984612999904, -5.635697468575719959 ) ) ;
#21900 = CARTESIAN_POINT ( 'NONE',  ( 41.67343713632900659, -43.97793718056139767, -4.319880517921928842 ) ) ;
#21901 = CARTESIAN_POINT ( 'NONE',  ( 72.00787155028989162, 0.9860880133278648874, -61.06736746306670227 ) ) ;
#21902 = DIRECTION ( 'NONE',  ( 1.000000000000000000, 0.000000000000000000, 0.000000000000000000 ) ) ;
#21903 = TOROIDAL_SURFACE ( 'NONE', #22765, 36.50000000076989437, 1.500000000038270054 ) ;
#21904 = CARTESIAN_POINT ( 'NONE',  ( 64.56875406779060711, 1.236296663685629849, -70.35802301309989559 ) ) ;
#21905 = CARTESIAN_POINT ( 'NONE',  ( 51.13393739769659874, -50.61618894467899565, 17.35000000000000142 ) ) ;
#21906 = CARTESIAN_POINT ( 'NONE',  ( 68.11939347576729631, -0.4694106769779339827, -18.02961996124970057 ) ) ;
#21907 = ORIENTED_EDGE ( 'NONE', *, *, #48025, .T. ) ;
#21908 = CARTESIAN_POINT ( 'NONE',  ( 14.74433690757950011, -52.44145270522060542, -76.03823174343609992 ) ) ;
#21909 = EDGE_CURVE ( 'NONE', #36898, #40749, #39819, .T. ) ;
#21910 = CARTESIAN_POINT ( 'NONE',  ( 57.26283653205659618, 19.37968206195550280, -53.75815473100109898 ) ) ;
#21911 = CARTESIAN_POINT ( 'NONE',  ( 46.17042861094817852, -40.10310485825260685, -56.13152800437062240 ) ) ;
#21912 = ADVANCED_FACE ( 'NONE', ( #36311 ), #16408, .T. ) ;
#21913 = CYLINDRICAL_SURFACE ( 'NONE', #41466, 1.000000000000001332 ) ;
#21914 = ADVANCED_FACE ( 'NONE', ( #26330 ), #13594, .F. ) ;
#21915 = CARTESIAN_POINT ( 'NONE',  ( 21.64619207794780209, -11.41351007145500063, -32.14999999999999858 ) ) ;
#21916 = EDGE_CURVE ( 'NONE', #18727, #218, #5935, .T. ) ;
#21917 = CARTESIAN_POINT ( 'NONE',  ( 63.19277908840750513, 0.9325382164350239922, -69.05375146239639150 ) ) ;
#21918 = CARTESIAN_POINT ( 'NONE',  ( 47.81682817682920472, -54.40980482828490494, -54.77348380241939907 ) ) ;
#21919 = DIRECTION ( 'NONE',  ( 0.000000000000000000, -1.000000000000000000, 0.000000000000000000 ) ) ;
#21920 = CARTESIAN_POINT ( 'NONE',  ( -6.924872749483005130, -45.82389030669077812, -4.775471302137791696 ) ) ;
#21921 = CARTESIAN_POINT ( 'NONE',  ( 48.25899205962569738, 22.95127335475299901, -54.74446225849390402 ) ) ;
#21922 = ORIENTED_EDGE ( 'NONE', *, *, #40384, .F. ) ;
#21923 = CARTESIAN_POINT ( 'NONE',  ( 10.60479889110639995, -19.99468030008900143, -73.63398261789269839 ) ) ;
#21924 = EDGE_LOOP ( 'NONE', ( #30521, #36233, #38705, #8294, #4610 ) ) ;
#21925 = CARTESIAN_POINT ( 'NONE',  ( -3.866062602303800499, -15.61618894467929763, -15.18999999999999950 ) ) ;
#21926 = CARTESIAN_POINT ( 'NONE',  ( 0.3209249304026170480, -50.71887597443840434, -35.14999999999999858 ) ) ;
#21927 = CARTESIAN_POINT ( 'NONE',  ( 22.90395747212406619, -9.567216934256503436, -34.79644660940672907 ) ) ;
#21929 = LINE ( 'NONE', #33981, #14767 ) ;
#21928 = CARTESIAN_POINT ( 'NONE',  ( 84.28893459517129827, 12.67753174781119974, -47.31525200062240089 ) ) ;
#21930 = CARTESIAN_POINT ( 'NONE',  ( 22.85072513555170204, -13.46506803194099788, -76.35416353349970109 ) ) ;
#21931 = PLANE ( 'NONE',  #10447 ) ;
#21932 = CARTESIAN_POINT ( 'NONE',  ( 57.21870030722980260, -45.11618894467940066, -16.66793634595250140 ) ) ;
#21933 = CARTESIAN_POINT ( 'NONE',  ( 55.91595722987329964, -45.90465052577939531, -25.32543029193989881 ) ) ;
#21934 = CARTESIAN_POINT ( 'NONE',  ( 52.10267382257649871, -33.11618894464340457, -77.60820171200670359 ) ) ;
#21935 = EDGE_LOOP ( 'NONE', ( #11516, #48271, #2763, #4679, #2097 ) ) ;
#21936 = ADVANCED_FACE ( 'NONE', ( #9592 ), #30263, .F. ) ;
#21937 = ORIENTED_EDGE ( 'NONE', *, *, #33117, .F. ) ;
#21938 = CARTESIAN_POINT ( 'NONE',  ( 12.23212070001810048, -64.70875017051861278, -15.94047990890019939 ) ) ;
#21939 = LINE ( 'NONE', #18797, #41572 ) ;
#21940 = CYLINDRICAL_SURFACE ( 'NONE', #15128, 1.000000000000003775 ) ;
#21941 = CARTESIAN_POINT ( 'NONE',  ( 51.05234094794748501, 3.895276377383162014, -76.43087611100055767 ) ) ;
#21942 = AXIS2_PLACEMENT_3D ( 'NONE', #1548, #17536, #49004 ) ;
#21943 = ORIENTED_EDGE ( 'NONE', *, *, #17692, .T. ) ;
#21944 = VERTEX_POINT ( 'NONE', #29997 ) ;
#21945 = CARTESIAN_POINT ( 'NONE',  ( -22.85259296468129975, -13.70909830080150016, -54.73566662495469615 ) ) ;
#21946 = B_SPLINE_CURVE_WITH_KNOTS ( 'NONE', 3,
 ( #34418, #14777, #1687, #9816, #10335, #25771, #41778, #5879, #21848, #50428, #45980, #37854, #1949, #30486, #46509, #42568 ),
 .UNSPECIFIED., .F., .F.,
 ( 4, 2, 2, 2, 2, 2, 2, 4 ),
 ( 0.1347299975730832100, 1.477915555902800104, 2.688805424479379980, 3.445611592339730134, 3.918615447252459916, 4.864623157077900828, 6.378235492798619788, 7.568061678603579701 ),
 .UNSPECIFIED. ) ;
#21947 = CARTESIAN_POINT ( 'NONE',  ( 64.93393739769709327, 10.88381105532040038, -69.84999999999999432 ) ) ;
#21948 = CARTESIAN_POINT ( 'NONE',  ( 47.21678712416260026, 23.54835302331790103, -54.66856283150690388 ) ) ;
#21949 = CARTESIAN_POINT ( 'NONE',  ( 62.27287536084629949, -1.795422579115219852, -16.09831546515840017 ) ) ;
#21950 = B_SPLINE_CURVE_WITH_KNOTS ( 'NONE', 3,
 ( #4904, #24532, #20102, #706, #12515, #28481, #36093, #4637, #199, #16178, #32136, #48153, #40548 ),
 .UNSPECIFIED., .F., .F.,
 ( 4, 2, 2, 1, 2, 2, 4 ),
 ( 0.000000000000000000, 0.2500000000000104916, 0.3750000000000195399, 0.4375000000000275890, 0.4687500000000315858, 0.5000000000000356382, 1.000000000000000000 ),
 .UNSPECIFIED. ) ;
#21951 = CARTESIAN_POINT ( 'NONE',  ( 51.79789283343050244, -50.16750000966669631, -76.50613280422149387 ) ) ;
#21952 = B_SPLINE_CURVE_WITH_KNOTS ( 'NONE', 3,
 ( #12667, #23650, #852, #23901, #8470, #40690, #20495, #35977, #12397, #16576, #28620 ),
 .UNSPECIFIED., .F., .F.,
 ( 4, 1, 1, 1, 1, 1, 1, 1, 4 ),
 ( 0.000000000000000000, 0.02088113791589244622, 0.1001000689795119303, 0.1793190000431291453, 0.2585379311067463881, 0.3377568621703658791, 0.4169757932339808182, 0.4961947242976002537, 0.5000013100879009409 ),
 .UNSPECIFIED. ) ;
#21953 = CARTESIAN_POINT ( 'NONE',  ( 56.67707220608559737, -50.45813178979619806, -52.89887292284029741 ) ) ;
#21954 = ORIENTED_EDGE ( 'NONE', *, *, #24917, .T. ) ;
#21955 = CARTESIAN_POINT ( 'NONE',  ( 24.04460909154476056, -15.61619055174803172, -33.79232989763376338 ) ) ;
#21956 = CARTESIAN_POINT ( 'NONE',  ( 68.13393739769810509, 19.38381105532030091, -71.50000000000198952 ) ) ;
#21957 = ORIENTED_EDGE ( 'NONE', *, *, #30921, .F. ) ;
#21958 = CARTESIAN_POINT ( 'NONE',  ( 20.11805166124982946, -8.703655564017157786, -53.45900027236253749 ) ) ;
#21959 = DIRECTION ( 'NONE',  ( -0.7071067811864684138, -0.7071067811866267316, 0.000000000000000000 ) ) ;
#21960 = ADVANCED_FACE ( 'NONE', ( #17707 ), #33675, .F. ) ;
#21961 = CARTESIAN_POINT ( 'NONE',  ( 11.37287907419960042, -21.85470408961259636, -34.71999357511560191 ) ) ;
#21962 = CARTESIAN_POINT ( 'NONE',  ( 13.40141241860720100, -50.83865301178659735, -21.60243653193219870 ) ) ;
#21963 = CARTESIAN_POINT ( 'NONE',  ( 57.01977359311290172, 19.39593467336339927, -74.37787343998699896 ) ) ;
#21964 = CARTESIAN_POINT ( 'NONE',  ( 47.64115383555780170, -54.53453007470059788, -74.19838441418400521 ) ) ;
#21965 = ORIENTED_EDGE ( 'NONE', *, *, #20022, .T. ) ;
#21966 = CARTESIAN_POINT ( 'NONE',  ( 55.69313694499650325, 14.20859937458799926, -15.97679700106960077 ) ) ;
#21967 = CARTESIAN_POINT ( 'NONE',  ( 11.10574934303680017, 32.24869790884810072, -44.26157399421149563 ) ) ;
#21968 =( BOUNDED_CURVE ( )  B_SPLINE_CURVE ( 3, ( #15037, #47535, #11632, #22884 ),
 .UNSPECIFIED., .F., .F. ) 
 B_SPLINE_CURVE_WITH_KNOTS ( ( 4, 4 ),
 ( 1.585967333057443135E-14, 0.7853981633974705945 ),
 .UNSPECIFIED. ) 
 CURVE ( )  GEOMETRIC_REPRESENTATION_ITEM ( )  RATIONAL_B_SPLINE_CURVE ( ( 1.000000000000000000, 0.9492530216741903448, 0.9492530216741903448, 1.000000000000000000 ) ) 
 REPRESENTATION_ITEM ( '' )  );
#21969 = FACE_OUTER_BOUND ( 'NONE', #48606, .T. ) ;
#21970 = CARTESIAN_POINT ( 'NONE',  ( -21.36606260230379917, -62.11618894467930119, 16.35000000000000142 ) ) ;
#21971 = FACE_OUTER_BOUND ( 'NONE', #45235, .T. ) ;
#21972 = ORIENTED_EDGE ( 'NONE', *, *, #7344, .T. ) ;
#21973 = CARTESIAN_POINT ( 'NONE',  ( 47.46041225084670145, 23.10728982931480147, -75.12131124014999273 ) ) ;
#21974 = CARTESIAN_POINT ( 'NONE',  ( 65.25794138637670017, 1.383811055320669947, -60.91804007473620430 ) ) ;
#21975 = CARTESIAN_POINT ( 'NONE',  ( 75.27017760932777435, -35.23061375743377965, -12.38324198906882145 ) ) ;
#21976 = CARTESIAN_POINT ( 'NONE',  ( 12.94686910253266809, -65.51455027584026425, -23.34704060099317502 ) ) ;
#21977 = AXIS2_PLACEMENT_3D ( 'NONE', #34732, #42885, #46825 ) ;
#21978 = DIRECTION ( 'NONE',  ( 0.9200120562340469155, 0.3918900565005459247, 8.326672684688669123E-17 ) ) ;
#21979 = CARTESIAN_POINT ( 'NONE',  ( 68.13393739769620083, -48.61618894467930119, -65.65000000000000568 ) ) ;
#21980 = EDGE_CURVE ( 'NONE', #45554, #25535, #26715, .T. ) ;
#21981 = FACE_OUTER_BOUND ( 'NONE', #37324, .T. ) ;
#21982 = CARTESIAN_POINT ( 'NONE',  ( -21.07041245915929650, -4.022908985583359964, -53.08810431803729557 ) ) ;
#21984 = CARTESIAN_POINT ( 'NONE',  ( 43.01334310488699941, -38.96107795727259315, -75.34527945086897205 ) ) ;
#21983 = CARTESIAN_POINT ( 'NONE',  ( 45.07858682377059978, 14.88010818488339915, -9.026855431852879974 ) ) ;
#21985 = CARTESIAN_POINT ( 'NONE',  ( 61.21318727958689720, 14.03622819520689902, -46.64662901492760483 ) ) ;
#21986 = CARTESIAN_POINT ( 'NONE',  ( 23.04645919661562914, -11.63205485126550087, -69.34100441893906464 ) ) ;
#21987 = CARTESIAN_POINT ( 'NONE',  ( -0.3068767133109390199, 32.08499073367880783, -50.59628790670770115 ) ) ;
#21988 = ORIENTED_EDGE ( 'NONE', *, *, #18189, .F. ) ;
#21989 = CARTESIAN_POINT ( 'NONE',  ( 53.03884173268740199, -49.55871672378989956, -48.90887834982989801 ) ) ;
#21990 = ORIENTED_EDGE ( 'NONE', *, *, #8675, .F. ) ;
#21991 = CARTESIAN_POINT ( 'NONE',  ( 46.15168749950237270, 8.992152203351947648, -55.73704961754241083 ) ) ;
#21992 = CARTESIAN_POINT ( 'NONE',  ( 83.89200044194980421, 17.38381105532069881, -53.92796738110899923 ) ) ;
#21993 = CARTESIAN_POINT ( 'NONE',  ( 56.25705355070190450, 14.33441359163029993, -25.50876077399200170 ) ) ;
#21994 = CARTESIAN_POINT ( 'NONE',  ( 9.230581035993791872, -14.17181031012109926, -47.51847262634220215 ) ) ;
#21995 = CARTESIAN_POINT ( 'NONE',  ( 16.13393739769620083, -15.61618894467929941, -28.45282021618999835 ) ) ;
#21996 = CARTESIAN_POINT ( 'NONE',  ( 52.69140883990100122, 18.51580850568210224, -48.48983502735960371 ) ) ;
#21997 = DIRECTION ( 'NONE',  ( -1.000000000000000000, 0.000000000000000000, 0.000000000000000000 ) ) ;
#21998 = CARTESIAN_POINT ( 'NONE',  ( 9.807847332228750048, -20.47796341179069657, -58.29933495138985222 ) ) ;
#21999 = DIRECTION ( 'NONE',  ( 0.3569024281753415129, 0.000000000000000000, 0.9341416684649846980 ) ) ;
#22000 = TOROIDAL_SURFACE ( 'NONE', #42107, 38.50000000000000000, 0.5000000000000000000 ) ;
#22001 = ORIENTED_EDGE ( 'NONE', *, *, #5990, .T. ) ;
#22002 = CARTESIAN_POINT ( 'NONE',  ( 22.84307013152569965, -12.37670867548260034, -78.92415710861509126 ) ) ;
#22003 = EDGE_CURVE ( 'NONE', #44239, #32442, #26095, .T. ) ;
#22004 = CARTESIAN_POINT ( 'NONE',  ( 56.68070624494579590, 16.55316904772309883, -48.38861384420910383 ) ) ;
#22005 = FACE_BOUND ( 'NONE', #21882, .T. ) ;
#22006 = CARTESIAN_POINT ( 'NONE',  ( 72.86255183691179127, 1.369664981662529923, -62.55358821066108987 ) ) ;
#22007 = CARTESIAN_POINT ( 'NONE',  ( 11.06596496313670031, -65.18630305408680670, -17.90443099707960073 ) ) ;
#22008 = CARTESIAN_POINT ( 'NONE',  ( 52.89416328055860106, 18.39479795143689955, -48.70339646180270421 ) ) ;
#22009 = FACE_OUTER_BOUND ( 'NONE', #32191, .T. ) ;
#22010 = CARTESIAN_POINT ( 'NONE',  ( 71.44807725908989937, 0.8904513541338849869, -60.64834380034769623 ) ) ;
#22011 = CARTESIAN_POINT ( 'NONE',  ( 0.1457839871805953758, -45.96255801450852374, -34.68167748489142355 ) ) ;
#22012 = CARTESIAN_POINT ( 'NONE',  ( 64.89338513303370348, 1.264489825601020190, -70.50788383491540401 ) ) ;
#22013 = ORIENTED_EDGE ( 'NONE', *, *, #35169, .T. ) ;
#22014 = CARTESIAN_POINT ( 'NONE',  ( 8.953416032341278807, -63.13563415162649761, -46.63440066212280044 ) ) ;
#22015 = CARTESIAN_POINT ( 'NONE',  ( 52.11631747943250303, 21.39637954122449770, -46.39999999999999858 ) ) ;
#22016 = ORIENTED_EDGE ( 'NONE', *, *, #17381, .T. ) ;
#22017 = DIRECTION ( 'NONE',  ( 0.9223605572462016955, -0.3863301728269178947, 0.000000000000000000 ) ) ;
#22018 = CARTESIAN_POINT ( 'NONE',  ( 57.20288281111999851, 18.94155152855249824, -52.64687565416169690 ) ) ;
#22019 = CARTESIAN_POINT ( 'NONE',  ( 22.60131651358703664, -13.53789388470488397, -50.35393761413898517 ) ) ;
#22020 = CARTESIAN_POINT ( 'NONE',  ( 53.57534982089429576, 19.31353316830639955, -77.11818283286250164 ) ) ;
#22021 = CIRCLE ( 'NONE', #42090, 5.999999999999998224 ) ;
#22022 = VERTEX_POINT ( 'NONE', #38145 ) ;
#22023 = CONICAL_SURFACE ( 'NONE', #51335, 9.750000000000000000, 0.7853981633974476129 ) ;
#22024 = CARTESIAN_POINT ( 'NONE',  ( 10.52748815138901328, -64.93771388208423900, -47.11278009429390323 ) ) ;
#22025 = CARTESIAN_POINT ( 'NONE',  ( 23.62400244246320113, 17.52418497763099836, -35.12503119152809461 ) ) ;
#22026 = CARTESIAN_POINT ( 'NONE',  ( 24.04487538420616843, -15.58383734352081440, -43.79102361582464198 ) ) ;
#22027 = EDGE_CURVE ( 'NONE', #12957, #50005, #34455, .T. ) ;
#22028 = CARTESIAN_POINT ( 'NONE',  ( 21.10308478659139908, -22.19572496809090367, -52.08643336858809647 ) ) ;
#22029 = EDGE_CURVE ( 'NONE', #36517, #42919, #39519, .T. ) ;
#22030 = DIRECTION ( 'NONE',  ( 0.000000000000000000, 0.000000000000000000, -1.000000000000000000 ) ) ;
#22031 = CARTESIAN_POINT ( 'NONE',  ( 45.79168803806123123, -38.13146365633215140, -61.36124641343345587 ) ) ;
#22032 = EDGE_CURVE ( 'NONE', #11240, #51433, #49946, .T. ) ;
#22033 = ORIENTED_EDGE ( 'NONE', *, *, #24618, .T. ) ;
#22034 = CARTESIAN_POINT ( 'NONE',  ( 56.77510575719860242, -46.03395327836230422, -26.24796325860310020 ) ) ;
#22035 = CARTESIAN_POINT ( 'NONE',  ( 20.50180696762360100, -9.580593760668989489, -47.93206117220019991 ) ) ;
#22036 = CARTESIAN_POINT ( 'NONE',  ( 10.79172117177870049, -11.23010277562130099, -32.14999999999999858 ) ) ;
#22037 = CARTESIAN_POINT ( 'NONE',  ( 13.85739208368369901, 20.19843276291189937, -74.93307507168100301 ) ) ;
#22038 = CARTESIAN_POINT ( 'NONE',  ( 17.16956853822826901, -7.705200890051467688, -51.33399677538780992 ) ) ;
#22039 = ADVANCED_FACE ( 'NONE', ( #18219 ), #20910, .T. ) ;
#22040 = DIRECTION ( 'NONE',  ( 0.1961161351381840445, -2.713878504639270283E-16, 0.9805806756909201116 ) ) ;
#22041 = CARTESIAN_POINT ( 'NONE',  ( 8.856000844739879696, -19.49102574641920071, -60.35193945864850207 ) ) ;
#22042 = ADVANCED_FACE ( 'NONE', ( #19461 ), #10840, .F. ) ;
#22043 = VERTEX_POINT ( 'NONE', #34662 ) ;
#22044 = CARTESIAN_POINT ( 'NONE',  ( 53.45178337541119618, -48.93644626688359978, -26.86578694399930001 ) ) ;
#22045 = CARTESIAN_POINT ( 'NONE',  ( 54.04287499173630493, -51.09449692274579746, -75.65863628419570830 ) ) ;
#22047 = CARTESIAN_POINT ( 'NONE',  ( 42.22239453466733750, -39.78826103684639293, -75.25768512366673235 ) ) ;
#22046 = CARTESIAN_POINT ( 'NONE',  ( 12.12058638835210012, 33.31847000525309710, -15.78474273040839826 ) ) ;
#22048 = CARTESIAN_POINT ( 'NONE',  ( 22.90099491887654182, -15.61618908163285546, -52.84717737022585027 ) ) ;
#22049 = CARTESIAN_POINT ( 'NONE',  ( 13.19564766795559940, 10.36739510386719942, -74.14999999999999147 ) ) ;
#22050 = AXIS2_PLACEMENT_3D ( 'NONE', #51023, #15124, #31082 ) ;
#22051 = ORIENTED_EDGE ( 'NONE', *, *, #6269, .F. ) ;
#22052 = CARTESIAN_POINT ( 'NONE',  ( -2.629620173063649702, -48.67441424446350595, -4.565428259182719550 ) ) ;
#22053 = TOROIDAL_SURFACE ( 'NONE', #39658, 9.000000000000000000, 1.000000000000000000 ) ;
#22054 = CARTESIAN_POINT ( 'NONE',  ( 47.57599655811520023, 23.29777716724849768, -54.66624935529340235 ) ) ;
#22055 = CARTESIAN_POINT ( 'NONE',  ( 22.06776932978649697, -10.30416640759050928, -65.56010685651600056 ) ) ;
#22056 = CARTESIAN_POINT ( 'NONE',  ( 63.19468704395299596, 0.8986939045430379913, -62.24348040161360274 ) ) ;
#22057 = CARTESIAN_POINT ( 'NONE',  ( 13.13594234983320064, 19.37673283217589670, -21.36925545734460030 ) ) ;
#22058 = CARTESIAN_POINT ( 'NONE',  ( 56.79283174838518278, 14.01333454635517484, -25.29533692629807362 ) ) ;
#22059 = CARTESIAN_POINT ( 'NONE',  ( 11.94685995288999969, 34.08567592416299874, -17.08231285071160244 ) ) ;
#22060 = CARTESIAN_POINT ( 'NONE',  ( 52.26505149639940129, 18.55116626494530152, -77.19463936772390866 ) ) ;
#22061 = DIRECTION ( 'NONE',  ( -0.7071067811865475727, 0.000000000000000000, 0.7071067811865475727 ) ) ;
#22062 = DIRECTION ( 'NONE',  ( 0.000000000000000000, 0.000000000000000000, -1.000000000000000000 ) ) ;
#22063 = CARTESIAN_POINT ( 'NONE',  ( 53.59226879027059454, -49.40789622861730379, -49.22934975137650326 ) ) ;
#22064 = CARTESIAN_POINT ( 'NONE',  ( 54.49383788419760322, 16.89893908078170170, -26.73738845760439986 ) ) ;
#22065 = CARTESIAN_POINT ( 'NONE',  ( 55.56556980353779807, 19.70710272740160107, -53.05958889729620154 ) ) ;
#22066 = APPLICATION_CONTEXT ( 'automotive_design' ) ;
#22067 = CARTESIAN_POINT ( 'NONE',  ( 63.45871665573360332, 1.367045641526529964, -68.91833781196129394 ) ) ;
#22068 = CYLINDRICAL_SURFACE ( 'NONE', #42859, 2.000000000000000888 ) ;
#22069 = CARTESIAN_POINT ( 'NONE',  ( 17.98749078828957337, 10.53025766472752522, -34.79644660940672907 ) ) ;
#22070 = CARTESIAN_POINT ( 'NONE',  ( 19.44385660017238138, 22.20530810434653546, -16.61545052194239247 ) ) ;
#22071 = CARTESIAN_POINT ( 'NONE',  ( 10.97782414026809938, 31.90204039037219985, -44.74265096482220372 ) ) ;
#22072 = CARTESIAN_POINT ( 'NONE',  ( 17.07108633743450099, 19.88381105532299742, -15.67606611410359996 ) ) ;
#22073 = CARTESIAN_POINT ( 'NONE',  ( 65.61835811606158586, -31.74415475557530186, -17.32553893461689754 ) ) ;
#22074 = CARTESIAN_POINT ( 'NONE',  ( 17.99230109774930142, 19.88380302201240113, -74.34036667011370980 ) ) ;
#22075 = VERTEX_POINT ( 'NONE', #23628 ) ;
#22076 = EDGE_LOOP ( 'NONE', ( #49227, #40312, #43017, #6504, #16290 ) ) ;
#22077 = AXIS2_PLACEMENT_3D ( 'NONE', #13502, #8523, #16907 ) ;
#22078 = CARTESIAN_POINT ( 'NONE',  ( 18.20470610557513069, -23.32126384531657237, -79.92433626156834237 ) ) ;
#22079 = CARTESIAN_POINT ( 'NONE',  ( 50.98083915167267577, 0.1184463107911828128, -16.83642266816315214 ) ) ;
#22080 = ORIENTED_EDGE ( 'NONE', *, *, #30464, .F. ) ;
#22081 = CARTESIAN_POINT ( 'NONE',  ( 11.12442287039499966, -63.87901563523511328, -44.48448433309780370 ) ) ;
#22082 = CARTESIAN_POINT ( 'NONE',  ( 57.53167045908470101, -45.29965578464429399, -25.93059424638790134 ) ) ;
#22083 = FACE_OUTER_BOUND ( 'NONE', #38352, .T. ) ;
#22084 = CARTESIAN_POINT ( 'NONE',  ( 18.20467351747694096, -7.911104839119652787, -63.09100278528516270 ) ) ;
#22085 = DIRECTION ( 'NONE',  ( 0.000000000000000000, 0.000000000000000000, 1.000000000000000000 ) ) ;
#22086 = ORIENTED_EDGE ( 'NONE', *, *, #20808, .T. ) ;
#22087 = DIRECTION ( 'NONE',  ( 0.000000000000000000, 0.000000000000000000, -1.000000000000000000 ) ) ;
#22088 = CARTESIAN_POINT ( 'NONE',  ( 45.78920227927463316, 6.898993018891284024, -61.37367372640163410 ) ) ;
#22089 = ORIENTED_EDGE ( 'NONE', *, *, #12053, .F. ) ;
#22090 = CARTESIAN_POINT ( 'NONE',  ( 48.02062614174979416, -45.57114167671549865, -10.53674581177119940 ) ) ;
#22091 = ADVANCED_FACE ( 'NONE', ( #47517 ), #38560, .T. ) ;
#22092 = CARTESIAN_POINT ( 'NONE',  ( 24.00136113245211789, -16.46404240851678580, -33.82649071835572130 ) ) ;
#22093 = CIRCLE ( 'NONE', #16305, 1.999999999999997113 ) ;
#22094 = CARTESIAN_POINT ( 'NONE',  ( 15.12151582312089992, 19.77629001565449940, -21.37863257646460013 ) ) ;
#22095 = LINE ( 'NONE', #21839, #5921 ) ;
#22096 = EDGE_CURVE ( 'NONE', #27414, #8004, #27787, .T. ) ;
#22097 = AXIS2_PLACEMENT_3D ( 'NONE', #44176, #8797, #16927 ) ;
#22098 = CARTESIAN_POINT ( 'NONE',  ( -35.14957091781822385, 3.655592887048059403, -65.33131157870826655 ) ) ;
#22099 = CARTESIAN_POINT ( 'NONE',  ( 47.07821196700830058, -54.56982298144170329, -75.12266286288350159 ) ) ;
#22100 = CARTESIAN_POINT ( 'NONE',  ( 61.79285179583219900, 13.10481322255020054, -9.877340765310581361 ) ) ;
#22101 = CARTESIAN_POINT ( 'NONE',  ( 50.67690155642070238, -50.61106055578139973, -76.14999999999999147 ) ) ;
#22102 = CARTESIAN_POINT ( 'NONE',  ( 22.37318698975080267, 22.37488585622680048, -34.64999999999999858 ) ) ;
#22103 = CARTESIAN_POINT ( 'NONE',  ( 51.04849474376590024, 19.66358989377309996, -76.15025768601358891 ) ) ;
#22104 = CARTESIAN_POINT ( 'NONE',  ( 59.29192855637670334, 13.93150092321869948, -26.12720780484039906 ) ) ;
#22105 = CARTESIAN_POINT ( 'NONE',  ( 18.31782017144560015, -23.15392097850119768, -71.69774049128601234 ) ) ;
#22106 = EDGE_CURVE ( 'NONE', #7516, #31721, #25308, .T. ) ;
#22107 = EDGE_LOOP ( 'NONE', ( #383, #10893, #30821, #26731, #30309, #24443, #29713, #43273, #35505, #10773, #28649, #25291, #6966, #395, #2246, #2899 ) ) ;
#22108 = PLANE ( 'NONE',  #50657 ) ;
#22109 = CIRCLE ( 'NONE', #43904, 30.50439988982899564 ) ;
#22110 = CARTESIAN_POINT ( 'NONE',  ( -11.07245470237450036, -42.11047228534719977, -5.947362040326959587 ) ) ;
#22111 = ADVANCED_FACE ( 'NONE', ( #31747 ), #4410, .T. ) ;
#22112 = CARTESIAN_POINT ( 'NONE',  ( 72.65628610108569774, 1.412203896155640015, -69.03044017489760620 ) ) ;
#22113 = CARTESIAN_POINT ( 'NONE',  ( 17.07108737582920455, -51.11618894467930119, -15.67606610107699971 ) ) ;
#22114 = PLANE ( 'NONE',  #18132 ) ;
#22115 = CARTESIAN_POINT ( 'NONE',  ( 24.03895263636016111, -15.10140185694807968, -65.48698662191623043 ) ) ;
#22116 = AXIS2_PLACEMENT_3D ( 'NONE', #37404, #29269, #45272 ) ;
#22117 = CARTESIAN_POINT ( 'NONE',  ( 41.26036483009979605, 12.97521128452129879, -4.192607600171130322 ) ) ;
#22118 = CARTESIAN_POINT ( 'NONE',  ( 18.20455775428947831, -7.911072023573607837, -59.37571045720464724 ) ) ;
#22119 = CARTESIAN_POINT ( 'NONE',  ( 19.93042471013020034, 24.20303158999493576, -75.02879301527407563 ) ) ;
#22120 = CARTESIAN_POINT ( 'NONE',  ( 16.13393739769620083, -1.182432214938700099, -34.64999999999999858 ) ) ;
#22121 = AXIS2_PLACEMENT_3D ( 'NONE', #44164, #29199, #8527 ) ;
#22122 = CARTESIAN_POINT ( 'NONE',  ( 22.89142744636506421, -16.00358783246685945, -62.47105660056999454 ) ) ;
#22123 = CARTESIAN_POINT ( 'NONE',  ( 18.72308090817790216, -51.82694627962250422, -74.93568190818520236 ) ) ;
#22124 = DIRECTION ( 'NONE',  ( 1.000000000000000000, 0.000000000000000000, 0.000000000000000000 ) ) ;
#22125 = ORIENTED_EDGE ( 'NONE', *, *, #41450, .F. ) ;
#22126 = AXIS2_PLACEMENT_3D ( 'NONE', #50902, #3209, #34639 ) ;
#22127 = CARTESIAN_POINT ( 'NONE',  ( 22.29748881350769807, -19.80155969086050050, -53.25722344400249852 ) ) ;
#22128 = CARTESIAN_POINT ( 'NONE',  ( 63.91114391772079273, 1.454949836291180132, -61.73964252679819964 ) ) ;
#22129 = EDGE_LOOP ( 'NONE', ( #22775, #33491, #5534, #46223 ) ) ;
#22130 = CARTESIAN_POINT ( 'NONE',  ( -0.1295185695942999982, 0.6472670226113349523, -59.64999999999999147 ) ) ;
#22131 = CARTESIAN_POINT ( 'NONE',  ( 60.79255070202940203, -45.73115554882360101, -47.75226182717869960 ) ) ;
#22132 = CARTESIAN_POINT ( 'NONE',  ( 22.59648755964504829, -13.01690795190288519, -74.72494365400706329 ) ) ;
#22133 = CARTESIAN_POINT ( 'NONE',  ( 24.04493739453105761, -15.62695325930471490, -61.50809781073701288 ) ) ;
#22135 = CARTESIAN_POINT ( 'NONE',  ( 22.73379249883699060, -13.53922887446369572, -54.74949983865565173 ) ) ;
#22134 = CARTESIAN_POINT ( 'NONE',  ( 44.44582319305163054, 8.758006262679185028, -64.49853979666923465 ) ) ;
#22136 = CARTESIAN_POINT ( 'NONE',  ( 75.13393739769618662, 1.883811055320649963, -84.38499399519520239 ) ) ;
#22137 = CARTESIAN_POINT ( 'NONE',  ( 60.83133137330749918, -45.46867109277970087, -47.01992810568810199 ) ) ;
#22138 = ORIENTED_EDGE ( 'NONE', *, *, #15800, .F. ) ;
#22139 = VERTEX_POINT ( 'NONE', #27833 ) ;
#22140 = VERTEX_POINT ( 'NONE', #4768 ) ;
#22141 = CARTESIAN_POINT ( 'NONE',  ( -22.73139975955365344, -18.77686687743244320, -54.68857781686908481 ) ) ;
#22142 = DIRECTION ( 'NONE',  ( 0.000000000000000000, 0.000000000000000000, 1.000000000000000000 ) ) ;
#22143 = ORIENTED_EDGE ( 'NONE', *, *, #9571, .F. ) ;
#22144 = ORIENTED_EDGE ( 'NONE', *, *, #5872, .T. ) ;
#22145 = CARTESIAN_POINT ( 'NONE',  ( 24.03886748631395776, -15.28162044291991961, -77.49421311239169086 ) ) ;
#22146 = CIRCLE ( 'NONE', #40562, 6.000000000000000000 ) ;
#22147 = EDGE_CURVE ( 'NONE', #24962, #36035, #39084, .T. ) ;
#22148 = DIRECTION ( 'NONE',  ( -1.000000000000000000, 0.000000000000000000, 0.000000000000000000 ) ) ;
#22149 = CARTESIAN_POINT ( 'NONE',  ( 18.63393739769599833, 14.38381105532070059, -34.64999999999999858 ) ) ;
#22150 = EDGE_LOOP ( 'NONE', ( #21943, #40327 ) ) ;
#22151 = LINE ( 'NONE', #1741, #6597 ) ;
#22152 = CARTESIAN_POINT ( 'NONE',  ( 53.80071036277350061, -50.68582778161849234, -76.57022530412510264 ) ) ;
#22153 = CARTESIAN_POINT ( 'NONE',  ( 60.59756557471860106, 14.41685909332530002, -47.48166371871570846 ) ) ;
#22154 = CARTESIAN_POINT ( 'NONE',  ( 18.19207604292220282, -8.043156995148798671, -75.59696200394320442 ) ) ;
#22155 = DIRECTION ( 'NONE',  ( 0.000000000000000000, 0.000000000000000000, -1.000000000000000000 ) ) ;
#22156 = CARTESIAN_POINT ( 'NONE',  ( 45.96729298300089539, 13.88381088409749964, -7.679810999631830448 ) ) ;
#22157 = AXIS2_PLACEMENT_3D ( 'NONE', #30556, #14588, #33964 ) ;
#22158 = CARTESIAN_POINT ( 'NONE',  ( 41.13550660981270113, -44.31231073639379758, -4.257233742966690215 ) ) ;
#22159 = CARTESIAN_POINT ( 'NONE',  ( 14.34417029198879945, -51.11618894467930119, -76.14999999999999147 ) ) ;
#22160 = CARTESIAN_POINT ( 'NONE',  ( -10.87689599130639984, 11.12029513569609840, -6.286428452389710486 ) ) ;
#22162 = AXIS2_PLACEMENT_3D ( 'NONE', #9329, #10357, #45741 ) ;
#22161 = CARTESIAN_POINT ( 'NONE',  ( 64.59295435006930575, 1.031625743333890011, -70.48352829009921550 ) ) ;
#22163 = CARTESIAN_POINT ( 'NONE',  ( 46.63357160382179956, 8.689668561411270531, -54.59574113304929455 ) ) ;
#22164 = CARTESIAN_POINT ( 'NONE',  ( 12.91854708852281597, -3.616188944679342931, -22.15000000000000924 ) ) ;
#22165 = EDGE_CURVE ( 'NONE', #49956, #29481, #15281, .T. ) ;
#22166 = EDGE_LOOP ( 'NONE', ( #42813, #20152, #42893, #2567 ) ) ;
#22167 = FILL_AREA_STYLE_COLOUR ( '', #31319 ) ;
#22168 = CYLINDRICAL_SURFACE ( 'NONE', #44481, 4.649999999999999467 ) ;
#22169 = EDGE_CURVE ( 'NONE', #9734, #21743, #21592, .T. ) ;
#22170 = CARTESIAN_POINT ( 'NONE',  ( 61.28085240419530066, -45.60177449860450594, -47.67834116410560341 ) ) ;
#22171 = CARTESIAN_POINT ( 'NONE',  ( 8.222937397696192363, -15.61618894467929941, -81.23899999999999011 ) ) ;
#22172 = CARTESIAN_POINT ( 'NONE',  ( 20.83772691662250054, -10.64658677815640075, -32.14999999999999858 ) ) ;
#22173 = CARTESIAN_POINT ( 'NONE',  ( 63.47152504824990160, 1.384378348444520013, -68.73316704115080711 ) ) ;
#22174 = CARTESIAN_POINT ( 'NONE',  ( 48.07362292129520398, -54.31422102361820237, -54.91777794127389711 ) ) ;
#22175 = CONICAL_SURFACE ( 'NONE', #4609, 12.92820323027549989, 0.7481802937784480800 ) ;
#22176 = DIRECTION ( 'NONE',  ( 0.000000000000000000, 0.000000000000000000, -1.000000000000000000 ) ) ;
#22177 = CARTESIAN_POINT ( 'NONE',  ( -9.120882960378676074, -44.01580188157885232, -5.427931971034974268 ) ) ;
#22178 = CARTESIAN_POINT ( 'NONE',  ( 11.27220150064897553, -21.94231036716944061, -46.50070531515176953 ) ) ;
#22179 = CARTESIAN_POINT ( 'NONE',  ( 48.17397874823690529, 23.07566552192859888, -55.30238548989590441 ) ) ;
#22180 = ORIENTED_EDGE ( 'NONE', *, *, #11062, .T. ) ;
#22181 = CARTESIAN_POINT ( 'NONE',  ( 11.51802410812859989, -20.94872152101149965, -71.57429041023839034 ) ) ;
#22182 = EDGE_LOOP ( 'NONE', ( #40236, #20638, #26601, #18292 ) ) ;
#22183 = CARTESIAN_POINT ( 'NONE',  ( 71.40678801050209756, 1.186856010528209993, -70.56885973566780024 ) ) ;
#22184 = CARTESIAN_POINT ( 'NONE',  ( 16.13393739769620083, -15.61618894467929941, 17.07360679774999923 ) ) ;
#22185 = CARTESIAN_POINT ( 'NONE',  ( 83.87141997196457055, 13.62662327952309127, -47.47133103277113264 ) ) ;
#22186 = DIRECTION ( 'NONE',  ( -0.8340645993220436871, 0.5516667872527389882, 0.000000000000000000 ) ) ;
#22188 = CARTESIAN_POINT ( 'NONE',  ( 52.63503755353740132, 18.55503091818710004, -27.72364810048630090 ) ) ;
#22187 = CARTESIAN_POINT ( 'NONE',  ( 84.39650841167410533, 12.26252976892699920, -47.35795223498069362 ) ) ;
#22189 = CARTESIAN_POINT ( 'NONE',  ( 9.251438566469660785, -14.07548506148300049, -79.52292077604440124 ) ) ;
#22190 = FACE_OUTER_BOUND ( 'NONE', #12977, .T. ) ;
#22191 = CARTESIAN_POINT ( 'NONE',  ( 71.45588032111149346, 0.8910129994591539093, -70.64647704525299332 ) ) ;
#22192 = CARTESIAN_POINT ( 'NONE',  ( 17.01966294822905112, -22.38319941436395411, -40.91109367937480812 ) ) ;
#22193 = B_SPLINE_SURFACE_WITH_KNOTS ( 'NONE', 3, 3, ( 
 ( #36103, #3634, #39786, #20110, #15429, #31895, #47911, #39272, #27203 ),
 ( #12015, #206, #15169, #19606, #27968, #19087, #43972, #31126, #11241 ),
 ( #43214, #3377, #24021, #35596, #48163, #43720, #12265, #19349, #7820 ),
 ( #44227, #3120, #35064, #9381, #1245, #48690, #16981, #981, #1502 ),
 ( #13562, #25324, #8328, #45268, #12792, #9110, #32928, #44490, #28748 ),
 ( #44747, #48956, #24281, #45007, #41327, #29011, #8853, #25059, #17487 ),
 ( #17233, #28489, #8593, #24802, #41076, #5189, #13059, #21140, #33451 ),
 ( #36348, #33194, #40814, #37147, #49213, #49471, #13306, #29525, #5442 ),
 ( #21399, #4913, #29266, #37400, #24537, #20886, #40555, #36881, #40301 ),
 ( #4392, #20361, #460, #16446, #32400, #48422, #4645, #12522, #20620 ),
 ( #36608, #714, #16704, #32659, #30295, #38706, #42633, #21649, #49724 ),
 ( #50746, #50492, #17739, #30548, #6730, #46573, #2013, #41847, #2794 ),
 ( #33708, #10140, #21908, #5696, #26618, #10401, #14323, #46312, #18767 ),
 ( #2272, #14582, #22686, #34739, #34487, #49975, #14842, #45788, #25581 ),
 ( #45529, #9624, #41586, #10661, #18246, #37654, #13812, #1753, #29770 ),
 ( #9878, #25834, #5950, #18513, #37919, #17994, #33960, #14068, #30030 ) ),
 .UNSPECIFIED., .F., .F., .F.,
 ( 4, 2, 2, 2, 2, 2, 2, 4 ),
 ( 4, 1, 1, 1, 1, 1, 4 ),
 ( -3.203522274500000355E-05, 0.2957445120220140167, 0.5890486225480849880, 0.7853981633974459475, 0.8835729338221269824, 1.040652566501619969, 1.291979978788799999, 1.570796326794889897 ),
 ( -3.203522271700000133E-05, 0.1666666666666670182, 0.3333333333333329818, 0.5000000000000000000, 0.6666666666666670737, 0.8333333333333330373, 1.000032035222700122 ),
 .UNSPECIFIED. ) ;
#22194 = VERTEX_POINT ( 'NONE', #49837 ) ;
#22195 = DIRECTION ( 'NONE',  ( 0.000000000000000000, -1.000000000000000000, 0.000000000000000000 ) ) ;
#22196 = VECTOR ( 'NONE', #39468, 1000.000000000000000 ) ;
#22197 = ORIENTED_EDGE ( 'NONE', *, *, #5561, .T. ) ;
#22198 = ORIENTED_EDGE ( 'NONE', *, *, #13641, .F. ) ;
#22199 = CARTESIAN_POINT ( 'NONE',  ( 12.10858429747099940, -64.84551244548728732, -16.12611387919940142 ) ) ;
#22200 = LINE ( 'NONE', #25358, #3953 ) ;
#22201 = CARTESIAN_POINT ( 'NONE',  ( -33.86606260230286125, -15.61618894467806484, -57.75434458024869855 ) ) ;
#22202 = CARTESIAN_POINT ( 'NONE',  ( 51.10510889049552219, 3.800546900492662417, -76.46299428730267778 ) ) ;
#22203 = ORIENTED_EDGE ( 'NONE', *, *, #4916, .T. ) ;
#22204 = ORIENTED_EDGE ( 'NONE', *, *, #47452, .F. ) ;
#22205 = CARTESIAN_POINT ( 'NONE',  ( -1.572464511459390035, -50.27926404661009485, -36.17267532414179954 ) ) ;
#22206 = FACE_OUTER_BOUND ( 'NONE', #48018, .T. ) ;
#22207 = EDGE_CURVE ( 'NONE', #24877, #29876, #17603, .T. ) ;
#22208 = CARTESIAN_POINT ( 'NONE',  ( 52.75874701511860110, 18.42236751908479775, -48.21692926115490252 ) ) ;
#22209 = CARTESIAN_POINT ( 'NONE',  ( 64.96436114686899543, -1.516193279748339950, -16.48292108836169945 ) ) ;
#22210 = CARTESIAN_POINT ( 'NONE',  ( 51.30775034956070613, -48.70729205768719794, -76.60305689054860068 ) ) ;
#22211 = EDGE_CURVE ( 'NONE', #20803, #46160, #7755, .T. ) ;
#22212 = CARTESIAN_POINT ( 'NONE',  ( 60.83826515012160030, -46.13970514846629811, -48.26656313140399845 ) ) ;
#22213 = ORIENTED_EDGE ( 'NONE', *, *, #8979, .T. ) ;
#22214 = ADVANCED_FACE ( 'NONE', ( #21251 ), #50440, .T. ) ;
#22215 = CARTESIAN_POINT ( 'NONE',  ( 52.67941827447170056, -49.73994065207379123, -27.56303321415330032 ) ) ;
#22216 = CARTESIAN_POINT ( 'NONE',  ( 68.13393739769706769, 17.98087126524489321, -74.20351669811762463 ) ) ;
#22217 = ORIENTED_EDGE ( 'NONE', *, *, #51277, .T. ) ;
#22218 = DIRECTION ( 'NONE',  ( 1.000000000000000000, 0.000000000000000000, 0.000000000000000000 ) ) ;
#22219 = CARTESIAN_POINT ( 'NONE',  ( 23.83903760508270864, -17.68686475598193297, -53.59100462632350315 ) ) ;
#22220 = VECTOR ( 'NONE', #19089, 1000.000000000000000 ) ;
#22221 = CARTESIAN_POINT ( 'NONE',  ( 23.98092394894220192, -15.50871961813850142, -42.00813523296849894 ) ) ;
#22222 = AXIS2_PLACEMENT_3D ( 'NONE', #37407, #24546, #9631 ) ;
#22223 = CARTESIAN_POINT ( 'NONE',  ( 14.07747898808480080, -51.04610731982879912, -22.00391413710600119 ) ) ;
#22224 = CARTESIAN_POINT ( 'NONE',  ( 55.57043806660909979, 19.45794959307779592, -75.70375535085590002 ) ) ;
#22225 = CARTESIAN_POINT ( 'NONE',  ( 47.36202133841670303, -54.21176582509019681, -75.36157798374209449 ) ) ;
#22226 = CARTESIAN_POINT ( 'NONE',  ( 54.89464421352140278, 14.83598063949260037, -15.98485522678499926 ) ) ;
#22227 = CARTESIAN_POINT ( 'NONE',  ( 47.67821675608059451, 23.28668618819479619, -55.12141599180650076 ) ) ;
#22228 = CARTESIAN_POINT ( 'NONE',  ( 56.52293937326459883, -50.63229154223470374, -53.14906066081460523 ) ) ;
#22229 = ADVANCED_FACE ( 'NONE', ( #37780 ), #29384, .T. ) ;
#22230 = CARTESIAN_POINT ( 'NONE',  ( 15.57679709041789984, -22.64698931536659998, -43.37235095159000053 ) ) ;
#22231 = DIRECTION ( 'NONE',  ( 0.3294064756440925335, -0.9441882088883222224, -3.330669073875471100E-16 ) ) ;
#22232 = ORIENTED_EDGE ( 'NONE', *, *, #3663, .T. ) ;
#22233 = CARTESIAN_POINT ( 'NONE',  ( 47.54872616799120522, 23.22222337448880225, -74.81054825214430082 ) ) ;
#22234 = CARTESIAN_POINT ( 'NONE',  ( 65.00022493107950083, 0.9952464559119579279, -60.54306244337860221 ) ) ;
#22235 = EDGE_CURVE ( 'NONE', #26382, #36140, #37442, .T. ) ;
#22236 = CYLINDRICAL_SURFACE ( 'NONE', #14681, 6.766999999999998572 ) ;
#22237 = CARTESIAN_POINT ( 'NONE',  ( 12.40751055747876919, -65.38681240857033572, -23.57252729928288915 ) ) ;
#22238 = CARTESIAN_POINT ( 'NONE',  ( 59.13340102237120277, -15.61618894467929941, -15.65754737356207116 ) ) ;
#22239 = DIRECTION ( 'NONE',  ( -1.000000000000000000, -7.683667316014053881E-33, 8.592609827796581962E-15 ) ) ;
#22240 = CIRCLE ( 'NONE', #14709, 25.00000000000000000 ) ;
#22241 = CARTESIAN_POINT ( 'NONE',  ( 82.13853704237929776, 14.41284512186622102, -47.72712807259519963 ) ) ;
#22243 = CARTESIAN_POINT ( 'NONE',  ( 41.86472757144029799, -37.59316321825600227, -80.99597773300310166 ) ) ;
#22242 = CARTESIAN_POINT ( 'NONE',  ( 7.853097003783789276, 29.28805065900050053, -20.86915960608759946 ) ) ;
#22244 = DIRECTION ( 'NONE',  ( 0.000000000000000000, -0.7071067811865492381, 0.7071067811865457964 ) ) ;
#22245 = CARTESIAN_POINT ( 'NONE',  ( 12.77400604982229915, 32.54918712825639915, -45.78449089158890217 ) ) ;
#22246 = VERTEX_POINT ( 'NONE', #41700 ) ;
#22247 = CARTESIAN_POINT ( 'NONE',  ( 53.00021633606750271, -49.57817710704839698, -48.89297489742170200 ) ) ;
#22248 = ORIENTED_EDGE ( 'NONE', *, *, #33265, .T. ) ;
#22249 = EDGE_CURVE ( 'NONE', #12167, #51433, #40362, .T. ) ;
#22250 = CARTESIAN_POINT ( 'NONE',  ( 17.54621496640162448, 20.94681317766335127, -75.92929758211226954 ) ) ;
#22251 = CIRCLE ( 'NONE', #32265, 0.5000000000000004441 ) ;
#22252 = CARTESIAN_POINT ( 'NONE',  ( 14.06335507478330449, -23.32131402515702234, -74.37566484649038046 ) ) ;
#22253 = CARTESIAN_POINT ( 'NONE',  ( 13.93865262801319993, 19.96876084912479854, -22.80126943285790020 ) ) ;
#22254 = CARTESIAN_POINT ( 'NONE',  ( 55.98639049795390576, 14.70696325443280017, -25.73482700409929791 ) ) ;
#22255 = CARTESIAN_POINT ( 'NONE',  ( 23.18611651039899968, -15.51960499682390093, -42.44846103827049433 ) ) ;
#22256 = FACE_OUTER_BOUND ( 'NONE', #13411, .T. ) ;
#22257 = CARTESIAN_POINT ( 'NONE',  ( 53.11419542519070092, 18.31613794100389825, -49.05615257636990378 ) ) ;
#22258 = CARTESIAN_POINT ( 'NONE',  ( 54.47258461985209976, -46.25235281383459807, -15.76423277873260176 ) ) ;
#22259 = DIRECTION ( 'NONE',  ( -1.000000000000000000, 0.000000000000000000, 0.000000000000000000 ) ) ;
#22260 = TOROIDAL_SURFACE ( 'NONE', #50744, 2.500000000000000000, 0.5000000000000000000 ) ;
#22261 = ORIENTED_EDGE ( 'NONE', *, *, #44650, .T. ) ;
#22262 = CARTESIAN_POINT ( 'NONE',  ( 12.28926181007750174, -22.45762284475839721, -37.95047585818409885 ) ) ;
#22263 = CARTESIAN_POINT ( 'NONE',  ( 59.03492131492150463, 15.32045715074029957, -47.92638814198690511 ) ) ;
#22264 = CARTESIAN_POINT ( 'NONE',  ( 12.89372882336123638, -8.399748356796177262, -81.15800232914327239 ) ) ;
#22265 = CARTESIAN_POINT ( 'NONE',  ( 73.04943094402750603, 1.269319268680890067, -62.52104542963419931 ) ) ;
#22266 = CARTESIAN_POINT ( 'NONE',  ( 11.42280562904119989, -65.35797272322230356, -18.14299411099350223 ) ) ;
#22267 = CARTESIAN_POINT ( 'NONE',  ( 52.63953642234348251, -49.80174121720273916, -48.69586908824972227 ) ) ;
#22268 = CARTESIAN_POINT ( 'NONE',  ( 24.04468182044177738, -15.61618932230105017, -75.79232603942232060 ) ) ;
#22269 = CARTESIAN_POINT ( 'NONE',  ( 22.90091300232175442, -15.59650344546338907, -62.45190239597013004 ) ) ;
#22270 = CARTESIAN_POINT ( 'NONE',  ( 10.72267184746520030, -11.45744867721397142, -57.66115349055309025 ) ) ;
#22271 = CARTESIAN_POINT ( 'NONE',  ( 65.11747358718560008, 1.386342629514219826, -70.29952392096339508 ) ) ;
#22272 = VERTEX_POINT ( 'NONE', #41190 ) ;
#22273 = CARTESIAN_POINT ( 'NONE',  ( 10.13539115020860137, -63.12861584496490508, -45.99741659280339690 ) ) ;
#22274 = EDGE_CURVE ( 'NONE', #37798, #8663, #9745, .T. ) ;
#22275 = CARTESIAN_POINT ( 'NONE',  ( 58.92073396209919878, -28.11618894467929763, -18.64999999999999858 ) ) ;
#22276 = EDGE_LOOP ( 'NONE', ( #24723, #6189, #30181, #43131, #40763, #25489, #29231, #12693 ) ) ;
#22277 = CARTESIAN_POINT ( 'NONE',  ( 20.30127474080329719, 10.88381105532070059, -34.64999999999999858 ) ) ;
#22278 = CARTESIAN_POINT ( 'NONE',  ( 56.93701001012390606, 19.40825549115340110, -53.86363390784850225 ) ) ;
#22279 = CARTESIAN_POINT ( 'NONE',  ( 53.07826437316199275, 19.12198495391469777, -77.22375576538830444 ) ) ;
#22280 =( BOUNDED_CURVE ( )  B_SPLINE_CURVE ( 3, ( #29482, #25282, #29988, #34177 ),
 .UNSPECIFIED., .F., .T. ) 
 B_SPLINE_CURVE_WITH_KNOTS ( ( 4, 4 ),
 ( 4.787162522534349485, 4.797305365512180231 ),
 .UNSPECIFIED. ) 
 CURVE ( )  GEOMETRIC_REPRESENTATION_ITEM ( )  RATIONAL_B_SPLINE_CURVE ( ( 1.000000000000000000, 0.9999914269130683042, 0.9999914269130683042, 1.000000000000000000 ) ) 
 REPRESENTATION_ITEM ( '' )  );
#22281 = ORIENTED_EDGE ( 'NONE', *, *, #51496, .F. ) ;
#22282 = ADVANCED_FACE ( 'NONE', ( #30920, #35118 ), #10778, .T. ) ;
#22283 = DIRECTION ( 'NONE',  ( 0.000000000000000000, 0.9319748226751540798, -0.3625230060280524302 ) ) ;
#22284 = CARTESIAN_POINT ( 'NONE',  ( 47.13393739769619373, 4.883811055320659733, -35.14999999999999858 ) ) ;
#22286 = DIRECTION ( 'NONE',  ( 0.000000000000000000, 0.000000000000000000, -1.000000000000000000 ) ) ;
#22285 = VECTOR ( 'NONE', #5313, 1000.000000000000000 ) ;
#22287 = CARTESIAN_POINT ( 'NONE',  ( 8.428798744621994743, -13.54564960420282205, -42.87567841755609521 ) ) ;
#22288 = EDGE_CURVE ( 'NONE', #26276, #36069, #6937, .T. ) ;
#22289 = CARTESIAN_POINT ( 'NONE',  ( 24.11850265849220065, -13.55962928057420136, -65.71208951153069222 ) ) ;
#22290 = LINE ( 'NONE', #27005, #5451 ) ;
#22291 = CARTESIAN_POINT ( 'NONE',  ( 43.95557740140245784, -37.91148288773651132, -70.54174288651782376 ) ) ;
#22292 = ORIENTED_EDGE ( 'NONE', *, *, #8769, .T. ) ;
#22293 = CARTESIAN_POINT ( 'NONE',  ( 61.75019796695539753, -46.11618894467930119, -37.26101630944549470 ) ) ;
#22294 = CARTESIAN_POINT ( 'NONE',  ( 12.75093326110940062, -22.25410855981340319, -48.88268834496359716 ) ) ;
#22295 = CIRCLE ( 'NONE', #49925, 12.00000000000000000 ) ;
#22296 = CARTESIAN_POINT ( 'NONE',  ( 9.233376442599690037, -18.60157552794879976, -32.14999999999999858 ) ) ;
#22297 = CARTESIAN_POINT ( 'NONE',  ( -21.36606260230379917, -62.11618894467930119, 10.84999999999999964 ) ) ;
#22298 = CARTESIAN_POINT ( 'NONE',  ( 14.00739969242919969, 20.40964180427139851, -75.33373089150879309 ) ) ;
#22299 = EDGE_CURVE ( 'NONE', #25615, #47514, #15957, .T. ) ;
#22300 = CARTESIAN_POINT ( 'NONE',  ( 8.222678474964419948, -15.61600660124389961, -50.79233150823699816 ) ) ;
#22301 = CARTESIAN_POINT ( 'NONE',  ( 43.41582131227239927, -45.06410286474709181, -6.498296231305429771 ) ) ;
#22302 = CARTESIAN_POINT ( 'NONE',  ( 19.23238759590467239, -8.313067289789655590, -61.13547072799036641 ) ) ;
#22303 = CARTESIAN_POINT ( 'NONE',  ( 24.26898003732519626, -16.95924589075189814, -59.55975014801229861 ) ) ;
#22304 = ORIENTED_EDGE ( 'NONE', *, *, #43490, .T. ) ;
#22305 = CARTESIAN_POINT ( 'NONE',  ( 52.61201418140420571, -49.81418459234139817, -28.07267484291759985 ) ) ;
#22306 = CARTESIAN_POINT ( 'NONE',  ( 56.35989604313040502, -50.72843546871860099, -74.81725475743600384 ) ) ;
#22308 = CARTESIAN_POINT ( 'NONE',  ( 41.96035236647510658, -39.76017481032943124, -76.52331057427426231 ) ) ;
#22307 = CARTESIAN_POINT ( 'NONE',  ( -0.09053481959779700883, 22.39771088603180260, -9.857808184667490536 ) ) ;
#22309 = CARTESIAN_POINT ( 'NONE',  ( 47.40880866017789685, -54.64074575612490037, -54.64987641489110359 ) ) ;
#22310 = DIRECTION ( 'NONE',  ( 0.000000000000000000, 0.000000000000000000, 1.000000000000000000 ) ) ;
#22311 = ORIENTED_EDGE ( 'NONE', *, *, #4259, .F. ) ;
#22312 = CARTESIAN_POINT ( 'NONE',  ( -3.306064913546559847, -48.27659316127069644, -4.296538301066338938 ) ) ;
#22313 = CARTESIAN_POINT ( 'NONE',  ( 47.44230769974480211, 23.39977620147499948, -54.85721486140309366 ) ) ;
#22314 = AXIS2_PLACEMENT_3D ( 'NONE', #13879, #14133, #46386 ) ;
#22315 = EDGE_CURVE ( 'NONE', #15981, #20265, #27828, .T. ) ;
#22316 = CARTESIAN_POINT ( 'NONE',  ( 45.82850501745777905, -45.11588806901219328, -7.494124676809759578 ) ) ;
#22317 = CARTESIAN_POINT ( 'NONE',  ( 16.13393739769620083, -15.61618894467929941, -28.45282021618999835 ) ) ;
#22318 = CARTESIAN_POINT ( 'NONE',  ( 57.06431677472210140, 13.92418399160115428, -25.30300627412070114 ) ) ;
#22319 = CARTESIAN_POINT ( 'NONE',  ( 11.38858895854670017, 33.99473195841849815, -17.28671580462109958 ) ) ;
#22320 = CARTESIAN_POINT ( 'NONE',  ( 51.67588111593440203, 17.38380895277190064, -77.01364305260611332 ) ) ;
#22321 = CARTESIAN_POINT ( 'NONE',  ( 53.37786163247539406, 18.14274543012349739, -48.82821703136220037 ) ) ;
#22322 = DIRECTION ( 'NONE',  ( -0.3294064756441279496, -0.9441882088883098989, 0.000000000000000000 ) ) ;
#22323 = CARTESIAN_POINT ( 'NONE',  ( 57.22510014093110442, -47.50321319438739920, -48.27967399149409999 ) ) ;
#22324 = CARTESIAN_POINT ( 'NONE',  ( 52.81005723544840436, 18.43886315067999959, -28.15002577751260304 ) ) ;
#22325 = EDGE_CURVE ( 'NONE', #50249, #40580, #14449, .T. ) ;
#22326 = CARTESIAN_POINT ( 'NONE',  ( 50.44957631477119975, 22.08479505950380073, -54.57514961256589459 ) ) ;
#22327 = CARTESIAN_POINT ( 'NONE',  ( 63.59767441460930115, 1.382577763791200010, -69.21733240916789498 ) ) ;
#22328 = CARTESIAN_POINT ( 'NONE',  ( 53.05489977530229595, 18.36750851102400262, -49.10811586475909962 ) ) ;
#22329 = DIRECTION ( 'NONE',  ( 0.000000000000000000, -1.000000000000000000, 0.000000000000000000 ) ) ;
#22330 = CARTESIAN_POINT ( 'NONE',  ( 22.36082438643301273, -18.90756276022864668, -73.00202728647948902 ) ) ;
#22331 = CARTESIAN_POINT ( 'NONE',  ( 10.49154450428839880, 32.04238758567439760, -45.62559114465060617 ) ) ;
#22332 = CARTESIAN_POINT ( 'NONE',  ( 72.94908864064930754, 0.9618757110850010283, -62.06981987203609918 ) ) ;
#22333 = CIRCLE ( 'NONE', #20640, 16.00000000000000000 ) ;
#22334 = CYLINDRICAL_SURFACE ( 'NONE', #42706, 2.000000000000170530 ) ;
#22335 = VERTEX_POINT ( 'NONE', #15478 ) ;
#22336 = CARTESIAN_POINT ( 'NONE',  ( 12.71077838082760891, 24.23706720221435162, -75.54041227948643211 ) ) ;
#22337 = VERTEX_POINT ( 'NONE', #11035 ) ;
#22338 = ORIENTED_EDGE ( 'NONE', *, *, #16254, .F. ) ;
#22339 = CARTESIAN_POINT ( 'NONE',  ( 56.53399784873889899, 19.21501630139210093, -52.81205167924800037 ) ) ;
#22340 = CARTESIAN_POINT ( 'NONE',  ( 76.50051362292605006, -2.884157946879440715, -13.22963151320726283 ) ) ;
#22341 = ORIENTED_EDGE ( 'NONE', *, *, #41710, .T. ) ;
#22342 = CARTESIAN_POINT ( 'NONE',  ( 12.89514957290669983, -65.50886968517070841, -47.53407047177050515 ) ) ;
#22343 = CARTESIAN_POINT ( 'NONE',  ( 57.44551019405400183, -45.12993590191310034, -25.53739291223670094 ) ) ;
#22344 = DIRECTION ( 'NONE',  ( 1.000000000000000000, 0.000000000000000000, 0.000000000000000000 ) ) ;
#22345 = FACE_OUTER_BOUND ( 'NONE', #3219, .T. ) ;
#22346 = EDGE_CURVE ( 'NONE', #45450, #18491, #2655, .T. ) ;
#22347 = CARTESIAN_POINT ( 'NONE',  ( 63.48441347673288959, 1.386342629514219826, -68.66646381051069170 ) ) ;
#22348 = ORIENTED_EDGE ( 'NONE', *, *, #34531, .T. ) ;
#22349 = CARTESIAN_POINT ( 'NONE',  ( 11.83411043809303465, 34.19861816370081442, -22.31001989919771944 ) ) ;
#22350 = CARTESIAN_POINT ( 'NONE',  ( 45.17780009201627678, 6.831281286145213016, -64.43066996210254160 ) ) ;
#22351 = LINE ( 'NONE', #36588, #44670 ) ;
#22352 = EDGE_CURVE ( 'NONE', #12686, #38024, #39548, .T. ) ;
#22353 = ORIENTED_EDGE ( 'NONE', *, *, #17863, .F. ) ;
#22354 = CARTESIAN_POINT ( 'NONE',  ( 46.21902970698399571, -45.19874479850450655, -8.545594584115770331 ) ) ;
#22355 = DIRECTION ( 'NONE',  ( -1.000000000000000000, 0.000000000000000000, 0.000000000000000000 ) ) ;
#22356 = CARTESIAN_POINT ( 'NONE',  ( 16.49314696555249782, 19.88381105389379755, -20.88058500138470208 ) ) ;
#22357 = DIRECTION ( 'NONE',  ( 0.000000000000000000, 0.000000000000000000, 1.000000000000000000 ) ) ;
#22358 = CARTESIAN_POINT ( 'NONE',  ( 21.28448762020170193, -20.00650175921066065, -46.67749910197144914 ) ) ;
#22359 = CARTESIAN_POINT ( 'NONE',  ( 63.93393739769619089, 1.883811055320669947, -62.44999999999999574 ) ) ;
#22360 = CARTESIAN_POINT ( 'NONE',  ( 47.25417729284069424, -54.61827072552059548, -74.80726814568210159 ) ) ;
#22361 = CARTESIAN_POINT ( 'NONE',  ( 45.09885310914830114, 13.74449180402419834, -6.429922486547810401 ) ) ;
#22362 = CARTESIAN_POINT ( 'NONE',  ( 57.50723796702470025, 15.88381105532069704, -31.98003398807230369 ) ) ;
#22363 = PRODUCT ( 'MAS-691', 'MAS-691', '', ( #23824 ) ) ;
#22364 = CARTESIAN_POINT ( 'NONE',  ( 51.93948715274890304, 19.85719722970700118, -76.10418646478689197 ) ) ;
#22365 = AXIS2_PLACEMENT_3D ( 'NONE', #781, #32214, #8404 ) ;
#22366 = CYLINDRICAL_SURFACE ( 'NONE', #44555, 2.000000000000058620 ) ;
#22367 = CARTESIAN_POINT ( 'NONE',  ( 23.76520713869530255, -17.44668068275500161, -81.36245008104741316 ) ) ;
#22368 = ORIENTED_EDGE ( 'NONE', *, *, #48203, .F. ) ;
#22369 = CARTESIAN_POINT ( 'NONE',  ( 44.13393739769620083, -36.11618894467930119, -35.14999999999999858 ) ) ;
#22370 = CARTESIAN_POINT ( 'NONE',  ( 6.047473704414409568, -58.85581576903580014, -11.31522686691929991 ) ) ;
#22371 = CARTESIAN_POINT ( 'NONE',  ( 76.39679632360071082, -12.51312258731159766, -12.78270703766589911 ) ) ;
#22372 = CARTESIAN_POINT ( 'NONE',  ( 75.12449000029563706, 13.75696482515094310, -14.63746784062838913 ) ) ;
#22373 = CARTESIAN_POINT ( 'NONE',  ( 16.65420337943509566, -51.11618894467930119, -15.67544740040250062 ) ) ;
#22374 = CARTESIAN_POINT ( 'NONE',  ( 13.58714272597830686, -55.53442211211926605, -76.07915437886748578 ) ) ;
#22375 = CARTESIAN_POINT ( 'NONE',  ( 14.74632770935266102, -16.62434639553314142, -170.7999095292539948 ) ) ;
#22376 = EDGE_CURVE ( 'NONE', #20336, #16602, #51123, .T. ) ;
#22377 = CARTESIAN_POINT ( 'NONE',  ( 82.41472024409949881, -45.17082120583620508, -46.87528017089150012 ) ) ;
#22378 = CARTESIAN_POINT ( 'NONE',  ( 63.54731047306190561, 1.396834109478129804, -68.84999999999999432 ) ) ;
#22379 = CARTESIAN_POINT ( 'NONE',  ( 42.37474662607149867, 12.16745287750829974, -4.189334837800680056 ) ) ;
#22380 = CARTESIAN_POINT ( 'NONE',  ( 65.25681082723269810, 1.383811055320669947, -70.34375346881599000 ) ) ;
#22381 = DIRECTION ( 'NONE',  ( 0.000000000000000000, 0.000000000000000000, 1.000000000000000000 ) ) ;
#22382 = CARTESIAN_POINT ( 'NONE',  ( 66.23540447448814916, -49.95860450174473044, -71.35146707679193412 ) ) ;
#22383 = EDGE_CURVE ( 'NONE', #37252, #30218, #3437, .T. ) ;
#22384 = CARTESIAN_POINT ( 'NONE',  ( 75.98223876097091534, -43.32481619739640166, -13.62276456639723321 ) ) ;
#22385 = CARTESIAN_POINT ( 'NONE',  ( 57.48324947012589803, 13.88381105532070059, -17.42702405245080044 ) ) ;
#22386 = EDGE_CURVE ( 'NONE', #13106, #41523, #12338, .T. ) ;
#22387 = ORIENTED_EDGE ( 'NONE', *, *, #44461, .F. ) ;
#22388 = CARTESIAN_POINT ( 'NONE',  ( 9.837961696380780552, -11.63280039888219974, -50.24690406358499217 ) ) ;
#22389 = CARTESIAN_POINT ( 'NONE',  ( 63.58579710287288833, 1.402020837643050077, -62.24736188354039257 ) ) ;
#22390 = VERTEX_POINT ( 'NONE', #19656 ) ;
#22391 = CARTESIAN_POINT ( 'NONE',  ( 53.29384558423090112, -50.54670888882439783, -48.47378032971909789 ) ) ;
#22392 = CARTESIAN_POINT ( 'NONE',  ( 60.49059093688929778, -45.82073196953280814, -47.74858579941459880 ) ) ;
#22393 = DIRECTION ( 'NONE',  ( 0.000000000000000000, 0.000000000000000000, 1.000000000000000000 ) ) ;
#22394 = DIRECTION ( 'NONE',  ( -1.000000000000000000, 0.000000000000000000, 0.000000000000000000 ) ) ;
#22395 = CARTESIAN_POINT ( 'NONE',  ( 46.28203251265257023, 8.876941422008853166, -55.58930854417799594 ) ) ;
#22396 = DIRECTION ( 'NONE',  ( 1.000000000000000000, 0.000000000000000000, 0.000000000000000000 ) ) ;
#22397 = CARTESIAN_POINT ( 'NONE',  ( 10.07635536168542245, -54.02136955896584425, -34.82441657595373385 ) ) ;
#22398 = ORIENTED_EDGE ( 'NONE', *, *, #39645, .T. ) ;
#22399 = ORIENTED_EDGE ( 'NONE', *, *, #20485, .F. ) ;
#22400 = ORIENTED_EDGE ( 'NONE', *, *, #9370, .F. ) ;
#22401 = DIRECTION ( 'NONE',  ( 0.5685928097855378338, 0.5944782866685498490, -0.5685928097855378338 ) ) ;
#22402 = CARTESIAN_POINT ( 'NONE',  ( 61.16489974143080133, -45.30856623237389869, -46.97020373819919570 ) ) ;
#22403 = CARTESIAN_POINT ( 'NONE',  ( 52.70547899565750072, -49.76225394339979857, -48.81521342827540622 ) ) ;
#22404 = DIRECTION ( 'NONE',  ( -1.031008731411319881E-16, 1.000000000000000000, 0.000000000000000000 ) ) ;
#22405 = AXIS2_PLACEMENT_3D ( 'NONE', #48862, #40214, #32572 ) ;
#22406 = ORIENTED_EDGE ( 'NONE', *, *, #8846, .F. ) ;
#22407 = EDGE_CURVE ( 'NONE', #37013, #31554, #7619, .T. ) ;
#22408 = VERTEX_POINT ( 'NONE', #43768 ) ;
#22409 = CARTESIAN_POINT ( 'NONE',  ( 24.01053399803918253, -14.85515835932281625, -77.47701762277769433 ) ) ;
#22410 = B_SPLINE_CURVE_WITH_KNOTS ( 'NONE', 3,
 ( #8436, #32760, #16287, #811, #12893, #41427, #16813, #28848, #44851, #21237, #12360, #32493, #32242, #49313, #45108, #24380, #28324, #8956, #48520, #49053, #5544, #24899, #13160, #36448, #44324, #555, #13408, #12627, #40912 ),
 .UNSPECIFIED., .F., .F.,
 ( 4, 2, 1, 1, 1, 1, 1, 2, 2, 2, 2, 2, 2, 2, 2, 2, 4 ),
 ( 0.5000036381911079353, 0.5002477770396474011, 0.5004919158881868668, 0.5009801935852656873, 0.5019567489794234394, 0.5039098597677392766, 0.5078160813443711730, 0.5156285244976349658, 0.5312534108041627734, 0.5625031834172187217, 0.6250027286433301743, 0.6875022738694417379, 0.7500018190955533015, 0.8125013643216649761, 0.8750009095477766508, 0.9375004547738883254, 1.000000000000000000 ),
 .UNSPECIFIED. ) ;
#22411 = B_SPLINE_CURVE_WITH_KNOTS ( 'NONE', 3,
 ( #43912, #44166, #16637, #36288, #48625, #44683, #40489, #48359, #16382, #31574 ),
 .UNSPECIFIED., .F., .F.,
 ( 4, 2, 2, 2, 4 ),
 ( -0.0004107207312076359960, 0.000000000000000000, 0.01419180571516310066, 0.04450164637011760210, 0.05031563485841133304 ),
 .UNSPECIFIED. ) ;
#22412 = CARTESIAN_POINT ( 'NONE',  ( 16.13393739769620083, -29.47259540523039689, -35.14999999999999858 ) ) ;
#22413 = EDGE_LOOP ( 'NONE', ( #48286, #3617, #21990, #40858 ) ) ;
#22414 = CARTESIAN_POINT ( 'NONE',  ( 66.63393739769620083, -38.11618894467930119, -73.25000000000000000 ) ) ;
#22415 = CARTESIAN_POINT ( 'NONE',  ( 51.98443728612009096, -51.36758245232200437, -75.98853294935470615 ) ) ;
#22416 = CARTESIAN_POINT ( 'NONE',  ( 60.59271029648169105, 14.39476059538499975, -47.40213830669640060 ) ) ;
#22417 = CARTESIAN_POINT ( 'NONE',  ( 13.83141090584470057, -23.11852987216700228, -78.60728138436070367 ) ) ;
#22418 = CARTESIAN_POINT ( 'NONE',  ( 2.422196078461530178, -5.407548561780520124, -35.02873218748179340 ) ) ;
#22419 = CARTESIAN_POINT ( 'NONE',  ( 42.34708436978809942, 14.06745345395279934, -6.529032511125610228 ) ) ;
#22420 = CARTESIAN_POINT ( 'NONE',  ( 42.42181531931939986, -43.19228534352320281, -3.882827786889420096 ) ) ;
#22421 = CARTESIAN_POINT ( 'NONE',  ( 24.04519454997480210, -15.61618869140488997, -79.50766696426083513 ) ) ;
#22422 = CARTESIAN_POINT ( 'NONE',  ( 66.72561048563099462, 1.883811055320649963, -20.64999999980150136 ) ) ;
#22423 = CARTESIAN_POINT ( 'NONE',  ( 64.62814679718090360, 1.136680095839029958, -70.46339166529689635 ) ) ;
#22424 = LINE ( 'NONE', #50488, #11043 ) ;
#22425 = CARTESIAN_POINT ( 'NONE',  ( 8.303488653731021074, -15.09578462944280020, -50.30862910410869659 ) ) ;
#22426 = ORIENTED_EDGE ( 'NONE', *, *, #3923, .F. ) ;
#22427 = CARTESIAN_POINT ( 'NONE',  ( 43.55793695338589799, 14.79940918324820132, -7.980363424730000155 ) ) ;
#22428 = CARTESIAN_POINT ( 'NONE',  ( 44.39055831136107599, -39.98592374925685533, -64.76712992094270760 ) ) ;
#22429 = CARTESIAN_POINT ( 'NONE',  ( 27.86468381613284961, -7.093302786438550278, -6.928362978644219794 ) ) ;
#22430 = AXIS2_PLACEMENT_3D ( 'NONE', #34791, #42682, #50797 ) ;
#22431 = CARTESIAN_POINT ( 'NONE',  ( 85.84022851002180232, 17.38381105532069881, -53.47585302082339354 ) ) ;
#22432 = CARTESIAN_POINT ( 'NONE',  ( 63.15863832053869942, 1.096036836948800053, -68.93088433361418765 ) ) ;
#22433 = CARTESIAN_POINT ( 'NONE',  ( 47.84470410613830182, -54.42058614811499950, -54.90151223973010275 ) ) ;
#22434 = DIRECTION ( 'NONE',  ( 0.000000000000000000, 0.000000000000000000, 1.000000000000000000 ) ) ;
#22435 = EDGE_CURVE ( 'NONE', #7479, #19147, #11947, .T. ) ;
#22436 = CARTESIAN_POINT ( 'NONE',  ( 56.45679588454870412, 19.42305698160840066, -53.17273421675590583 ) ) ;
#22437 = CARTESIAN_POINT ( 'NONE',  ( 41.40756759976829926, 13.53921337778190015, -5.393983492778530398 ) ) ;
#22438 = CARTESIAN_POINT ( 'NONE',  ( 48.04015573092420510, 23.13167815216619871, -55.20742902216350245 ) ) ;
#22439 = VERTEX_POINT ( 'NONE', #31943 ) ;
#22440 = CARTESIAN_POINT ( 'NONE',  ( 17.01654511880040133, -8.618792084267338893, -78.38711848170969176 ) ) ;
#22441 = ORIENTED_EDGE ( 'NONE', *, *, #19397, .T. ) ;
#22442 = CARTESIAN_POINT ( 'NONE',  ( 71.22849534471220068, 1.384708701328909886, -70.30837376962780638 ) ) ;
#22443 = DIRECTION ( 'NONE',  ( 0.000000000000000000, 0.000000000000000000, -1.000000000000000000 ) ) ;
#22444 = CARTESIAN_POINT ( 'NONE',  ( 83.76204656006096627, 13.76116163493793820, -47.48603732758919449 ) ) ;
#22445 = CARTESIAN_POINT ( 'NONE',  ( 16.13393739769620083, -15.61618894467929941, -15.65000000000000036 ) ) ;
#22447 = CARTESIAN_POINT ( 'NONE',  ( 53.37088539291629985, 17.75190881940800125, -26.62991259020409984 ) ) ;
#22446 = CYLINDRICAL_SURFACE ( 'NONE', #28198, 1.999999999999997335 ) ;
#22448 = CARTESIAN_POINT ( 'NONE',  ( 14.50584207537670167, -22.47854016842669722, -73.02696842882760109 ) ) ;
#22449 = DIRECTION ( 'NONE',  ( 0.6918010270571969267, 0.3994115091971329190, 0.6015661104845219098 ) ) ;
#22450 = CARTESIAN_POINT ( 'NONE',  ( 18.20468117247153472, -23.32127088709334828, -41.92433441774539915 ) ) ;
#22451 = CARTESIAN_POINT ( 'NONE',  ( 55.92358841828349370, -45.89462731853816280, -25.40852269161388222 ) ) ;
#22452 = ORIENTED_EDGE ( 'NONE', *, *, #19976, .T. ) ;
#22453 = CARTESIAN_POINT ( 'NONE',  ( 68.13393739845096775, -29.66618894467940137, -41.65000000139604452 ) ) ;
#22454 = ORIENTED_EDGE ( 'NONE', *, *, #5051, .F. ) ;
#22455 = ORIENTED_EDGE ( 'NONE', *, *, #34110, .F. ) ;
#22456 = CARTESIAN_POINT ( 'NONE',  ( 12.09242720215750033, -64.92301394585230412, -16.23377612492940258 ) ) ;
#22457 = EDGE_CURVE ( 'NONE', #49949, #45766, #18633, .T. ) ;
#22458 = CARTESIAN_POINT ( 'NONE',  ( 24.04483892795884969, -15.57353102523303434, -39.50595550450194082 ) ) ;
#22459 = CARTESIAN_POINT ( 'NONE',  ( 11.79211174348889912, 33.77432752955800055, -45.32950553571880192 ) ) ;
#22460 = B_SPLINE_CURVE_WITH_KNOTS ( 'NONE', 3,
 ( #30746, #18704, #31514, #43598, #10600, #2986, #14778, #39407, #39150, #46769 ),
 .UNSPECIFIED., .F., .F.,
 ( 4, 1, 1, 1, 1, 1, 1, 4 ),
 ( 0.000000000000000000, 0.1428507730289225175, 0.2857076245177915252, 0.4285644760066605330, 0.5714213274955285415, 0.7142781789843976048, 0.8571350304732666681, 1.000000000000000000 ),
 .UNSPECIFIED. ) ;
#22461 = CARTESIAN_POINT ( 'NONE',  ( 13.00893739769619906, -65.51843714052719747, -47.75434321273180416 ) ) ;
#22462 = ORIENTED_EDGE ( 'NONE', *, *, #38951, .F. ) ;
#22463 = ORIENTED_EDGE ( 'NONE', *, *, #38766, .F. ) ;
#22464 = EDGE_CURVE ( 'NONE', #38344, #6571, #28695, .T. ) ;
#22465 = CARTESIAN_POINT ( 'NONE',  ( 24.04215779552914256, -15.84268908224270511, -55.51678385230713531 ) ) ;
#22466 = DIRECTION ( 'NONE',  ( 0.000000000000000000, 0.000000000000000000, -1.000000000000000000 ) ) ;
#22467 = CARTESIAN_POINT ( 'NONE',  ( 52.84041160373019608, 18.34707223868749892, -48.42032881049700421 ) ) ;
#22468 = EDGE_CURVE ( 'NONE', #49938, #14025, #19104, .T. ) ;
#22469 = CARTESIAN_POINT ( 'NONE',  ( 62.29010619281529415, -1.891186742061369941, -16.10088301903060071 ) ) ;
#22470 = CARTESIAN_POINT ( 'NONE',  ( 50.90450148898350591, -49.87900598378690376, -76.22583875105431162 ) ) ;
#22471 = CARTESIAN_POINT ( 'NONE',  ( 58.20425128766380141, -49.07305351875690036, -51.45101314545409821 ) ) ;
#22472 = ORIENTED_EDGE ( 'NONE', *, *, #31624, .F. ) ;
#22473 = CARTESIAN_POINT ( 'NONE',  ( 8.380192598090266287, -13.82703671535675305, -32.86439260443115273 ) ) ;
#22474 = CARTESIAN_POINT ( 'NONE',  ( 68.13393739769819035, 19.47158195952109594, -72.59354914830207406 ) ) ;
#22475 = ORIENTED_EDGE ( 'NONE', *, *, #47243, .F. ) ;
#22476 = DIRECTION ( 'NONE',  ( -0.8660254037844387076, -0.4999999999999998890, 0.000000000000000000 ) ) ;
#22477 = CIRCLE ( 'NONE', #9924, 5.499999999999998224 ) ;
#22478 = CARTESIAN_POINT ( 'NONE',  ( 57.22322293371580315, -47.50141109488779989, -48.27531557238859961 ) ) ;
#22479 = AXIS2_PLACEMENT_3D ( 'NONE', #35881, #7342, #3673 ) ;
#22480 = CARTESIAN_POINT ( 'NONE',  ( 23.97139847576909943, -16.01737648346080078, -48.02877399380358980 ) ) ;
#22481 = CARTESIAN_POINT ( 'NONE',  ( 13.09367229119200005, -50.61305962739500330, -21.36973413670409983 ) ) ;
#22482 = CARTESIAN_POINT ( 'NONE',  ( 54.08449847407359812, 19.43926436916860112, -76.52238400108929284 ) ) ;
#22483 = AXIS2_PLACEMENT_3D ( 'NONE', #45677, #2418, #9779 ) ;
#22484 = CARTESIAN_POINT ( 'NONE',  ( 46.50380985604989803, -53.09853600777310589, -76.13981661584659832 ) ) ;
#22485 = CARTESIAN_POINT ( 'NONE',  ( 56.73667514912609988, 14.03196534028450060, -17.72798751313560217 ) ) ;
#22486 = CARTESIAN_POINT ( 'NONE',  ( 17.01654511880040133, -8.618792084267338893, -78.38711848170969176 ) ) ;
#22487 = CARTESIAN_POINT ( 'NONE',  ( 56.68249757891010177, -50.44500735585980067, -52.87688493394379918 ) ) ;
#22488 = CARTESIAN_POINT ( 'NONE',  ( 9.567436321604839478, -18.18982893351659769, -39.72828012266349873 ) ) ;
#22489 = CARTESIAN_POINT ( 'NONE',  ( -7.298084762738758613, -16.21081643554488494, 4.943674098299959851 ) ) ;
#22490 = VERTEX_POINT ( 'NONE', #15991 ) ;
#22491 = CARTESIAN_POINT ( 'NONE',  ( 47.64143405400400866, 23.30250925608780221, -74.14999581260518369 ) ) ;
#22492 = CARTESIAN_POINT ( 'NONE',  ( 64.81394005445639550, 0.9259537755896120048, -60.65222959644560063 ) ) ;
#22493 = CARTESIAN_POINT ( 'NONE',  ( 24.04493741226235315, -14.58064815428408245, -51.46599901981314673 ) ) ;
#22494 = CARTESIAN_POINT ( 'NONE',  ( 12.52565026941822168, -65.42862977055203544, -23.52286200862776511 ) ) ;
#22495 = CARTESIAN_POINT ( 'NONE',  ( 46.03123730580679762, -45.11618894467689955, -7.582885969263020165 ) ) ;
#22496 = CARTESIAN_POINT ( 'NONE',  ( 29.04782745927229826, -4.524248062580669583, -34.86734588637909837 ) ) ;
#22497 = CARTESIAN_POINT ( 'NONE',  ( 34.13393739769599478, 17.88381105532079829, -35.14999999999999858 ) ) ;
#22498 = CARTESIAN_POINT ( 'NONE',  ( 82.34924927927150407, 14.41608331847699986, -47.73066065071600406 ) ) ;
#22499 = CARTESIAN_POINT ( 'NONE',  ( 16.13393739769620083, -15.61618894467929941, -11.23251175440650051 ) ) ;
#22501 = CARTESIAN_POINT ( 'NONE',  ( 46.70905700370144586, -39.31695218441910100, -57.02994487585867489 ) ) ;
#22500 = CARTESIAN_POINT ( 'NONE',  ( 53.63393739769619373, -62.82329572586585442, 11.14289321881345529 ) ) ;
#22502 = ADVANCED_FACE ( 'NONE', ( #28020 ), #26381, .T. ) ;
#22503 = CARTESIAN_POINT ( 'NONE',  ( 16.34469624625884521, -23.55230478456017806, -32.28382467401409173 ) ) ;
#22504 = CARTESIAN_POINT ( 'NONE',  ( -0.3561701380248140092, 32.06759910672769820, -50.35138997524130389 ) ) ;
#22505 = VERTEX_POINT ( 'NONE', #4700 ) ;
#22506 = AXIS2_PLACEMENT_3D ( 'NONE', #44984, #14761, #6643 ) ;
#22507 = CARTESIAN_POINT ( 'NONE',  ( 52.73800511975559857, -49.72354018477579274, -48.71590736184970183 ) ) ;
#22508 = ORIENTED_EDGE ( 'NONE', *, *, #4979, .F. ) ;
#22509 = AXIS2_PLACEMENT_3D ( 'NONE', #46180, #18888, #30675 ) ;
#22510 = CARTESIAN_POINT ( 'NONE',  ( 14.34417029198830029, 19.88381105532299742, -22.49240188329279988 ) ) ;
#22511 = CARTESIAN_POINT ( 'NONE',  ( 17.01981251849182186, -8.849199924388678085, -41.99448657106753302 ) ) ;
#22512 = CARTESIAN_POINT ( 'NONE',  ( 13.61938558558030010, 20.19483563532820014, -23.15000001641130112 ) ) ;
#22513 = CARTESIAN_POINT ( 'NONE',  ( 57.57776213900729800, 13.88371113915540001, -25.40878180930539898 ) ) ;
#22514 = AXIS2_PLACEMENT_3D ( 'NONE', #46528, #18718, #34695 ) ;
#22515 = CARTESIAN_POINT ( 'NONE',  ( 10.31980611544169868, -19.60848604401130402, -49.26128910974169628 ) ) ;
#22517 = CARTESIAN_POINT ( 'NONE',  ( 28.84982806847620296, -26.63452174666150185, -34.69901084462020435 ) ) ;
#22516 = AXIS2_PLACEMENT_3D ( 'NONE', #8698, #20730, #36990 ) ;
#22518 = CARTESIAN_POINT ( 'NONE',  ( 52.65605176727499526, 18.54635246044519903, -48.59646220643460879 ) ) ;
#22519 = CARTESIAN_POINT ( 'NONE',  ( 55.17090527502239894, -46.00774235025210146, -16.22561265231399830 ) ) ;
#22520 = DIRECTION ( 'NONE',  ( 0.000000000000000000, 0.000000000000000000, 1.000000000000000000 ) ) ;
#22521 = VERTEX_POINT ( 'NONE', #15730 ) ;
#22522 = CARTESIAN_POINT ( 'NONE',  ( 9.015194180556269643, -12.31312321847780034, -38.42578944456590051 ) ) ;
#22523 = CARTESIAN_POINT ( 'NONE',  ( 11.35626914494079998, -65.29495917086049417, -17.73521909030350230 ) ) ;
#22524 = CARTESIAN_POINT ( 'NONE',  ( 11.28331493908370042, 33.98248205784230436, -47.30875510506540138 ) ) ;
#22525 = CARTESIAN_POINT ( 'NONE',  ( 72.95172982307090592, 1.328073773609220076, -62.51929651814780442 ) ) ;
#22526 = CARTESIAN_POINT ( 'NONE',  ( 10.72852875956099972, -64.94169572740939600, -18.17421237900510178 ) ) ;
#22527 = CARTESIAN_POINT ( 'NONE',  ( 52.67198760255845968, -49.78119412946662692, -48.75777783608981508 ) ) ;
#22528 = DIRECTION ( 'NONE',  ( -0.1686178020941689892, 0.6660492713794449182, 0.7265992051412129005 ) ) ;
#22529 = CARTESIAN_POINT ( 'NONE',  ( 15.09841768666722572, -7.705185590434979304, -45.25062777107746825 ) ) ;
#22530 = CARTESIAN_POINT ( 'NONE',  ( 22.90093740290240731, -14.73039754886785957, -58.41115327826027936 ) ) ;
#22531 = EDGE_LOOP ( 'NONE', ( #14817, #17247, #43129, #40996, #27425, #28451, #11723 ) ) ;
#22532 = CARTESIAN_POINT ( 'NONE',  ( 64.73018593529990028, 0.9325382164350189962, -70.59115830928880087 ) ) ;
#22533 = ORIENTED_EDGE ( 'NONE', *, *, #26950, .T. ) ;
#22534 = CARTESIAN_POINT ( 'NONE',  ( 10.98008937475129976, -63.44096224164839981, -44.74889856825390666 ) ) ;
#22535 = DIRECTION ( 'NONE',  ( 0.000000000000000000, 0.000000000000000000, -1.000000000000000000 ) ) ;
#22536 = ORIENTED_EDGE ( 'NONE', *, *, #1110, .F. ) ;
#22537 = ADVANCED_FACE ( 'NONE', ( #31685 ), #10267, .T. ) ;
#22538 = CARTESIAN_POINT ( 'NONE',  ( 64.93393739769619799, 10.88381105532070059, -61.44999999999999574 ) ) ;
#22539 = CARTESIAN_POINT ( 'NONE',  ( 57.32356178356099718, 19.18213064475359886, -53.00097363025420094 ) ) ;
#22540 = CARTESIAN_POINT ( 'NONE',  ( 52.75996715995819386, 18.93637462048650022, -77.25935876731659846 ) ) ;
#22541 = ORIENTED_EDGE ( 'NONE', *, *, #35366, .F. ) ;
#22542 = CARTESIAN_POINT ( 'NONE',  ( 34.38393739769620083, -15.61618894467929941, 7.849999999999999645 ) ) ;
#22543 = FACE_BOUND ( 'NONE', #31803, .T. ) ;
#22544 = DIRECTION ( 'NONE',  ( 1.000000000000000000, 0.000000000000000000, 0.000000000000000000 ) ) ;
#22545 = CARTESIAN_POINT ( 'NONE',  ( 24.13155739828989965, -17.62138080134500129, -65.87052737365779365 ) ) ;
#22546 = DIRECTION ( 'NONE',  ( -0.7071067811865475727, 0.000000000000000000, -0.7071067811865475727 ) ) ;
#22547 = CARTESIAN_POINT ( 'NONE',  ( 44.32161486965532049, -37.95901749436502826, -68.71160878878293943 ) ) ;
#22548 = ORIENTED_EDGE ( 'NONE', *, *, #36725, .T. ) ;
#22549 = CIRCLE ( 'NONE', #10863, 24.00000000000000000 ) ;
#22550 = VECTOR ( 'NONE', #21767, 1000.000000000000000 ) ;
#22551 = CYLINDRICAL_SURFACE ( 'NONE', #35082, 1.999999999999999112 ) ;
#22552 = CARTESIAN_POINT ( 'NONE',  ( 11.20062545640499962, -21.19912070989539998, -56.96301931345279712 ) ) ;
#22553 = TOROIDAL_SURFACE ( 'NONE', #31745, 25.10000000000000142, 4.000000000000050626 ) ;
#22554 = CARTESIAN_POINT ( 'NONE',  ( 8.829388714618341183, -15.77602776797299988, -32.14999999999999858 ) ) ;
#22555 = CIRCLE ( 'NONE', #44294, 6.099999999999994316 ) ;
#22556 = DIRECTION ( 'NONE',  ( 0.000000000000000000, 0.000000000000000000, 1.000000000000000000 ) ) ;
#22557 = CARTESIAN_POINT ( 'NONE',  ( 13.76101378273559916, 20.06273318926150040, -74.35769860268439402 ) ) ;
#22558 = DIRECTION ( 'NONE',  ( 0.000000000000000000, 0.000000000000000000, -1.000000000000000000 ) ) ;
#22559 = CARTESIAN_POINT ( 'NONE',  ( 41.12782547105919662, -44.91524683664780326, -5.505761199517789528 ) ) ;
#22560 = CARTESIAN_POINT ( 'NONE',  ( 8.298958134817842947, -14.29909715232032852, -60.56060963056555124 ) ) ;
#22561 = CARTESIAN_POINT ( 'NONE',  ( 23.92311594283500042, -12.91222550170799899, -59.40131228588499823 ) ) ;
#22562 = ORIENTED_EDGE ( 'NONE', *, *, #12550, .T. ) ;
#22563 = CARTESIAN_POINT ( 'NONE',  ( 20.07980155385570242, -22.42390109179229896, -32.14999999999999858 ) ) ;
#22564 = CARTESIAN_POINT ( 'NONE',  ( 56.25504298498950817, -50.77785272729379784, -74.74462238221099142 ) ) ;
#22566 = CARTESIAN_POINT ( 'NONE',  ( 42.22528920520127826, -39.78856913145678220, -75.24368859111383756 ) ) ;
#22565 = CARTESIAN_POINT ( 'NONE',  ( -6.219785763107670284, 14.61265879496390063, -4.702705381378909699 ) ) ;
#22567 = ADVANCED_FACE ( 'NONE', ( #21449 ), #14114, .F. ) ;
#22568 = CARTESIAN_POINT ( 'NONE',  ( 63.24698825150780124, 1.338092079250050137, -68.62019553714330300 ) ) ;
#22569 = DIRECTION ( 'NONE',  ( 0.3445670372598628184, 0.6174735272333260472, -0.7071067811865442421 ) ) ;
#22570 = VERTEX_POINT ( 'NONE', #45577 ) ;
#22571 = CARTESIAN_POINT ( 'NONE',  ( 38.67452568954060155, 1.883811055320659955, -81.65000000000000568 ) ) ;
#22572 = EDGE_CURVE ( 'NONE', #15955, #34773, #25114, .T. ) ;
#22573 = CARTESIAN_POINT ( 'NONE',  ( 47.48084007132430173, 23.37089297048629888, -54.76237024660140662 ) ) ;
#22574 = CARTESIAN_POINT ( 'NONE',  ( 72.83393739769620367, 1.383811055320669947, -68.50657137141709541 ) ) ;
#22575 = CARTESIAN_POINT ( 'NONE',  ( 63.39331655121669939, 1.326134026835559920, -62.35486255807249734 ) ) ;
#22576 = DIRECTION ( 'NONE',  ( -3.885780586188051426E-13, 0.9739538916850928318, 0.2267461507313025260 ) ) ;
#22577 = CARTESIAN_POINT ( 'NONE',  ( 11.84416398831050010, 33.85620967646509882, -16.58498012167680002 ) ) ;
#22578 = ADVANCED_FACE ( 'NONE', ( #1292 ), #4965, .T. ) ;
#22579 = DIRECTION ( 'NONE',  ( 0.000000000000000000, 0.000000000000000000, -1.000000000000000000 ) ) ;
#22580 = CARTESIAN_POINT ( 'NONE',  ( 53.04797525238309674, 18.31477690342330078, -48.83268161531540130 ) ) ;
#22581 = CARTESIAN_POINT ( 'NONE',  ( 61.13393739769620083, -43.11618894467930119, -84.38499399519520239 ) ) ;
#22582 = DIRECTION ( 'NONE',  ( 0.000000000000000000, 0.000000000000000000, -1.000000000000000000 ) ) ;
#22583 = CARTESIAN_POINT ( 'NONE',  ( 55.52913409436600034, 15.90026116505450027, -26.42135380471329853 ) ) ;
#22584 = DIRECTION ( 'NONE',  ( 0.000000000000000000, 1.000000000000000000, 0.000000000000000000 ) ) ;
#22585 = CARTESIAN_POINT ( 'NONE',  ( 18.20460997748778098, -7.911086879560232710, -37.37566666715131447 ) ) ;
#22586 = AXIS2_PLACEMENT_3D ( 'NONE', #31119, #47648, #27710 ) ;
#22587 = CYLINDRICAL_SURFACE ( 'NONE', #9375, 0.4999999999999980571 ) ;
#22588 = CARTESIAN_POINT ( 'NONE',  ( 46.23055864956999983, -45.11618894467940066, -7.629554990163329720 ) ) ;
#22589 = CARTESIAN_POINT ( 'NONE',  ( 71.23944111523938716, 1.270877794983130027, -60.72281693841739525 ) ) ;
#22590 = CARTESIAN_POINT ( 'NONE',  ( 11.13393739769619906, 31.88305279702909800, -43.91250110351749925 ) ) ;
#22591 = DIRECTION ( 'NONE',  ( 1.000000000000000000, 0.000000000000000000, 0.000000000000000000 ) ) ;
#22592 = AXIS2_PLACEMENT_3D ( 'NONE', #43819, #11341, #23352 ) ;
#22593 = CARTESIAN_POINT ( 'NONE',  ( 66.50409435687238613, -33.11595941302709889, -20.28080645395380088 ) ) ;
#22594 = CARTESIAN_POINT ( 'NONE',  ( 18.66237858775300040, 20.19926697308340380, -74.35527526576579760 ) ) ;
#22595 = EDGE_LOOP ( 'NONE', ( #3890, #26916, #9239, #33742 ) ) ;
#22596 = ORIENTED_EDGE ( 'NONE', *, *, #12964, .F. ) ;
#22597 = CARTESIAN_POINT ( 'NONE',  ( 14.13393739769640156, 10.38381105532060111, -54.64999999999999858 ) ) ;
#22598 = CARTESIAN_POINT ( 'NONE',  ( 49.06135853991354168, -2.772563640123296924, -15.65933779184700647 ) ) ;
#22599 = ORIENTED_EDGE ( 'NONE', *, *, #9038, .F. ) ;
#22600 = EDGE_CURVE ( 'NONE', #49606, #28015, #8579, .T. ) ;
#22601 = CARTESIAN_POINT ( 'NONE',  ( 11.52518891765600095, -64.75101289998659126, -45.36825986196159732 ) ) ;
#22602 = CARTESIAN_POINT ( 'NONE',  ( 55.99739780941779799, -45.92760302930049932, -25.73393128425269794 ) ) ;
#22603 = DIRECTION ( 'NONE',  ( 0.000000000000000000, 0.000000000000000000, 1.000000000000000000 ) ) ;
#22604 = DIRECTION ( 'NONE',  ( -0.8732394366197182567, 0.4872913772396111343, -1.665334536937735304E-16 ) ) ;
#22605 = VERTEX_POINT ( 'NONE', #5741 ) ;
#22606 = CARTESIAN_POINT ( 'NONE',  ( 11.63938621547738705, 34.14834037275974055, -22.50902133189791243 ) ) ;
#22607 = CARTESIAN_POINT ( 'NONE',  ( 46.27121035923033077, 6.948460380232488021, -58.96360570400401713 ) ) ;
#22608 = CARTESIAN_POINT ( 'NONE',  ( 43.46647314489950276, -45.04259908834720250, -6.433232421327499395 ) ) ;
#22609 = ORIENTED_EDGE ( 'NONE', *, *, #30208, .F. ) ;
#22610 = CARTESIAN_POINT ( 'NONE',  ( 9.369669958260699261, -20.33077770372739934, -32.59857632693769602 ) ) ;
#22611 = CARTESIAN_POINT ( 'NONE',  ( 0.3209249304026170480, -15.61618894467929941, -35.14999999999999858 ) ) ;
#22612 = FACE_OUTER_BOUND ( 'NONE', #46771, .T. ) ;
#22613 = B_SPLINE_CURVE_WITH_KNOTS ( 'NONE', 3,
 ( #6158, #25001, #5129, #21085, #37086 ),
 .UNSPECIFIED., .F., .F.,
 ( 4, 1, 4 ),
 ( 0.000000000000000000, 0.3333435241872368393, 0.5000152864445784884 ),
 .UNSPECIFIED. ) ;
#22614 = VECTOR ( 'NONE', #25321, 1000.000000000000000 ) ;
#22615 = CARTESIAN_POINT ( 'NONE',  ( 16.41974898881801082, -22.37754970791813136, -46.93937931256282070 ) ) ;
#22616 = CARTESIAN_POINT ( 'NONE',  ( 14.55219274796575313, 20.46959765477225091, -75.56421372419544014 ) ) ;
#22617 = CARTESIAN_POINT ( 'NONE',  ( 46.72272053391589708, -53.55196115563460779, -76.01521976086429788 ) ) ;
#22618 = CARTESIAN_POINT ( 'NONE',  ( 60.86286082204030379, 12.20400039278949933, -9.318368423349330243 ) ) ;
#22619 = EDGE_CURVE ( 'NONE', #26354, #13074, #17027, .T. ) ;
#22620 = DIRECTION ( 'NONE',  ( 0.000000000000000000, -1.000000000000000000, 0.000000000000000000 ) ) ;
#22621 = AXIS2_PLACEMENT_3D ( 'NONE', #43646, #35253, #51254 ) ;
#22622 = AXIS2_PLACEMENT_3D ( 'NONE', #38806, #35107, #18867 ) ;
#22623 = VECTOR ( 'NONE', #28821, 1000.000000000000000 ) ;
#22624 = DIRECTION ( 'NONE',  ( 0.05643417272666774454, -0.04100182651872442269, -0.9975640502598241977 ) ) ;
#22625 = CARTESIAN_POINT ( 'NONE',  ( 60.51496306430259864, 13.88379478767680020, -26.40814067861359860 ) ) ;
#22626 = AXIS2_PLACEMENT_3D ( 'NONE', #44598, #28861, #8447 ) ;
#22627 = VECTOR ( 'NONE', #40667, 1000.000000000000000 ) ;
#22628 = CARTESIAN_POINT ( 'NONE',  ( 18.50775712175209620, -7.720120979975890307, -33.10062717276339583 ) ) ;
#22629 = B_SPLINE_SURFACE_WITH_KNOTS ( 'NONE', 3, 3, ( 
 ( #37395, #13555, #21641, #30288, #33702, #45523, #37914, #2007, #29763, #17989, #45783, #41842, #49971, #14063, #46048, #42101 ),
 ( #6206, #22160, #34733, #27901, #50993, #35524, #35782, #47589, #23186, #7490, #3820, #34993, #15614, #31569, #42886, #10915 ),
 ( #15096, #51260, #30798, #43653, #19793, #7754, #31058, #23703, #51516, #47083, #35263, #11683, #11432, #27650, #39717, #3564 ),
 ( #23443, #51766, #38696, #31312, #15865, #31825, #47841, #18759, #6980, #19535, #3045, #11945, #43143, #7238, #6724, #39202 ),
 ( #11173, #38954, #22680, #27138, #47337, #3298, #2788, #50737, #14836, #46826, #19280, #26877, #22934, #19017, #15356, #39465 ),
 ( #27394, #43395, #40482, #36541, #12194, #139, #37073, #48353, #1171, #8255, #32584, #48880, #23952, #49147, #12985, #16114 ),
 ( #41003, #44940, #391, #40232, #33119, #13244, #32077, #8522, #20289, #4067, #24987, #8779, #12718, #28672, #43906, #48095 ),
 ( #40744, #24469, #7999, #28935, #20546, #9041, #4322, #39975, #20033, #28154, #16375, #36031, #5119, #21071, #36280, #32332 ),
 ( #44158, #24203, #12446, #28413, #44420, #16906, #4574, #648, #32848, #16631, #48619, #44676, #24729, #20811, #36801, #911 ) ),
 .UNSPECIFIED., .F., .F., .F.,
 ( 4, 1, 1, 1, 1, 1, 4 ),
 ( 4, 2, 2, 2, 2, 2, 2, 4 ),
 ( 0.000000000000000000, 0.1666666666666670182, 0.3333333333333329818, 0.5000000000000000000, 0.6666666666666670737, 0.8333333333333330373, 1.000000003372510049 ),
 ( -11.88254149278500016, -9.803096731538550657, -7.426588432971120035, -5.941270746366480004, -5.198611903064159989, -4.010357753780449563, -2.109151114926509862, 3.424587999999999838E-09 ),
 .UNSPECIFIED. ) ;
#22630 = ORIENTED_EDGE ( 'NONE', *, *, #37984, .F. ) ;
#22631 = LINE ( 'NONE', #25776, #51449 ) ;
#22632 = CARTESIAN_POINT ( 'NONE',  ( -8.120841049443690451, -43.88478719140770323, -4.398687954041819559 ) ) ;
#22633 = CARTESIAN_POINT ( 'NONE',  ( 75.26680305930699433, -18.74898951345290143, -11.37374796283529932 ) ) ;
#22634 = CARTESIAN_POINT ( 'NONE',  ( 75.11664760679863662, 13.76739462715691431, -14.66476025242160475 ) ) ;
#22635 = CARTESIAN_POINT ( 'NONE',  ( 16.13393739769620083, -15.61618894467929941, -20.15000000000000213 ) ) ;
#22636 = FACE_OUTER_BOUND ( 'NONE', #18854, .T. ) ;
#22637 = CARTESIAN_POINT ( 'NONE',  ( 82.13853704237929776, -45.12072225811939319, -46.53690974066719832 ) ) ;
#22638 = CARTESIAN_POINT ( 'NONE',  ( 16.13393739769620083, -15.61618894467929941, -20.65000000000000213 ) ) ;
#22639 = CARTESIAN_POINT ( 'NONE',  ( 42.63139190005710333, 11.62219417602310045, -3.312314667585950279 ) ) ;
#22640 = EDGE_CURVE ( 'NONE', #13029, #10507, #41125, .T. ) ;
#22641 = FACE_OUTER_BOUND ( 'NONE', #47944, .T. ) ;
#22642 = CARTESIAN_POINT ( 'NONE',  ( 9.894687805641389389, -53.60726374558549878, -34.64999999999999858 ) ) ;
#22643 = CARTESIAN_POINT ( 'NONE',  ( 68.13393739769847457, -50.70395984888145335, -72.15645085170113759 ) ) ;
#22644 = CARTESIAN_POINT ( 'NONE',  ( 22.04684669439291156, -19.02418497068438796, -62.61948962174666633 ) ) ;
#22645 = CARTESIAN_POINT ( 'NONE',  ( 17.93348425303889826, -51.26614876191910497, -74.93568190818520236 ) ) ;
#22646 = CARTESIAN_POINT ( 'NONE',  ( 44.88192221582870189, -45.11618894467940066, -7.000245857760280188 ) ) ;
#22647 = VERTEX_POINT ( 'NONE', #33505 ) ;
#22648 = CARTESIAN_POINT ( 'NONE',  ( 9.366197046019539840, -18.73137511417689893, -49.93002833933049800 ) ) ;
#22649 = CARTESIAN_POINT ( 'NONE',  ( 63.72368862820488999, 1.434949534324519993, -62.02708488646099738 ) ) ;
#22650 = ORIENTED_EDGE ( 'NONE', *, *, #9804, .T. ) ;
#22651 = CARTESIAN_POINT ( 'NONE',  ( 2.404741263826560171, -25.85214510508460251, -35.14999999999999858 ) ) ;
#22652 = CARTESIAN_POINT ( 'NONE',  ( 60.62539537963969849, -45.77966094345969594, -47.75584023230200614 ) ) ;
#22653 = CARTESIAN_POINT ( 'NONE',  ( 73.13312216970089708, 0.9955677559369568996, -68.95442834019429768 ) ) ;
#22654 = CARTESIAN_POINT ( 'NONE',  ( 45.81506188687751546, 8.850597565810659262, -57.85721284573491374 ) ) ;
#22655 = CARTESIAN_POINT ( 'NONE',  ( 9.700417070101229555, -18.19071222218930117, -81.23899999999999011 ) ) ;
#22656 = CARTESIAN_POINT ( 'NONE',  ( 41.33278336659260077, -45.54329717826499291, -6.226146794320340128 ) ) ;
#22657 = ORIENTED_EDGE ( 'NONE', *, *, #44404, .F. ) ;
#22658 = EDGE_LOOP ( 'NONE', ( #21045, #3535, #23843, #36577, #10120, #50654 ) ) ;
#22659 = VERTEX_POINT ( 'NONE', #44799 ) ;
#22660 = DIRECTION ( 'NONE',  ( 0.06889765579810419593, 0.01091231665325485996, -0.9975640502598241977 ) ) ;
#22661 = CARTESIAN_POINT ( 'NONE',  ( 61.34010690585019887, -45.20347833372960622, -46.45024392112279799 ) ) ;
#22662 = CARTESIAN_POINT ( 'NONE',  ( 82.45630311851421368, -45.09271792554360303, -46.38988467804559690 ) ) ;
#22663 = AXIS2_PLACEMENT_3D ( 'NONE', #46830, #3049, #42104 ) ;
#22664 = ORIENTED_EDGE ( 'NONE', *, *, #26228, .F. ) ;
#22665 = CIRCLE ( 'NONE', #40228, 2.999999999999994227 ) ;
#22666 = DIRECTION ( 'NONE',  ( 0.000000000000000000, 0.000000000000000000, -1.000000000000000000 ) ) ;
#22667 = ORIENTED_EDGE ( 'NONE', *, *, #29431, .T. ) ;
#22668 = LINE ( 'NONE', #43645, #43663 ) ;
#22669 = CARTESIAN_POINT ( 'NONE',  ( 45.14919548887390022, -33.29386571476810275, -35.12503119152809461 ) ) ;
#22670 = EDGE_LOOP ( 'NONE', ( #47062, #15966, #39502, #31317 ) ) ;
#22671 = CARTESIAN_POINT ( 'NONE',  ( 31.10075179363273179, -4.742161777268546707, 7.849999999999997868 ) ) ;
#22672 = CARTESIAN_POINT ( 'NONE',  ( 52.82839229275239745, -51.22091222732959892, -75.91621971673269798 ) ) ;
#22673 = CARTESIAN_POINT ( 'NONE',  ( 60.95425169575680258, 14.19472640642180039, -47.19051797104440027 ) ) ;
#22674 = EDGE_CURVE ( 'NONE', #23933, #23138, #6000, .T. ) ;
#22675 = EDGE_CURVE ( 'NONE', #38928, #21370, #20291, .T. ) ;
#22676 = DIRECTION ( 'NONE',  ( 0.000000000000000000, 1.000000000000000000, 0.000000000000000000 ) ) ;
#22677 = CARTESIAN_POINT ( 'NONE',  ( 40.75026606626570214, -44.57835314504790603, -4.220911785948969985 ) ) ;
#22678 = EDGE_CURVE ( 'NONE', #7583, #47128, #5491, .T. ) ;
#22679 = DIRECTION ( 'NONE',  ( 0.000000000000000000, 0.000000000000000000, 1.000000000000000000 ) ) ;
#22680 = CARTESIAN_POINT ( 'NONE',  ( -10.43316342469580071, 11.56352937203230091, -6.076102107692801013 ) ) ;
#22681 = CARTESIAN_POINT ( 'NONE',  ( 64.74323834027589442, 1.229084191802189974, -70.46414972969270707 ) ) ;
#22682 = CARTESIAN_POINT ( 'NONE',  ( 22.65728558640282131, -17.99966492201340529, -38.95926740740573990 ) ) ;
#22683 = CARTESIAN_POINT ( 'NONE',  ( 17.92370450360863998, -51.11618894467903118, -74.34716300802168121 ) ) ;
#22684 = CARTESIAN_POINT ( 'NONE',  ( 12.24155400994649945, -22.43059278844679838, -53.95269993303519840 ) ) ;
#22685 = EDGE_LOOP ( 'NONE', ( #15901, #50402, #36607, #41105, #50062 ) ) ;
#22686 = CARTESIAN_POINT ( 'NONE',  ( 14.89313683410190059, -52.76520172820870158, -76.12661215459480957 ) ) ;
#22687 = DIRECTION ( 'NONE',  ( 0.5720614028176826960, 0.4156269377774550189, 0.7071067811865479058 ) ) ;
#22688 = UNCERTAINTY_MEASURE_WITH_UNIT (LENGTH_MEASURE( 1.000000000000000082E-05 ), #24338, 'distance_accuracy_value', 'NONE');
#22689 = CARTESIAN_POINT ( 'NONE',  ( 71.45220707235199598, 1.395841836298969962, -70.23186791216220115 ) ) ;
#22690 = CARTESIAN_POINT ( 'NONE',  ( 45.46288062967357746, -40.06128974838797774, -59.56694921511265761 ) ) ;
#22691 = DIRECTION ( 'NONE',  ( 0.000000000000000000, 0.000000000000000000, -1.000000000000000000 ) ) ;
#22692 = VECTOR ( 'NONE', #28245, 1000.000000000000000 ) ;
#22693 = CARTESIAN_POINT ( 'NONE',  ( 11.13393739769619906, 32.28996932333459569, -43.76018303787720498 ) ) ;
#22694 = AXIS2_PLACEMENT_3D ( 'NONE', #39571, #40084, #19646 ) ;
#22695 = EDGE_CURVE ( 'NONE', #8205, #18792, #9443, .T. ) ;
#22696 = CARTESIAN_POINT ( 'NONE',  ( 63.32276749867028798, 1.263823323415670163, -68.97683676677020514 ) ) ;
#22697 = CARTESIAN_POINT ( 'NONE',  ( 47.83873146774000418, -54.45004056421520033, -55.16375355595400265 ) ) ;
#22698 = FACE_OUTER_BOUND ( 'NONE', #37685, .T. ) ;
#22699 = DIRECTION ( 'NONE',  ( -0.5516667872527389882, -0.8340645993220436871, 8.326672684688667890E-17 ) ) ;
#22700 = CARTESIAN_POINT ( 'NONE',  ( 47.71207051903009955, 23.26369402866030001, -54.98518041347200125 ) ) ;
#22701 = EDGE_LOOP ( 'NONE', ( #5980, #15150, #22353, #35440, #5738, #32644 ) ) ;
#22702 = CARTESIAN_POINT ( 'NONE',  ( 20.25033824699210072, -9.889252315854481168, -78.54555634383710583 ) ) ;
#22703 = B_SPLINE_CURVE_WITH_KNOTS ( 'NONE', 3,
 ( #24796, #21135, #16975, #40803, #32920, #21901, #21389, #41578, #2006, #1236, #41841, #37394, #37913, #33446, #17226, #49206, #17988, #29259, #1496, #25053 ),
 .UNSPECIFIED., .F., .F.,
 ( 4, 2, 2, 2, 2, 2, 2, 2, 2, 4 ),
 ( -1.826192301619909975, -1.710015269444949970, -1.458000257333699867, -1.209852399823190039, -1.027233169661200041, -0.9130961508099529889, -0.6848221131074649914, -0.4130753771364510385, -0.1614840352283428704, 0.000000000000000000 ),
 .UNSPECIFIED. ) ;
#22704 = EDGE_LOOP ( 'NONE', ( #33175, #7710, #21397, #22086 ) ) ;
#22705 = CARTESIAN_POINT ( 'NONE',  ( 71.29701819511369365, 1.369719003397489976, -70.35226930031730319 ) ) ;
#22706 = DIRECTION ( 'NONE',  ( 0.000000000000000000, 1.000000000000000000, 0.000000000000000000 ) ) ;
#22707 = DIRECTION ( 'NONE',  ( 0.05023550054956202326, 0.000000000000000000, 0.9987374001630934250 ) ) ;
#22709 = FACE_OUTER_BOUND ( 'NONE', #1346, .T. ) ;
#22708 = CARTESIAN_POINT ( 'NONE',  ( 83.67079303953970282, 13.80909354995310068, -47.45584445533860674 ) ) ;
#22710 = CARTESIAN_POINT ( 'NONE',  ( 10.33272111206849964, -19.62722883991240153, -79.65462137872758319 ) ) ;
#22711 = CARTESIAN_POINT ( 'NONE',  ( 71.48855272380090753, 0.8936201581567910779, -70.62461353540280129 ) ) ;
#22712 = DIRECTION ( 'NONE',  ( 1.000000000000000000, 0.000000000000000000, 0.000000000000000000 ) ) ;
#22713 = ORIENTED_EDGE ( 'NONE', *, *, #16678, .F. ) ;
#22714 = CARTESIAN_POINT ( 'NONE',  ( 53.63393739769619373, 31.88381105532059934, 16.35000000000000142 ) ) ;
#22715 = ORIENTED_EDGE ( 'NONE', *, *, #16241, .F. ) ;
#22716 = ORIENTED_EDGE ( 'NONE', *, *, #35690, .T. ) ;
#22717 = CARTESIAN_POINT ( 'NONE',  ( 11.89829296289419958, -64.83233913608019350, -16.17105426249170108 ) ) ;
#22718 = DIRECTION ( 'NONE',  ( 3.281478866952075176E-28, -2.435884827299240233E-11, -1.000000000000000000 ) ) ;
#22719 = CARTESIAN_POINT ( 'NONE',  ( 76.45177665192957761, -25.09083072484978416, -13.01961666583026300 ) ) ;
#22720 = CARTESIAN_POINT ( 'NONE',  ( 9.367149180512809536, -63.29633625153390142, -46.50590274669379909 ) ) ;
#22721 = EDGE_LOOP ( 'NONE', ( #7678, #1218, #42922, #4449 ) ) ;
#22722 = ORIENTED_EDGE ( 'NONE', *, *, #39030, .T. ) ;
#22723 = CARTESIAN_POINT ( 'NONE',  ( 22.13393739769619728, -54.15188668067469990, -35.14999999999999858 ) ) ;
#22724 = CARTESIAN_POINT ( 'NONE',  ( 52.86576716034980450, 18.31963347231479844, -48.38645722914640146 ) ) ;
#22725 = CARTESIAN_POINT ( 'NONE',  ( 61.27130757359800128, -0.5767551585763339705, -16.33740500793329886 ) ) ;
#22726 = CARTESIAN_POINT ( 'NONE',  ( 51.79630867582309861, -49.28713043378009218, -76.98491571383419796 ) ) ;
#22727 = CARTESIAN_POINT ( 'NONE',  ( 57.01128662093320543, -50.56557199667180669, -53.09478151126450030 ) ) ;
#22728 = VECTOR ( 'NONE', #32597, 1000.000000000000000 ) ;
#22729 = ORIENTED_EDGE ( 'NONE', *, *, #27017, .F. ) ;
#22730 = CARTESIAN_POINT ( 'NONE',  ( 52.61990787174079998, -49.80354421666690001, -27.74322489265389891 ) ) ;
#22732 = CARTESIAN_POINT ( 'NONE',  ( -6.866062602303790285, -15.61618894467929941, -59.64999999999999147 ) ) ;
#22731 = AXIS2_PLACEMENT_3D ( 'NONE', #43308, #3472, #15771 ) ;
#22733 = ORIENTED_EDGE ( 'NONE', *, *, #43387, .F. ) ;
#22734 = CARTESIAN_POINT ( 'NONE',  ( 29.13393466042962032, -26.74790781212725221, -35.10904485683931142 ) ) ;
#22735 = DIRECTION ( 'NONE',  ( 0.4999999999999998890, 0.8660254037844387076, 0.000000000000000000 ) ) ;
#22736 = AXIS2_PLACEMENT_3D ( 'NONE', #24003, #44988, #40280 ) ;
#22737 = CARTESIAN_POINT ( 'NONE',  ( 19.46890126474820093, -8.512333400185202237, -45.65220606189509311 ) ) ;
#22738 = EDGE_CURVE ( 'NONE', #16397, #47254, #11125, .T. ) ;
#22739 = CARTESIAN_POINT ( 'NONE',  ( 13.67288539103119938, -51.17054487835680021, -22.23396216461150132 ) ) ;
#22740 = CARTESIAN_POINT ( 'NONE',  ( 47.32111516514439842, -54.12775347911220081, -75.47461153638509757 ) ) ;
#22741 = ADVANCED_FACE ( 'NONE', ( #45057 ), #29571, .F. ) ;
#22742 = CARTESIAN_POINT ( 'NONE',  ( 56.17414541250489890, 14.05430885410310005, -16.17612370156109947 ) ) ;
#22743 = CARTESIAN_POINT ( 'NONE',  ( 9.543082594814544350, -13.84487447432519680, -77.53615328806994000 ) ) ;
#22744 = CARTESIAN_POINT ( 'NONE',  ( 71.03155062328740144, 1.383928098097870096, -70.33743540642140601 ) ) ;
#22745 = CARTESIAN_POINT ( 'NONE',  ( 11.25287529172470080, -20.70714090792739981, -45.59048102137129632 ) ) ;
#22746 = CARTESIAN_POINT ( 'NONE',  ( 19.54188575374945813, -9.703251766430753378, -44.11945704888728415 ) ) ;
#22747 = ORIENTED_EDGE ( 'NONE', *, *, #25494, .T. ) ;
#22748 = CARTESIAN_POINT ( 'NONE',  ( 47.57129143639170366, 23.33298354540060160, -74.19756735440549278 ) ) ;
#22749 = CARTESIAN_POINT ( 'NONE',  ( 65.13185782384009315, 1.385888765344509999, -60.99577487439199786 ) ) ;
#22750 =( REPRESENTATION_RELATIONSHIP ('NONE','NONE', #29764, #49550 ) REPRESENTATION_RELATIONSHIP_WITH_TRANSFORMATION ( #51640 )SHAPE_REPRESENTATION_RELATIONSHIP( ) );
#22751 = CARTESIAN_POINT ( 'NONE',  ( 15.09847552854969344, -7.705178599813004681, -50.96600048343916001 ) ) ;
#22752 = CARTESIAN_POINT ( 'NONE',  ( 30.68460988201149320, -15.41618894468070344, -28.20067248431509199 ) ) ;
#22753 = CARTESIAN_POINT ( 'NONE',  ( 8.787528872100399013, -49.03431820457670653, -34.71551406240349280 ) ) ;
#22754 = CARTESIAN_POINT ( 'NONE',  ( 14.63393739769620083, -32.15793020853440254, -34.64999999999999858 ) ) ;
#22755 = ADVANCED_FACE ( 'NONE', ( #17785 ), #33758, .T. ) ;
#22756 = CARTESIAN_POINT ( 'NONE',  ( 82.13853704237929776, 13.90869809199659990, -46.70066698695239893 ) ) ;
#22757 = CARTESIAN_POINT ( 'NONE',  ( -18.31222503402669943, 3.035017555580589832, -50.71178994223060243 ) ) ;
#22758 = CARTESIAN_POINT ( 'NONE',  ( 8.223605785152290792, -15.61620117245469963, -52.50766849176299900 ) ) ;
#22759 = EDGE_CURVE ( 'NONE', #21433, #17657, #26136, .T. ) ;
#22760 = CARTESIAN_POINT ( 'NONE',  ( 8.887019836252781246, -18.85787674178415330, -32.65851392028359612 ) ) ;
#22761 = CARTESIAN_POINT ( 'NONE',  ( -29.08731580419370033, 4.375077605369980027, -55.16774717297709429 ) ) ;
#22762 = VERTEX_POINT ( 'NONE', #46106 ) ;
#22763 = AXIS2_PLACEMENT_3D ( 'NONE', #23741, #35564, #8295 ) ;
#22764 = CARTESIAN_POINT ( 'NONE',  ( 52.93241479646199821, -49.61258791452640082, -48.85493845497290266 ) ) ;
#22765 = AXIS2_PLACEMENT_3D ( 'NONE', #28837, #14609, #42397 ) ;
#22766 = ORIENTED_EDGE ( 'NONE', *, *, #17451, .F. ) ;
#22767 = CARTESIAN_POINT ( 'NONE',  ( 47.23800599814349255, 8.041507069165529487, -54.67567028232367932 ) ) ;
#22768 = CARTESIAN_POINT ( 'NONE',  ( 15.24823002788296122, -8.849177966009543539, -41.91115328570175080 ) ) ;
#22769 = CARTESIAN_POINT ( 'NONE',  ( 14.13581725382830001, 19.88180066538970081, -22.31751565788919933 ) ) ;
#22770 = CARTESIAN_POINT ( 'NONE',  ( 53.63393739769619373, 21.88381105532059934, 17.35000000000000142 ) ) ;
#22771 = CARTESIAN_POINT ( 'NONE',  ( 12.40804001521799904, -9.627846319890059235, -45.77565614294249485 ) ) ;
#22772 = CARTESIAN_POINT ( 'NONE',  ( 52.59421258935810073, 18.59942272400250118, -48.47378032971769812 ) ) ;
#22773 = CARTESIAN_POINT ( 'NONE',  ( 55.82670324262860362, -45.92590652002289886, -17.31876773537310044 ) ) ;
#22774 = CARTESIAN_POINT ( 'NONE',  ( 14.34417029198830029, 19.88381105532299742, -74.14999999999999147 ) ) ;
#22775 = ORIENTED_EDGE ( 'NONE', *, *, #31874, .F. ) ;
#22776 = CARTESIAN_POINT ( 'NONE',  ( 9.028267923962127739, -18.94728626226500268, -34.14796716713029667 ) ) ;
#22777 = ORIENTED_EDGE ( 'NONE', *, *, #39766, .T. ) ;
#22778 = CARTESIAN_POINT ( 'NONE',  ( 60.05889968639040433, 14.78467075934760011, -47.76686567462839861 ) ) ;
#22779 = CARTESIAN_POINT ( 'NONE',  ( 10.97012820795380073, 33.88053142178789301, -47.22757037167239957 ) ) ;
#22780 = CARTESIAN_POINT ( 'NONE',  ( 73.04443511092439678, 0.9036513197889520788, -62.20214363597960272 ) ) ;
#22781 = CARTESIAN_POINT ( 'NONE',  ( 56.46551567295650642, 19.54378694285259854, -74.14999999999999147 ) ) ;
#22782 = LINE ( 'NONE', #6309, #13767 ) ;
#22783 = FACE_OUTER_BOUND ( 'NONE', #18621, .T. ) ;
#22784 = CARTESIAN_POINT ( 'NONE',  ( 23.83903608302206223, -13.54550562940452352, -45.70899248858425779 ) ) ;
#22785 = CARTESIAN_POINT ( 'NONE',  ( 49.40539548389180879, -53.49785366681999932, -54.15746054660920095 ) ) ;
#22786 = ORIENTED_EDGE ( 'NONE', *, *, #12029, .F. ) ;
#22787 = CARTESIAN_POINT ( 'NONE',  ( 64.72196861157999592, 1.188860127980290171, -70.48451794758260291 ) ) ;
#22788 = ORIENTED_EDGE ( 'NONE', *, *, #8515, .F. ) ;
#22789 = CARTESIAN_POINT ( 'NONE',  ( 10.77178238407419997, -63.25331191240289286, -45.20468163478559376 ) ) ;
#22790 = DIRECTION ( 'NONE',  ( -1.000000000000000000, 0.000000000000000000, 0.000000000000000000 ) ) ;
#22791 = ORIENTED_EDGE ( 'NONE', *, *, #14250, .F. ) ;
#22792 = DIRECTION ( 'NONE',  ( 0.000000000000000000, 0.000000000000000000, -1.000000000000000000 ) ) ;
#22793 = CARTESIAN_POINT ( 'NONE',  ( 57.34583854495710398, 19.00625385608790197, -52.73888232642729434 ) ) ;
#22794 = CARTESIAN_POINT ( 'NONE',  ( 52.84397956633110027, 19.27108008843849873, -76.72969847962329482 ) ) ;
#22795 = ORIENTED_EDGE ( 'NONE', *, *, #22802, .T. ) ;
#22796 = CARTESIAN_POINT ( 'NONE',  ( 9.374134760172621483, -64.20245714614587484, -46.81441715244631041 ) ) ;
#22797 = B_SPLINE_SURFACE_WITH_KNOTS ( 'NONE', 3, 3, ( 
 ( #44402, #36011, #39958, #8239, #35511, #3806, #126, #27379, #16100, #15600, #24190, #7478, #375, #47574, #16356, #28397 ),
 ( #23427, #39450, #3550, #31553, #27634, #43639, #4824, #13482, #21569, #48858, #44922, #1415, #9023, #37565, #17401, #29440 ),
 ( #12700, #49129, #24967, #12965, #892, #40986, #5099, #5615, #21053, #41245, #20792, #48599, #36785, #49386, #16887, #13228 ),
 ( #1674, #9547, #37054, #25498, #21312, #41501, #33368, #1150, #32832, #45445, #17661, #28653, #33099, #16611, #17147, #5357 ),
 ( #29177, #37313, #45180, #28916, #32569, #44656, #8762, #24711, #25240, #40728, #9293, #12598, #19928, #7894, #20691, #32731 ),
 ( #28042, #39863, #280, #35920, #27537, #36681, #3965, #35, #20436, #31968, #785, #36423, #28560, #16516, #23588, #16264 ),
 ( #16010, #43793, #47989, #12088, #16784, #44047, #44301, #31708, #43543, #47732, #32465, #23840, #32217, #24615, #4726, #8660 ),
 ( #40626, #40369, #11575, #530, #8150, #11837, #48495, #7643, #39606, #20182, #44561, #24094, #28296, #40117, #4210, #8409 ),
 ( #24355, #36172, #3710, #19678, #27797, #35675, #4466, #48241, #51661, #12335, #15754, #48762, #44823, #29845, #29342, #49544 ),
 ( #12866, #6025, #13383, #5763, #13886, #36953, #45344, #49027, #21728, #1571, #25141, #49794, #9697, #21473, #29595, #13636 ),
 ( #17563, #45600, #33531, #25658, #9449, #9189, #21985, #25914, #45866, #9949, #20957, #41660, #41927, #37473, #37734, #18069 ) ),
 .UNSPECIFIED., .F., .F., .F.,
 ( 4, 1, 1, 1, 1, 1, 1, 1, 4 ),
 ( 4, 2, 2, 2, 2, 2, 2, 4 ),
 ( -1.411926611000000059E-06, 0.1250000000000000000, 0.2500000000000000000, 0.3750000000000000000, 0.5000000000000000000, 0.6250000000000000000, 0.7500000000000000000, 0.8750000000000000000, 1.000010174520270079 ),
 ( -0.5134457415475799369, -0.4235843427975279907, -0.3208972293920659968, -0.2567177835136529862, -0.2246280605744469805, -0.1732845038717159836, -0.09113481314734700467, 1.017452027400000023E-05 ),
 .UNSPECIFIED. ) ;
#22798 = CARTESIAN_POINT ( 'NONE',  ( 50.97251424797730124, 19.73188950824126309, -76.14992187212315855 ) ) ;
#22799 = DIRECTION ( 'NONE',  ( 1.000000000000000000, 0.000000000000000000, 0.000000000000000000 ) ) ;
#22800 = CARTESIAN_POINT ( 'NONE',  ( 57.24929578232330130, -50.61618894764249887, -53.91492796143979405 ) ) ;
#22801 = CARTESIAN_POINT ( 'NONE',  ( 22.20375567613890055, -21.19651385660140264, -66.02896523578519350 ) ) ;
#22802 = EDGE_CURVE ( 'NONE', #19884, #19952, #42234, .T. ) ;
#22803 = CARTESIAN_POINT ( 'NONE',  ( 23.83903869581317991, -17.68685937611830283, -47.59100309625389258 ) ) ;
#22804 = CARTESIAN_POINT ( 'NONE',  ( 46.77958021070534045, -38.22981356621252758, -56.42173487551926314 ) ) ;
#22805 = ORIENTED_EDGE ( 'NONE', *, *, #24807, .T. ) ;
#22806 = B_SPLINE_CURVE_WITH_KNOTS ( 'NONE', 3,
 ( #42585, #9832, #6681, #41794, #1966, #14281, #17943, #29979, #10616, #22642 ),
 .UNSPECIFIED., .F., .F.,
 ( 4, 2, 2, 2, 4 ),
 ( 0.1272047750358668849, 0.1420319546175010106, 0.1570382458081870103, 0.1723372614084489884, 0.1727139781544710095 ),
 .UNSPECIFIED. ) ;
#22807 = EDGE_LOOP ( 'NONE', ( #49094, #22281, #5670, #30524 ) ) ;
#22808 = DIRECTION ( 'NONE',  ( 0.000000000000000000, 1.000000000000000000, 0.000000000000000000 ) ) ;
#22809 = CARTESIAN_POINT ( 'NONE',  ( 14.46478753480960044, -22.87708644708019889, -56.80458145132549674 ) ) ;
#22810 = TOROIDAL_SURFACE ( 'NONE', #29509, 32.00000000000000000, 1.000000000000000000 ) ;
#22811 = CARTESIAN_POINT ( 'NONE',  ( 53.51283228710530437, -49.43204137189339775, -49.22146279461640006 ) ) ;
#22812 = CARTESIAN_POINT ( 'NONE',  ( 9.738742532837820320, -12.64405718765570086, -32.14999999999999858 ) ) ;
#22813 = DIRECTION ( 'NONE',  ( 0.000000000000000000, 0.000000000000000000, -1.000000000000000000 ) ) ;
#22814 = CARTESIAN_POINT ( 'NONE',  ( -0.007164427059776000244, 14.47565373231149977, -34.77269723891829756 ) ) ;
#22815 = DIRECTION ( 'NONE',  ( -1.000000000000000000, 0.000000000000000000, 0.000000000000000000 ) ) ;
#22816 = DIRECTION ( 'NONE',  ( 0.8660254037844383745, -0.5000000000000003331, -2.775557561562891844E-16 ) ) ;
#22817 = CARTESIAN_POINT ( 'NONE',  ( 10.01530563823780007, -21.14294804030860320, -68.27383256501039455 ) ) ;
#22818 = CARTESIAN_POINT ( 'NONE',  ( 53.00983118628400348, -49.38275580526859443, -27.01103834705430273 ) ) ;
#22819 = AXIS2_PLACEMENT_3D ( 'NONE', #24892, #44064, #12352 ) ;
#22820 = CARTESIAN_POINT ( 'NONE',  ( 55.56519842082970229, -50.87569675573109862, -75.15977926761300409 ) ) ;
#22822 = DIRECTION ( 'NONE',  ( -1.000000000000000000, 0.000000000000000000, 0.000000000000000000 ) ) ;
#22821 = CARTESIAN_POINT ( 'NONE',  ( -10.13547705207719929, 11.41357116503390046, -5.029204105224179600 ) ) ;
#22824 = EDGE_CURVE ( 'NONE', #1802, #40665, #4068, .T. ) ;
#22823 = CARTESIAN_POINT ( 'NONE',  ( 47.61217947097659930, -54.50984741584490223, -54.68372563208449577 ) ) ;
#22825 = DIRECTION ( 'NONE',  ( 0.3294064756441309472, 0.9441882088883087887, 3.053113317719179500E-16 ) ) ;
#22826 = ORIENTED_EDGE ( 'NONE', *, *, #34759, .T. ) ;
#22827 = CARTESIAN_POINT ( 'NONE',  ( 52.83011299386760129, -49.66073358055960085, -48.49877547121819532 ) ) ;
#22828 = CARTESIAN_POINT ( 'NONE',  ( 47.58649647341519540, 23.31928261732160124, -54.89219699614270098 ) ) ;
#22829 = DIRECTION ( 'NONE',  ( -0.7071067811864684138, -0.7071067811866267316, 0.000000000000000000 ) ) ;
#22830 = CARTESIAN_POINT ( 'NONE',  ( 14.13393739769619906, -45.61618894467940066, -62.64999999999999858 ) ) ;
#22831 = CARTESIAN_POINT ( 'NONE',  ( 61.22425882976509826, 14.43492084046710033, -47.75784053982390276 ) ) ;
#22832 = CARTESIAN_POINT ( 'NONE',  ( 11.25424573356439950, 33.80288494388220499, -16.95782968490189901 ) ) ;
#22833 = CARTESIAN_POINT ( 'NONE',  ( 52.19989370126119610, 18.55847580453720269, -77.09681678487270062 ) ) ;
#22834 = CARTESIAN_POINT ( 'NONE',  ( 52.95585356374179042, 18.36289647769510225, -48.79473315328430516 ) ) ;
#22835 = DIRECTION ( 'NONE',  ( 1.882763000000000063E-17, 1.367908000000000040E-17, -1.000000000000000000 ) ) ;
#22836 = CARTESIAN_POINT ( 'NONE',  ( 55.68173555697770638, 17.70376283165290232, -53.85224183627919814 ) ) ;
#22837 = CARTESIAN_POINT ( 'NONE',  ( 52.77991141011769827, 18.45283218612549803, -28.02125929211980093 ) ) ;
#22838 = CARTESIAN_POINT ( 'NONE',  ( 49.72648160330989953, 22.41435850158119791, -55.11972614036179863 ) ) ;
#22839 = VECTOR ( 'NONE', #4731, 1000.000000000000114 ) ;
#22840 = CARTESIAN_POINT ( 'NONE',  ( 54.63655381128389621, -48.05296878824569973, -26.73577887340519865 ) ) ;
#22841 = CARTESIAN_POINT ( 'NONE',  ( 52.84346299185870066, 18.45884386080550144, -48.96941050064629763 ) ) ;
#22842 = DIRECTION ( 'NONE',  ( 1.000000000000000000, 0.000000000000000000, 0.000000000000000000 ) ) ;
#22843 = CARTESIAN_POINT ( 'NONE',  ( 71.25020460053529803, 1.328674444234389851, -60.82574149480920056 ) ) ;
#22844 = CARTESIAN_POINT ( 'NONE',  ( 10.48773063397930017, 31.94422603044110076, -45.62697307978170613 ) ) ;
#22845 = CIRCLE ( 'NONE', #17851, 2.500000000000000000 ) ;
#22846 = CARTESIAN_POINT ( 'NONE',  ( 17.49475172342960150, 19.88381105532299742, -15.67743212163030186 ) ) ;
#22847 = CARTESIAN_POINT ( 'NONE',  ( 66.62839972533728883, -32.95476632565599573, -19.40718689916469941 ) ) ;
#22848 = CARTESIAN_POINT ( 'NONE',  ( 9.458985575556051018, -14.34378805948378499, -65.51270995478979842 ) ) ;
#22849 = ORIENTED_EDGE ( 'NONE', *, *, #6985, .F. ) ;
#22850 = VERTEX_POINT ( 'NONE', #42427 ) ;
#22851 = CARTESIAN_POINT ( 'NONE',  ( 41.27829246776259708, 12.87545685813379848, -3.596739354799309840 ) ) ;
#22852 = CARTESIAN_POINT ( 'NONE',  ( 76.57339177411788000, 0.8951608601394540621, -13.54367431337692729 ) ) ;
#22853 = ORIENTED_EDGE ( 'NONE', *, *, #44786, .T. ) ;
#22854 = CARTESIAN_POINT ( 'NONE',  ( 11.36758345312349938, -64.52529782468211295, -45.06392959096150719 ) ) ;
#22855 = CARTESIAN_POINT ( 'NONE',  ( 56.78246058254009654, -45.33631709052220060, -25.70543994511969998 ) ) ;
#22856 = CARTESIAN_POINT ( 'NONE',  ( 21.09675763201389387, -21.77905901208185568, -77.79186885214345182 ) ) ;
#22857 = CARTESIAN_POINT ( 'NONE',  ( 12.08165187759344761, 24.17815767738823141, -22.62772784292297956 ) ) ;
#22858 = EDGE_LOOP ( 'NONE', ( #26855, #7795, #8307, #44017 ) ) ;
#22859 = CARTESIAN_POINT ( 'NONE',  ( 61.29923175484539399, -47.67319342919869740, -45.87705171400279625 ) ) ;
#22860 = CARTESIAN_POINT ( 'NONE',  ( 42.72578186200144756, 6.504558357780759970, -76.69071525042791393 ) ) ;
#22861 = CARTESIAN_POINT ( 'NONE',  ( 11.73100068668170159, 32.29067168418070111, -24.74706328898560059 ) ) ;
#22862 = ORIENTED_EDGE ( 'NONE', *, *, #35422, .F. ) ;
#22863 = CARTESIAN_POINT ( 'NONE',  ( 45.90332635223469993, -45.11618894461400231, -7.776724400097649870 ) ) ;
#22864 = VECTOR ( 'NONE', #608, 1000.000000000000114 ) ;
#22865 = ADVANCED_FACE ( 'NONE', ( #18561 ), #11228, .T. ) ;
#22866 = FACE_OUTER_BOUND ( 'NONE', #20390, .T. ) ;
#22867 = CARTESIAN_POINT ( 'NONE',  ( 16.44553025965459980, 19.88381305015400002, -20.85618808645970290 ) ) ;
#22868 = CARTESIAN_POINT ( 'NONE',  ( 21.60877393982859473, -19.65386968817948343, -50.65516752091996722 ) ) ;
#22869 = EDGE_CURVE ( 'NONE', #17592, #11419, #23625, .T. ) ;
#22870 = CARTESIAN_POINT ( 'NONE',  ( 60.15822031048740826, -28.97818250310960053, -15.79925957823600058 ) ) ;
#22871 = ADVANCED_FACE ( 'NONE', ( #51318 ), #6517, .T. ) ;
#22872 = CARTESIAN_POINT ( 'NONE',  ( 63.13746035244320609, 0.8910129994591539093, -62.32805707658469885 ) ) ;
#22873 = CARTESIAN_POINT ( 'NONE',  ( 46.76359541693670252, -53.62286661502929519, -75.98188598372340152 ) ) ;
#22874 = CARTESIAN_POINT ( 'NONE',  ( 44.96327775120639814, 13.88381306199719845, -7.018648154247789428 ) ) ;
#22875 = EDGE_CURVE ( 'NONE', #32305, #6769, #9092, .T. ) ;
#22876 = B_SPLINE_CURVE_WITH_KNOTS ( 'NONE', 3,
 ( #39255, #47390, #48866, #31108 ),
 .UNSPECIFIED., .F., .F.,
 ( 4, 4 ),
 ( 0.000000000000000000, 1.000000000000000000 ),
 .UNSPECIFIED. ) ;
#22877 = DIRECTION ( 'NONE',  ( 1.000000000000000000, 0.000000000000000000, 0.000000000000000000 ) ) ;
#22878 = AXIS2_PLACEMENT_3D ( 'NONE', #6434, #22393, #10628 ) ;
#22879 = CIRCLE ( 'NONE', #20367, 1.000000000000000888 ) ;
#22880 = ADVANCED_FACE ( 'NONE', ( #8062 ), #22810, .T. ) ;
#22881 = LINE ( 'NONE', #27339, #32347 ) ;
#22882 = CARTESIAN_POINT ( 'NONE',  ( 23.71320255129930032, -13.58133288703929864, -81.20401221892029753 ) ) ;
#22883 = EDGE_LOOP ( 'NONE', ( #47695, #7167, #33520, #1893, #50011, #33623 ) ) ;
#22884 = CARTESIAN_POINT ( 'NONE',  ( 3.987490788289478783, -8.603434725040944642, -34.79644660940672907 ) ) ;
#22885 = CARTESIAN_POINT ( 'NONE',  ( -6.046672580744979264, -47.40279481310589915, -7.123502465237989689 ) ) ;
#22886 = CARTESIAN_POINT ( 'NONE',  ( 75.29396857310361213, -8.410730295738069628, -11.50483984771559953 ) ) ;
#22888 = EDGE_CURVE ( 'NONE', #9498, #49564, #8582, .T. ) ;
#22887 = CARTESIAN_POINT ( 'NONE',  ( 75.09775766446816192, 13.79064084518985744, -14.73081397881156640 ) ) ;
#22889 = CARTESIAN_POINT ( 'NONE',  ( 0.5469381754224795777, -4.307629671082502831, -43.67210485792230656 ) ) ;
#22890 = CARTESIAN_POINT ( 'NONE',  ( 59.13340102237120277, -3.116188944679349593, -15.65754737356207116 ) ) ;
#22891 = CARTESIAN_POINT ( 'NONE',  ( 12.14987702140462744, -22.52875230863022793, -38.45899921809279220 ) ) ;
#22892 = CARTESIAN_POINT ( 'NONE',  ( 57.49008984609597661, 18.87413028802463089, -52.59398425856332437 ) ) ;
#22893 = CARTESIAN_POINT ( 'NONE',  ( 9.633937397696209715, -15.61618894467929941, -22.64999999999999858 ) ) ;
#22894 = CARTESIAN_POINT ( 'NONE',  ( 40.87457764023000095, 13.37883080456079909, -4.704571308414649877 ) ) ;
#22895 = CARTESIAN_POINT ( 'NONE',  ( 63.60923929913089836, 1.000506532485009981, -61.70853630543769697 ) ) ;
#22896 = LINE ( 'NONE', #42324, #25830 ) ;
#22897 = CARTESIAN_POINT ( 'NONE',  ( 68.13393739769745139, -49.21324915460503036, -70.54648330188275906 ) ) ;
#22898 = CIRCLE ( 'NONE', #43868, 6.099999999999994316 ) ;
#22899 = CARTESIAN_POINT ( 'NONE',  ( 76.13000578349209491, -43.30572666886710209, -13.72134801843236218 ) ) ;
#22900 = CARTESIAN_POINT ( 'NONE',  ( 18.09998078254310272, -52.35976395901120384, -75.83262351151699932 ) ) ;
#22901 = CARTESIAN_POINT ( 'NONE',  ( 60.86356685786619636, -43.43553833881050252, -9.316062384177440592 ) ) ;
#22902 = CARTESIAN_POINT ( 'NONE',  ( 22.36782798052980326, -11.53632343959220030, -66.88287958694509427 ) ) ;
#22903 = CARTESIAN_POINT ( 'NONE',  ( 63.61601920124529386, 1.328802495350130064, -61.91104772260080580 ) ) ;
#22904 = ORIENTED_EDGE ( 'NONE', *, *, #22675, .F. ) ;
#22905 = DIRECTION ( 'NONE',  ( 0.6933752452815367118, 0.7071067811865475727, -0.1386750490563054827 ) ) ;
#22906 = CARTESIAN_POINT ( 'NONE',  ( 73.12399047084761605, 1.191644800533219861, -68.79793125682789423 ) ) ;
#22907 = DIRECTION ( 'NONE',  ( 0.000000000000000000, 0.000000000000000000, -1.000000000000000000 ) ) ;
#22908 = EDGE_CURVE ( 'NONE', #45765, #46021, #12774, .T. ) ;
#22909 = DIRECTION ( 'NONE',  ( 0.000000000000000000, -1.000000000000000000, 0.000000000000000000 ) ) ;
#22910 = CARTESIAN_POINT ( 'NONE',  ( 43.28342787795109814, -45.55823673264939799, -7.371216836625280600 ) ) ;
#22911 = VERTEX_POINT ( 'NONE', #43705 ) ;
#22912 = ORIENTED_EDGE ( 'NONE', *, *, #28559, .T. ) ;
#22913 = EDGE_LOOP ( 'NONE', ( #12819, #6006, #41877, #11023, #34726 ) ) ;
#22914 = LINE ( 'NONE', #47570, #42780 ) ;
#22915 = CARTESIAN_POINT ( 'NONE',  ( 21.82498608452069888, -10.18542486436930083, -81.23899999999999011 ) ) ;
#22916 = CARTESIAN_POINT ( 'NONE',  ( 53.59226879024850376, -49.40789622861189656, -49.22934975135349589 ) ) ;
#22917 = CIRCLE ( 'NONE', #17922, 0.5000000000822003576 ) ;
#22918 = CARTESIAN_POINT ( 'NONE',  ( 0.1155611319282749960, -51.17475502668380472, -35.14999999933320396 ) ) ;
#22919 = ORIENTED_EDGE ( 'NONE', *, *, #6981, .F. ) ;
#22920 = CARTESIAN_POINT ( 'NONE',  ( 9.366944253490801842, -14.82503573980447342, -79.49003206933410581 ) ) ;
#22921 = ORIENTED_EDGE ( 'NONE', *, *, #7682, .F. ) ;
#22922 = CARTESIAN_POINT ( 'NONE',  ( 24.04513930477782679, -15.61618913701998146, -67.79233342760500136 ) ) ;
#22923 = CARTESIAN_POINT ( 'NONE',  ( 71.83393739769618946, 10.88381105532070059, -68.84999999999999432 ) ) ;
#22924 = VERTEX_POINT ( 'NONE', #47900 ) ;
#22925 = EDGE_CURVE ( 'NONE', #19324, #7222, #12000, .T. ) ;
#22926 = DIRECTION ( 'NONE',  ( 0.000000000000000000, 0.000000000000000000, 1.000000000000000000 ) ) ;
#22927 = CARTESIAN_POINT ( 'NONE',  ( 53.43416304911610126, -51.19054688946549447, -75.78314156995350004 ) ) ;
#22928 = CARTESIAN_POINT ( 'NONE',  ( 60.27616520369410580, 14.52716031431759980, -47.25859949951769323 ) ) ;
#22929 = EDGE_CURVE ( 'NONE', #45896, #677, #31143, .T. ) ;
#22930 = CARTESIAN_POINT ( 'NONE',  ( 22.90081829478373976, -15.57281448673799495, -40.45078489836800628 ) ) ;
#22931 = AXIS2_PLACEMENT_3D ( 'NONE', #21519, #37516, #49590 ) ;
#22932 = CARTESIAN_POINT ( 'NONE',  ( 41.53965823250400291, -44.22865657591820110, -4.633657428418399782 ) ) ;
#22933 = CARTESIAN_POINT ( 'NONE',  ( 65.10753607264098264, 0.7662848317789809904, -17.50331135171781227 ) ) ;
#22934 = CARTESIAN_POINT ( 'NONE',  ( -4.852296971786230095, 16.18044332419180265, -5.030532656363839727 ) ) ;
#22935 = B_SPLINE_CURVE_WITH_KNOTS ( 'NONE', 3,
 ( #4762, #28333, #32503, #36719, #19958, #16296, #35950, #16044, #31999, #1088, #12121, #48020, #40147, #8445, #24390, #4499, #48794, #20469, #28858, #44861, #29879, #22019, #9732, #15145, #21763, #29379 ),
 .UNSPECIFIED., .F., .F.,
 ( 4, 2, 2, 2, 2, 2, 2, 2, 2, 2, 2, 2, 4 ),
 ( 0.000000000000000000, 0.03124996214440351264, 0.06249992428880702527, 0.09374988643321054138, 0.1249998485776140505, 0.1562498107220175736, 0.1874997728664210828, 0.2187497350108245919, 0.2499996971552281011, 0.3124996214440353692, 0.3749995457328426096, 0.4374994700216498500, 0.4999993943104570904 ),
 .UNSPECIFIED. ) ;
#22936 = CARTESIAN_POINT ( 'NONE',  ( 8.222937397696199469, -15.61618894467929941, -32.14999999999999858 ) ) ;
#22937 = DIRECTION ( 'NONE',  ( -1.000000000000000000, 0.000000000000000000, 0.000000000000000000 ) ) ;
#22938 = CARTESIAN_POINT ( 'NONE',  ( 17.92370450339669929, -51.11618894467930119, -74.14999999999999147 ) ) ;
#22939 = CARTESIAN_POINT ( 'NONE',  ( 18.37043360245199963, -23.13847801844509888, -55.69551641643489859 ) ) ;
#22940 = ORIENTED_EDGE ( 'NONE', *, *, #36645, .T. ) ;
#22941 = DIRECTION ( 'NONE',  ( 0.3445670372598625963, -0.6174735272333260472, -0.7071067811865442421 ) ) ;
#22942 = CARTESIAN_POINT ( 'NONE',  ( 57.31868460842820667, 19.28698455871409934, -53.29708888710140258 ) ) ;
#22944 = EDGE_CURVE ( 'NONE', #5288, #11422, #35584, .T. ) ;
#22943 = CARTESIAN_POINT ( 'NONE',  ( 71.33393739769670105, 1.396834109478129804, -70.23662692463440749 ) ) ;
#22945 = CARTESIAN_POINT ( 'NONE',  ( 44.36160194340284590, -39.98360157410301952, -64.90776822339829266 ) ) ;
#22946 = AXIS2_PLACEMENT_3D ( 'NONE', #42533, #22584, #39115 ) ;
#22947 = CARTESIAN_POINT ( 'NONE',  ( 14.73074138134250077, 19.35333670681460205, -20.78918949795229665 ) ) ;
#22948 = CARTESIAN_POINT ( 'NONE',  ( 46.74845599210109981, -53.81985652269789711, -75.90842213619210099 ) ) ;
#22949 = CARTESIAN_POINT ( 'NONE',  ( 9.366809454094768839, -15.61635577034980038, -65.45282021618999124 ) ) ;
#22950 = CARTESIAN_POINT ( 'NONE',  ( 48.03526516117440082, -54.27886751425110390, -54.71370355240560457 ) ) ;
#22951 = CARTESIAN_POINT ( 'NONE',  ( 9.367282414267279478, -15.61633198492950036, -43.45282021618999835 ) ) ;
#22952 = CARTESIAN_POINT ( 'NONE',  ( 22.90015373937838916, -14.70062920033102749, -36.80410166171807873 ) ) ;
#22953 = CARTESIAN_POINT ( 'NONE',  ( 47.84600491270340683, 23.14802384070760155, -54.72009433156399894 ) ) ;
#22954 = ORIENTED_EDGE ( 'NONE', *, *, #49637, .F. ) ;
#22955 = CARTESIAN_POINT ( 'NONE',  ( 9.989812541601329698, -12.15320050589289913, -76.01055054980109560 ) ) ;
#22956 = EDGE_LOOP ( 'NONE', ( #26157, #35110, #31775, #37369, #191, #7272 ) ) ;
#22957 = CARTESIAN_POINT ( 'NONE',  ( 71.19853741683878923, 1.383922910988889976, -70.31893907080630868 ) ) ;
#22958 = CARTESIAN_POINT ( 'NONE',  ( 60.60266389430760370, -45.58847639179440137, -47.13124125531790298 ) ) ;
#22959 = CARTESIAN_POINT ( 'NONE',  ( 59.52869175205803032, 14.25746298374641441, -26.73578769780420572 ) ) ;
#22960 = FACE_OUTER_BOUND ( 'NONE', #22670, .T. ) ;
#22962 = CARTESIAN_POINT ( 'NONE',  ( 44.58553514073535951, -33.15021188507264327, -46.23822836818835924 ) ) ;
#22961 = CARTESIAN_POINT ( 'NONE',  ( 57.50723798014340105, 13.88381064843590096, -25.33268340738889890 ) ) ;
#22963 = EDGE_CURVE ( 'NONE', #25181, #34982, #36334, .T. ) ;
#22964 = CARTESIAN_POINT ( 'NONE',  ( 59.52869410915831594, -45.48984219772450643, -26.73579121603098585 ) ) ;
#22965 = LINE ( 'NONE', #10686, #46870 ) ;
#22966 = CARTESIAN_POINT ( 'NONE',  ( 9.026390854479029002, -47.84168788784550230, -54.64999999999999858 ) ) ;
#22967 = ORIENTED_EDGE ( 'NONE', *, *, #16556, .F. ) ;
#22968 = CYLINDRICAL_SURFACE ( 'NONE', #19745, 7.910999999999997812 ) ;
#22969 = EDGE_CURVE ( 'NONE', #46894, #13682, #2780, .T. ) ;
#22970 = CIRCLE ( 'NONE', #29671, 0.9999999999999964473 ) ;
#22971 = ORIENTED_EDGE ( 'NONE', *, *, #18636, .F. ) ;
#22972 = ORIENTED_EDGE ( 'NONE', *, *, #26228, .T. ) ;
#22973 = CARTESIAN_POINT ( 'NONE',  ( 11.76101335022769945, -64.89508155409039603, -16.31614116036690021 ) ) ;
#22974 = CARTESIAN_POINT ( 'NONE',  ( 24.04493737870865289, -14.58063638308804144, -39.75066769201711736 ) ) ;
#22975 = CARTESIAN_POINT ( 'NONE',  ( 76.42375628065715887, -22.57305820191152890, -12.89887670999500102 ) ) ;
#22976 = CARTESIAN_POINT ( 'NONE',  ( 10.10021300068440020, -64.40744690142780371, -46.68963158283009562 ) ) ;
#22977 = ORIENTED_EDGE ( 'NONE', *, *, #12683, .T. ) ;
#22978 = EDGE_LOOP ( 'NONE', ( #34535, #20169, #17915, #37428 ) ) ;
#22979 = CARTESIAN_POINT ( 'NONE',  ( 23.94343571634030354, -16.90563865392866205, -55.55974166775742873 ) ) ;
#22980 = CARTESIAN_POINT ( 'NONE',  ( 56.87601579295709797, 14.74005962510780066, -26.24549083051520171 ) ) ;
#22981 = DIRECTION ( 'NONE',  ( 0.5721078732755690011, 0.8201783838507971103, 0.000000000000000000 ) ) ;
#22982 = CARTESIAN_POINT ( 'NONE',  ( 24.04493739769619864, -15.61618894467929941, -32.14999999999999858 ) ) ;
#22983 = CARTESIAN_POINT ( 'NONE',  ( 60.05814672930910092, -1.519238805058580111, -15.90733267895319969 ) ) ;
#22984 = CARTESIAN_POINT ( 'NONE',  ( 51.62537655945009618, -49.19526475647730024, -76.81862610561158533 ) ) ;
#22985 = CARTESIAN_POINT ( 'NONE',  ( 59.61233446001679681, -47.78174833862750148, -50.05788297521610275 ) ) ;
#22986 = EDGE_CURVE ( 'NONE', #35817, #12296, #4380, .T. ) ;
#22987 = ORIENTED_EDGE ( 'NONE', *, *, #22032, .F. ) ;
#22988 = DIRECTION ( 'NONE',  ( 1.000000000000000000, -1.703274131079987031E-27, 2.066387465239710029E-12 ) ) ;
#22989 = DIRECTION ( 'NONE',  ( 1.000000000000000000, 0.000000000000000000, 0.000000000000000000 ) ) ;
#22990 = CARTESIAN_POINT ( 'NONE',  ( 10.22109116384483229, -12.20808603923138769, -51.61948645223564824 ) ) ;
#22991 = CARTESIAN_POINT ( 'NONE',  ( 22.46011918284800757, -20.47784417130683821, -53.71600424433798082 ) ) ;
#22992 = EDGE_CURVE ( 'NONE', #8898, #17993, #33723, .T. ) ;
#22993 = CARTESIAN_POINT ( 'NONE',  ( 14.42922720758920008, -23.27652253789360159, -40.58219447382339951 ) ) ;
#22994 = CARTESIAN_POINT ( 'NONE',  ( 13.61471636588469991, -51.00593421810309991, -21.87339661680830361 ) ) ;
#22995 = B_SPLINE_CURVE_WITH_KNOTS ( 'NONE', 3,
 ( #45446, #45961, #6128, #34137 ),
 .UNSPECIFIED., .F., .F.,
 ( 4, 4 ),
 ( 0.000000000000000000, 1.000000000000000000 ),
 .UNSPECIFIED. ) ;
#22996 = CARTESIAN_POINT ( 'NONE',  ( 56.63393739769620083, 19.38381105532069881, 14.21249999999999858 ) ) ;
#22997 = CARTESIAN_POINT ( 'NONE',  ( 56.89868990065399856, 13.89633980461660023, -16.37351210530319889 ) ) ;
#22998 = CARTESIAN_POINT ( 'NONE',  ( 61.12579551892830665, -45.35598161261900430, -47.14991131457540519 ) ) ;
#22999 = CARTESIAN_POINT ( 'NONE',  ( 71.20900144662560649, 1.388715606738730068, -70.28003120372629553 ) ) ;
#23000 = CARTESIAN_POINT ( 'NONE',  ( 22.91342759294889930, -17.56068678909149838, -38.93609081202739475 ) ) ;
#23001 = CARTESIAN_POINT ( 'NONE',  ( 9.367282414267279478, -15.61633198492950036, -43.45282021618999835 ) ) ;
#23002 = VERTEX_POINT ( 'NONE', #32387 ) ;
#23003 = AXIS2_PLACEMENT_3D ( 'NONE', #12192, #3041, #11169 ) ;
#23004 = CARTESIAN_POINT ( 'NONE',  ( 47.11719193978310471, 22.63726203342839582, -75.76637087395009473 ) ) ;
#23005 = CARTESIAN_POINT ( 'NONE',  ( 65.00039235738410071, 1.369544300367010026, -60.93595317393490518 ) ) ;
#23006 = CARTESIAN_POINT ( 'NONE',  ( 44.02992521606390142, -46.06978035797460080, -8.311541264417458663 ) ) ;
#23007 = VECTOR ( 'NONE', #31433, 1000.000000000000000 ) ;
#23008 = CARTESIAN_POINT ( 'NONE',  ( 17.73211690492210479, 20.42331746234410161, -75.51793353176734058 ) ) ;
#23009 = CARTESIAN_POINT ( 'NONE',  ( 22.20417850065061671, 22.76024865223504889, -34.79644414665609986 ) ) ;
#23010 = CARTESIAN_POINT ( 'NONE',  ( 8.943569970476740849, -49.33365190531349498, -34.64999999999999858 ) ) ;
#23011 = LINE ( 'NONE', #26429, #23891 ) ;
#23012 = CARTESIAN_POINT ( 'NONE',  ( 82.34961391206009296, 14.41937359025589949, -47.73425003811119893 ) ) ;
#23013 = CARTESIAN_POINT ( 'NONE',  ( 0.2715958990298489861, 19.60531400798089763, -34.53033264416539794 ) ) ;
#23015 = DIRECTION ( 'NONE',  ( 0.000000000000000000, 0.000000000000000000, -1.000000000000000000 ) ) ;
#23014 = DIRECTION ( 'NONE',  ( 0.000000000000000000, 0.000000000000000000, 1.000000000000000000 ) ) ;
#23016 = CIRCLE ( 'NONE', #13840, 3.500000000000003109 ) ;
#23017 = CARTESIAN_POINT ( 'NONE',  ( 8.222431652840050731, -15.61631456792169992, -70.50766849176299900 ) ) ;
#23018 = CARTESIAN_POINT ( 'NONE',  ( 48.90562224917519529, 22.57469039213979656, -54.45244080928650021 ) ) ;
#23019 = ORIENTED_EDGE ( 'NONE', *, *, #31311, .F. ) ;
#23020 = CARTESIAN_POINT ( 'NONE',  ( 53.45905338263879969, -49.36511705999589594, -49.00044516267050199 ) ) ;
#23021 = ORIENTED_EDGE ( 'NONE', *, *, #28683, .F. ) ;
#23022 = CARTESIAN_POINT ( 'NONE',  ( 45.37168861558401289, 7.906016184253609858, -63.92127268888761193 ) ) ;
#23023 = CARTESIAN_POINT ( 'NONE',  ( -5.594977155544602176, -15.61618894467930119, 9.349999999999999645 ) ) ;
#23024 = CARTESIAN_POINT ( 'NONE',  ( 13.92801754442050033, 19.97389345108679848, -22.96894029843029728 ) ) ;
#23025 = CARTESIAN_POINT ( 'NONE',  ( 51.68229386145609539, -48.76553798961150221, -77.01557736628760154 ) ) ;
#23026 = CARTESIAN_POINT ( 'NONE',  ( 15.00250949113439880, -22.57768516236690104, -51.00410559314149594 ) ) ;
#23027 = CARTESIAN_POINT ( 'NONE',  ( 52.84810394027419989, 18.43930803410469821, -48.89993304137779973 ) ) ;
#23028 = CARTESIAN_POINT ( 'NONE',  ( 54.79773977241499949, -46.08976703690969146, -15.91708512117589969 ) ) ;
#23029 = DIRECTION ( 'NONE',  ( 0.000000000000000000, 0.000000000000000000, 1.000000000000000000 ) ) ;
#23030 = EDGE_CURVE ( 'NONE', #12954, #22246, #8312, .T. ) ;
#23031 = ORIENTED_EDGE ( 'NONE', *, *, #20069, .T. ) ;
#23032 = CARTESIAN_POINT ( 'NONE',  ( 8.816156803201931069, -12.78140736318490056, -32.40515068373079544 ) ) ;
#23033 = VERTEX_POINT ( 'NONE', #39774 ) ;
#23034 = EDGE_CURVE ( 'NONE', #46345, #38625, #16160, .T. ) ;
#23035 = CARTESIAN_POINT ( 'NONE',  ( 72.72056432233058842, 1.396834109478120034, -68.84999999999999432 ) ) ;
#23036 = CARTESIAN_POINT ( 'NONE',  ( 10.22879563217340149, 33.47692832875780056, -46.94094174653320550 ) ) ;
#23037 = CARTESIAN_POINT ( 'NONE',  ( 72.74776047649520194, 1.391252479931859964, -62.52735703481241103 ) ) ;
#23038 =( BOUNDED_CURVE ( )  B_SPLINE_CURVE ( 2, ( #49465, #29518, #49970 ),
 .UNSPECIFIED., .F., .T. ) 
 B_SPLINE_CURVE_WITH_KNOTS ( ( 3, 3 ),
 ( 2.168627590050209886, 3.232274745523169734 ),
 .UNSPECIFIED. ) 
 CURVE ( )  GEOMETRIC_REPRESENTATION_ITEM ( )  RATIONAL_B_SPLINE_CURVE ( ( 1.425426480542939967, 1.425426480542939967, 1.323085463760209857 ) ) 
 REPRESENTATION_ITEM ( '' )  );
#23039 = CARTESIAN_POINT ( 'NONE',  ( 47.94507282302989637, -54.66591535502590204, -55.53467711414020158 ) ) ;
#23040 = CARTESIAN_POINT ( 'NONE',  ( 53.05489980299899599, -49.59988638911212178, -49.10811587859365801 ) ) ;
#23041 = DIRECTION ( 'NONE',  ( 0.000000000000000000, 0.000000000000000000, 1.000000000000000000 ) ) ;
#23042 = AXIS2_PLACEMENT_3D ( 'NONE', #32729, #12086, #4208 ) ;
#23043 = CARTESIAN_POINT ( 'NONE',  ( 52.83236252576280378, -52.32374954317370452, -54.28770559089719683 ) ) ;
#23044 = ORIENTED_EDGE ( 'NONE', *, *, #17499, .T. ) ;
#23045 = CARTESIAN_POINT ( 'NONE',  ( 64.68608103367590445, 0.9036513197889380899, -70.56049771322820163 ) ) ;
#23046 = ORIENTED_EDGE ( 'NONE', *, *, #5718, .F. ) ;
#23047 = CARTESIAN_POINT ( 'NONE',  ( 10.77397357765519814, -63.36960133942959317, -45.20699438509760171 ) ) ;
#23048 = CARTESIAN_POINT ( 'NONE',  ( 68.13393739769819035, 19.47158195952289717, -70.40645085170196182 ) ) ;
#23049 = EDGE_LOOP ( 'NONE', ( #30975, #847, #10166, #41119, #16459 ) ) ;
#23050 = CARTESIAN_POINT ( 'NONE',  ( 18.63393739769619728, -45.61618894467940066, -34.64999999999999858 ) ) ;
#23051 = CARTESIAN_POINT ( 'NONE',  ( 57.03355800488689908, 19.22800892903980241, -53.04057970399039590 ) ) ;
#23052 = CARTESIAN_POINT ( 'NONE',  ( 52.23775048363239648, 18.59126050118990037, -77.10775523732289116 ) ) ;
#23053 = ORIENTED_EDGE ( 'NONE', *, *, #50213, .T. ) ;
#23054 = CARTESIAN_POINT ( 'NONE',  ( 10.13693647382719476, -64.73981908136153152, -47.01156320461868887 ) ) ;
#23055 = DIRECTION ( 'NONE',  ( -1.965094753941435058E-11, 1.000000000000000000, 0.000000000000000000 ) ) ;
#23056 = CARTESIAN_POINT ( 'NONE',  ( 14.58506229057406678, 20.56215755416807056, -75.65677362359035385 ) ) ;
#23057 = DIRECTION ( 'NONE',  ( 0.000000000000000000, 0.000000000000000000, 1.000000000000000000 ) ) ;
#23058 = EDGE_CURVE ( 'NONE', #27937, #13523, #13674, .T. ) ;
#23059 = B_SPLINE_SURFACE_WITH_KNOTS ( 'NONE', 3, 3, ( 
 ( #34627, #50632, #22827, #48244, #48499, #8413, #7897, #284, #24358, #534, #4470, #28045, #36426, #23844, #36177, #39867, #12092, #16268, #3968, #39609, #35409, #12602, #16520, #20439, #51664, #44050, #4213, #32468, #27801, #15757 ),
 ( #15506, #28563, #40, #20186, #40120, #40372, #43798, #44564, #28301, #8665, #7648, #16015, #19684, #44304, #24098, #47736, #24620, #32221, #8154, #12339, #40630, #19429, #51410, #31460, #47484, #11579, #31972, #31711, #27541, #11842 ),
 ( #19931, #43547, #23592, #35679, #3713, #35923, #47992, #25917, #16788, #33007, #1576, #45870, #33787, #17815, #45349, #37225, #33534, #44827, #49030, #17311, #49798, #29346, #24878, #45083, #13889, #21477, #20960, #9453, #5767, #13137 ),
 ( #36685, #40888, #25661, #1058, #25402, #29848, #9953, #1836, #21214, #4730, #49551, #20696, #45603, #9193, #37477, #9700, #37739, #41664, #13387, #21732, #25144, #17567, #41148, #49289, #13639, #5263, #4999, #788, #32736, #48765 ),
 ( #41404, #5522, #12869, #29087, #17053, #28825, #8934, #36958, #1322, #33274, #29599, #6811, #14402, #42716, #46396, #22764, #10484, #38519, #22247, #21989, #26439, #31142, #46912, #34304, #37999, #14144, #30883, #10998, #11256, #26693 ),
 ( #18844, #2618, #2349, #26965, #50317, #38784, #19103, #2096, #18072, #42455, #42975, #34826, #41931, #39041, #50828, #51084, #3136, #50050, #30630, #10223, #47168, #42193, #38256, #14920, #6543, #18322, #46133, #7070, #23020, #35080 ),
 ( #2876, #6291, #46655, #15182, #30371, #6030, #34041, #30114, #22507, #10738, #26182, #18588, #34566, #50571, #14661, #15695, #36118, #47674, #473, #220, #44240, #32162, #39289, #15956, #31650, #19622, #7584, #11778, #27737, #36365 ),
 ( #35863, #43736, #16460, #48178, #35612, #23270, #51346, #16204, #12280, #48438, #12032, #32415, #43230, #11517, #28242, #8093, #19364, #7837, #47931, #23530, #31909, #51854, #27477, #35345, #8345, #27985, #27218, #3397, #3651, #24037 ),
 ( #47424, #7323, #43479, #39547, #20125, #23786, #51600, #31397, #24298, #40313, #4409, #20376, #15444, #39801, #3908, #43987, #19872, #4150, #40058, #37695, #42151, #50532, #33494, #30333, #25619, #42414, #41622, #34002, #2054, #14103 ),
 ( #26395, #10699, #38746, #45826, #6249, #37958, #41890, #10180, #8052, #30843, #48027, #7359, #19404, #24335, #4703, #1295, #36934, #41635, #26153, #47079, #643, #1167, #40935, #10268, #41978, #34350, #50094, #1622, #45913, #26227 ),
 ( #33321, #13685, #45650, #45131, #9243, #1365, #29393, #25705, #17613, #6078, #21781, #37787, #1884, #49846, #38047, #11562, #27521, #50361, #46701, #46439, #30417, #26485, #38567, #27013, #51135, #47214, #3440, #22811, #18634, #7367 ),
 ( #6859, #14706, #38830, #14964, #23067, #39087, #27263, #35392, #16502, #264, #16767, #12851, #40872, #44283, #32719, #36667, #35657, #31949, #11820, #51644, #43777, #48746, #32203, #515, #32454, #40611, #24598, #3952, #4710, #49780 ),
 ( #1303, #9169, #9435, #20944, #25126, #9681, #41385, #5502, #49270, #1556, #49529, #41643, #21708, #29829, #37718, #45849, #4882, #23993, #12488, #36580, #12232, #20586, #40524, #32114, #4101, #16947, #4615, #15907, #43943, #20330 ),
 ( #32892, #36071, #21113, #16415, #28978, #9079, #25027, #29497, #5409, #46287, #22403, #1211, #42082, #21367, #45501, #21620, #17969, #9599, #30002, #41556, #37624, #25808, #33681, #45761, #41815, #5922, #37895, #2506, #3027, #22916 ) ),
 .UNSPECIFIED., .F., .F., .F.,
 ( 4, 1, 1, 1, 1, 1, 1, 1, 3, 4 ),
 ( 4, 2, 2, 2, 2, 2, 2, 2, 2, 2, 2, 2, 2, 2, 4 ),
 ( 0.000000000000000000, 0.1250000000000000000, 0.2500000000000000000, 0.3750000000000000000, 0.5000000000000000000, 0.6250000000000000000, 0.7500000000000000000, 0.8750000000000000000, 1.000000000000000000, 1.010000000000000009 ),
 ( 0.000000000000000000, 0.03744778849575899904, 0.1081480782291359966, 0.1523357593124970155, 0.1872251531838270144, 0.2221145470551559864, 0.2911210082761750417, 0.3342500465393130060, 0.3773790848024499711, 0.4312903826313710387, 0.4852016804602920508, 0.5714597569865660365, 0.6485380782585299375, 0.7718633922936719571, 0.8625807652627420774 ),
 .UNSPECIFIED. ) ;
#23060 = CARTESIAN_POINT ( 'NONE',  ( 7.891499209906831069, -15.40421541707130082, -60.80051578558619241 ) ) ;
#23061 = DIRECTION ( 'NONE',  ( 0.000000000000000000, 0.000000000000000000, 1.000000000000000000 ) ) ;
#23062 = CARTESIAN_POINT ( 'NONE',  ( 46.76953110038879657, -38.22888952695009124, -56.47198051342422787 ) ) ;
#23063 = VERTEX_POINT ( 'NONE', #31623 ) ;
#23064 = ORIENTED_EDGE ( 'NONE', *, *, #3726, .F. ) ;
#23065 = LINE ( 'NONE', #39085, #26695 ) ;
#23066 = CARTESIAN_POINT ( 'NONE',  ( 9.731824066760630387, -19.42665331309980203, -55.06176496792579655 ) ) ;
#23067 = CARTESIAN_POINT ( 'NONE',  ( 52.60226675332729940, -49.82835823082800175, -48.60906011901539614 ) ) ;
#23068 = CARTESIAN_POINT ( 'NONE',  ( 51.75217146182449568, 13.88381105532070059, -11.53056162543830077 ) ) ;
#23069 = CARTESIAN_POINT ( 'NONE',  ( 9.859321938117989959, -19.95003254321919783, -32.14999999999999858 ) ) ;
#23070 = AXIS2_PLACEMENT_3D ( 'NONE', #23083, #27027, #39101 ) ;
#23071 = DIRECTION ( 'NONE',  ( 0.000000000000000000, 0.000000000000000000, -1.000000000000000000 ) ) ;
#23072 = CARTESIAN_POINT ( 'NONE',  ( 45.14276133008436886, -45.91161332868410483, -8.929567349377213858 ) ) ;
#23073 = CARTESIAN_POINT ( 'NONE',  ( 68.13393739769847457, -50.70395984887981200, -74.34354914830335304 ) ) ;
#23074 = CARTESIAN_POINT ( 'NONE',  ( 12.16231664502929988, 33.44509448364060233, -15.91745067705889838 ) ) ;
#23075 = CONICAL_SURFACE ( 'NONE', #13097, 0.6300000000000018918, 0.7853981633974476129 ) ;
#23076 = CARTESIAN_POINT ( 'NONE',  ( 21.58244677357819796, -21.80460281980919746, -61.77788021779359440 ) ) ;
#23077 = CARTESIAN_POINT ( 'NONE',  ( 54.75911359420950220, -47.36916784795560176, -25.73144026446449928 ) ) ;
#23078 = VECTOR ( 'NONE', #6802, 1000.000000000000114 ) ;
#23079 = CARTESIAN_POINT ( 'NONE',  ( 54.87218746053860485, -50.87499351157259753, -75.61051383423139782 ) ) ;
#23081 = CARTESIAN_POINT ( 'NONE',  ( 47.81335647225210295, 23.16511464041720103, -54.71582838624409817 ) ) ;
#23080 = CARTESIAN_POINT ( 'NONE',  ( -3.348521525975739710, 18.94928180732459921, -7.645520396857000023 ) ) ;
#23082 = CARTESIAN_POINT ( 'NONE',  ( 47.42962603948429745, -54.62656463334229784, -54.65340493925440057 ) ) ;
#23083 = CARTESIAN_POINT ( 'NONE',  ( 16.13393739769620083, -15.61618894467929941, -22.14999999999999858 ) ) ;
#23084 = ORIENTED_EDGE ( 'NONE', *, *, #5561, .F. ) ;
#23085 = DIRECTION ( 'NONE',  ( 0.000000000000000000, 0.000000000000000000, -1.000000000000000000 ) ) ;
#23086 = CARTESIAN_POINT ( 'NONE',  ( 47.73137043576249994, 23.21653874435460096, -54.73785977659620272 ) ) ;
#23087 = CARTESIAN_POINT ( 'NONE',  ( 72.83393739769620367, 1.883811055320669947, -65.65000000000000568 ) ) ;
#23088 = CARTESIAN_POINT ( 'NONE',  ( 63.23690831390890565, 1.005545696829380109, -62.19455336271669665 ) ) ;
#23089 = CARTESIAN_POINT ( 'NONE',  ( 61.06116337346599465, 14.20715986148650067, -47.36084287260779746 ) ) ;
#23090 = CARTESIAN_POINT ( 'NONE',  ( 17.19328695544820107, -8.241606262222608947, -79.77807145977529046 ) ) ;
#23091 = CARTESIAN_POINT ( 'NONE',  ( 51.24580074018999198, 18.16659437971649993, -76.45613186000909423 ) ) ;
#23092 = CARTESIAN_POINT ( 'NONE',  ( 52.87376177351259798, 18.40584817417369834, -48.72414004473989735 ) ) ;
#23093 = CARTESIAN_POINT ( 'NONE',  ( 61.04001029137710077, -45.35933836075930259, -46.86320535112459851 ) ) ;
#23094 = CARTESIAN_POINT ( 'NONE',  ( -0.2043949983302396078, -45.45597504765002839, -34.94418884479945575 ) ) ;
#23095 = CARTESIAN_POINT ( 'NONE',  ( 56.02491708892659972, 15.50432384546050102, -26.35756105441370067 ) ) ;
#23096 = EDGE_CURVE ( 'NONE', #15061, #38484, #11164, .T. ) ;
#23097 = CARTESIAN_POINT ( 'NONE',  ( 49.53395860104499349, 22.37801950097359693, -54.45855173817810169 ) ) ;
#23098 = CARTESIAN_POINT ( 'NONE',  ( 71.62484648860579739, 0.9098571636355720083, -70.52991329011129551 ) ) ;
#23099 = CARTESIAN_POINT ( 'NONE',  ( 52.74562310603300119, 18.50712734077499988, -48.86764753959050012 ) ) ;
#23100 = CARTESIAN_POINT ( 'NONE',  ( 59.85389437514099598, -29.73929060095769827, -15.91137588707199768 ) ) ;
#23101 = CARTESIAN_POINT ( 'NONE',  ( 71.31531788893299506, 1.266538207494809942, -60.76118683403129950 ) ) ;
#23102 = CYLINDRICAL_SURFACE ( 'NONE', #32563, 1.999999999999998224 ) ;
#23103 = CARTESIAN_POINT ( 'NONE',  ( 72.26754656970919655, 1.277124412296160028, -61.38619408099160069 ) ) ;
#23104 = VECTOR ( 'NONE', #45588, 1000.000000000000000 ) ;
#23105 = DIRECTION ( 'NONE',  ( 1.000000000000000000, 8.008164437427536525E-27, -1.590235242698479852E-09 ) ) ;
#23106 = AXIS2_PLACEMENT_3D ( 'NONE', #24629, #4739, #9202 ) ;
#23107 = CARTESIAN_POINT ( 'NONE',  ( 13.24540460468610270, -9.472626712212976585, -65.81300538149071144 ) ) ;
#23108 = ORIENTED_EDGE ( 'NONE', *, *, #39684, .T. ) ;
#23109 = ORIENTED_EDGE ( 'NONE', *, *, #50652, .T. ) ;
#23110 = CARTESIAN_POINT ( 'NONE',  ( 41.83063930790589779, 12.37849180622510126, -3.362295849109719903 ) ) ;
#23111 = CARTESIAN_POINT ( 'NONE',  ( 9.366957159598959137, -16.50213183952788754, -59.41115353772929097 ) ) ;
#23112 = ORIENTED_EDGE ( 'NONE', *, *, #32206, .T. ) ;
#23113 = CARTESIAN_POINT ( 'NONE',  ( 55.90097409207919554, -45.92300129936620579, -25.39712007592949661 ) ) ;
#23114 = CARTESIAN_POINT ( 'NONE',  ( 0.6045892726184427524, -8.790618991491967904, -34.79644291222913921 ) ) ;
#23115 = EDGE_CURVE ( 'NONE', #51612, #40071, #37758, .T. ) ;
#23116 = ORIENTED_EDGE ( 'NONE', *, *, #33638, .F. ) ;
#23117 = CARTESIAN_POINT ( 'NONE',  ( 22.78356519185971862, -14.13275206067546463, -80.38311699616438943 ) ) ;
#23118 = CARTESIAN_POINT ( 'NONE',  ( 44.73832203227348003, 6.778932900174915233, -66.62801705372713457 ) ) ;
#23119 = VECTOR ( 'NONE', #29604, 1000.000000000000000 ) ;
#23120 = CARTESIAN_POINT ( 'NONE',  ( 41.33192604761929800, -44.75281548107679441, -5.349971310512899869 ) ) ;
#23121 = ORIENTED_EDGE ( 'NONE', *, *, #49271, .F. ) ;
#23122 = EDGE_CURVE ( 'NONE', #6528, #7222, #41468, .T. ) ;
#23123 = CARTESIAN_POINT ( 'NONE',  ( 23.54534064816039773, -12.00274526973129952, -31.64794915417429166 ) ) ;
#23124 = AXIS2_PLACEMENT_3D ( 'NONE', #38915, #34438, #3527 ) ;
#23125 = CYLINDRICAL_SURFACE ( 'NONE', #32991, 1.999999999999999112 ) ;
#23126 = DIRECTION ( 'NONE',  ( 0.000000000000000000, 0.000000000000000000, -1.000000000000000000 ) ) ;
#23127 = EDGE_CURVE ( 'NONE', #43345, #11471, #21653, .T. ) ;
#23128 =( NAMED_UNIT ( * ) PLANE_ANGLE_UNIT ( ) SI_UNIT ( $, .RADIAN. ) );
#23129 = CARTESIAN_POINT ( 'NONE',  ( 59.34396388824480084, -28.26380901204359830, -15.68000386546350100 ) ) ;
#23130 = FACE_OUTER_BOUND ( 'NONE', #31346, .T. ) ;
#23131 = CARTESIAN_POINT ( 'NONE',  ( 47.21533240379599761, -54.54479670161060056, -75.00425604315580586 ) ) ;
#23132 = CARTESIAN_POINT ( 'NONE',  ( 55.22142780376210425, 14.83850043050260048, -16.34787572981039716 ) ) ;
#23133 = DIRECTION ( 'NONE',  ( 0.000000000000000000, 0.000000000000000000, -1.000000000000000000 ) ) ;
#23134 = CARTESIAN_POINT ( 'NONE',  ( 83.66059785054299880, -44.84460576056169856, -47.23564833931240514 ) ) ;
#23135 = CIRCLE ( 'NONE', #49955, 16.00000000000000000 ) ;
#23136 = CARTESIAN_POINT ( 'NONE',  ( 36.13393739769620083, -15.61618894467929941, -16.88999999999999702 ) ) ;
#23137 = CARTESIAN_POINT ( 'NONE',  ( 14.44977587363500149, -7.544888499689109906, -32.94218931063619493 ) ) ;
#23138 = VERTEX_POINT ( 'NONE', #21633 ) ;
#23139 = CARTESIAN_POINT ( 'NONE',  ( 11.51160566532390028, -51.12796951774690513, -23.15000000000000213 ) ) ;
#23140 = CARTESIAN_POINT ( 'NONE',  ( 9.416484201958351008, -63.56992309908239491, -16.81318693889570071 ) ) ;
#23141 = CARTESIAN_POINT ( 'NONE',  ( 76.17746443069590612, -21.84911981489240063, -12.19081726112320041 ) ) ;
#23142 = CARTESIAN_POINT ( 'NONE',  ( 68.13393739769620083, 1.883811055320669947, -60.94999999999999574 ) ) ;
#23143 = CARTESIAN_POINT ( 'NONE',  ( 75.40236786212628317, -44.30595597757749005, -13.67333791107008523 ) ) ;
#23144 = CARTESIAN_POINT ( 'NONE',  ( 12.73487495346794240, -55.47150669537813883, -75.56421462368682285 ) ) ;
#23145 = CARTESIAN_POINT ( 'NONE',  ( 24.04496217889941789, -15.61618911842929869, -37.79232902657031445 ) ) ;
#23146 = CARTESIAN_POINT ( 'NONE',  ( 82.34446664224419976, -45.60532208362960205, -47.68359978794560305 ) ) ;
#23147 = CARTESIAN_POINT ( 'NONE',  ( 57.31173127953859847, -50.51960560014510548, -53.29728758193470384 ) ) ;
#23148 = CARTESIAN_POINT ( 'NONE',  ( 43.01559835719159963, 11.40977387627630080, -3.897419375871189917 ) ) ;
#23149 = CARTESIAN_POINT ( 'NONE',  ( 8.222937397696199469, -15.61618894467929941, -32.14999999999999858 ) ) ;
#23150 = CARTESIAN_POINT ( 'NONE',  ( 63.36072709640390599, -45.11618894467940066, -12.04575099730080012 ) ) ;
#23151 = LINE ( 'NONE', #47046, #43205 ) ;
#23152 = EDGE_CURVE ( 'NONE', #5655, #48924, #33695, .T. ) ;
#23153 = CARTESIAN_POINT ( 'NONE',  ( 66.70613787219339486, -1.460923002439210139, -17.03146698529479863 ) ) ;
#23154 = CARTESIAN_POINT ( 'NONE',  ( 18.65170598449359929, -51.88814251562649815, -75.11575902015950135 ) ) ;
#23155 = CARTESIAN_POINT ( 'NONE',  ( 41.36014816789919735, -44.98000569772389667, -5.614915768826699960 ) ) ;
#23156 = CARTESIAN_POINT ( 'NONE',  ( 11.63313639469540028, -21.55331658940179906, -65.77381455205440375 ) ) ;
#23157 = CARTESIAN_POINT ( 'NONE',  ( 63.51710413059809213, 1.389801772588449946, -62.42722031148289830 ) ) ;
#23158 = EDGE_LOOP ( 'NONE', ( #24888, #31940, #37570, #36481 ) ) ;
#23159 = CARTESIAN_POINT ( 'NONE',  ( 8.784728771152188642, 31.88305279702909800, -46.67204636145419983 ) ) ;
#23160 = CARTESIAN_POINT ( 'NONE',  ( 68.13393739769618662, -2.166188944679360073, -31.09383709942130380 ) ) ;
#23161 = CARTESIAN_POINT ( 'NONE',  ( 73.19885236215881719, 0.9940695285616559795, -68.85188839627709001 ) ) ;
#23162 = CARTESIAN_POINT ( 'NONE',  ( 45.39782597164072797, 8.824816061999294803, -59.88240093257450525 ) ) ;
#23163 = CARTESIAN_POINT ( 'NONE',  ( 9.115768759226799745, -13.63938762484340117, -81.23899999999999011 ) ) ;
#23164 = CARTESIAN_POINT ( 'NONE',  ( 45.18452560921219430, -45.82136313292339480, -8.866308695862619160 ) ) ;
#23165 = ORIENTED_EDGE ( 'NONE', *, *, #36788, .T. ) ;
#23166 = CARTESIAN_POINT ( 'NONE',  ( 17.21347160910339724, 21.88381105532300097, -76.14999999999999147 ) ) ;
#23167 = ORIENTED_EDGE ( 'NONE', *, *, #32590, .F. ) ;
#23168 = TOROIDAL_SURFACE ( 'NONE', #2273, 9.000000000000000000, 1.000000000000000000 ) ;
#23169 = EDGE_LOOP ( 'NONE', ( #50153, #45647, #26741, #34395, #44925 ) ) ;
#23170 = DIRECTION ( 'NONE',  ( -0.01091231665325478710, 0.06889765579810418206, -0.9975640502598241977 ) ) ;
#23171 = CARTESIAN_POINT ( 'NONE',  ( 23.58224949043920304, -15.59470245701460023, -81.23899999999999011 ) ) ;
#23172 = CARTESIAN_POINT ( 'NONE',  ( 44.07452568954059302, 1.883811055320659955, -54.64999999999999858 ) ) ;
#23173 = ORIENTED_EDGE ( 'NONE', *, *, #18742, .T. ) ;
#23174 = CARTESIAN_POINT ( 'NONE',  ( 12.09245220501500739, -10.13125348064280473, -79.75051504134326308 ) ) ;
#23175 = VERTEX_POINT ( 'NONE', #13800 ) ;
#23176 = DIRECTION ( 'NONE',  ( 1.000000000000000000, 0.000000000000000000, 0.000000000000000000 ) ) ;
#23177 = EDGE_CURVE ( 'NONE', #4162, #39703, #10301, .T. ) ;
#23178 = CARTESIAN_POINT ( 'NONE',  ( 2.558369240368420172, -25.18609768228349921, -34.64999999999999858 ) ) ;
#23179 = ORIENTED_EDGE ( 'NONE', *, *, #30916, .T. ) ;
#23180 = DIRECTION ( 'NONE',  ( -0.8857883891771971552, 0.4640893551880569956, 0.000000000000000000 ) ) ;
#23181 = CARTESIAN_POINT ( 'NONE',  ( 53.19108586364980340, -51.21468528679280041, -75.83523861080040263 ) ) ;
#23182 = CARTESIAN_POINT ( 'NONE',  ( 60.66118264286809847, 14.41976552486340069, -47.55100573580950396 ) ) ;
#23183 = AXIS2_PLACEMENT_3D ( 'NONE', #44558, #36678, #36420 ) ;
#23184 = CARTESIAN_POINT ( 'NONE',  ( 12.34850528888871857, -9.930145591977167285, -39.76618442199777803 ) ) ;
#23185 = CARTESIAN_POINT ( 'NONE',  ( -3.839728563314020349, -6.393788602144800493, -54.64999999999999858 ) ) ;
#23186 = CARTESIAN_POINT ( 'NONE',  ( -6.917132356002309912, 14.81246362652350079, -5.581884250354890220 ) ) ;
#23187 = CARTESIAN_POINT ( 'NONE',  ( 46.52115705324671779, 22.06631441008168792, -76.11314270329992837 ) ) ;
#23188 = CARTESIAN_POINT ( 'NONE',  ( 9.367846250551377096, -16.45859118363538798, -39.80754656342805475 ) ) ;
#23189 = CARTESIAN_POINT ( 'NONE',  ( 9.005166737681101097, -18.89755711361290125, -50.15019124198139622 ) ) ;
#23190 = ORIENTED_EDGE ( 'NONE', *, *, #37084, .F. ) ;
#23191 = CARTESIAN_POINT ( 'NONE',  ( 56.82514455556469812, -50.66164335286360654, -53.84957932322389951 ) ) ;
#23192 = CARTESIAN_POINT ( 'NONE',  ( 57.55751162087899786, 19.21837686176930049, -53.12582022096169965 ) ) ;
#23193 = UNCERTAINTY_MEASURE_WITH_UNIT (LENGTH_MEASURE( 1.000000000000000082E-05 ), #24024, 'distance_accuracy_value', 'NONE');
#23194 = CARTESIAN_POINT ( 'NONE',  ( 72.08589079625491536, 1.185470598955550292, -70.12663493719820451 ) ) ;
#23195 = CARTESIAN_POINT ( 'NONE',  ( 45.18678546796069639, -40.04353233429138470, -60.90568228453756205 ) ) ;
#23196 = CARTESIAN_POINT ( 'NONE',  ( 15.80830505657939966, 19.69806453318900097, -20.14990715359050100 ) ) ;
#23197 = B_SPLINE_CURVE_WITH_KNOTS ( 'NONE', 3,
 ( #31195, #19425, #39604, #47226, #46975, #42773, #31455, #11058, #15245, #31965, #35673, #7129, #31705, #3963, #11316, #47987, #47730, #26760 ),
 .UNSPECIFIED., .F., .F.,
 ( 4, 2, 2, 2, 2, 2, 2, 2, 4 ),
 ( 0.000000000000000000, 0.06250000041432862696, 0.1250000008286572539, 0.1875000012429858809, 0.2500000016573145079, 0.3125000020716431348, 0.3750000024859717618, 0.4375000029003003887, 0.5000000033146290157 ),
 .UNSPECIFIED. ) ;
#23198 = CARTESIAN_POINT ( 'NONE',  ( -21.36606260230379917, 21.88381105532059934, 16.35000000000000142 ) ) ;
#23199 = CARTESIAN_POINT ( 'NONE',  ( 8.223031589278729570, -15.61632747405269939, -32.50766849176289952 ) ) ;
#23200 = CARTESIAN_POINT ( 'NONE',  ( 75.13393739769618662, -43.11618894467930119, -84.38499399519520239 ) ) ;
#23201 = CARTESIAN_POINT ( 'NONE',  ( 48.75008997992030402, -54.05277686579759688, -55.10220984819350321 ) ) ;
#23202 = CARTESIAN_POINT ( 'NONE',  ( 24.04478666521990959, -15.61618936535764668, -45.50767606031119783 ) ) ;
#23203 = EDGE_CURVE ( 'NONE', #21823, #25078, #27029, .T. ) ;
#23204 = CARTESIAN_POINT ( 'NONE',  ( 63.46802213033259221, 0.9644268476137549673, -69.42324179401769868 ) ) ;
#23205 = DIRECTION ( 'NONE',  ( 0.3294064756441053565, -0.9441882088883176705, 9.436895709313929201E-16 ) ) ;
#23206 = ORIENTED_EDGE ( 'NONE', *, *, #17049, .T. ) ;
#23207 = CARTESIAN_POINT ( 'NONE',  ( 10.67550186159990133, -20.68690643203139956, -35.82905861000619296 ) ) ;
#23208 = ADVANCED_FACE ( 'NONE', ( #968 ), #28996, .T. ) ;
#23209 = ORIENTED_EDGE ( 'NONE', *, *, #40756, .F. ) ;
#23210 = CARTESIAN_POINT ( 'NONE',  ( 17.36506586026114363, 21.76199782478837008, -76.14999999999999147 ) ) ;
#23211 = CARTESIAN_POINT ( 'NONE',  ( 8.222957243667082139, -16.65188170221874131, -58.46600178368837675 ) ) ;
#23212 = CARTESIAN_POINT ( 'NONE',  ( 49.20993668789943598, -53.61219117315735616, -54.26298610208210249 ) ) ;
#23213 = COLOUR_RGB ( '', 0.72549020, 0.75294118, 0.79215686) ;
#23214 = DIRECTION ( 'NONE',  ( 0.000000000000000000, 1.000000000000000000, 0.000000000000000000 ) ) ;
#23216 = CARTESIAN_POINT ( 'NONE',  ( 14.43662147174979893, 1.104866772713560152, -34.68801049095919353 ) ) ;
#23215 = CARTESIAN_POINT ( 'NONE',  ( 40.79482532997379707, 8.392676044869128660, -82.14319696191608955 ) ) ;
#23218 = ADVANCED_FACE ( 'NONE', ( #21383 ), #6760, .T. ) ;
#23217 = CARTESIAN_POINT ( 'NONE',  ( -0.2067785137990631461, -10.69301208835099537, -34.94627313319775652 ) ) ;
#23219 = CARTESIAN_POINT ( 'NONE',  ( 0.4644698840366340287, -22.39564254398910137, -34.95504743437659556 ) ) ;
#23220 = CARTESIAN_POINT ( 'NONE',  ( 17.16956237237686267, -7.705200009872939404, -67.04933363861024986 ) ) ;
#23221 = ORIENTED_EDGE ( 'NONE', *, *, #11130, .F. ) ;
#23222 = CARTESIAN_POINT ( 'NONE',  ( -0.1437508118502728860, -22.76409625575194795, -34.89146800830128825 ) ) ;
#23223 = EDGE_LOOP ( 'NONE', ( #33239, #13444, #5223, #23358 ) ) ;
#23224 = VECTOR ( 'NONE', #21814, 1000.000000000000000 ) ;
#23225 = ORIENTED_EDGE ( 'NONE', *, *, #48561, .F. ) ;
#23226 = CARTESIAN_POINT ( 'NONE',  ( 0.2019507440921958497, -26.68395609241781585, -34.66067286864802099 ) ) ;
#23227 = CARTESIAN_POINT ( 'NONE',  ( 24.04465145034966156, -15.61618865458276595, -39.79233592887338489 ) ) ;
#23228 = CARTESIAN_POINT ( 'NONE',  ( 31.69621505835715070, -15.61618894406255187, -7.049999999955885777 ) ) ;
#23229 = CARTESIAN_POINT ( 'NONE',  ( 10.21539763879230023, -64.50324338944329838, -46.72617082249710307 ) ) ;
#23230 = ORIENTED_EDGE ( 'NONE', *, *, #29623, .T. ) ;
#23231 = ORIENTED_EDGE ( 'NONE', *, *, #10497, .T. ) ;
#23232 = CARTESIAN_POINT ( 'NONE',  ( 24.04424253783098209, -15.72944217639657083, -55.51222777783377893 ) ) ;
#23233 = CARTESIAN_POINT ( 'NONE',  ( 57.15892657999940241, -45.14675268583049927, -25.30896480302860141 ) ) ;
#23234 = CARTESIAN_POINT ( 'NONE',  ( 56.45387226280909942, -50.77876243562330671, -53.73846350693940366 ) ) ;
#23235 = CARTESIAN_POINT ( 'NONE',  ( 22.42300288295763622, -13.03544233720007206, -46.32879295383082763 ) ) ;
#23236 = CARTESIAN_POINT ( 'NONE',  ( 59.54599179390969965, -1.644003503891439788, -15.85381421209810071 ) ) ;
#23237 = EDGE_CURVE ( 'NONE', #31153, #5028, #26170, .T. ) ;
#23238 = CARTESIAN_POINT ( 'NONE',  ( 52.04690325057050160, -49.64260248550559851, -77.05403615378560289 ) ) ;
#23239 = CARTESIAN_POINT ( 'NONE',  ( 59.16562437307299405, -48.30719178829460247, -50.63109401121659658 ) ) ;
#23240 = ORIENTED_EDGE ( 'NONE', *, *, #16192, .F. ) ;
#23241 = CARTESIAN_POINT ( 'NONE',  ( 63.06393505168800573, 0.8850831926798620186, -68.85873448833349642 ) ) ;
#23242 = DIRECTION ( 'NONE',  ( 0.000000000000000000, 0.000000000000000000, -1.000000000000000000 ) ) ;
#23243 = DIRECTION ( 'NONE',  ( 0.000000000000000000, 0.000000000000000000, 1.000000000000000000 ) ) ;
#23244 = CARTESIAN_POINT ( 'NONE',  ( 24.04500464303940888, -15.61618902416171295, -53.50766607493442706 ) ) ;
#23245 = CARTESIAN_POINT ( 'NONE',  ( 9.418507324180998452, -19.67694583463340052, -38.83937799042379879 ) ) ;
#23246 = CARTESIAN_POINT ( 'NONE',  ( 13.19554430041099913, -50.05398002221009790, -21.01912116497090111 ) ) ;
#23247 = CARTESIAN_POINT ( 'NONE',  ( 54.26063908242769429, 19.39368898450049983, -76.71671800660969609 ) ) ;
#23248 = LINE ( 'NONE', #19079, #16720 ) ;
#23249 = CARTESIAN_POINT ( 'NONE',  ( 56.41668308765360251, 14.04457932355130012, -16.58850673112480223 ) ) ;
#23250 = CARTESIAN_POINT ( 'NONE',  ( 61.09295143732159517, -45.56367091068960207, -47.61628434988689662 ) ) ;
#23251 = CARTESIAN_POINT ( 'NONE',  ( 56.84933714557369910, -50.65633608292760215, -53.71862200040009583 ) ) ;
#23252 = TOROIDAL_SURFACE ( 'NONE', #49261, 5.500000000000000000, 0.5000000000000000000 ) ;
#23253 = EDGE_CURVE ( 'NONE', #19286, #46894, #49663, .T. ) ;
#23254 = CARTESIAN_POINT ( 'NONE',  ( 20.83141696938240273, -20.87701063411540048, -45.11516743498959414 ) ) ;
#23255 = CARTESIAN_POINT ( 'NONE',  ( 22.90093741598583676, -14.73038902033105479, -44.41114283429698162 ) ) ;
#23256 = EDGE_LOOP ( 'NONE', ( #4607, #5055, #50141, #30466 ) ) ;
#23257 = CARTESIAN_POINT ( 'NONE',  ( 46.37947015913910320, 21.71088129859489868, -76.14999999999999147 ) ) ;
#23258 = CARTESIAN_POINT ( 'NONE',  ( 64.78158399514478560, 0.9281439705311279598, -60.67386159597580075 ) ) ;
#23259 = CARTESIAN_POINT ( 'NONE',  ( 0.1605025566177880891, 19.59002818087794040, -34.67617345845554411 ) ) ;
#23260 = CARTESIAN_POINT ( 'NONE',  ( 17.74774429082748384, 20.37931109195205792, -75.46937998419048199 ) ) ;
#23261 = CARTESIAN_POINT ( 'NONE',  ( 64.36502057692270284, 13.88381105532070059, -12.32037188644589953 ) ) ;
#23262 = CARTESIAN_POINT ( 'NONE',  ( 46.70520323956110076, -53.35084480228680093, -76.07728942632040514 ) ) ;
#23263 = CARTESIAN_POINT ( 'NONE',  ( 82.55450662793859351, 14.39374320518479955, -47.70628961803360113 ) ) ;
#23264 = FACE_OUTER_BOUND ( 'NONE', #49056, .T. ) ;
#23265 = CARTESIAN_POINT ( 'NONE',  ( 17.16956573677604680, -23.52717739683416198, -58.25066468824845600 ) ) ;
#23266 = CARTESIAN_POINT ( 'NONE',  ( 8.222954481030059881, -16.28154840277095872, -32.76556799064630354 ) ) ;
#23267 = CARTESIAN_POINT ( 'NONE',  ( 49.21898449315310131, 22.63053291997670158, -55.19912396961220225 ) ) ;
#23268 = ORIENTED_EDGE ( 'NONE', *, *, #18111, .F. ) ;
#23269 = EDGE_CURVE ( 'NONE', #43625, #41459, #4840, .T. ) ;
#23270 = CARTESIAN_POINT ( 'NONE',  ( 52.67786065000549911, -49.76447174785660366, -48.65293559773409982 ) ) ;
#23271 = EDGE_LOOP ( 'NONE', ( #22472, #48189, #25607, #42456 ) ) ;
#23272 = CARTESIAN_POINT ( 'NONE',  ( 47.77173862087886391, 6.796530529533522547, -51.39044986337782461 ) ) ;
#23273 = CARTESIAN_POINT ( 'NONE',  ( 19.13393739769600188, 18.38381105532069881, -83.01107220193038927 ) ) ;
#23274 = CARTESIAN_POINT ( 'NONE',  ( 13.72891134303729999, 20.05318723622899668, -22.65898119229509788 ) ) ;
#23275 = DIRECTION ( 'NONE',  ( 1.000000000000000000, 0.000000000000000000, 0.000000000000000000 ) ) ;
#23276 = CARTESIAN_POINT ( 'NONE',  ( 11.06493085870990001, -10.71234031280460108, -53.69754924930450102 ) ) ;
#23278 = EDGE_CURVE ( 'NONE', #39996, #16045, #37905, .T. ) ;
#23277 = CARTESIAN_POINT ( 'NONE',  ( 52.62897435024740389, 18.57025500941220031, -48.60270736271959890 ) ) ;
#23279 = CARTESIAN_POINT ( 'NONE',  ( 55.96902840122019995, -45.83494316293919724, -17.93019966846399882 ) ) ;
#23280 = CARTESIAN_POINT ( 'NONE',  ( 52.67986940689019804, 18.50721041040169723, -27.55370633776830047 ) ) ;
#23281 = ORIENTED_EDGE ( 'NONE', *, *, #37866, .T. ) ;
#23282 = CARTESIAN_POINT ( 'NONE',  ( 11.05757125146939934, -9.631379859604059845, -32.56358854585789686 ) ) ;
#23283 = ORIENTED_EDGE ( 'NONE', *, *, #8811, .F. ) ;
#23284 = CARTESIAN_POINT ( 'NONE',  ( 10.86720904402820054, -64.97138516849830125, -17.53558607436760042 ) ) ;
#23285 = CARTESIAN_POINT ( 'NONE',  ( 8.892600493579569942, 32.33025239218060420, -46.69114580456879793 ) ) ;
#23286 = CARTESIAN_POINT ( 'NONE',  ( 72.96606887121211571, 1.263738073398980033, -62.36141320605320004 ) ) ;
#23287 = CARTESIAN_POINT ( 'NONE',  ( 52.94422481404690473, -50.11505731177610556, -50.07963147481419952 ) ) ;
#23288 = CARTESIAN_POINT ( 'NONE',  ( 33.20393739695829538, -15.61618894434099936, -11.11999999965936858 ) ) ;
#23289 = DIRECTION ( 'NONE',  ( -1.000000000000000000, -5.465567116091310088E-15, 0.000000000000000000 ) ) ;
#23290 = VECTOR ( 'NONE', #23180, 999.9999999999998863 ) ;
#23291 = VECTOR ( 'NONE', #8113, 1000.000000000000000 ) ;
#23292 = ORIENTED_EDGE ( 'NONE', *, *, #30428, .T. ) ;
#23293 = CARTESIAN_POINT ( 'NONE',  ( 64.67849076041298417, 1.005545696829380109, -70.54702908378739323 ) ) ;
#23294 = CARTESIAN_POINT ( 'NONE',  ( 10.48902586684800120, -63.20932193476740224, -45.62615988541170253 ) ) ;
#23295 = CARTESIAN_POINT ( 'NONE',  ( 65.43393739769584272, 16.88381105532339532, -68.79999999999942872 ) ) ;
#23296 = ORIENTED_EDGE ( 'NONE', *, *, #30553, .T. ) ;
#23297 = CARTESIAN_POINT ( 'NONE',  ( 68.38971107296249841, -30.11618894467929763, -18.15384911730639672 ) ) ;
#23298 = CARTESIAN_POINT ( 'NONE',  ( 56.72454650675000210, 19.42863887235380105, -53.46416969237759531 ) ) ;
#23299 = CARTESIAN_POINT ( 'NONE',  ( 52.28361328024040233, 18.56717822572520404, -77.20042836414900478 ) ) ;
#23300 = ORIENTED_EDGE ( 'NONE', *, *, #38169, .F. ) ;
#23301 = CARTESIAN_POINT ( 'NONE',  ( 22.46010115032094845, -20.47786891796735986, -35.71599943221371376 ) ) ;
#23302 = CARTESIAN_POINT ( 'NONE',  ( -21.86606260230379917, -15.61618894467929408, 1.600000000000000089 ) ) ;
#23303 = DIRECTION ( 'NONE',  ( 0.8090169943749472292, -0.5877852522924734702, 0.000000000000000000 ) ) ;
#23304 = DIRECTION ( 'NONE',  ( 0.000000000000000000, 1.000000000000000000, 0.000000000000000000 ) ) ;
#23305 = CARTESIAN_POINT ( 'NONE',  ( 11.04065704516700031, -22.10010869329390104, -66.50427882216679620 ) ) ;
#23306 = DIRECTION ( 'NONE',  ( -0.7071067811865475727, -0.7071067811865475727, 0.000000000000000000 ) ) ;
#23307 = LINE ( 'NONE', #51384, #23007 ) ;
#23308 = EDGE_LOOP ( 'NONE', ( #44604, #36215, #24536, #20921 ) ) ;
#23309 = ORIENTED_EDGE ( 'NONE', *, *, #21826, .F. ) ;
#23310 = CARTESIAN_POINT ( 'NONE',  ( 47.26610112325450075, -54.05804861832230301, -75.56421356201970241 ) ) ;
#23311 = CARTESIAN_POINT ( 'NONE',  ( 16.17870178787689994, -8.166041969315839921, -51.73456986325379603 ) ) ;
#23312 = EDGE_CURVE ( 'NONE', #19286, #26463, #22845, .T. ) ;
#23313 = CARTESIAN_POINT ( 'NONE',  ( 47.13393739769622215, 7.715342668379952862, -54.35302931744276833 ) ) ;
#23314 = CARTESIAN_POINT ( 'NONE',  ( -21.36606260230379917, 21.88381105532059934, 16.35000000000000142 ) ) ;
#23315 = ADVANCED_FACE ( 'NONE', ( #24984 ), #17672, .T. ) ;
#23316 = CARTESIAN_POINT ( 'NONE',  ( 46.37248745885530354, 21.71508437276260040, -76.14999999999999147 ) ) ;
#23317 = CARTESIAN_POINT ( 'NONE',  ( 51.13393739769659874, -45.11618894467899565, 16.85000000000000142 ) ) ;
#23318 = EDGE_CURVE ( 'NONE', #9892, #28507, #40999, .T. ) ;
#23319 = CARTESIAN_POINT ( 'NONE',  ( 10.13393739769619906, -54.15188668067469990, -54.64999999999999858 ) ) ;
#23320 = CARTESIAN_POINT ( 'NONE',  ( 11.98171981665849906, 33.81671209943120004, -16.46086821534060007 ) ) ;
#23321 = CIRCLE ( 'NONE', #13343, 9.000000000000007105 ) ;
#23322 = AXIS2_PLACEMENT_3D ( 'NONE', #14795, #10353, #6423 ) ;
#23324 = CIRCLE ( 'NONE', #4079, 3.000000000000005773 ) ;
#23323 = CARTESIAN_POINT ( 'NONE',  ( 7.898808619120661234, -16.02285183855100215, -70.49196263479178981 ) ) ;
#23325 = CARTESIAN_POINT ( 'NONE',  ( 21.19542947997879878, -21.50580551610960001, -32.14999999999999858 ) ) ;
#23326 = CARTESIAN_POINT ( 'NONE',  ( 55.54166167750689453, -50.64959640008070352, -75.92050756598530370 ) ) ;
#23328 = CARTESIAN_POINT ( 'NONE',  ( 31.06510394192407887, -35.76182709040440955, -84.62926581869410825 ) ) ;
#23327 = CARTESIAN_POINT ( 'NONE',  ( 0.4348764806820569762, 21.36561379262120042, -7.218237925363110818 ) ) ;
#23329 = AXIS2_PLACEMENT_3D ( 'NONE', #11588, #47239, #15765 ) ;
#23330 = DIRECTION ( 'NONE',  ( 0.000000000000000000, 0.000000000000000000, -1.000000000000000000 ) ) ;
#23331 = LINE ( 'NONE', #8151, #13088 ) ;
#23332 = ORIENTED_EDGE ( 'NONE', *, *, #43444, .F. ) ;
#23333 =( BOUNDED_CURVE ( )  B_SPLINE_CURVE ( 2, ( #51046, #42932, #33567 ),
 .UNSPECIFIED., .F., .T. ) 
 B_SPLINE_CURVE_WITH_KNOTS ( ( 3, 3 ),
 ( 0.1321855491534549842, 2.139356573199050260 ),
 .UNSPECIFIED. ) 
 CURVE ( )  GEOMETRIC_REPRESENTATION_ITEM ( )  RATIONAL_B_SPLINE_CURVE ( ( 1.001093714210619989, 1.008874108804550085, 1.000760730680250177 ) ) 
 REPRESENTATION_ITEM ( '' )  );
#23334 = CARTESIAN_POINT ( 'NONE',  ( 20.18583041119828891, -8.779548377150556249, -81.17805570793466075 ) ) ;
#23335 = CARTESIAN_POINT ( 'NONE',  ( 47.59457368048200721, 23.32277084168419989, -55.07961569987379846 ) ) ;
#23336 = CARTESIAN_POINT ( 'NONE',  ( 8.222918874503296394, -14.86491039005461090, -64.82257030091628280 ) ) ;
#23337 = CYLINDRICAL_SURFACE ( 'NONE', #36885, 6.766999999999998572 ) ;
#23338 = DIRECTION ( 'NONE',  ( 0.000000000000000000, 0.000000000000000000, 1.000000000000000000 ) ) ;
#23339 = CARTESIAN_POINT ( 'NONE',  ( 10.81269192673220125, -20.83069183200840158, -78.98588214913890226 ) ) ;
#23340 = CARTESIAN_POINT ( 'NONE',  ( 51.34919120559619188, 18.37200898748080036, -76.46527063284669623 ) ) ;
#23342 = ADVANCED_FACE ( 'NONE', ( #21580 ), #29293, .T. ) ;
#23341 = CARTESIAN_POINT ( 'NONE',  ( 52.88990462379319979, 18.39739278198799965, -48.74279802066659784 ) ) ;
#23343 = CARTESIAN_POINT ( 'NONE',  ( 78.22251691734010137, 1.883811055320649963, -20.65000000000000213 ) ) ;
#23344 = CARTESIAN_POINT ( 'NONE',  ( 52.87578377016760101, -49.63680538124820885, -48.67531175415540190 ) ) ;
#23345 = CARTESIAN_POINT ( 'NONE',  ( 51.04520179763379417, 21.63149099170350098, -53.86124592026170177 ) ) ;
#23346 = FACE_OUTER_BOUND ( 'NONE', #40455, .T. ) ;
#23347 = CARTESIAN_POINT ( 'NONE',  ( 8.978915886419921222, -63.28580153388660534, -46.63388789120410394 ) ) ;
#23348 = DIRECTION ( 'NONE',  ( -1.000000000000000000, 0.000000000000000000, 0.000000000000000000 ) ) ;
#23349 = CARTESIAN_POINT ( 'NONE',  ( 63.76915202389999138, -31.63922660026030087, -17.09407974168160038 ) ) ;
#23350 = CARTESIAN_POINT ( 'NONE',  ( 71.42462519098069151, 0.8888742037077609348, -60.63285689971630177 ) ) ;
#23351 = CARTESIAN_POINT ( 'NONE',  ( 72.34252581843109908, 1.117797034538490220, -61.38010380652460185 ) ) ;
#23352 = DIRECTION ( 'NONE',  ( 0.000000000000000000, 0.000000000000000000, -1.000000000000000000 ) ) ;
#23353 = CARTESIAN_POINT ( 'NONE',  ( 22.57287615846372475, -13.45385276121991325, -66.34964033311129583 ) ) ;
#23354 = ORIENTED_EDGE ( 'NONE', *, *, #51371, .F. ) ;
#23355 = VERTEX_POINT ( 'NONE', #10596 ) ;
#23356 = LINE ( 'NONE', #38345, #45505 ) ;
#23357 = CARTESIAN_POINT ( 'NONE',  ( 11.88511791769057346, -35.52924089863758184, -59.64999999999999147 ) ) ;
#23358 = ORIENTED_EDGE ( 'NONE', *, *, #23096, .T. ) ;
#23359 = CARTESIAN_POINT ( 'NONE',  ( 57.22147638113349899, -45.13525055360219795, -25.38212350801009975 ) ) ;
#23360 = CARTESIAN_POINT ( 'NONE',  ( 15.90741866609855037, -23.52440880927948186, -78.01678402928762068 ) ) ;
#23361 = TOROIDAL_SURFACE ( 'NONE', #42666, 23.00000000000000000, 1.000000000000000000 ) ;
#23362 = ORIENTED_EDGE ( 'NONE', *, *, #22165, .F. ) ;
#23363 = DIRECTION ( 'NONE',  ( 0.000000000000000000, 0.000000000000000000, -1.000000000000000000 ) ) ;
#23364 = CIRCLE ( 'NONE', #4152, 1.999999999999419131 ) ;
#23365 = CARTESIAN_POINT ( 'NONE',  ( 44.72938784791404743, 6.777849755104416118, -66.67268761791444831 ) ) ;
#23366 = CARTESIAN_POINT ( 'NONE',  ( 11.00351569080370062, 32.38571639576179706, -24.01957829310750014 ) ) ;
#23367 = AXIS2_PLACEMENT_3D ( 'NONE', #35992, #27611, #43617 ) ;
#23368 = CIRCLE ( 'NONE', #17521, 16.50000000000000000 ) ;
#23369 = ORIENTED_EDGE ( 'NONE', *, *, #6699, .F. ) ;
#23370 = CARTESIAN_POINT ( 'NONE',  ( 22.08864837242989765, -9.913195135824970805, -33.54920349970110038 ) ) ;
#23371 = FACE_OUTER_BOUND ( 'NONE', #44699, .T. ) ;
#23372 = CIRCLE ( 'NONE', #35962, 6.099999999999994316 ) ;
#23373 = CARTESIAN_POINT ( 'NONE',  ( 23.95250516387262252, -16.86464842754593008, -49.84272613458953316 ) ) ;
#23374 = CARTESIAN_POINT ( 'NONE',  ( 62.88919424588500107, -30.09987604331610100, -16.25000278776590079 ) ) ;
#23375 = CARTESIAN_POINT ( 'NONE',  ( 14.46046508473829739, 20.21129459968669906, -75.25166008039606425 ) ) ;
#23376 = CARTESIAN_POINT ( 'NONE',  ( 46.58185961912909789, -53.30757753662899745, -76.10130133987269119 ) ) ;
#23377 = CARTESIAN_POINT ( 'NONE',  ( 16.74414179616239906, -7.792225870656369402, -73.53726979628919480 ) ) ;
#23378 = DIRECTION ( 'NONE',  ( 0.000000000000000000, -1.000000000000000000, 0.000000000000000000 ) ) ;
#23379 = CARTESIAN_POINT ( 'NONE',  ( 42.70760066071729710, 14.62349772956079974, -7.311903287840700649 ) ) ;
#23380 = ADVANCED_FACE ( 'NONE', ( #43337 ), #32717, .T. ) ;
#23381 = CARTESIAN_POINT ( 'NONE',  ( 74.28246655494574213, -31.81618894467930403, -61.18283208257732753 ) ) ;
#23382 = EDGE_CURVE ( 'NONE', #22911, #50303, #17167, .T. ) ;
#23383 = CARTESIAN_POINT ( 'NONE',  ( 83.68633570933860710, -44.57328881918749630, -46.84648411755270558 ) ) ;
#23384 = CARTESIAN_POINT ( 'NONE',  ( 61.71847798149180164, 13.88380456764680027, -28.01475703387260197 ) ) ;
#23385 = CARTESIAN_POINT ( 'NONE',  ( 20.71427229670339898, -9.243804751362528549, -78.98588214913890226 ) ) ;
#23386 = VERTEX_POINT ( 'NONE', #11368 ) ;
#23387 = CARTESIAN_POINT ( 'NONE',  ( 14.53168785080005776, -16.78029138097666717, -16.68902128623620129 ) ) ;
#23388 = CARTESIAN_POINT ( 'NONE',  ( 13.95190178771889933, -50.80797314161940648, -21.48693983945890196 ) ) ;
#23389 = CARTESIAN_POINT ( 'NONE',  ( 75.28448646084041229, -21.88343552876009923, -11.45926160344929912 ) ) ;
#23390 = CARTESIAN_POINT ( 'NONE',  ( 8.943569970476740849, -49.33365190531349498, -34.64999999999999858 ) ) ;
#23391 = LINE ( 'NONE', #16070, #10599 ) ;
#23392 = AXIS2_PLACEMENT_3D ( 'NONE', #29506, #34466, #45254 ) ;
#23393 = AXIS2_PLACEMENT_3D ( 'NONE', #7806, #32646, #698 ) ;
#23394 = CARTESIAN_POINT ( 'NONE',  ( 71.33393739769628894, 1.530257664727400879, -61.30355339059330078 ) ) ;
#23395 = CIRCLE ( 'NONE', #16723, 1.500000000038269388 ) ;
#23396 = CARTESIAN_POINT ( 'NONE',  ( 47.18324198357279897, 23.57489020266570279, -54.61058319554400242 ) ) ;
#23397 = CARTESIAN_POINT ( 'NONE',  ( 17.58210831189408552, 18.38379234151610930, -83.19397497661219631 ) ) ;
#23398 = CARTESIAN_POINT ( 'NONE',  ( 63.33805919087440373, 1.375383258925270136, -62.73515566246579311 ) ) ;
#23399 = CARTESIAN_POINT ( 'NONE',  ( 57.33583209739280306, -50.39857923248089833, -53.00720873729819971 ) ) ;
#23400 = CIRCLE ( 'NONE', #25087, 2.999999999999960920 ) ;
#23401 = CARTESIAN_POINT ( 'NONE',  ( 43.83393256038859676, 12.23250093112789827, -5.056952191481049574 ) ) ;
#23403 = EDGE_CURVE ( 'NONE', #26843, #35884, #24470, .T. ) ;
#23402 = CARTESIAN_POINT ( 'NONE',  ( 68.13393739769618662, -1.666188944679350081, -65.65000000000000568 ) ) ;
#23404 = CARTESIAN_POINT ( 'NONE',  ( 59.13393739769620083, 1.883811055320659955, -34.64999999999999858 ) ) ;
#23405 = CARTESIAN_POINT ( 'NONE',  ( 59.82327988359549664, -45.99681751185720202, -47.29966340866579344 ) ) ;
#23406 = CARTESIAN_POINT ( 'NONE',  ( 68.13393739769649926, -48.11618894467630270, -70.54999999999999716 ) ) ;
#23407 = AXIS2_PLACEMENT_3D ( 'NONE', #6051, #34322, #2113 ) ;
#23408 = CARTESIAN_POINT ( 'NONE',  ( 68.13393739769598767, -2.032350560840590070, -29.09832030244560741 ) ) ;
#23409 = CARTESIAN_POINT ( 'NONE',  ( 18.14469253414399930, -51.80504026018019914, -75.54815173289030383 ) ) ;
#23410 = EDGE_CURVE ( 'NONE', #13264, #50203, #28396, .T. ) ;
#23411 = CARTESIAN_POINT ( 'NONE',  ( 41.58072008512179707, -43.56399069942670366, -4.585251495889560047 ) ) ;
#23412 = CARTESIAN_POINT ( 'NONE',  ( 12.13367023409020184, -9.330923878024021789, -60.38692723972829413 ) ) ;
#23413 = CARTESIAN_POINT ( 'NONE',  ( 47.13393739769619373, 8.048130187719129580, -35.14999999999999858 ) ) ;
#23414 = CARTESIAN_POINT ( 'NONE',  ( 63.29751574937540681, 1.134292167764730186, -62.17859900726310229 ) ) ;
#23415 = EDGE_LOOP ( 'NONE', ( #23221, #50787, #50358, #40914 ) ) ;
#23416 = CARTESIAN_POINT ( 'NONE',  ( 45.64759345662743328, 13.96552997495392390, -8.164371371256416765 ) ) ;
#23417 = CARTESIAN_POINT ( 'NONE',  ( 13.34937765935505638, -21.87182001026540945, -35.08569598604245954 ) ) ;
#23418 = CARTESIAN_POINT ( 'NONE',  ( 73.17063711417530669, 1.097895768572089814, -68.83057487531520735 ) ) ;
#23419 = CARTESIAN_POINT ( 'NONE',  ( 45.98741248406297899, 8.860759954654445991, -57.01957150137892683 ) ) ;
#23420 = CARTESIAN_POINT ( 'NONE',  ( 11.89976507272660022, -9.206373029106490691, -81.23899999999999011 ) ) ;
#23421 = VERTEX_POINT ( 'NONE', #27075 ) ;
#23422 = CARTESIAN_POINT ( 'NONE',  ( 17.28335488448169954, 21.70396400196510100, -76.14999999999999147 ) ) ;
#23423 = ORIENTED_EDGE ( 'NONE', *, *, #28704, .F. ) ;
#23424 = VERTEX_POINT ( 'NONE', #11886 ) ;
#23425 = CARTESIAN_POINT ( 'NONE',  ( 57.48392795645190034, -45.11618894467940066, -17.43413289997389981 ) ) ;
#23426 = CARTESIAN_POINT ( 'NONE',  ( 23.34584626182279976, -13.12694180994139970, -81.23899999999999011 ) ) ;
#23427 = CARTESIAN_POINT ( 'NONE',  ( 61.48313195732390568, 14.13204578777779830, -47.33728109067860146 ) ) ;
#23428 = ORIENTED_EDGE ( 'NONE', *, *, #6922, .T. ) ;
#23429 = CARTESIAN_POINT ( 'NONE',  ( 20.11806357404540435, -8.703662688652663348, -53.17433719568577999 ) ) ;
#23430 = ORIENTED_EDGE ( 'NONE', *, *, #20048, .T. ) ;
#23431 = FACE_BOUND ( 'NONE', #4622, .T. ) ;
#23432 = DIRECTION ( 'NONE',  ( -1.000000000000000000, 0.000000000000000000, 0.000000000000000000 ) ) ;
#23433 = VECTOR ( 'NONE', #17156, 1000.000000000000000 ) ;
#23434 = AXIS2_PLACEMENT_3D ( 'NONE', #32436, #749, #36917 ) ;
#23435 = ORIENTED_EDGE ( 'NONE', *, *, #16186, .F. ) ;
#23436 = CARTESIAN_POINT ( 'NONE',  ( 72.78816252330430814, 1.385888765344509999, -62.64792042614379852 ) ) ;
#23437 = CARTESIAN_POINT ( 'NONE',  ( 53.35840066752189870, -51.38288175838889771, -75.63634975937459615 ) ) ;
#23438 = AXIS2_PLACEMENT_3D ( 'NONE', #11719, #51291, #51797 ) ;
#23439 = CARTESIAN_POINT ( 'NONE',  ( 60.55338150670809938, 14.46439363635230180, -47.56067349930459898 ) ) ;
#23440 = CARTESIAN_POINT ( 'NONE',  ( 16.13393739769620083, -15.61618894467929941, -12.65000000000000036 ) ) ;
#23441 = ADVANCED_FACE ( 'NONE', ( #15796 ), #16763, .T. ) ;
#23442 = CYLINDRICAL_SURFACE ( 'NONE', #15019, 7.910999999999997812 ) ;
#23443 = CARTESIAN_POINT ( 'NONE',  ( -11.32734370190460105, 10.64934056395049922, -6.430192534648650593 ) ) ;
#23444 = CYLINDRICAL_SURFACE ( 'NONE', #27068, 7.910999999999997812 ) ;
#23445 = DIRECTION ( 'NONE',  ( 0.000000000000000000, 0.000000000000000000, -1.000000000000000000 ) ) ;
#23446 = CARTESIAN_POINT ( 'NONE',  ( 11.50016019542810142, -9.282559888370199630, -54.58645138154409437 ) ) ;
#23447 = ORIENTED_EDGE ( 'NONE', *, *, #35422, .T. ) ;
#23448 = DIRECTION ( 'NONE',  ( 0.6933752452815368228, -0.7071067811865473507, -0.1386750490563055105 ) ) ;
#23449 = CARTESIAN_POINT ( 'NONE',  ( 57.30647849094400215, 19.33005196432110040, -53.44855329768490293 ) ) ;
#23450 = CARTESIAN_POINT ( 'NONE',  ( 71.88854470306299049, 1.063298638254559947, -70.32231691988620526 ) ) ;
#23451 = CARTESIAN_POINT ( 'NONE',  ( 46.13897661844973186, -40.10140556276615342, -56.28420545448003054 ) ) ;
#23452 = CARTESIAN_POINT ( 'NONE',  ( 14.30723785212189902, 19.48216086971750016, -21.19168582719050065 ) ) ;
#23453 = CARTESIAN_POINT ( 'NONE',  ( 22.29130106582129756, 22.56200410046560023, -34.67842804303189297 ) ) ;
#23454 = CYLINDRICAL_SURFACE ( 'NONE', #48174, 0.4999999999999994449 ) ;
#23455 = CARTESIAN_POINT ( 'NONE',  ( 12.86222957544669931, 18.76465490122250301, -21.07385131904699804 ) ) ;
#23456 = DIRECTION ( 'NONE',  ( 1.000000000000000000, 0.000000000000000000, 0.000000000000000000 ) ) ;
#23457 = CARTESIAN_POINT ( 'NONE',  ( 48.31161565387870382, -54.20246409351659622, -54.89734529629400583 ) ) ;
#23458 = CARTESIAN_POINT ( 'NONE',  ( 16.13393739769620083, -15.61618894467929941, -10.21818181818179916 ) ) ;
#23459 = CARTESIAN_POINT ( 'NONE',  ( 64.46842165375500144, 0.9408120350972789536, -70.40100145642890084 ) ) ;
#23460 = CARTESIAN_POINT ( 'NONE',  ( 14.06333702061520086, -23.32130935170018304, -38.09100306346796572 ) ) ;
#23461 = EDGE_CURVE ( 'NONE', #49612, #33931, #40406, .T. ) ;
#23462 = DIRECTION ( 'NONE',  ( 0.000000000000000000, 0.000000000000000000, 1.000000000000000000 ) ) ;
#23463 = AXIS2_PLACEMENT_3D ( 'NONE', #12379, #8453, #11298 ) ;
#23464 = ORIENTED_EDGE ( 'NONE', *, *, #29071, .T. ) ;
#23465 = CARTESIAN_POINT ( 'NONE',  ( 9.375716657886298933, -12.48040407158219978, -38.20562654191490282 ) ) ;
#23466 = CARTESIAN_POINT ( 'NONE',  ( 64.86559958573499785, 1.367045641526529964, -60.97477925803730159 ) ) ;
#23467 = ORIENTED_EDGE ( 'NONE', *, *, #36042, .F. ) ;
#23468 = LINE ( 'NONE', #39491, #6683 ) ;
#23469 = CARTESIAN_POINT ( 'NONE',  ( 60.33296087198709756, -45.76927181686579615, -47.49787425318459810 ) ) ;
#23470 = CARTESIAN_POINT ( 'NONE',  ( 47.88879426235697423, -54.35786135377512807, -54.72388424469790635 ) ) ;
#23471 = CARTESIAN_POINT ( 'NONE',  ( 10.47385200046668707, 23.98129158042145548, -45.62050397739949403 ) ) ;
#23473 = CARTESIAN_POINT ( 'NONE',  ( 11.13393739769619906, 24.07008072128950005, -24.15000000000000213 ) ) ;
#23472 = CARTESIAN_POINT ( 'NONE',  ( 84.42051485081360340, 12.29857348627670000, -47.44928677006510043 ) ) ;
#23474 = CIRCLE ( 'NONE', #34374, 2.000000000000002220 ) ;
#23475 = CARTESIAN_POINT ( 'NONE',  ( 68.13393739769618662, 0.9838110553206419473, -51.14999999999999858 ) ) ;
#23476 = CARTESIAN_POINT ( 'NONE',  ( 8.222598545279129922, -15.61602001634830117, -66.50766849176299900 ) ) ;
#23477 = ORIENTED_EDGE ( 'NONE', *, *, #24976, .T. ) ;
#23478 = ORIENTED_EDGE ( 'NONE', *, *, #43839, .T. ) ;
#23479 = VERTEX_POINT ( 'NONE', #44806 ) ;
#23480 = DIRECTION ( 'NONE',  ( 0.000000000000000000, 0.000000000000000000, -1.000000000000000000 ) ) ;
#23481 = DIRECTION ( 'NONE',  ( -0.9304380493636926763, 0.3664492274467048283, 0.000000000000000000 ) ) ;
#23482 = CARTESIAN_POINT ( 'NONE',  ( 76.42418064599820582, -22.61660856622344085, -12.90070511953996046 ) ) ;
#23483 = CARTESIAN_POINT ( 'NONE',  ( 10.00488484307560100, -64.56416557920189803, -46.87927852444020260 ) ) ;
#23484 = ORIENTED_EDGE ( 'NONE', *, *, #18736, .T. ) ;
#23485 = VERTEX_POINT ( 'NONE', #40868 ) ;
#23486 = CARTESIAN_POINT ( 'NONE',  ( 71.65445125112970004, 0.9525601718068800183, -60.79122054831070443 ) ) ;
#23487 = CARTESIAN_POINT ( 'NONE',  ( -20.24088394071658570, -1.549377950793656034, -52.62430360528765050 ) ) ;
#23488 = CARTESIAN_POINT ( 'NONE',  ( 56.43927191853270386, -50.77432121216759953, -53.62502937860860186 ) ) ;
#23489 = CARTESIAN_POINT ( 'NONE',  ( 12.58751561127507124, -9.785251382443901136, -45.77867976294210450 ) ) ;
#23490 = CARTESIAN_POINT ( 'NONE',  ( 59.77091825180480100, -2.116024841059339856, -15.76949253102769788 ) ) ;
#23491 = CARTESIAN_POINT ( 'NONE',  ( 52.14531965947189462, -49.88997716300030305, -76.93285152251229420 ) ) ;
#23492 = DIRECTION ( 'NONE',  ( 0.000000000000000000, -1.000000000000000000, 0.000000000000000000 ) ) ;
#23493 = VERTEX_POINT ( 'NONE', #51455 ) ;
#23494 = CYLINDRICAL_SURFACE ( 'NONE', #6566, 0.5000000000000049960 ) ;
#23495 = CARTESIAN_POINT ( 'NONE',  ( 9.569202567055908659, -17.83954696311837651, -51.74261907013472950 ) ) ;
#23496 = CARTESIAN_POINT ( 'NONE',  ( 9.366957815752284588, -14.73024123919837969, -51.49448677520141615 ) ) ;
#23497 = DIRECTION ( 'NONE',  ( 0.000000000000000000, 0.000000000000000000, 1.000000000000000000 ) ) ;
#23498 = CARTESIAN_POINT ( 'NONE',  ( 8.886842905012061422, -12.60514776168469808, -49.13783902869429454 ) ) ;
#23499 = CARTESIAN_POINT ( 'NONE',  ( 30.13393739769619728, -38.61618894467930119, -84.65000000000000568 ) ) ;
#23500 = ADVANCED_FACE ( 'NONE', ( #15550 ), #768, .F. ) ;
#23501 = CARTESIAN_POINT ( 'NONE',  ( 9.367814992753320524, -14.75118133266921916, -63.88787753192362828 ) ) ;
#23502 = CARTESIAN_POINT ( 'NONE',  ( 56.10889328822010214, 13.96147111367669957, -15.64994076471440110 ) ) ;
#23504 = ADVANCED_FACE ( 'NONE', ( #8910 ), #18452, .T. ) ;
#23503 = CARTESIAN_POINT ( 'NONE',  ( 61.10829104979099924, -45.34000981476349779, -47.03632675756029613 ) ) ;
#23505 = VECTOR ( 'NONE', #42196, 1000.000000000000000 ) ;
#23506 = EDGE_CURVE ( 'NONE', #51033, #40162, #37776, .T. ) ;
#23507 = CARTESIAN_POINT ( 'NONE',  ( 68.13393739769620083, 11.88381105532070059, -71.50000000000000000 ) ) ;
#23508 = VECTOR ( 'NONE', #27568, 1000.000000000000000 ) ;
#23509 = CARTESIAN_POINT ( 'NONE',  ( 10.63552672802899934, -20.03320595643510060, -57.63175854304149937 ) ) ;
#23510 = LINE ( 'NONE', #39531, #41894 ) ;
#23511 = AXIS2_PLACEMENT_3D ( 'NONE', #18101, #26467, #42482 ) ;
#23512 = EDGE_CURVE ( 'NONE', #25873, #18453, #38416, .T. ) ;
#23513 = ORIENTED_EDGE ( 'NONE', *, *, #5080, .F. ) ;
#23514 = CARTESIAN_POINT ( 'NONE',  ( 12.13393739769600010, -55.41568642894409180, -74.14999999999999147 ) ) ;
#23515 = CARTESIAN_POINT ( 'NONE',  ( 64.96708350509689467, 1.267233196669030004, -60.75373513970999539 ) ) ;
#23516 = CARTESIAN_POINT ( 'NONE',  ( 42.30370408490749412, -45.85561060964679569, -7.058032441766999732 ) ) ;
#23517 = CARTESIAN_POINT ( 'NONE',  ( 16.13393739769620083, -15.61618894467929941, -34.64999999999999858 ) ) ;
#23518 = CARTESIAN_POINT ( 'NONE',  ( -8.966062602303901841, -15.61618894467929941, 8.449999999999979750 ) ) ;
#23519 = EDGE_CURVE ( 'NONE', #9584, #16231, #7300, .T. ) ;
#23520 = CARTESIAN_POINT ( 'NONE',  ( 22.90071877914020249, -15.61618922162072565, -76.45281474520940890 ) ) ;
#23521 = CARTESIAN_POINT ( 'NONE',  ( 9.366937397696199596, -15.61618894467949836, -28.45282021618999835 ) ) ;
#23522 = FACE_OUTER_BOUND ( 'NONE', #15505, .T. ) ;
#23524 = CARTESIAN_POINT ( 'NONE',  ( 11.27235892926153937, -21.94242946667067073, -58.50066475901247998 ) ) ;
#23523 = CARTESIAN_POINT ( 'NONE',  ( 64.31436383256627209, 0.8397385815152118571, -17.57630501671912526 ) ) ;
#23525 = CARTESIAN_POINT ( 'NONE',  ( 8.049429273948879526, -62.14062887497920684, -15.83795189838459905 ) ) ;
#23526 = CARTESIAN_POINT ( 'NONE',  ( 17.63393739769629676, -7.616188944679219475, -35.14999999999999858 ) ) ;
#23527 = EDGE_CURVE ( 'NONE', #4421, #45554, #8983, .T. ) ;
#23528 = CYLINDRICAL_SURFACE ( 'NONE', #46561, 20.00000000000000355 ) ;
#23529 = ORIENTED_EDGE ( 'NONE', *, *, #20657, .T. ) ;
#23530 = CARTESIAN_POINT ( 'NONE',  ( 53.03054974377609909, -49.58583241490480020, -49.02174586602249917 ) ) ;
#23531 = VERTEX_POINT ( 'NONE', #20354 ) ;
#23532 = CARTESIAN_POINT ( 'NONE',  ( 47.10950441794090437, 6.750887858598658475, -54.70666253679335966 ) ) ;
#23533 = LINE ( 'NONE', #19875, #49512 ) ;
#23534 = FACE_OUTER_BOUND ( 'NONE', #15783, .T. ) ;
#23535 = CARTESIAN_POINT ( 'NONE',  ( 51.80594959294069213, -49.19315472720849414, -77.05312857362879697 ) ) ;
#23536 = CARTESIAN_POINT ( 'NONE',  ( 20.63031468509390365, -10.18248394845440075, -54.17286283568619609 ) ) ;
#23537 = CARTESIAN_POINT ( 'NONE',  ( 16.13393739769620083, -15.61618894467929941, -5.093415854460129566 ) ) ;
#23538 = CARTESIAN_POINT ( 'NONE',  ( 56.28345034116380674, -45.19089576527889562, -15.87205044493469863 ) ) ;
#23539 = CARTESIAN_POINT ( 'NONE',  ( 55.88720792914200075, 14.71003294998529931, -25.33276946690889986 ) ) ;
#23540 = ORIENTED_EDGE ( 'NONE', *, *, #30788, .T. ) ;
#23541 = CARTESIAN_POINT ( 'NONE',  ( 10.05032457551389946, -20.57364829529049999, -42.06986027349229573 ) ) ;
#23542 = ORIENTED_EDGE ( 'NONE', *, *, #35198, .F. ) ;
#23543 = CARTESIAN_POINT ( 'NONE',  ( 11.31571027617879999, -65.02774978745999590, -16.86897512598950044 ) ) ;
#23544 = CARTESIAN_POINT ( 'NONE',  ( 10.51008157369509988, 33.62871359210459588, -47.02029114578689928 ) ) ;
#23545 = CARTESIAN_POINT ( 'NONE',  ( 72.83620669801349834, 1.369719003397489976, -62.48691920258249155 ) ) ;
#23546 = AXIS2_PLACEMENT_3D ( 'NONE', #17957, #26327, #49942 ) ;
#23547 = FACE_OUTER_BOUND ( 'NONE', #12337, .T. ) ;
#23548 = CARTESIAN_POINT ( 'NONE',  ( 8.815605938792600682, 32.05029769220720226, -46.67186391141279955 ) ) ;
#23549 = LINE ( 'NONE', #30903, #3354 ) ;
#23550 = AXIS2_PLACEMENT_3D ( 'NONE', #45338, #33261, #4204 ) ;
#23551 = ADVANCED_FACE ( 'NONE', ( #40549 ), #1943, .F. ) ;
#23552 = VECTOR ( 'NONE', #31104, 1000.000000000000000 ) ;
#23553 = EDGE_LOOP ( 'NONE', ( #47582, #20592, #44662, #16097 ) ) ;
#23554 = CARTESIAN_POINT ( 'NONE',  ( 8.428799735006899496, -13.54564620887036952, -74.59099179580000794 ) ) ;
#23555 = CARTESIAN_POINT ( 'NONE',  ( 10.97938593161299892, -63.34067210474159282, -44.74408272625530003 ) ) ;
#23556 = CARTESIAN_POINT ( 'NONE',  ( 8.222373579151801337, -15.61629175287649929, -54.79233150823699816 ) ) ;
#23557 = VERTEX_POINT ( 'NONE', #5943 ) ;
#23558 = CARTESIAN_POINT ( 'NONE',  ( 23.73307481796224394, -17.88869294176529223, -43.88484386199081655 ) ) ;
#23559 = CARTESIAN_POINT ( 'NONE',  ( 13.69578881323610275, -8.072486773562250306, -76.90822709060780937 ) ) ;
#23560 = CARTESIAN_POINT ( 'NONE',  ( 16.13393739769620083, -15.61618894467929941, -15.18999999999999950 ) ) ;
#23561 = VERTEX_POINT ( 'NONE', #13298 ) ;
#23562 = SURFACE_STYLE_FILL_AREA ( #7616 ) ;
#23563 = CARTESIAN_POINT ( 'NONE',  ( 62.88393739769619373, 11.88381105532070059, -84.94863984844531046 ) ) ;
#23564 = CARTESIAN_POINT ( 'NONE',  ( 4.820228898711410359, -36.82939238027569928, -59.64999999999999147 ) ) ;
#23565 = CARTESIAN_POINT ( 'NONE',  ( 53.36310540583830431, 18.42371825317529854, -49.52410620756050008 ) ) ;
#23566 = CARTESIAN_POINT ( 'NONE',  ( 17.77171699767420066, -23.69705511221659933, -78.22868061958260455 ) ) ;
#23567 = DIRECTION ( 'NONE',  ( 0.000000000000000000, 0.000000000000000000, -1.000000000000000000 ) ) ;
#23568 = DIRECTION ( 'NONE',  ( 0.000000000000000000, 1.000000000000000000, 0.000000000000000000 ) ) ;
#23569 = ITEM_DEFINED_TRANSFORMATION ( 'NONE', 'NONE', #31042,  #20940 ) ;
#23570 = ORIENTED_EDGE ( 'NONE', *, *, #2678, .F. ) ;
#23571 = ORIENTED_EDGE ( 'NONE', *, *, #14256, .T. ) ;
#23572 = CARTESIAN_POINT ( 'NONE',  ( 13.58872809970029927, -22.61823174907150147, -52.84363489814459314 ) ) ;
#23573 = CARTESIAN_POINT ( 'NONE',  ( 13.05521822061487214, -49.46974233527257780, -34.79644660940672907 ) ) ;
#23574 = CARTESIAN_POINT ( 'NONE',  ( 10.99494701313530065, -21.43108936971439960, -32.14999999999999858 ) ) ;
#23575 = EDGE_CURVE ( 'NONE', #43692, #13650, #29762, .T. ) ;
#23576 = CARTESIAN_POINT ( 'NONE',  ( 47.24370950863509933, 23.52822492643439745, -74.14999583207030298 ) ) ;
#23577 = DIRECTION ( 'NONE',  ( 0.000000000000000000, 0.000000000000000000, -1.000000000000000000 ) ) ;
#23578 = DIRECTION ( 'NONE',  ( 0.000000000000000000, 0.000000000000000000, -1.000000000000000000 ) ) ;
#23579 = AXIS2_PLACEMENT_3D ( 'NONE', #24610, #16512, #4723 ) ;
#23580 = VECTOR ( 'NONE', #41550, 1000.000000000000000 ) ;
#23581 = CARTESIAN_POINT ( 'NONE',  ( 11.86340152622300081, 33.76504418661139795, -16.42027960339740034 ) ) ;
#23582 = CARTESIAN_POINT ( 'NONE',  ( 24.25939741457850118, -17.01605330347319978, -75.56197422286328447 ) ) ;
#23583 = CARTESIAN_POINT ( 'NONE',  ( 53.09137791023449893, -49.29352759859440170, -26.91462423334489884 ) ) ;
#23584 = CARTESIAN_POINT ( 'NONE',  ( 56.72911628704090248, -50.61618894563009263, -75.43431501713151022 ) ) ;
#23586 = CARTESIAN_POINT ( 'NONE',  ( 44.07452568954059302, -33.11618894467940066, -54.64999999999999858 ) ) ;
#23585 = CARTESIAN_POINT ( 'NONE',  ( -0.5445768713979989295, 21.67700174432700067, -8.410206044792879254 ) ) ;
#23587 = CARTESIAN_POINT ( 'NONE',  ( 63.13551795786779053, 1.096291039689149871, -68.89363957891330870 ) ) ;
#23588 = CARTESIAN_POINT ( 'NONE',  ( 61.51108537876409343, 13.91219412833640057, -46.41805243735920072 ) ) ;
#23589 = EDGE_CURVE ( 'NONE', #14719, #36315, #45782, .T. ) ;
#23590 = CARTESIAN_POINT ( 'NONE',  ( 68.38971107296249841, -1.116188944679350037, -18.15384911730639672 ) ) ;
#23591 = VERTEX_POINT ( 'NONE', #33952 ) ;
#23592 = CARTESIAN_POINT ( 'NONE',  ( 52.79481824716010863, -49.67983215287559773, -48.50059634193729607 ) ) ;
#23593 = CARTESIAN_POINT ( 'NONE',  ( 47.56952775046020321, 23.32449217223370042, -54.84171050377470635 ) ) ;
#23594 = CARTESIAN_POINT ( 'NONE',  ( 2.277530937145189949, -15.61618894467929941, -32.14999999999999858 ) ) ;
#23595 = CARTESIAN_POINT ( 'NONE',  ( 20.11801407433656408, -22.52874480314362771, -72.12568687505527976 ) ) ;
#23596 = CARTESIAN_POINT ( 'NONE',  ( 61.07002009609450255, 14.12889903531000080, -47.07613370539880293 ) ) ;
#23597 = CARTESIAN_POINT ( 'NONE',  ( 19.39393648379719792, -8.917002444580459652, -77.87681711424829700 ) ) ;
#23598 = CARTESIAN_POINT ( 'NONE',  ( 51.37232752684040094, 18.41177481517059888, -76.46732852243368939 ) ) ;
#23599 = CARTESIAN_POINT ( 'NONE',  ( 52.75763158996860369, 18.47217075649399831, -48.62437232909790197 ) ) ;
#23600 = CARTESIAN_POINT ( 'NONE',  ( 20.99563619527035030, -21.94233761205614286, -70.08400039586911134 ) ) ;
#23601 = CARTESIAN_POINT ( 'NONE',  ( 52.83531802359640039, -49.65800651964969603, -48.55820785178020316 ) ) ;
#23602 = ORIENTED_EDGE ( 'NONE', *, *, #11370, .F. ) ;
#23603 = CARTESIAN_POINT ( 'NONE',  ( 22.90069280194860113, -15.61618434420927670, -40.45282443214609458 ) ) ;
#23604 = CARTESIAN_POINT ( 'NONE',  ( 47.68090551657530085, -54.49693150964059640, -54.85613361089130535 ) ) ;
#23605 = CARTESIAN_POINT ( 'NONE',  ( 10.14913760601130122, -63.33847347462889843, -45.99399621147029649 ) ) ;
#23606 = CARTESIAN_POINT ( 'NONE',  ( 22.72481172681589712, -17.38743078316283075, -70.53615642371306649 ) ) ;
#23607 = CARTESIAN_POINT ( 'NONE',  ( 60.77505974369530151, -30.37856211516960059, -16.18800847133800147 ) ) ;
#23608 = CARTESIAN_POINT ( 'NONE',  ( 71.40893329644839582, 0.8879664753683469414, -60.62259972594610247 ) ) ;
#23609 = CYLINDRICAL_SURFACE ( 'NONE', #26750, 6.766999999999998572 ) ;
#23610 = CARTESIAN_POINT ( 'NONE',  ( 72.34709478978140851, 1.033004162168289941, -61.37787765298320153 ) ) ;
#23611 = ADVANCED_FACE ( 'NONE', ( #9102 ), #36875, .T. ) ;
#23612 = FACE_OUTER_BOUND ( 'NONE', #33997, .T. ) ;
#23613 = CARTESIAN_POINT ( 'NONE',  ( 20.03328359842011608, -10.03004935987004487, -66.14666764028179102 ) ) ;
#23614 = EDGE_LOOP ( 'NONE', ( #40724, #7225, #6846, #10676 ) ) ;
#23615 = EDGE_CURVE ( 'NONE', #51085, #41914, #22703, .T. ) ;
#23616 = ORIENTED_EDGE ( 'NONE', *, *, #4916, .F. ) ;
#23617 = CARTESIAN_POINT ( 'NONE',  ( 12.14974750058458675, -8.703698850530118492, -55.12565519788404345 ) ) ;
#23618 = CARTESIAN_POINT ( 'NONE',  ( 21.54530164568834039, -19.77480089234691008, -58.66115332543646588 ) ) ;
#23619 = ORIENTED_EDGE ( 'NONE', *, *, #14140, .F. ) ;
#23620 = CARTESIAN_POINT ( 'NONE',  ( 12.31664131201799961, -65.34953315657870121, -46.39762439856330900 ) ) ;
#23621 = CARTESIAN_POINT ( 'NONE',  ( 21.72480972862922854, -21.21315989654026879, -77.75783541609207816 ) ) ;
#23622 = EDGE_CURVE ( 'NONE', #41523, #14553, #23038, .T. ) ;
#23623 = CARTESIAN_POINT ( 'NONE',  ( 29.13393739769619728, -33.11618894467940066, -53.85091742636659973 ) ) ;
#23624 = EDGE_LOOP ( 'NONE', ( #22398, #6842, #37839, #12228 ) ) ;
#23625 = CIRCLE ( 'NONE', #38739, 6.049999999999999822 ) ;
#23626 = CARTESIAN_POINT ( 'NONE',  ( 11.21896018345050727, 33.88794933533077369, -22.95123051540872439 ) ) ;
#23627 = CARTESIAN_POINT ( 'NONE',  ( 44.80920505379729235, 6.787426711885585995, -66.27361051051437357 ) ) ;
#23628 = CARTESIAN_POINT ( 'NONE',  ( 61.62036109055981115, 14.01986140997038888, -47.09707863094710945 ) ) ;
#23629 = CARTESIAN_POINT ( 'NONE',  ( 20.52487568859579881, -8.637479824688210073, -41.47109660606309944 ) ) ;
#23630 = DIRECTION ( 'NONE',  ( 0.000000000000000000, 0.000000000000000000, -1.000000000000000000 ) ) ;
#23631 = DIRECTION ( 'NONE',  ( 0.7071067811865475727, 0.000000000000000000, 0.7071067811865475727 ) ) ;
#23632 =( NAMED_UNIT ( * ) PLANE_ANGLE_UNIT ( ) SI_UNIT ( $, .RADIAN. ) );
#23633 = CARTESIAN_POINT ( 'NONE',  ( 60.09862518859029734, -29.13340823245889766, -15.80421788918070014 ) ) ;
#23634 = EDGE_CURVE ( 'NONE', #37946, #46311, #30020, .T. ) ;
#23635 = CARTESIAN_POINT ( 'NONE',  ( 9.367462981151710721, -15.61611677545310073, -63.45282021618999124 ) ) ;
#23636 = CARTESIAN_POINT ( 'NONE',  ( 47.43599255125010217, -54.63612274721339901, -74.17395249489511855 ) ) ;
#23637 = CARTESIAN_POINT ( 'NONE',  ( 12.07787674043479953, -22.33445654400859937, -70.68538827799879698 ) ) ;
#23638 = CARTESIAN_POINT ( 'NONE',  ( 9.543072035750400417, -17.38746502142067740, -37.36948665442063344 ) ) ;
#23639 = CARTESIAN_POINT ( 'NONE',  ( 44.72942195059490444, 14.16990783988029889, -7.990949946541189952 ) ) ;
#23640 = ADVANCED_FACE ( 'NONE', ( #5690 ), #42962, .T. ) ;
#23641 = DIRECTION ( 'NONE',  ( 0.000000000000000000, 0.000000000000000000, -1.000000000000000000 ) ) ;
#23642 =( BOUNDED_CURVE ( )  B_SPLINE_CURVE ( 3, ( #39551, #49231, #21159, #32680 ),
 .UNSPECIFIED., .F., .T. ) 
 B_SPLINE_CURVE_WITH_KNOTS ( ( 4, 4 ),
 ( 4.712388980593789967, 6.283185307179586232 ),
 .UNSPECIFIED. ) 
 CURVE ( )  GEOMETRIC_REPRESENTATION_ITEM ( )  RATIONAL_B_SPLINE_CURVE ( ( 1.000000000000000000, 0.8047378541736504021, 0.8047378541736504021, 1.000000000000000000 ) ) 
 REPRESENTATION_ITEM ( '' )  );
#23643 = CARTESIAN_POINT ( 'NONE',  ( 83.38337402972518930, -45.06848590938879795, -47.24826086172119233 ) ) ;
#23644 = DIRECTION ( 'NONE',  ( -1.000000000000000000, 0.000000000000000000, 0.000000000000000000 ) ) ;
#23645 = CARTESIAN_POINT ( 'NONE',  ( 15.50764696403139986, -7.394845927770500538, -44.98346683230629850 ) ) ;
#23646 = ORIENTED_EDGE ( 'NONE', *, *, #48367, .F. ) ;
#23647 = DIRECTION ( 'NONE',  ( -0.000000000000000000, 1.000000000000000000, 0.000000000000000000 ) ) ;
#23648 = CARTESIAN_POINT ( 'NONE',  ( 14.14835400965569967, -50.34648095446409855, -20.86158003109909842 ) ) ;
#23649 = CARTESIAN_POINT ( 'NONE',  ( 76.14068792729830193, 12.13509142339390046, -13.68365738061490156 ) ) ;
#23650 = CARTESIAN_POINT ( 'NONE',  ( 9.366759954081400608, -15.32006465563015851, -55.86110054242375611 ) ) ;
#23651 = FACE_OUTER_BOUND ( 'NONE', #36272, .T. ) ;
#23652 = VECTOR ( 'NONE', #32535, 1000.000000000000000 ) ;
#23653 = ORIENTED_EDGE ( 'NONE', *, *, #32267, .F. ) ;
#23654 = CARTESIAN_POINT ( 'NONE',  ( -8.075504256637460188, -45.03553824879330847, -5.700448868517660195 ) ) ;
#23655 = AXIS2_PLACEMENT_3D ( 'NONE', #16173, #3877, #12508 ) ;
#23656 = CARTESIAN_POINT ( 'NONE',  ( 15.09845420510242242, -23.52719671236787846, -38.33399960928872474 ) ) ;
#23657 = CARTESIAN_POINT ( 'NONE',  ( 50.95939078474919626, 10.05946586878370042, -76.37902184192930122 ) ) ;
#23658 = CARTESIAN_POINT ( 'NONE',  ( 63.29300171101180439, 1.330484379554849994, -62.57139521546640992 ) ) ;
#23659 = CARTESIAN_POINT ( 'NONE',  ( 13.02862176429879781, 19.08811602440689725, -21.18331087829950121 ) ) ;
#23660 = CARTESIAN_POINT ( 'NONE',  ( 57.55751162052580128, -50.59130190800640747, -53.59933301306699605 ) ) ;
#23661 = CARTESIAN_POINT ( 'NONE',  ( 43.52753934370100097, 12.39697735565209946, -5.023899789804930904 ) ) ;
#23662 = DIRECTION ( 'NONE',  ( -1.000000000000000000, 0.000000000000000000, 0.000000000000000000 ) ) ;
#23663 = CARTESIAN_POINT ( 'NONE',  ( 16.13393739769620083, -15.61618894467929941, 6.072546842075589701 ) ) ;
#23664 = CARTESIAN_POINT ( 'NONE',  ( 56.95646850581400145, -47.49882031525390147, -47.91148979950029485 ) ) ;
#23665 = CARTESIAN_POINT ( 'NONE',  ( 22.46007902905824594, -10.75447858878715479, -75.58403018435342346 ) ) ;
#23666 = DIRECTION ( 'NONE',  ( 0.000000000000000000, 0.000000000000000000, -1.000000000000000000 ) ) ;
#23667 = CARTESIAN_POINT ( 'NONE',  ( 18.25826542137950170, -52.10962414010410271, -75.64877291256318870 ) ) ;
#23668 = CARTESIAN_POINT ( 'NONE',  ( 16.10260131614859702, -8.165973351266268665, -66.56600386269059300 ) ) ;
#23669 = CARTESIAN_POINT ( 'NONE',  ( 23.04647760501543274, -11.63208930286926091, -41.34100076697600912 ) ) ;
#23670 = CARTESIAN_POINT ( 'NONE',  ( 63.25101889642220954, 0.9479899806831150189, -62.16329186921600325 ) ) ;
#23671 = EDGE_LOOP ( 'NONE', ( #47463, #8370, #7333, #51673, #50274, #308, #3084 ) ) ;
#23672 = CARTESIAN_POINT ( 'NONE',  ( 8.794764235947729603, 31.93474649087269768, -46.67042062406039804 ) ) ;
#23673 = CARTESIAN_POINT ( 'NONE',  ( 9.751163809707072971, -17.93838706908490366, -35.34166202078984043 ) ) ;
#23674 = CARTESIAN_POINT ( 'NONE',  ( 72.85934862407960111, 1.383411777981069957, -68.54655896616850441 ) ) ;
#23675 = CARTESIAN_POINT ( 'NONE',  ( 52.68908936341578908, -49.75029824513269716, -28.15000000000000213 ) ) ;
#23676 = CARTESIAN_POINT ( 'NONE',  ( 9.950787553869369972, -11.43239409667170037, -81.23899999999999011 ) ) ;
#23677 = ORIENTED_EDGE ( 'NONE', *, *, #16521, .T. ) ;
#23678 = CARTESIAN_POINT ( 'NONE',  ( 17.54620179519039880, 20.94680560585019791, -75.92929371827810314 ) ) ;
#23679 = EDGE_CURVE ( 'NONE', #35239, #16944, #6116, .T. ) ;
#23680 = EDGE_LOOP ( 'NONE', ( #48600, #10969, #45962, #17340 ) ) ;
#23681 = AXIS2_PLACEMENT_3D ( 'NONE', #2950, #18920, #11335 ) ;
#23682 = ORIENTED_EDGE ( 'NONE', *, *, #29794, .F. ) ;
#23683 = CARTESIAN_POINT ( 'NONE',  ( 16.13393739769620083, -15.61618894467929941, -28.45282021618999835 ) ) ;
#23684 = CARTESIAN_POINT ( 'NONE',  ( 22.09174715103110032, -10.52175256428180106, -81.23899999999999011 ) ) ;
#23685 = ADVANCED_FACE ( 'NONE', ( #46565 ), #3044, .T. ) ;
#23686 = CARTESIAN_POINT ( 'NONE',  ( 15.09845518977402890, -7.705181060181322650, -62.96600257953041790 ) ) ;
#23687 = CARTESIAN_POINT ( 'NONE',  ( 14.06335473615125764, -7.911063951914787395, -73.20899817982366642 ) ) ;
#23688 = VERTEX_POINT ( 'NONE', #2787 ) ;
#23689 = B_SPLINE_CURVE_WITH_KNOTS ( 'NONE', 3,
 ( #13901, #33799, #7593, #47178, #23280, #3919, #12041, #31919, #15965, #7846, #11266, #27747, #19881, #35872, #39301, #39051, #8104, #51865, #15704, #27227, #43241, #43492, #23539, #16214 ),
 .UNSPECIFIED., .F., .F.,
 ( 4, 2, 2, 2, 2, 2, 2, 2, 2, 2, 2, 4 ),
 ( 0.000000000000000000, 0.2627958365207210267, 0.8013173561513319276, 1.332723478065980016, 1.850236617094970004, 2.367749756123960214, 3.156999674831939995, 3.551624634185940099, 4.183024569152329342, 5.193264465098549998, 6.167115316339319975, 6.313999209016010639 ),
 .UNSPECIFIED. ) ;
#23690 = CARTESIAN_POINT ( 'NONE',  ( 11.47502755572986111, -10.64500410686288667, -79.71330318819909166 ) ) ;
#23691 = ORIENTED_EDGE ( 'NONE', *, *, #49644, .F. ) ;
#23692 = CARTESIAN_POINT ( 'NONE',  ( 22.46011217105117908, -10.75452410440155404, -63.58399993108093895 ) ) ;
#23693 = EDGE_LOOP ( 'NONE', ( #51501, #45947, #10688, #4295 ) ) ;
#23694 = AXIS2_PLACEMENT_3D ( 'NONE', #51405, #43544, #36 ) ;
#23695 = ORIENTED_EDGE ( 'NONE', *, *, #26740, .T. ) ;
#23696 = CARTESIAN_POINT ( 'NONE',  ( 11.02421726237627375, -21.68417027918511764, -50.23044728260685332 ) ) ;
#23697 = CARTESIAN_POINT ( 'NONE',  ( 41.40756759976829926, 13.53921337778190015, -5.393983492778530398 ) ) ;
#23698 = CARTESIAN_POINT ( 'NONE',  ( 60.42383115829219520, 14.54589923391379891, -47.62650397435140093 ) ) ;
#23699 = ADVANCED_FACE ( 'NONE', ( #34208 ), #18671, .T. ) ;
#23700 = CARTESIAN_POINT ( 'NONE',  ( 22.90069280194860113, -15.61618434420927670, -40.45282443214609458 ) ) ;
#23701 = EDGE_CURVE ( 'NONE', #12879, #31811, #2127, .T. ) ;
#23702 = B_SPLINE_CURVE_WITH_KNOTS ( 'NONE', 3,
 ( #3139, #38259, #2879, #6546, #11001, #34569, #2352, #34307, #22768, #22511, #15185, #30887, #26969, #38787, #50574, #18847, #46399, #50320 ),
 .UNSPECIFIED., .F., .F.,
 ( 4, 2, 2, 2, 2, 2, 2, 2, 4 ),
 ( 0.000000000000000000, 0.06249996402432939774, 0.1249999280486587955, 0.1874998920729882002, 0.2499998560973175910, 0.3124998201216468985, 0.3749997841459761783, 0.4374997481703054580, 0.4999997121946347378 ),
 .UNSPECIFIED. ) ;
#23703 = CARTESIAN_POINT ( 'NONE',  ( -7.084120996664410086, 14.62350974809900173, -5.509165850239240214 ) ) ;
#23704 = CARTESIAN_POINT ( 'NONE',  ( 68.13393739769618662, -0.5161889446793590519, -65.65000000000000568 ) ) ;
#23705 = LINE ( 'NONE', #31571, #2087 ) ;
#23706 = CARTESIAN_POINT ( 'NONE',  ( 18.49813341320899696, -8.133052878602720526, -64.88491241981458302 ) ) ;
#23707 = VERTEX_POINT ( 'NONE', #18758 ) ;
#23708 = B_SPLINE_CURVE_WITH_KNOTS ( 'NONE', 3,
 ( #19400, #10777, #27002, #30919, #11550, #51380, #39324, #15728, #34602, #3428 ),
 .UNSPECIFIED., .F., .F.,
 ( 4, 2, 2, 2, 4 ),
 ( 0.5540946774305016698, 0.5625000000428368452, 0.6625000000401861655, 0.8225000000359454777, 1.000000000000000000 ),
 .UNSPECIFIED. ) ;
#23709 = CARTESIAN_POINT ( 'NONE',  ( 87.61621807841599718, -48.61618894467930119, -61.12885639714370001 ) ) ;
#23710 = TOROIDAL_SURFACE ( 'NONE', #12042, 7.050000000000200551, 2.999999999999960032 ) ;
#23711 = CARTESIAN_POINT ( 'NONE',  ( 12.38873293430890143, -9.639902246245529938, -76.16898841192839598 ) ) ;
#23712 = CARTESIAN_POINT ( 'NONE',  ( 72.42083049230619451, 1.199410787637519960, -69.81037093930601145 ) ) ;
#23713 = CARTESIAN_POINT ( 'NONE',  ( 44.07301638960753820, -39.96058317689758610, -66.30624784718879994 ) ) ;
#23714 = CARTESIAN_POINT ( 'NONE',  ( 15.79694611016800287, 19.73115256075769963, -20.52360778208829828 ) ) ;
#23715 =( LENGTH_UNIT ( ) NAMED_UNIT ( * ) SI_UNIT ( .MILLI., .METRE. ) );
#23716 = CARTESIAN_POINT ( 'NONE',  ( 9.833644626755106088, -20.45756770380817002, -32.29902853823453768 ) ) ;
#23717 = CARTESIAN_POINT ( 'NONE',  ( 61.37880583284824354, 14.09584805848855815, -47.24536948349046384 ) ) ;
#23718 = CARTESIAN_POINT ( 'NONE',  ( 48.47831330238179959, -54.12362947456229989, -54.86665052696550049 ) ) ;
#23719 = CARTESIAN_POINT ( 'NONE',  ( 52.08182543943776466, -33.08310422624513336, -19.98519270871916476 ) ) ;
#23720 = AXIS2_PLACEMENT_3D ( 'NONE', #48845, #40967, #5084 ) ;
#23721 = CARTESIAN_POINT ( 'NONE',  ( 63.25402410758490390, 0.9098571636355720083, -69.14090909090960224 ) ) ;
#23722 = CARTESIAN_POINT ( 'NONE',  ( 47.80730873599560482, 23.17301113850950145, -54.73352113644760664 ) ) ;
#23723 = EDGE_LOOP ( 'NONE', ( #25547, #13839, #42216, #1861, #24700 ) ) ;
#23724 = CARTESIAN_POINT ( 'NONE',  ( 18.27890701731350021, -8.481348111111490340, -32.66030136746149992 ) ) ;
#23725 = FACE_OUTER_BOUND ( 'NONE', #17143, .T. ) ;
#23726 = ORIENTED_EDGE ( 'NONE', *, *, #45663, .T. ) ;
#23727 = CARTESIAN_POINT ( 'NONE',  ( 71.33393739769660158, 1.396834109478120034, -70.23662692463440749 ) ) ;
#23728 = CARTESIAN_POINT ( 'NONE',  ( 60.75261223076579853, -45.51339453889590203, -47.16721473501090145 ) ) ;
#23729 = CARTESIAN_POINT ( 'NONE',  ( 53.80794059781069194, -49.14842230199280237, -48.63343936029099979 ) ) ;
#23730 = CARTESIAN_POINT ( 'NONE',  ( 83.23750471071477364, 13.58710101679191062, -46.42261246174885514 ) ) ;
#23732 = CARTESIAN_POINT ( 'NONE',  ( 22.89999440246446838, -14.86247066410843942, -58.81172304349431101 ) ) ;
#23731 = CARTESIAN_POINT ( 'NONE',  ( 41.50533919090486279, 8.477239747926573088, -78.71846675104687563 ) ) ;
#23733 = CARTESIAN_POINT ( 'NONE',  ( 12.16981617636350066, 18.81688479155219795, -21.14999999999999858 ) ) ;
#23734 = CARTESIAN_POINT ( 'NONE',  ( 15.09848148096914322, -7.705177880388851541, -66.96600053909531880 ) ) ;
#23735 = ORIENTED_EDGE ( 'NONE', *, *, #7504, .T. ) ;
#23736 = CARTESIAN_POINT ( 'NONE',  ( 0.07087462514320330698, 19.88569008439129959, -34.96641315697679175 ) ) ;
#23737 = EDGE_LOOP ( 'NONE', ( #17878, #26038, #38062, #9597 ) ) ;
#23738 = EDGE_CURVE ( 'NONE', #34714, #23561, #43776, .T. ) ;
#23739 =( REPRESENTATION_RELATIONSHIP ('NONE','NONE', #29764, #28088 ) REPRESENTATION_RELATIONSHIP_WITH_TRANSFORMATION ( #35653 )SHAPE_REPRESENTATION_RELATIONSHIP( ) );
#23740 = ORIENTED_EDGE ( 'NONE', *, *, #34004, .T. ) ;
#23741 = CARTESIAN_POINT ( 'NONE',  ( 16.13393739769620083, -15.61618894467929941, -22.64999999999999858 ) ) ;
#23742 = CARTESIAN_POINT ( 'NONE',  ( 29.11900864776890074, -4.497910611074960485, -35.02873218748179340 ) ) ;
#23743 = CARTESIAN_POINT ( 'NONE',  ( 47.18324198357289845, 23.57489020266570279, -74.14999999999999147 ) ) ;
#23744 = CARTESIAN_POINT ( 'NONE',  ( 10.23176309419300090, -64.70699932978828883, -46.94201679684390172 ) ) ;
#23745 = VERTEX_POINT ( 'NONE', #18504 ) ;
#23746 = DIRECTION ( 'NONE',  ( -1.000000000000000000, 0.000000000000000000, 0.000000000000000000 ) ) ;
#23747 = CARTESIAN_POINT ( 'NONE',  ( 23.24148394091319858, 16.60930999848680401, -54.64999999999999858 ) ) ;
#23748 = DIRECTION ( 'NONE',  ( 0.8660254037844387076, 0.4999999999999998890, 2.775557561562889194E-17 ) ) ;
#23749 = AXIS2_PLACEMENT_3D ( 'NONE', #49148, #37582, #40745 ) ;
#23750 = DIRECTION ( 'NONE',  ( 0.9529257800132618916, 0.000000000000000000, -0.3032036572769470362 ) ) ;
#23751 = CARTESIAN_POINT ( 'NONE',  ( 64.18578493394871032, 0.2143848170464559832, -16.96023575528840155 ) ) ;
#23752 = CARTESIAN_POINT ( 'NONE',  ( 51.51980101732179662, -49.43950574372139783, -76.63338017989070750 ) ) ;
#23753 = DIRECTION ( 'NONE',  ( 0.000000000000000000, 1.000000000000000000, 0.000000000000000000 ) ) ;
#23754 = EDGE_CURVE ( 'NONE', #12303, #29238, #25342, .T. ) ;
#23755 = ORIENTED_EDGE ( 'NONE', *, *, #16902, .F. ) ;
#23756 = DIRECTION ( 'NONE',  ( 0.7071067811865656694, -0.7071067811865292541, 0.000000000000000000 ) ) ;
#23757 = CARTESIAN_POINT ( 'NONE',  ( 82.02429831058030629, 10.00628846694210061, -45.87976092105969883 ) ) ;
#23758 = FACE_OUTER_BOUND ( 'NONE', #40867, .T. ) ;
#23759 = CARTESIAN_POINT ( 'NONE',  ( 9.807841574886825953, -20.47795602692574946, -54.29933579507218866 ) ) ;
#23760 = CARTESIAN_POINT ( 'NONE',  ( 23.00413257069000039, -11.82314717367879986, -57.85192144569239758 ) ) ;
#23761 = ADVANCED_FACE ( 'NONE', ( #14835 ), #8606, .T. ) ;
#23762 = CARTESIAN_POINT ( 'NONE',  ( 13.77413875405740029, -50.62291444519870254, -21.29092247280310346 ) ) ;
#23763 = CARTESIAN_POINT ( 'NONE',  ( 54.96007620141639904, 19.38381105532069881, -76.67894625151460275 ) ) ;
#23764 = AXIS2_PLACEMENT_3D ( 'NONE', #29202, #45213, #45728 ) ;
#23765 = EDGE_CURVE ( 'NONE', #3407, #34403, #14317, .T. ) ;
#23766 = DIRECTION ( 'NONE',  ( -0.5547001962252289253, 0.000000000000000000, -0.8320502943378439431 ) ) ;
#23767 = CARTESIAN_POINT ( 'NONE',  ( 60.91034051199495281, -45.42727599127712779, -46.97125969418770097 ) ) ;
#23768 = CARTESIAN_POINT ( 'NONE',  ( 61.24450422717950460, -45.36922733462990465, -47.29134737333090044 ) ) ;
#23769 = CARTESIAN_POINT ( 'NONE',  ( 17.63393739769639978, 10.88381105532070059, -34.64999999999999858 ) ) ;
#23770 = CARTESIAN_POINT ( 'NONE',  ( 17.81845769390660195, -8.767470046512547910, -58.42394785367769572 ) ) ;
#23771 = CARTESIAN_POINT ( 'NONE',  ( -0.01592648613902455240, -22.81930388578409463, -34.78031642072629381 ) ) ;
#23772 = VERTEX_POINT ( 'NONE', #30287 ) ;
#23773 = CARTESIAN_POINT ( 'NONE',  ( 46.81019908455479595, 22.25026678784159984, -76.02856692477300271 ) ) ;
#23774 = CARTESIAN_POINT ( 'NONE',  ( 47.24767689108010416, -54.75733057101270163, -54.63867562300049485 ) ) ;
#23775 = DIRECTION ( 'NONE',  ( 0.000000000000000000, -1.000000000000000000, 0.000000000000000000 ) ) ;
#23776 = CARTESIAN_POINT ( 'NONE',  ( 24.04503344477293680, -15.61618896013167479, -37.50766614148061251 ) ) ;
#23777 = DIRECTION ( 'NONE',  ( -0.5877852522924661427, -0.8090169943749525583, 0.000000000000000000 ) ) ;
#23778 = CARTESIAN_POINT ( 'NONE',  ( 20.99564714593912029, -9.290049021956130915, -47.21600280735441402 ) ) ;
#23779 = CARTESIAN_POINT ( 'NONE',  ( 10.78192289011060012, -64.93864051461240194, -17.70651626566360193 ) ) ;
#23780 = VECTOR ( 'NONE', #41252, 1000.000000000000000 ) ;
#23781 = CYLINDRICAL_SURFACE ( 'NONE', #20114, 1.999999999999998890 ) ;
#23783 = CARTESIAN_POINT ( 'NONE',  ( 47.11197453701439741, -38.11534973524540248, -54.74201631774479182 ) ) ;
#23782 = CARTESIAN_POINT ( 'NONE',  ( 0.4937122138109050762, -8.827062753033800391, -34.90839531524139971 ) ) ;
#23784 = CARTESIAN_POINT ( 'NONE',  ( 49.08512682873279687, 22.68755118111490177, -55.26163594736860318 ) ) ;
#23785 = ORIENTED_EDGE ( 'NONE', *, *, #25127, .F. ) ;
#23786 = CARTESIAN_POINT ( 'NONE',  ( 52.65273120535449891, -49.78633184267020084, -48.66233031291120170 ) ) ;
#23787 = ORIENTED_EDGE ( 'NONE', *, *, #6820, .F. ) ;
#23788 = CARTESIAN_POINT ( 'NONE',  ( 46.65361620740416981, 6.724962863903830801, -56.99320044726326984 ) ) ;
#23789 = DIRECTION ( 'NONE',  ( 0.000000000000000000, 0.7071067811865521247, 0.7071067811865429098 ) ) ;
#23790 = CARTESIAN_POINT ( 'NONE',  ( 83.92831008986510710, 12.99935617635409990, -46.72264359244289977 ) ) ;
#23791 = CARTESIAN_POINT ( 'NONE',  ( 17.93601177679079939, -8.797458371556761136, -60.03506373439399368 ) ) ;
#23792 = CARTESIAN_POINT ( 'NONE',  ( 52.90434486281380799, 18.43107897257790029, -49.01850765170799917 ) ) ;
#23793 = CARTESIAN_POINT ( 'NONE',  ( 56.96434502685580270, -45.17967511238569500, -17.49912984090079959 ) ) ;
#23794 = CARTESIAN_POINT ( 'NONE',  ( 26.13393739769619728, -28.89524513604070322, -39.64999999999999858 ) ) ;
#23795 = ORIENTED_EDGE ( 'NONE', *, *, #33573, .F. ) ;
#23796 = EDGE_CURVE ( 'NONE', #48087, #29490, #42093, .T. ) ;
#23797 = VECTOR ( 'NONE', #3891, 1000.000000000000000 ) ;
#23798 = CARTESIAN_POINT ( 'NONE',  ( 17.00712189924800199, -7.817195611598919847, -46.82299613730939569 ) ) ;
#23799 = VERTEX_POINT ( 'NONE', #26349 ) ;
#23800 = EDGE_CURVE ( 'NONE', #9084, #27518, #20851, .T. ) ;
#23801 = CARTESIAN_POINT ( 'NONE',  ( 11.38858907665120057, -65.22710982081629538, -17.28671555175889907 ) ) ;
#23802 = CARTESIAN_POINT ( 'NONE',  ( 10.90497224517999975, 33.02336919903609669, -45.71389029108730284 ) ) ;
#23803 = CARTESIAN_POINT ( 'NONE',  ( 73.05279713336409486, 1.186856010528209993, -62.37714938719420132 ) ) ;
#23804 = LINE ( 'NONE', #43500, #1735 ) ;
#23805 = CARTESIAN_POINT ( 'NONE',  ( 11.31086268549694829, -65.19635327846651762, -22.85314699157382989 ) ) ;
#23806 = CARTESIAN_POINT ( 'NONE',  ( 13.13393739769619906, -49.61618894467939356, -83.01107220193038927 ) ) ;
#23807 = EDGE_LOOP ( 'NONE', ( #34329, #39710, #38959, #26333, #47054, #37110, #8186, #7481 ) ) ;
#23808 = CARTESIAN_POINT ( 'NONE',  ( 11.10552572835999996, -63.29074793436570445, -44.25199298686389682 ) ) ;
#23809 = CARTESIAN_POINT ( 'NONE',  ( 66.23540447448930024, 18.72622661238580122, -71.50000000000139266 ) ) ;
#23810 = ORIENTED_EDGE ( 'NONE', *, *, #23127, .T. ) ;
#23811 = CARTESIAN_POINT ( 'NONE',  ( 9.521363875773749541, -20.06653018670903066, -44.60392643449169725 ) ) ;
#23812 = CARTESIAN_POINT ( 'NONE',  ( 20.50318394250193421, -8.990010964302234342, -77.19331134062903743 ) ) ;
#23813 = CARTESIAN_POINT ( 'NONE',  ( 9.366383648607859769, -15.61614502978449970, -45.45282021618989177 ) ) ;
#23814 = CARTESIAN_POINT ( 'NONE',  ( 23.67876224802138196, -13.17252032151039920, -49.40793180963832754 ) ) ;
#23815 = ORIENTED_EDGE ( 'NONE', *, *, #22869, .T. ) ;
#23816 = CARTESIAN_POINT ( 'NONE',  ( 8.223551834036749497, -15.61610457483330094, -62.79233150823698395 ) ) ;
#23817 = FACE_OUTER_BOUND ( 'NONE', #48130, .T. ) ;
#23818 = CARTESIAN_POINT ( 'NONE',  ( -21.36606260230379917, 30.88381105532059934, 17.35000000000000142 ) ) ;
#23819 = CARTESIAN_POINT ( 'NONE',  ( 46.25525774125586054, 2.762490711761019568, -54.56299356781535437 ) ) ;
#23820 = CARTESIAN_POINT ( 'NONE',  ( 21.43470869307749993, -9.300767839955041083, -69.51459820258440914 ) ) ;
#23821 = AXIS2_PLACEMENT_3D ( 'NONE', #47968, #39329, #11815 ) ;
#23822 = CARTESIAN_POINT ( 'NONE',  ( 22.90056296481078135, -15.12337164449987270, -38.82400614065659283 ) ) ;
#23823 = CARTESIAN_POINT ( 'NONE',  ( 47.13393739769619373, -38.26167638829240047, -54.64999999999999858 ) ) ;
#23824 = PRODUCT_CONTEXT ( 'NONE', #6017, 'mechanical' ) ;
#23825 = EDGE_CURVE ( 'NONE', #39, #679, #34129, .T. ) ;
#23826 = ORIENTED_EDGE ( 'NONE', *, *, #31890, .F. ) ;
#23827 = CARTESIAN_POINT ( 'NONE',  ( 9.498384706515519582, -19.00383330141319860, -61.08240372876090163 ) ) ;
#23828 = FACE_OUTER_BOUND ( 'NONE', #5874, .T. ) ;
#23829 = CARTESIAN_POINT ( 'NONE',  ( 10.46014298659379982, -20.82286570460119890, -32.14999999999999858 ) ) ;
#23830 = CARTESIAN_POINT ( 'NONE',  ( 47.17278709481859522, 23.23193946581579894, -75.17206278554509424 ) ) ;
#23831 = DIRECTION ( 'NONE',  ( 0.8229030450105319083, 0.000000000000000000, 0.5681818181818162339 ) ) ;
#23832 = CARTESIAN_POINT ( 'NONE',  ( 11.13393739769619906, -65.36556080001030011, 8.349999999999999645 ) ) ;
#23833 = CARTESIAN_POINT ( 'NONE',  ( 12.00051660606520088, 33.89238323676829623, -16.59289575485349744 ) ) ;
#23834 = CARTESIAN_POINT ( 'NONE',  ( 14.36887759788570129, -23.67021182843550164, -72.07634125606408304 ) ) ;
#23835 = CARTESIAN_POINT ( 'NONE',  ( 23.42310265867699925, -15.54859658462440031, -32.14999999999999858 ) ) ;
#23836 = CARTESIAN_POINT ( 'NONE',  ( 56.61807468419900147, -50.61971398085310625, -75.33860262121818607 ) ) ;
#23838 = CARTESIAN_POINT ( 'NONE',  ( 10.66853968524194762, -55.24094850124689771, -45.35057670835523425 ) ) ;
#23837 =( LENGTH_UNIT ( ) NAMED_UNIT ( * ) SI_UNIT ( .MILLI., .METRE. ) );
#23839 = CARTESIAN_POINT ( 'NONE',  ( 63.11947343109709863, 1.194703186106690129, -68.75325824359919125 ) ) ;
#23840 = CARTESIAN_POINT ( 'NONE',  ( 61.43276948373569724, 13.94038599860599881, -46.57406651285639754 ) ) ;
#23841 = CARTESIAN_POINT ( 'NONE',  ( 22.33082320214399985, 22.47179399159420043, -34.65604926186119172 ) ) ;
#23842 = LINE ( 'NONE', #43035, #43999 ) ;
#23843 = ORIENTED_EDGE ( 'NONE', *, *, #33862, .T. ) ;
#23844 = CARTESIAN_POINT ( 'NONE',  ( 52.93498292564289187, -49.60578928504740048, -48.74287988808979577 ) ) ;
#23845 = CARTESIAN_POINT ( 'NONE',  ( 60.96737254747249324, -45.23440155981300137, -27.35231452095100124 ) ) ;
#23846 = AXIS2_PLACEMENT_3D ( 'NONE', #23832, #47474, #3701 ) ;
#23847 = FACE_OUTER_BOUND ( 'NONE', #16980, .T. ) ;
#23848 = CARTESIAN_POINT ( 'NONE',  ( 56.66669568006840052, 14.87756128898679897, -26.25347649126269900 ) ) ;
#23849 = CARTESIAN_POINT ( 'NONE',  ( 11.88155033719490028, -9.498681438118609321, -71.53930262915869775 ) ) ;
#23850 = CARTESIAN_POINT ( 'NONE',  ( 51.08268012532420244, 17.38380819494409835, -76.44192738162151102 ) ) ;
#23851 = CARTESIAN_POINT ( 'NONE',  ( 53.49062365255090157, 18.11806236342570031, -48.99764540719110073 ) ) ;
#23852 = CARTESIAN_POINT ( 'NONE',  ( 18.20465959255140476, -23.32127698777276592, -70.20900000393402252 ) ) ;
#23853 = CARTESIAN_POINT ( 'NONE',  ( 13.05521822061467319, 18.23736444591386174, -34.79644660940673617 ) ) ;
#23854 = VECTOR ( 'NONE', #17796, 1000.000000000000000 ) ;
#23855 = EDGE_LOOP ( 'NONE', ( #36766, #47327, #15381, #47567 ) ) ;
#23856 = EDGE_CURVE ( 'NONE', #36517, #15061, #18164, .T. ) ;
#23857 = CYLINDRICAL_SURFACE ( 'NONE', #36343, 2.000000000000006217 ) ;
#23858 = EDGE_CURVE ( 'NONE', #44239, #3175, #29433, .T. ) ;
#23859 = CARTESIAN_POINT ( 'NONE',  ( 47.58042881629169329, -54.55451462403799923, -54.88832507069039934 ) ) ;
#23860 = CARTESIAN_POINT ( 'NONE',  ( 11.01510582436389818, -10.76437253241610037, -68.08865744343920312 ) ) ;
#23861 = CARTESIAN_POINT ( 'NONE',  ( 9.366947021922275241, -16.50205762954551503, -71.41115368016832576 ) ) ;
#23862 = CARTESIAN_POINT ( 'NONE',  ( 62.57089764215618999, -31.49364712873180139, -16.95369364430399983 ) ) ;
#23864 = EDGE_CURVE ( 'NONE', #1009, #39844, #25232, .T. ) ;
#23863 = CARTESIAN_POINT ( 'NONE',  ( 71.37448966235888292, 1.264489825601020190, -60.79211616508469973 ) ) ;
#23865 = CARTESIAN_POINT ( 'NONE',  ( 11.13393739769619906, 32.00863872204660510, -43.74499609563760316 ) ) ;
#23866 = CARTESIAN_POINT ( 'NONE',  ( 72.34669642622959884, 1.061268603384970088, -61.37747933361649899 ) ) ;
#23867 = CARTESIAN_POINT ( 'NONE',  ( 13.45712100228560182, -22.14131064160670093, -41.47109660606309944 ) ) ;
#23868 = ADVANCED_FACE ( 'NONE', ( #37831 ), #25491, .T. ) ;
#23869 = CARTESIAN_POINT ( 'NONE',  ( 10.66574938343825529, -11.58597127047126563, -65.65508628724941786 ) ) ;
#23870 = VERTEX_POINT ( 'NONE', #45695 ) ;
#23871 = ORIENTED_EDGE ( 'NONE', *, *, #3394, .F. ) ;
#23872 = CARTESIAN_POINT ( 'NONE',  ( 14.06319120082964780, -7.911106295796193955, -55.20898789521619676 ) ) ;
#23873 = CARTESIAN_POINT ( 'NONE',  ( 22.90122453025153249, -15.61618899996915211, -58.45282045073077626 ) ) ;
#23874 = ORIENTED_EDGE ( 'NONE', *, *, #29496, .F. ) ;
#23875 = CARTESIAN_POINT ( 'NONE',  ( 9.221348903864539537, -11.63216924204988167, -58.67431483814366544 ) ) ;
#23876 = CARTESIAN_POINT ( 'NONE',  ( 11.27221720578971720, -21.94232306595641901, -78.21596981197565412 ) ) ;
#23877 = CARTESIAN_POINT ( 'NONE',  ( 29.13393739769620083, -29.55841766305462315, -42.42700139135359194 ) ) ;
#23878 = ORIENTED_EDGE ( 'NONE', *, *, #46532, .T. ) ;
#23879 = CARTESIAN_POINT ( 'NONE',  ( 14.02945871500176267, -22.09610439658294823, -81.05293847742703406 ) ) ;
#23880 = DIRECTION ( 'NONE',  ( -0.04251717301921900671, 0.000000000000000000, -0.9990957361526741076 ) ) ;
#23881 = DIRECTION ( 'NONE',  ( 0.3805321250008310008, 0.000000000000000000, -0.9247677015566404535 ) ) ;
#23882 = CARTESIAN_POINT ( 'NONE',  ( 23.32404688451439867, -11.58071553707250168, -41.62953446819029324 ) ) ;
#23883 = CARTESIAN_POINT ( 'NONE',  ( 9.366764248923921343, -15.61602670952840199, -67.45282021618999124 ) ) ;
#23884 =( NAMED_UNIT ( * ) SI_UNIT ( $, .STERADIAN. ) SOLID_ANGLE_UNIT ( ) );
#23885 = EDGE_CURVE ( 'NONE', #30115, #2811, #15858, .T. ) ;
#23886 = CARTESIAN_POINT ( 'NONE',  ( 61.64370769382880155, -29.21250595235679981, -16.00854006375729810 ) ) ;
#23887 = CARTESIAN_POINT ( 'NONE',  ( 12.14990538336951431, -22.52876835109338316, -42.45899798303421591 ) ) ;
#23888 = CARTESIAN_POINT ( 'NONE',  ( 21.68851505677390179, -20.58140404089619935, -34.46484289138480506 ) ) ;
#23889 = CIRCLE ( 'NONE', #39822, 0.5000000000814214252 ) ;
#23890 = CARTESIAN_POINT ( 'NONE',  ( 41.26310204296880357, 14.16900014587270107, -6.071150992149259906 ) ) ;
#23891 = VECTOR ( 'NONE', #30361, 1000.000000000000000 ) ;
#23892 = CARTESIAN_POINT ( 'NONE',  ( 14.92425731419689861, 21.51730579194029858, -76.12465403027070465 ) ) ;
#23893 = CARTESIAN_POINT ( 'NONE',  ( 83.33882225295539570, -44.99385703852960461, -47.09476873026769539 ) ) ;
#23894 = CARTESIAN_POINT ( 'NONE',  ( 13.55743739769619971, -15.61618894467929941, -40.14999999999999858 ) ) ;
#23895 = EDGE_CURVE ( 'NONE', #15334, #29806, #16997, .T. ) ;
#23896 = CARTESIAN_POINT ( 'NONE',  ( 24.05953913179460102, -17.88941525576920100, -39.59657951998030256 ) ) ;
#23897 = ORIENTED_EDGE ( 'NONE', *, *, #14660, .T. ) ;
#23898 = CARTESIAN_POINT ( 'NONE',  ( 55.88979882644740371, -46.58799578511379735, -26.24141907459939915 ) ) ;
#23899 = CARTESIAN_POINT ( 'NONE',  ( 12.63859970449419912, -64.82257329977309723, -16.00819051994519882 ) ) ;
#23900 = CARTESIAN_POINT ( 'NONE',  ( 9.205734167420709824, -3.616188944679339823, -32.14999999999999858 ) ) ;
#23901 = CARTESIAN_POINT ( 'NONE',  ( 10.43067722519432117, -11.46704655386096938, -56.04737992177221884 ) ) ;
#23902 = CARTESIAN_POINT ( 'NONE',  ( 40.76017235305160114, -45.36108721241059527, -5.740519108723990627 ) ) ;
#23903 = ORIENTED_EDGE ( 'NONE', *, *, #8920, .T. ) ;
#23904 = CARTESIAN_POINT ( 'NONE',  ( -5.724976569056140718, -47.03139907360350236, -5.524370486448079376 ) ) ;
#23905 = CYLINDRICAL_SURFACE ( 'NONE', #51624, 2.000000000000000444 ) ;
#23906 = AXIS2_PLACEMENT_3D ( 'NONE', #6238, #50267, #51294 ) ;
#23907 = CARTESIAN_POINT ( 'NONE',  ( -0.1295185695944109927, -31.87964491196989414, -84.65000000000000568 ) ) ;
#23908 = CARTESIAN_POINT ( 'NONE',  ( 63.25550833076970747, 1.336371993404949832, -62.65916430077300703 ) ) ;
#23909 = CARTESIAN_POINT ( 'NONE',  ( 57.32084457176560477, -50.51928695062449748, -53.29702802308130316 ) ) ;
#23910 = CARTESIAN_POINT ( 'NONE',  ( 41.35617332069819696, 13.41895923659610013, -5.195208887928910002 ) ) ;
#23911 = FACE_OUTER_BOUND ( 'NONE', #40145, .T. ) ;
#23912 = CARTESIAN_POINT ( 'NONE',  ( 0.3209249304026040028, 15.01904124785189865, -34.64999999999999858 ) ) ;
#23913 = CARTESIAN_POINT ( 'NONE',  ( 57.68257350692169894, -47.11839356109889820, -47.67368955113449402 ) ) ;
#23914 = AXIS2_PLACEMENT_3D ( 'NONE', #46977, #22310, #30434 ) ;
#23915 = CARTESIAN_POINT ( 'NONE',  ( -0.007164427059776000244, -20.74946784552680157, -34.77269723891829756 ) ) ;
#23916 = CARTESIAN_POINT ( 'NONE',  ( 104.6856170952499951, -2.032350560839819131, -29.09832030244561807 ) ) ;
#23917 = CARTESIAN_POINT ( 'NONE',  ( 17.54489239063250139, -52.26337343415740122, -75.96669286083250938 ) ) ;
#23918 = PRODUCT ( 'Swivel Caster Main Housing', 'Swivel Caster Main Housing', '', ( #27517 ) ) ;
#23919 = EDGE_CURVE ( 'NONE', #37366, #45283, #1951, .T. ) ;
#23920 = CARTESIAN_POINT ( 'NONE',  ( 12.81891151941730023, -22.28831737305080196, -63.71412234440029465 ) ) ;
#23921 = CARTESIAN_POINT ( 'NONE',  ( 9.221497393660930797, -11.63191539839947808, -72.67433504022238822 ) ) ;
#23922 = CARTESIAN_POINT ( 'NONE',  ( 63.25402410758490390, 0.9098571636355720083, -62.15909090909049439 ) ) ;
#23923 = ORIENTED_EDGE ( 'NONE', *, *, #22986, .F. ) ;
#23924 = CARTESIAN_POINT ( 'NONE',  ( 22.19151943370638591, -54.02136955896735770, -34.82441657595545337 ) ) ;
#23925 = DIRECTION ( 'NONE',  ( 0.6933752452815368228, -0.7071067811865473507, -0.1386750490563055105 ) ) ;
#23926 = VECTOR ( 'NONE', #6537, 1000.000000000000000 ) ;
#23927 = CARTESIAN_POINT ( 'NONE',  ( 10.00551172459159943, -11.34028037768539932, -81.23899999999999011 ) ) ;
#23928 = EDGE_CURVE ( 'NONE', #8545, #29423, #49014, .T. ) ;
#23929 = ORIENTED_EDGE ( 'NONE', *, *, #3071, .T. ) ;
#23930 = CARTESIAN_POINT ( 'NONE',  ( 17.98857762822040129, 21.26099547410819923, -75.92929371827810314 ) ) ;
#23931 = CIRCLE ( 'NONE', #1369, 20.29675463313339989 ) ;
#23932 = VERTEX_POINT ( 'NONE', #45439 ) ;
#23933 = VERTEX_POINT ( 'NONE', #1667 ) ;
#23934 = CYLINDRICAL_SURFACE ( 'NONE', #30227, 2.000000000000058620 ) ;
#23935 = CARTESIAN_POINT ( 'NONE',  ( 22.21025937705890030, -10.69142112527120148, -81.23899999999999011 ) ) ;
#23936 = CARTESIAN_POINT ( 'NONE',  ( 8.428884598867867339, -13.54533765120538469, -72.87566484255432897 ) ) ;
#23937 = ORIENTED_EDGE ( 'NONE', *, *, #15601, .T. ) ;
#23938 = CARTESIAN_POINT ( 'NONE',  ( 9.367509928541279507, -15.61618483373539767, -35.84717978380999881 ) ) ;
#23939 = VERTEX_POINT ( 'NONE', #17656 ) ;
#23940 = LINE ( 'NONE', #37060, #29443 ) ;
#23941 = AXIS2_PLACEMENT_3D ( 'NONE', #32031, #39930, #11903 ) ;
#23942 = CARTESIAN_POINT ( 'NONE',  ( 16.13393739769620083, -15.61618894467929941, 7.944363289481099599 ) ) ;
#23943 = ORIENTED_EDGE ( 'NONE', *, *, #50562, .T. ) ;
#23945 = EDGE_LOOP ( 'NONE', ( #31435, #9353, #33470 ) ) ;
#23944 =( BOUNDED_CURVE ( )  B_SPLINE_CURVE ( 2, ( #12567, #1283, #13103 ),
 .UNSPECIFIED., .F., .T. ) 
 B_SPLINE_CURVE_WITH_KNOTS ( ( 3, 3 ),
 ( 0.1321855492373369967, 2.139356573274270090 ),
 .UNSPECIFIED. ) 
 CURVE ( )  GEOMETRIC_REPRESENTATION_ITEM ( )  RATIONAL_B_SPLINE_CURVE ( ( 1.001093714235619991, 1.008874109002009911, 1.000760730696570011 ) ) 
 REPRESENTATION_ITEM ( '' )  );
#23946 = LINE ( 'NONE', #7230, #46796 ) ;
#23947 = CARTESIAN_POINT ( 'NONE',  ( 16.13393739769620083, -15.61618894467929941, -22.14999999999999858 ) ) ;
#23948 = CARTESIAN_POINT ( 'NONE',  ( 60.86422568982110448, 14.38054746056040045, -47.60180080821060500 ) ) ;
#23949 = CIRCLE ( 'NONE', #31367, 1.000000000000000444 ) ;
#23950 = CARTESIAN_POINT ( 'NONE',  ( 22.89327904803542069, -15.26842831173307680, -40.43646614761534153 ) ) ;
#23951 = FACE_OUTER_BOUND ( 'NONE', #13007, .T. ) ;
#23952 = CARTESIAN_POINT ( 'NONE',  ( -4.838091769851679658, 16.12562087950150058, -4.829461453175369456 ) ) ;
#23953 = CARTESIAN_POINT ( 'NONE',  ( 46.36969437874859779, 21.71676560242570631, -76.14999999999999147 ) ) ;
#23954 = CARTESIAN_POINT ( 'NONE',  ( 61.12152888756239832, 13.98644838521740041, -27.50614731511399924 ) ) ;
#23955 = EDGE_CURVE ( 'NONE', #3350, #39386, #4619, .T. ) ;
#23956 = CARTESIAN_POINT ( 'NONE',  ( 11.92027290906500170, -8.995631584423939842, -60.60709014237929892 ) ) ;
#23957 = VERTEX_POINT ( 'NONE', #22597 ) ;
#23958 = AXIS2_PLACEMENT_3D ( 'NONE', #29225, #45232, #25287 ) ;
#23960 = EDGE_CURVE ( 'NONE', #17149, #14841, #4488, .T. ) ;
#23959 = DIRECTION ( 'NONE',  ( 0.7071067811865457964, 0.000000000000000000, 0.7071067811865492381 ) ) ;
#23961 = CARTESIAN_POINT ( 'NONE',  ( 12.95491128060869990, -49.88685839599860117, -82.14319696191608955 ) ) ;
#23962 = CARTESIAN_POINT ( 'NONE',  ( 53.75473964300852714, -50.98815654850967150, -75.91867185088533176 ) ) ;
#23963 = CARTESIAN_POINT ( 'NONE',  ( 72.31717656023090512, 1.061277144319840104, -69.95204556025490206 ) ) ;
#23964 = EDGE_CURVE ( 'NONE', #32183, #30264, #37935, .T. ) ;
#23965 = CARTESIAN_POINT ( 'NONE',  ( 44.00576040509109532, -39.95514525231072156, -66.63177681307838895 ) ) ;
#23966 = CARTESIAN_POINT ( 'NONE',  ( 47.19189654124329536, 23.53431858022840117, -74.50357331166900110 ) ) ;
#23967 = CARTESIAN_POINT ( 'NONE',  ( 48.76904876940009359, -54.05456627190059749, -55.30034376619679648 ) ) ;
#23968 = LINE ( 'NONE', #7770, #27275 ) ;
#23969 = CARTESIAN_POINT ( 'NONE',  ( 16.13393739769620083, -15.61618894467929941, -32.14999999999999858 ) ) ;
#23970 = DIRECTION ( 'NONE',  ( 0.000000000000000000, 0.000000000000000000, -1.000000000000000000 ) ) ;
#23971 = CARTESIAN_POINT ( 'NONE',  ( 9.715893490282427436, -18.36164609346412036, -71.71806615547141917 ) ) ;
#23972 = ORIENTED_EDGE ( 'NONE', *, *, #14607, .F. ) ;
#23973 = CARTESIAN_POINT ( 'NONE',  ( 8.744713964810220119, -16.56817550042480036, -32.02654991895249736 ) ) ;
#23974 = CARTESIAN_POINT ( 'NONE',  ( 75.47966807050509885, 12.14072485751589880, -13.40512917118210012 ) ) ;
#23975 = ORIENTED_EDGE ( 'NONE', *, *, #25928, .F. ) ;
#23976 = CARTESIAN_POINT ( 'NONE',  ( 71.58179376171669617, 0.9036513197889520788, -70.56049771322810216 ) ) ;
#23977 = CARTESIAN_POINT ( 'NONE',  ( 60.66485807962820331, -45.57220713008260304, -47.29680594952690598 ) ) ;
#23978 = AXIS2_PLACEMENT_3D ( 'NONE', #48559, #5060, #17367 ) ;
#23979 = CARTESIAN_POINT ( 'NONE',  ( 48.93508874961765542, -53.77152385436457394, -54.40024034726641844 ) ) ;
#23980 = CARTESIAN_POINT ( 'NONE',  ( -6.866062602303790285, -15.61618894467929941, 4.943674098299959851 ) ) ;
#23982 = CARTESIAN_POINT ( 'NONE',  ( 44.64648917221038715, -33.16028773000454066, -45.09461220786214142 ) ) ;
#23981 = CARTESIAN_POINT ( 'NONE',  ( 41.13211650194840274, 8.433633102539264570, -80.51793142025734085 ) ) ;
#23983 = CARTESIAN_POINT ( 'NONE',  ( 67.48834183618497207, -25.01418894467940035, -66.11905263132939581 ) ) ;
#23984 = FACE_OUTER_BOUND ( 'NONE', #30087, .T. ) ;
#23985 = EDGE_CURVE ( 'NONE', #51387, #44765, #43060, .T. ) ;
#23986 = ORIENTED_EDGE ( 'NONE', *, *, #3416, .T. ) ;
#23987 = DIRECTION ( 'NONE',  ( -0.5685928097855378338, 0.5944782866685498490, 0.5685928097855378338 ) ) ;
#23988 = B_SPLINE_CURVE_WITH_KNOTS ( 'NONE', 3,
 ( #28456, #35819, #47883, #48133, #48658, #9080, #13024, #32893, #8564, #12489, #12757, #23994, #12233, #44457, #27939, #24505, #16156, #8296 ),
 .UNSPECIFIED., .F., .F.,
 ( 4, 2, 2, 2, 2, 2, 2, 2, 4 ),
 ( 0.000000000000000000, 0.01645352784434715721, 0.1775000000366272201, 0.3375000000696457003, 0.4375000000902801167, 0.5000000001031779107, 0.6250000001289733875, 0.7632226885852325671, 1.000000000000000000 ),
 .UNSPECIFIED. ) ;
#23989 = VERTEX_POINT ( 'NONE', #38613 ) ;
#23990 = B_SPLINE_CURVE_WITH_KNOTS ( 'NONE', 3,
 ( #10321, #22349, #37121, #2969, #18943, #34923, #26282, #9085, #22606, #2713, #5163, #21118, #33167, #13284, #3999, #47769, #31744, #51693, #32002, #30986, #23626, #15282, #47012, #73, #43830, #39387, #7679, #43578, #44084, #11875, #4248, #16046, #50922, #35954, #3491 ),
 .UNSPECIFIED., .F., .F.,
 ( 4, 2, 2, 1, 1, 2, 2, 2, 1, 1, 2, 2, 2, 2, 1, 1, 1, 2, 2, 2, 4 ),
 ( 0.000000000000000000, 0.06250000000003767819, 0.09375000000005774548, 0.1093750000000684730, 0.1171875000000714567, 0.1210937500000717759, 0.1250000000000721090, 0.1875000000000927036, 0.2187500000001041944, 0.2343750000001105227, 0.2421875000001139366, 0.2500000000001173506, 0.3750000000001291744, 0.4375000000001351141, 0.4687500000001366129, 0.4843750000001361133, 0.4921875000001392220, 0.4960937500001375566, 0.5000000000001357803, 0.7500000000000679456, 1.000000000000000000 ),
 .UNSPECIFIED. ) ;
#23991 = ORIENTED_EDGE ( 'NONE', *, *, #21078, .F. ) ;
#23992 = CARTESIAN_POINT ( 'NONE',  ( 9.366365007129969555, -15.61616877484880028, -59.84717978381009118 ) ) ;
#23993 = CARTESIAN_POINT ( 'NONE',  ( 52.95041285254770003, -49.64391847752840192, -49.05228050339000134 ) ) ;
#23994 = CARTESIAN_POINT ( 'NONE',  ( 53.23465407748010847, -50.42897142312819625, -77.19488661283054398 ) ) ;
#23995 = CARTESIAN_POINT ( 'NONE',  ( 76.39397256973549588, -18.14611920900664188, -12.77057708294060490 ) ) ;
#23996 = CARTESIAN_POINT ( 'NONE',  ( 52.41075892860209962, -52.38690917609680042, -53.79179071692110625 ) ) ;
#23997 = VECTOR ( 'NONE', #16223, 1000.000000000000000 ) ;
#23998 = ORIENTED_EDGE ( 'NONE', *, *, #17509, .F. ) ;
#23999 = ORIENTED_EDGE ( 'NONE', *, *, #8621, .T. ) ;
#24000 = CARTESIAN_POINT ( 'NONE',  ( 24.04490680206547992, -15.61618865440000192, -77.79233401716611240 ) ) ;
#24001 = CARTESIAN_POINT ( 'NONE',  ( 18.13393739769620083, -37.52509124488599923, -54.64999999999999858 ) ) ;
#24002 = CARTESIAN_POINT ( 'NONE',  ( 56.35191260731789953, -50.54342274251170153, -52.86474260619870336 ) ) ;
#24003 = CARTESIAN_POINT ( 'NONE',  ( 68.13393739769620083, -33.11618894467940066, -65.65000000000000568 ) ) ;
#24004 = CARTESIAN_POINT ( 'NONE',  ( 63.16535863595050415, 0.3893935637993060084, -17.07704178728910094 ) ) ;
#24005 = CARTESIAN_POINT ( 'NONE',  ( 51.80595388240210042, -49.19315315062009830, -77.05313553807228288 ) ) ;
#24006 = VERTEX_POINT ( 'NONE', #18677 ) ;
#24007 = DIRECTION ( 'NONE',  ( 1.000000000000000000, 0.000000000000000000, 0.000000000000000000 ) ) ;
#24008 = CARTESIAN_POINT ( 'NONE',  ( 8.643744238043749917, -48.75525398023999912, -35.14999999999999858 ) ) ;
#24009 = CARTESIAN_POINT ( 'NONE',  ( 22.04673644639285257, -12.24748586501180370, -34.28812115404945615 ) ) ;
#24010 = DIRECTION ( 'NONE',  ( 0.000000000000000000, 0.000000000000000000, 1.000000000000000000 ) ) ;
#24011 = CARTESIAN_POINT ( 'NONE',  ( 23.71976105349749986, -13.60570963499520047, -49.93002833933059748 ) ) ;
#24012 = CARTESIAN_POINT ( 'NONE',  ( 12.57902733935019945, -50.33803507323350601, -21.19240466621000252 ) ) ;
#24013 = DIRECTION ( 'NONE',  ( 8.409939412270706254E-12, -1.000000000000000000, 0.000000000000000000 ) ) ;
#24014 = CARTESIAN_POINT ( 'NONE',  ( 65.43393739769584272, -48.11618894467441976, -75.95000000000109708 ) ) ;
#24015 = FACE_OUTER_BOUND ( 'NONE', #10633, .T. ) ;
#24016 = CARTESIAN_POINT ( 'NONE',  ( 0.5964323607431272212, 0.7622463544159004956, 4.943674098299870145 ) ) ;
#24017 = CARTESIAN_POINT ( 'NONE',  ( 21.48628740521269975, -11.02326954940469861, -54.62143916262389354 ) ) ;
#24018 = CARTESIAN_POINT ( 'NONE',  ( 18.34504066045640513, -52.20691909698821576, -75.61049359297886951 ) ) ;
#24019 = B_SPLINE_SURFACE_WITH_KNOTS ( 'NONE', 3, 3, ( 
 ( #30481, #30740, #32913, #48940, #28995, #35964, #23886, #27327, #11619, #43333, #11881, #31244, #23129, #43078 ),
 ( #35192, #35716, #15546, #39398, #10849, #3235, #27840, #19211, #43838, #39650, #39142, #3498, #15793, #31502 ),
 ( #47522, #51195, #31757, #27582, #7939, #42822, #35455, #7171, #30995, #22870, #15290, #47020, #7689, #47274 ),
 ( #11362, #7425, #19967, #23374, #43586, #19469, #51451, #26811, #38891, #23633, #47776, #39910, #4006, #2979 ),
 ( #3757, #19724, #81, #51701, #16052, #32008, #18953, #6918, #34931, #50932, #15028, #11108, #27072, #44066 ),
 ( #8170, #15264, #39627, #3984, #30965, #4230, #24114, #57, #35427, #27555, #16031, #7401, #47247, #40134 ),
 ( #39118, #15522, #27301, #11080, #31987, #15772, #19702, #35694, #20204, #3212, #7664, #43814, #51426, #3473 ),
 ( #51171, #46995, #23349, #50905, #14997, #28063, #48007, #23607, #27048, #23100, #12106, #43052, #47498, #7913 ),
 ( #31726, #51678, #7148, #19183, #35164, #47752, #11859, #27814, #39372, #3730, #31474, #31220, #11337, #11596 ),
 ( #43563, #43309, #19444, #23862, #39885, #19947, #35937, #9210, #40907, #12888, #36191, #28581, #37242, #44581 ) ),
 .UNSPECIFIED., .F., .F., .F.,
 ( 4, 1, 1, 1, 1, 1, 1, 4 ),
 ( 4, 2, 2, 2, 2, 2, 4 ),
 ( -0.001640340358549000066, 0.1428571428571430157, 0.2857142857142860315, 0.4285714285714289917, 0.5714285714285709528, 0.7142857142857139685, 0.8571428571428569843, 1.000038638203759822 ),
 ( -0.9741865675133749569, -0.7931653508785260209, -0.6345322807028209722, -0.5552157456149680037, -0.4283092894744039980, -0.2252589596495010171, 0.001640340358549000066 ),
 .UNSPECIFIED. ) ;
#24020 = VERTEX_POINT ( 'NONE', #35176 ) ;
#24022 = EDGE_CURVE ( 'NONE', #5342, #23957, #23356, .T. ) ;
#24021 = CARTESIAN_POINT ( 'NONE',  ( 14.15391798052560013, -51.16362366046359966, -74.57010117179498820 ) ) ;
#24023 = CARTESIAN_POINT ( 'NONE',  ( 47.39567005599690219, -54.65671969365300242, -54.74175872089709571 ) ) ;
#24024 =( LENGTH_UNIT ( ) NAMED_UNIT ( * ) SI_UNIT ( .MILLI., .METRE. ) );
#24025 = DIRECTION ( 'NONE',  ( 0.000000000000000000, 0.000000000000000000, -1.000000000000000000 ) ) ;
#24026 = CARTESIAN_POINT ( 'NONE',  ( 74.17629866868290378, -43.11618894467930119, -65.34607522167520699 ) ) ;
#24027 = CARTESIAN_POINT ( 'NONE',  ( 24.04309491136240950, -15.43172091523828193, -55.50025134836989338 ) ) ;
#24028 = TOROIDAL_SURFACE ( 'NONE', #34079, 1.499999999905649917, 0.4999999999954780061 ) ;
#24029 = CARTESIAN_POINT ( 'NONE',  ( 47.26610112325450075, -54.05804861832230301, -75.56421356201970241 ) ) ;
#24030 = CARTESIAN_POINT ( 'NONE',  ( 16.13393739769620083, -15.61618894467929941, -54.64999999999999858 ) ) ;
#24031 = CARTESIAN_POINT ( 'NONE',  ( 72.55472656186499592, 1.019773975906290042, -69.70721229073478753 ) ) ;
#24033 = CARTESIAN_POINT ( 'NONE',  ( 8.428852674553464652, -17.68692416471474615, -52.70899795959353895 ) ) ;
#24032 = DIRECTION ( 'NONE',  ( 1.000000000000000000, -6.091302000000000065E-09, -6.644969000000000155E-09 ) ) ;
#24034 = CARTESIAN_POINT ( 'NONE',  ( 16.13393739769620083, -15.61618894467929941, -18.08174999999999955 ) ) ;
#24035 = CARTESIAN_POINT ( 'NONE',  ( 49.29567348006049343, 22.45443271384029771, -54.47873722526050244 ) ) ;
#24036 = ORIENTED_EDGE ( 'NONE', *, *, #38086, .T. ) ;
#24037 = CARTESIAN_POINT ( 'NONE',  ( 53.53746104731280298, -49.37100955498770105, -49.11443482729089993 ) ) ;
#24038 = EDGE_LOOP ( 'NONE', ( #31868, #25846, #39754, #33031, #14080, #36366, #11146, #30012, #34399, #24554, #23878, #23064, #39641, #119, #28461, #27857, #38028, #49488 ) ) ;
#24039 = CARTESIAN_POINT ( 'NONE',  ( 40.94097710274119351, 6.580928486660690524, -85.72111169200137226 ) ) ;
#24040 = DIRECTION ( 'NONE',  ( 0.4156269377774524099, 0.5720614028176843613, -0.7071067811865481278 ) ) ;
#24041 = DIRECTION ( 'NONE',  ( -1.000000000000000000, 0.000000000000000000, 0.000000000000000000 ) ) ;
#24043 = CARTESIAN_POINT ( 'NONE',  ( 55.90075151227409833, 15.08720832841919979, -26.05342630048340169 ) ) ;
#24042 = CARTESIAN_POINT ( 'NONE',  ( 83.68633570933860710, 13.34091092982879978, -46.84648411755270558 ) ) ;
#24044 = CARTESIAN_POINT ( 'NONE',  ( 13.30008482799290093, -22.07465922097630084, -59.08443656163060353 ) ) ;
#24045 = CARTESIAN_POINT ( 'NONE',  ( 52.66873572145449600, 18.54828968354710028, -48.73460864874000009 ) ) ;
#24046 = CARTESIAN_POINT ( 'NONE',  ( 56.50061855793390464, -45.38130615441500026, -17.93020122267619954 ) ) ;
#24047 = EDGE_CURVE ( 'NONE', #21674, #38448, #2703, .T. ) ;
#24048 = CARTESIAN_POINT ( 'NONE',  ( 53.62552786343490396, 20.09834016026489678, -75.58099297212140755 ) ) ;
#24049 = ORIENTED_EDGE ( 'NONE', *, *, #43268, .F. ) ;
#24050 = ADVANCED_BREP_SHAPE_REPRESENTATION ( '', ( #44821, #20940 ), #10115 ) ;
#24051 = CARTESIAN_POINT ( 'NONE',  ( 23.52949167024300081, -12.99082702962889968, -43.17892530838289389 ) ) ;
#24052 = ADVANCED_FACE ( 'NONE', ( #6634 ), #19452, .F. ) ;
#24053 = ORIENTED_EDGE ( 'NONE', *, *, #17789, .T. ) ;
#24054 = CARTESIAN_POINT ( 'NONE',  ( 10.98135327145790008, -65.06876835564288797, -17.57575595872290108 ) ) ;
#24055 = CARTESIAN_POINT ( 'NONE',  ( 11.31310665686720007, 33.54695633304280022, -46.14727449326090181 ) ) ;
#24056 = CARTESIAN_POINT ( 'NONE',  ( 73.01385068780759013, 0.9098571636355680115, -62.15909090909049439 ) ) ;
#24057 = CARTESIAN_POINT ( 'NONE',  ( 49.54367864761420037, -52.88831591555140221, -52.75219176336310056 ) ) ;
#24058 = CARTESIAN_POINT ( 'NONE',  ( 10.83247370603695003, -64.53797486497589375, -23.38721072466407236 ) ) ;
#24059 = CARTESIAN_POINT ( 'NONE',  ( 8.222963953614101484, -16.65193083243917371, -64.46600189368123779 ) ) ;
#24060 = ORIENTED_EDGE ( 'NONE', *, *, #4519, .T. ) ;
#24061 = CARTESIAN_POINT ( 'NONE',  ( 11.27216563094260948, -9.290094659119313647, -74.79930795411219435 ) ) ;
#24062 = CARTESIAN_POINT ( 'NONE',  ( 10.97767197991529997, -63.11543068638779630, -44.74312619248830458 ) ) ;
#24063 = DIRECTION ( 'NONE',  ( 0.000000000000000000, 0.000000000000000000, -1.000000000000000000 ) ) ;
#24064 = ORIENTED_EDGE ( 'NONE', *, *, #41356, .T. ) ;
#24065 = CARTESIAN_POINT ( 'NONE',  ( 23.55667557762257758, -48.88697541251522694, -34.82978046822304918 ) ) ;
#24066 = CARTESIAN_POINT ( 'NONE',  ( 56.39270784037419304, 19.29512405589720103, -52.86271187285759510 ) ) ;
#24067 = CARTESIAN_POINT ( 'NONE',  ( 63.51391054266390768, 1.390208944942409985, -68.75457626026799574 ) ) ;
#24068 = FACE_OUTER_BOUND ( 'NONE', #46027, .T. ) ;
#24069 = ORIENTED_EDGE ( 'NONE', *, *, #42369, .F. ) ;
#24070 = CARTESIAN_POINT ( 'NONE',  ( 20.11804278661281487, -22.52872763293026992, -62.12566277362611089 ) ) ;
#24071 = CARTESIAN_POINT ( 'NONE',  ( 18.00872666787282839, -32.49681002921883533, -34.81767276520689336 ) ) ;
#24072 = CARTESIAN_POINT ( 'NONE',  ( 57.35590716831809743, -50.13655087819479661, -52.61987026682340485 ) ) ;
#24073 = VECTOR ( 'NONE', #13883, 1000.000000000000000 ) ;
#24074 = CARTESIAN_POINT ( 'NONE',  ( 50.51283422208840079, 21.26479333751330003, -52.94373263262310303 ) ) ;
#24075 = CARTESIAN_POINT ( 'NONE',  ( 10.63124583700320080, -21.75647441392359838, -72.52491758300199365 ) ) ;
#24076 = FACE_OUTER_BOUND ( 'NONE', #47845, .T. ) ;
#24077 = CARTESIAN_POINT ( 'NONE',  ( 56.50064219191239800, 19.52881903142939635, -74.14937127320040133 ) ) ;
#24078 = PRODUCT_CONTEXT ( 'NONE', #3339, 'mechanical' ) ;
#24079 = ORIENTED_EDGE ( 'NONE', *, *, #45414, .T. ) ;
#24080 = CARTESIAN_POINT ( 'NONE',  ( 23.08447553396189988, -18.29885803002349931, -62.34990662577889964 ) ) ;
#24081 = CARTESIAN_POINT ( 'NONE',  ( 0.1457841021255935343, -8.319710351909083812, -34.68167779225149161 ) ) ;
#24082 = CARTESIAN_POINT ( 'NONE',  ( 12.26068851955660044, -22.47136919790400000, -32.14999999999999858 ) ) ;
#24084 = EDGE_CURVE ( 'NONE', #10936, #9424, #50508, .T. ) ;
#24083 = CARTESIAN_POINT ( 'NONE',  ( 46.54864319858230459, 22.04971653235029905, -76.11254988220410667 ) ) ;
#24085 = DIRECTION ( 'NONE',  ( -1.000000000000000000, 0.000000000000000000, 0.000000000000000000 ) ) ;
#24086 = CYLINDRICAL_SURFACE ( 'NONE', #49854, 13.50000000000000178 ) ;
#24087 =( BOUNDED_CURVE ( )  B_SPLINE_CURVE ( 2, ( #19669, #2666, #11309, #23073, #43025 ),
 .UNSPECIFIED., .F., .T. ) 
 B_SPLINE_CURVE_WITH_KNOTS ( ( 3, 2, 3 ),
 ( -0.003205554299145560102, 0.8238407534178779912, 1.650887061134900025 ),
 .UNSPECIFIED. ) 
 CURVE ( )  GEOMETRIC_REPRESENTATION_ITEM ( )  RATIONAL_B_SPLINE_CURVE ( ( 1.000000000000000000, 0.9157107718028779653, 1.000000000000000000, 0.9157107718028449916, 1.000000000000000000 ) ) 
 REPRESENTATION_ITEM ( '' )  );
#24088 = CARTESIAN_POINT ( 'NONE',  ( 12.17681940038050037, 33.64169525760830481, -16.15032133962059646 ) ) ;
#24089 = CARTESIAN_POINT ( 'NONE',  ( 17.91047190612059836, -23.66768854721899729, -77.93854215477199432 ) ) ;
#24090 = CARTESIAN_POINT ( 'NONE',  ( 54.86175947632980154, -50.65972080371189890, -76.24591593276051071 ) ) ;
#24092 = CARTESIAN_POINT ( 'NONE',  ( 61.00258867160625442, -28.71632116457892181, -42.47246584482020637 ) ) ;
#24091 = CYLINDRICAL_SURFACE ( 'NONE', #49992, 0.4999999999999986677 ) ;
#24093 = CARTESIAN_POINT ( 'NONE',  ( 63.45501836690030473, 1.383357884654609959, -68.68594134708139620 ) ) ;
#24094 = CARTESIAN_POINT ( 'NONE',  ( 61.37578811247220045, 13.95917485428159921, -46.55532700619050246 ) ) ;
#24095 = CARTESIAN_POINT ( 'NONE',  ( 76.87859684847769870, -43.11619168008749625, -14.85884840380859906 ) ) ;
#24096 = DIRECTION ( 'NONE',  ( 0.000000000000000000, 0.000000000000000000, 1.000000000000000000 ) ) ;
#24097 = ORIENTED_EDGE ( 'NONE', *, *, #47117, .F. ) ;
#24098 = CARTESIAN_POINT ( 'NONE',  ( 52.94089229371839878, -49.60269320154350225, -48.75998159659980047 ) ) ;
#24099 = CIRCLE ( 'NONE', #14939, 31.45861873485090143 ) ;
#24100 = CARTESIAN_POINT ( 'NONE',  ( 59.06502219811700627, -45.32330029555010498, -26.35699478639849858 ) ) ;
#24101 = CARTESIAN_POINT ( 'NONE',  ( 21.73328479000853264, -21.28338846926865102, -66.04403864357212228 ) ) ;
#24102 = CARTESIAN_POINT ( 'NONE',  ( 56.59921044315609606, 14.68325417103389974, -26.17131425341809958 ) ) ;
#24103 = CARTESIAN_POINT ( 'NONE',  ( 13.09279613430840072, -22.41752363878649845, -74.86649773383079776 ) ) ;
#24104 = CARTESIAN_POINT ( 'NONE',  ( 50.62459437698230147, 18.71911933297949915, -76.16377488163089993 ) ) ;
#24105 = CARTESIAN_POINT ( 'NONE',  ( 52.75872642489079567, 18.46922250474269944, -48.48805342991609990 ) ) ;
#24106 = CARTESIAN_POINT ( 'NONE',  ( 71.26289196806200721, 1.269319268680890067, -70.56549354633131088 ) ) ;
#24107 = CARTESIAN_POINT ( 'NONE',  ( 40.64814218619559938, -44.65225711300980294, -4.018323718197329697 ) ) ;
#24108 = ORIENTED_EDGE ( 'NONE', *, *, #36414, .T. ) ;
#24109 = CARTESIAN_POINT ( 'NONE',  ( 20.13393739083949896, -55.41568640430479320, -20.65000000000000213 ) ) ;
#24110 = EDGE_CURVE ( 'NONE', #14613, #44797, #43007, .T. ) ;
#24111 = CARTESIAN_POINT ( 'NONE',  ( 47.78329665909949853, -54.43353293614439536, -54.80119951604820017 ) ) ;
#24112 = CARTESIAN_POINT ( 'NONE',  ( -7.653322382745200159, 14.02129102307469921, -4.959142631146099767 ) ) ;
#24113 = LINE ( 'NONE', #51425, #17700 ) ;
#24114 = CARTESIAN_POINT ( 'NONE',  ( 61.41002981261989646, -30.19755464412979862, -16.14587537362810110 ) ) ;
#24115 = CARTESIAN_POINT ( 'NONE',  ( 71.45332619318591583, 1.096305581841150012, -60.69897858480909747 ) ) ;
#24116 = CARTESIAN_POINT ( 'NONE',  ( 2.464092196720385708, -25.62390951037214037, -34.77490583097451804 ) ) ;
#24117 = CARTESIAN_POINT ( 'NONE',  ( 72.33986051001160433, 1.456055805561079941, -61.71730126733579169 ) ) ;
#24118 = CARTESIAN_POINT ( 'NONE',  ( 22.38486747247302233, -18.84477224106433724, -40.99906234112837922 ) ) ;
#24119 = CARTESIAN_POINT ( 'NONE',  ( 65.12253294394879788, 1.334812829108570131, -70.51979614837409827 ) ) ;
#24120 = ORIENTED_EDGE ( 'NONE', *, *, #49422, .T. ) ;
#24121 = ORIENTED_EDGE ( 'NONE', *, *, #17903, .T. ) ;
#24122 = CARTESIAN_POINT ( 'NONE',  ( 72.33393739769574893, 11.38368607098449914, -62.44999999999853202 ) ) ;
#24123 = CARTESIAN_POINT ( 'NONE',  ( 10.22108902069157210, -19.02428818417996581, -59.28615350234715464 ) ) ;
#24124 = ORIENTED_EDGE ( 'NONE', *, *, #17615, .F. ) ;
#24125 = CARTESIAN_POINT ( 'NONE',  ( 55.82582291612180114, -46.03321360888129732, -25.33858244797220038 ) ) ;
#24126 = CARTESIAN_POINT ( 'NONE',  ( 53.81599905896988645, 20.06114670800089428, -75.54047393059830995 ) ) ;
#24128 = ORIENTED_EDGE ( 'NONE', *, *, #22352, .T. ) ;
#24127 = B_SPLINE_CURVE_WITH_KNOTS ( 'NONE', 3,
 ( #39100, #50113, #46717, #3193 ),
 .UNSPECIFIED., .F., .F.,
 ( 4, 4 ),
 ( 0.000000000000000000, 1.000000000000000000 ),
 .UNSPECIFIED. ) ;
#24129 = DIRECTION ( 'NONE',  ( 1.000000000000000000, 0.000000000000000000, 0.000000000000000000 ) ) ;
#24130 = CARTESIAN_POINT ( 'NONE',  ( 42.43208337334868929, 6.460128661955979013, -78.15925233081755152 ) ) ;
#24131 = CARTESIAN_POINT ( 'NONE',  ( 23.18974198866444070, -19.29653021243158051, -65.66053363189716663 ) ) ;
#24132 = B_SPLINE_CURVE_WITH_KNOTS ( 'NONE', 3,
 ( #13266, #29222, #20575, #48378, #25284, #21355, #4349, #48913, #28443, #12220 ),
 .UNSPECIFIED., .F., .F.,
 ( 4, 2, 2, 2, 4 ),
 ( -0.1799215976184830035, -0.1795414484421369861, -0.1664059944892330167, -0.1383522341548960033, -0.1329710036333066059 ),
 .UNSPECIFIED. ) ;
#24133 = CARTESIAN_POINT ( 'NONE',  ( 8.236591511843410984, -17.98571379475770016, -46.69954605626199395 ) ) ;
#24134 = CARTESIAN_POINT ( 'NONE',  ( 45.34397758664299971, 2.696163290909390220, -34.64999999999999858 ) ) ;
#24135 = CARTESIAN_POINT ( 'NONE',  ( 23.89322328078525004, -17.19759884022353447, -49.85630258065442177 ) ) ;
#24136 = DIRECTION ( 'NONE',  ( 1.000000000000000000, 0.000000000000000000, 0.000000000000000000 ) ) ;
#24137 = EDGE_LOOP ( 'NONE', ( #22972, #767 ) ) ;
#24138 = CARTESIAN_POINT ( 'NONE',  ( 11.10346939884210116, -64.31936717124580127, -23.87841574096529840 ) ) ;
#24139 = CARTESIAN_POINT ( 'NONE',  ( 13.63771406388430130, -22.63584441150059945, -36.84141082329339412 ) ) ;
#24140 = CIRCLE ( 'NONE', #33371, 1.500000000000001332 ) ;
#24141 = CARTESIAN_POINT ( 'NONE',  ( 41.02377769398490415, 13.92370008184540175, -5.717048413919049388 ) ) ;
#24142 = AXIS2_PLACEMENT_3D ( 'NONE', #17593, #48272, #8443 ) ;
#24143 = EDGE_CURVE ( 'NONE', #30210, #17198, #25763, .T. ) ;
#24144 = CARTESIAN_POINT ( 'NONE',  ( 14.27678794190400069, 20.53764257940400029, -75.58342519351550948 ) ) ;
#24145 = CARTESIAN_POINT ( 'NONE',  ( 24.01641782975098849, -16.30113512706325096, -59.81990940572667625 ) ) ;
#24146 = EDGE_CURVE ( 'NONE', #24756, #32096, #45847, .T. ) ;
#24147 = CARTESIAN_POINT ( 'NONE',  ( 83.20652121431659509, -45.06907107880329733, -47.10047235024320145 ) ) ;
#24148 = CARTESIAN_POINT ( 'NONE',  ( 10.89208569013780448, 33.76849054883776802, -17.57297834644989720 ) ) ;
#24149 = EDGE_CURVE ( 'NONE', #9856, #41648, #67, .T. ) ;
#24150 = CARTESIAN_POINT ( 'NONE',  ( 12.53949280675929856, -8.195765183757039551, -40.86408241699819399 ) ) ;
#24151 = VERTEX_POINT ( 'NONE', #12117 ) ;
#24152 = CARTESIAN_POINT ( 'NONE',  ( 52.72304479398140131, -49.72255302625990225, -28.01707846523380141 ) ) ;
#24153 = CARTESIAN_POINT ( 'NONE',  ( 11.23965435610889863, -65.13936513006379414, -17.15438869215460116 ) ) ;
#24154 = CARTESIAN_POINT ( 'NONE',  ( 17.41362677703381934, -23.45504930627769369, -39.95607996559230202 ) ) ;
#24155 = CARTESIAN_POINT ( 'NONE',  ( 24.04493742283841584, -16.65172811301406597, -63.83400030080247944 ) ) ;
#24156 = CARTESIAN_POINT ( 'NONE',  ( 75.45730910492666510, 12.50011331391788794, -13.48270834329013645 ) ) ;
#24157 = CARTESIAN_POINT ( 'NONE',  ( 12.86227365712040083, -49.99703836812659574, -21.07384430750599691 ) ) ;
#24158 = ORIENTED_EDGE ( 'NONE', *, *, #22106, .T. ) ;
#24159 = CARTESIAN_POINT ( 'NONE',  ( -6.571053818291229476, -46.36898988238050379, -5.603118524855751126 ) ) ;
#24160 = CARTESIAN_POINT ( 'NONE',  ( 47.21165009223999931, 23.55238375380269744, -54.63209248662939643 ) ) ;
#24161 = EDGE_CURVE ( 'NONE', #15474, #2233, #27079, .T. ) ;
#24162 = CARTESIAN_POINT ( 'NONE',  ( 17.40001803049475981, 18.38378339404363970, -83.20618638369494136 ) ) ;
#24163 = CARTESIAN_POINT ( 'NONE',  ( 63.34531745652139989, 1.374300485541529948, -62.71457717039259450 ) ) ;
#24164 = CARTESIAN_POINT ( 'NONE',  ( 57.30262416817789983, -50.51992209788300414, -53.29749893028549934 ) ) ;
#24165 = CARTESIAN_POINT ( 'NONE',  ( 42.74124889056859899, 12.81040389201469942, -5.015693368315670142 ) ) ;
#24166 = DIRECTION ( 'NONE',  ( 0.8660254037844387076, 0.4999999999999998890, 2.775557561562889194E-17 ) ) ;
#24167 = CYLINDRICAL_SURFACE ( 'NONE', #30816, 40.00000000000000711 ) ;
#24168 = CARTESIAN_POINT ( 'NONE',  ( 53.80794059781069194, -49.14842230199280237, -48.63343936029099979 ) ) ;
#24169 = DIRECTION ( 'NONE',  ( 0.000000000000000000, 0.000000000000000000, -1.000000000000000000 ) ) ;
#24170 = FACE_OUTER_BOUND ( 'NONE', #16120, .T. ) ;
#24171 = CARTESIAN_POINT ( 'NONE',  ( 17.21347160910390173, -53.11618894467930119, -76.14999999999999147 ) ) ;
#24172 = EDGE_CURVE ( 'NONE', #29814, #29423, #3639, .T. ) ;
#24173 = CARTESIAN_POINT ( 'NONE',  ( 8.222342146248220018, -15.61610160653870061, -76.79233150823698395 ) ) ;
#24174 = AXIS2_PLACEMENT_3D ( 'NONE', #43766, #3943, #7871 ) ;
#24175 = CARTESIAN_POINT ( 'NONE',  ( 9.659254613363348341, -12.81954403390899877, -81.58261298369839665 ) ) ;
#24176 = CARTESIAN_POINT ( 'NONE',  ( 63.37668255464280520, 1.045341414535140068, -62.00499031178430442 ) ) ;
#24177 = ORIENTED_EDGE ( 'NONE', *, *, #23253, .F. ) ;
#24178 = FACE_OUTER_BOUND ( 'NONE', #41297, .T. ) ;
#24179 = CARTESIAN_POINT ( 'NONE',  ( 22.13393739769589885, 22.91950879131610108, -35.14999999999999858 ) ) ;
#24180 = CARTESIAN_POINT ( 'NONE',  ( 68.13393739769620083, 18.13381105532069881, -71.50000000000000000 ) ) ;
#24181 = AXIS2_PLACEMENT_3D ( 'NONE', #20032, #35781, #11431 ) ;
#24182 = AXIS2_PLACEMENT_3D ( 'NONE', #33858, #25215, #41220 ) ;
#24183 = CARTESIAN_POINT ( 'NONE',  ( 8.995234134042298990, -14.54159774915980030, -81.23899999999999011 ) ) ;
#24184 = ORIENTED_EDGE ( 'NONE', *, *, #6924, .T. ) ;
#24185 = CARTESIAN_POINT ( 'NONE',  ( 17.33622727253819917, 21.74151571116259873, -76.14999999999999147 ) ) ;
#24186 = ORIENTED_EDGE ( 'NONE', *, *, #39971, .F. ) ;
#24187 = ORIENTED_EDGE ( 'NONE', *, *, #7030, .F. ) ;
#24188 = CARTESIAN_POINT ( 'NONE',  ( 57.42983846519040725, -45.73690961613799999, -26.26079255916740252 ) ) ;
#24189 = CARTESIAN_POINT ( 'NONE',  ( 21.88702750807829744, -19.77779051261680010, -81.23899999999999011 ) ) ;
#24190 = CARTESIAN_POINT ( 'NONE',  ( 61.71598194884530386, 13.91966528094189925, -46.75058645329289675 ) ) ;
#24191 = EDGE_CURVE ( 'NONE', #16668, #32963, #18702, .T. ) ;
#24192 = CARTESIAN_POINT ( 'NONE',  ( 19.32514136844950059, -21.90576575011689897, -69.19772247832989365 ) ) ;
#24193 = CARTESIAN_POINT ( 'NONE',  ( 12.09990269636916871, 34.01294328777810705, -16.83009735979323196 ) ) ;
#24194 = EDGE_LOOP ( 'NONE', ( #38146, #49390, #18680, #8092 ) ) ;
#24195 = PLANE ( 'NONE',  #34448 ) ;
#24196 = DIRECTION ( 'NONE',  ( -1.000000000000000000, 0.000000000000000000, 0.000000000000000000 ) ) ;
#24197 = VERTEX_POINT ( 'NONE', #24384 ) ;
#24198 = VERTEX_POINT ( 'NONE', #11867 ) ;
#24199 = CARTESIAN_POINT ( 'NONE',  ( 72.13393739769620083, -1.116188944679340045, -20.65000000000000213 ) ) ;
#24200 = CARTESIAN_POINT ( 'NONE',  ( 22.90065656494205726, -15.61616387038935017, -34.45281736178981902 ) ) ;
#24201 = CARTESIAN_POINT ( 'NONE',  ( 61.16964974363649787, 14.21611140120430150, -47.43903885526910358 ) ) ;
#24202 = CARTESIAN_POINT ( 'NONE',  ( 49.03396268060160423, 14.94209610719759951, -11.76399786255080038 ) ) ;
#24203 = CARTESIAN_POINT ( 'NONE',  ( -10.89822638436359981, 11.09799366564529954, -6.199143116420779975 ) ) ;
#24204 = CIRCLE ( 'NONE', #9176, 5.999999999999998224 ) ;
#24205 = VECTOR ( 'NONE', #25626, 1000.000000000000114 ) ;
#24206 = CIRCLE ( 'NONE', #19230, 7.910999999999997812 ) ;
#24207 = DIRECTION ( 'NONE',  ( 0.000000000000000000, 0.000000000000000000, -1.000000000000000000 ) ) ;
#24208 = CARTESIAN_POINT ( 'NONE',  ( 60.57156752678139355, 14.04241620716539884, -27.07292534466720113 ) ) ;
#24209 = CIRCLE ( 'NONE', #45997, 40.00000000000000711 ) ;
#24210 = EDGE_CURVE ( 'NONE', #21618, #28327, #22879, .T. ) ;
#24211 = CARTESIAN_POINT ( 'NONE',  ( 23.77775089882910109, -17.39350808965049922, -65.36022600619639888 ) ) ;
#24212 = ORIENTED_EDGE ( 'NONE', *, *, #7221, .T. ) ;
#24213 = CARTESIAN_POINT ( 'NONE',  ( 53.41693480164789776, 18.12090330447900044, -48.75416851879769808 ) ) ;
#24214 = CARTESIAN_POINT ( 'NONE',  ( 22.90093739769620029, -15.61618894467913243, -28.45282021618999835 ) ) ;
#24215 = CARTESIAN_POINT ( 'NONE',  ( 11.65854852791870044, 33.64587830465290352, -45.04862363297149841 ) ) ;
#24216 = CARTESIAN_POINT ( 'NONE',  ( 72.40210087067039524, 1.451792515613489876, -69.49977495595670973 ) ) ;
#24217 = CARTESIAN_POINT ( 'NONE',  ( 42.61000615344636344, -39.82798686284615997, -73.38501703869289372 ) ) ;
#24218 = DIRECTION ( 'NONE',  ( 0.000000000000000000, 0.000000000000000000, -1.000000000000000000 ) ) ;
#24219 = B_SPLINE_CURVE_WITH_KNOTS ( 'NONE', 3,
 ( #10430, #14352, #1781, #2041, #41876, #42139, #2300, #41610 ),
 .UNSPECIFIED., .F., .F.,
 ( 4, 2, 2, 4 ),
 ( -0.1329710036334196266, -0.1164701438936319999, -0.09932952752696240506, -0.09339196852981200558 ),
 .UNSPECIFIED. ) ;
#24220 = CARTESIAN_POINT ( 'NONE',  ( 47.20049209618989750, 23.55315852235050045, -74.36225199019699517 ) ) ;
#24221 = CARTESIAN_POINT ( 'NONE',  ( 48.48681609642030566, -54.13994113942329278, -54.95545728264639962 ) ) ;
#24222 = CARTESIAN_POINT ( 'NONE',  ( 51.51228236258946680, -32.18033297859199138, -17.73310860033575764 ) ) ;
#24223 = DIRECTION ( 'NONE',  ( 0.000000000000000000, 0.000000000000000000, -1.000000000000000000 ) ) ;
#24224 = CARTESIAN_POINT ( 'NONE',  ( 71.33393739769628894, 11.38381102407070067, -69.35012499995160340 ) ) ;
#24225 = CARTESIAN_POINT ( 'NONE',  ( 24.04493320937934442, -15.61618918076996110, -53.79232900421944663 ) ) ;
#24226 = EDGE_LOOP ( 'NONE', ( #41813, #21372, #13004, #30749, #41023 ) ) ;
#24227 = CARTESIAN_POINT ( 'NONE',  ( 22.31020800752009947, -11.44961052869560092, -34.87843143724279571 ) ) ;
#24228 = CARTESIAN_POINT ( 'NONE',  ( 64.75444473847480253, 1.309114013480900063, -60.92108349576849946 ) ) ;
#24229 = VERTEX_POINT ( 'NONE', #7672 ) ;
#24230 = CARTESIAN_POINT ( 'NONE',  ( 71.53768886009270034, 0.9325382164350239922, -70.59115830928880087 ) ) ;
#24231 = CARTESIAN_POINT ( 'NONE',  ( 61.06210316266220417, -45.44419311714590748, -47.37017503401310137 ) ) ;
#24232 = CARTESIAN_POINT ( 'NONE',  ( 17.98749448546710994, -32.47778390180250341, -34.79644291222910368 ) ) ;
#24233 = DIRECTION ( 'NONE',  ( -1.451273000000000212E-17, 7.532081000000000189E-18, -1.000000000000000000 ) ) ;
#24235 = CARTESIAN_POINT ( 'NONE',  ( 9.807739393606267342, -20.47782491541499894, -78.58399752127002102 ) ) ;
#24234 = CARTESIAN_POINT ( 'NONE',  ( 42.21481387295106913, 8.555122854874271709, -75.29414714603025516 ) ) ;
#24236 = CARTESIAN_POINT ( 'NONE',  ( 30.26439304108700412, 4.386381194870886624, -84.60847545484261900 ) ) ;
#24237 = CARTESIAN_POINT ( 'NONE',  ( 20.99561924099482013, -21.94235114381296725, -51.79933308495947841 ) ) ;
#24238 = EDGE_LOOP ( 'NONE', ( #4555, #29943, #14702, #24186, #33888 ) ) ;
#24239 = CARTESIAN_POINT ( 'NONE',  ( 83.87142430054410625, -44.85900700689950327, -47.47134017317799959 ) ) ;
#24240 = ORIENTED_EDGE ( 'NONE', *, *, #25179, .T. ) ;
#24241 = ORIENTED_EDGE ( 'NONE', *, *, #48396, .T. ) ;
#24242 = EDGE_LOOP ( 'NONE', ( #48860, #45248, #22733, #31286, #955, #23021 ) ) ;
#24243 = DIRECTION ( 'NONE',  ( 0.000000000000000000, 0.000000000000000000, -1.000000000000000000 ) ) ;
#24244 = AXIS2_PLACEMENT_3D ( 'NONE', #21313, #21054, #9548 ) ;
#24245 = CARTESIAN_POINT ( 'NONE',  ( 11.53605495837543948, -55.35105376503654639, -21.73576846289474318 ) ) ;
#24246 = AXIS2_PLACEMENT_3D ( 'NONE', #39793, #11511, #31644 ) ;
#24247 = CARTESIAN_POINT ( 'NONE',  ( 76.42290226885830862, -8.715687769802094920, -12.89519280475484209 ) ) ;
#24248 = CARTESIAN_POINT ( 'NONE',  ( 49.80812477255949489, -53.32727295909180043, -54.05131971329959839 ) ) ;
#24249 = VECTOR ( 'NONE', #11144, 1000.000000000000000 ) ;
#24250 = ORIENTED_EDGE ( 'NONE', *, *, #36357, .T. ) ;
#24251 = ADVANCED_FACE ( 'NONE', ( #48269 ), #40399, .T. ) ;
#24252 = ORIENTED_EDGE ( 'NONE', *, *, #19220, .T. ) ;
#24253 = CIRCLE ( 'NONE', #20907, 16.50000000000000000 ) ;
#24254 = VECTOR ( 'NONE', #23880, 1000.000000000000114 ) ;
#24255 = CARTESIAN_POINT ( 'NONE',  ( -0.05020173012252868855, 14.40722748145230980, -34.80983693937416490 ) ) ;
#24256 = B_SPLINE_CURVE_WITH_KNOTS ( 'NONE', 3,
 ( #27431, #11474, #35820, #43434, #50784, #14874, #35032, #3345, #19321, #26648, #7537, #42667, #6767, #22719, #42925, #51038, #47375, #35302, #51300, #7023, #23482, #22975, #3605, #19576, #44199, #28715, #28980, #40782, #40273, #28458, #11987, #24507, #8822, #48392, #44458, #20081, #8041, #44979, #4361, #9081, #16158, #4103, #12490, #32116, #23995, #15911, #40016, #47884, #51805, #31867, #48134, #27940, #43945, #36073, #32895, #32373, #685, #25029, #12234, #44716, #431, #41045, #179, #8565, #24773, #36320, #36582, #4884, #20332, #13026, #28196, #8297, #24247, #5158, #21827, #16417, #953, #40526, #4618, #20588, #48927, #16673, #32632, #48659, #12758, #16949, #20850, #36849, #17908, #26794, #30209, #10828, #38346, #38614, #38089, #14493, #7160, #42805, #2185, #18419, #22340, #6379, #50140, #18165, #33877, #10314, #6901, #42545, #30465, #46225, #14753, #15008, #22852, #26275, #46485, #49890, #10574, #46746 ),
 .UNSPECIFIED., .F., .F.,
 ( 4, 2, 1, 1, 1, 2, 2, 1, 2, 2, 2, 1, 1, 1, 1, 1, 1, 1, 2, 2, 2, 2, 2, 1, 1, 1, 1, 1, 2, 2, 2, 2, 1, 1, 2, 2, 2, 2, 1, 1, 2, 2, 1, 1, 1, 1, 2, 2, 1, 1, 1, 1, 2, 2, 1, 1, 2, 2, 2, 1, 1, 1, 1, 2, 2, 1, 1, 2, 2, 2, 1, 2, 2, 1, 1, 1, 1, 1, 2, 4 ),
 ( 0.000000000000000000, 0.2499999999972345455, 0.2812499999968888775, 0.2968749999967161268, 0.2988281249966943665, 0.2998046874966834863, 0.3007812499966726616, 0.3046874999966289188, 0.3124999999965417663, 0.3437499999961932118, 0.3593749999960189068, 0.3671874999959318098, 0.3710937499958883445, 0.3730468749958665287, 0.3740234374958556485, 0.3745117187458500418, 0.3747558593708472663, 0.3748779296833459895, 0.3749389648395953789, 0.3749999999958447683, 0.4062499999955537788, 0.4218749999954082286, 0.4296874999953354535, 0.4335937499952993157, 0.4355468749952812746, 0.4365234374952717822, 0.4370117187452666196, 0.4372558593702645102, 0.4373779296827634555, 0.4374999999952623453, 0.4687499999950052731, 0.4843749999948768759, 0.4921874999948127605, 0.4960937499947808416, 0.4980468749947649099, 0.4999999999947489782, 0.5312499999944939599, 0.5390624999944302331, 0.5429687499943983697, 0.5449218749943823825, 0.5458984374943743889, 0.5468749999943663953, 0.5624999999942384976, 0.5781249999941105999, 0.5859374999940466511, 0.5898437499940146767, 0.5917968749939988005, 0.5937499999939828133, 0.6249999999937280171, 0.6562499999934733319, 0.6601562499934414685, 0.6621093749934254813, 0.6630859374934174877, 0.6633300781184153783, 0.6635742187434133799, 0.6640624999934093831, 0.6718749999933307793, 0.6874999999931732386, 0.7187499999928583794, 0.7226562499928189665, 0.7236328124928091965, 0.7241210937428042005, 0.7243652343678017580, 0.7244873046803005368, 0.7245483398365499816, 0.7246093749927994265, 0.7265624999928507188, 0.7343749999930548888, 0.7499999999934631179, 0.7812499999942796869, 0.7851562499943818274, 0.7856445312443947060, 0.7858886718694010343, 0.7861328124944074736, 0.7871093749944330087, 0.7890624999944840789, 0.7968749999946883600, 0.8124999999950969221, 0.8749999999967311703, 1.000000000000000000 ),
 .UNSPECIFIED. ) ;
#24257 = CARTESIAN_POINT ( 'NONE',  ( 57.20754666121199961, -45.13815381503769686, -25.31149905167690051 ) ) ;
#24258 = ADVANCED_FACE ( 'NONE', ( #19954 ), #39449, .F. ) ;
#24259 = CARTESIAN_POINT ( 'NONE',  ( 16.13393739769620083, -15.61618894467929941, -5.740514720465069942 ) ) ;
#24260 = LINE ( 'NONE', #4626, #45355 ) ;
#24261 = CARTESIAN_POINT ( 'NONE',  ( 24.04424252334385059, -15.50293471796945610, -59.78776946088952116 ) ) ;
#24262 = CARTESIAN_POINT ( 'NONE',  ( 52.15299206959110023, -49.68190268104039831, -77.15977264154089710 ) ) ;
#24263 = EDGE_CURVE ( 'NONE', #19930, #19589, #3325, .T. ) ;
#24264 = ORIENTED_EDGE ( 'NONE', *, *, #38951, .T. ) ;
#24265 = DIRECTION ( 'NONE',  ( 1.000000000000000000, 0.000000000000000000, 0.000000000000000000 ) ) ;
#24266 = CARTESIAN_POINT ( 'NONE',  ( 52.97782969051129953, -50.30123836914950175, -77.23919107196950051 ) ) ;
#24267 = CARTESIAN_POINT ( 'NONE',  ( 64.64302830678670375, 0.9098571636355720083, -70.52991329011129551 ) ) ;
#24268 = DIRECTION ( 'NONE',  ( 0.000000000000000000, 1.000000000000000000, 0.000000000000000000 ) ) ;
#24269 = CARTESIAN_POINT ( 'NONE',  ( 21.13707352621340263, -9.570084705492890365, -53.73253703038420070 ) ) ;
#24270 = CARTESIAN_POINT ( 'NONE',  ( 13.39861581086750064, -50.35706945913049992, -21.14264498997030017 ) ) ;
#24271 = CARTESIAN_POINT ( 'NONE',  ( -3.779114556262074487, -11.36736946467367204, -59.64999999999999147 ) ) ;
#24272 = DIRECTION ( 'NONE',  ( -1.000000000000000000, 0.000000000000000000, 0.000000000000000000 ) ) ;
#24273 = CIRCLE ( 'NONE', #1711, 10.00000000000000355 ) ;
#24274 = CARTESIAN_POINT ( 'NONE',  ( 57.41961282339919848, 13.88381105532070059, -17.93020877507790090 ) ) ;
#24275 = DIRECTION ( 'NONE',  ( 0.000000000000000000, 0.000000000000000000, 1.000000000000000000 ) ) ;
#24276 = CARTESIAN_POINT ( 'NONE',  ( 10.72264165131508129, -19.77489046754428159, -39.24448753485003749 ) ) ;
#24277 = CARTESIAN_POINT ( 'NONE',  ( 15.19249895237999937, -8.626464141217319082, -54.30456343836939936 ) ) ;
#24278 = DIRECTION ( 'NONE',  ( 0.000000000000000000, 0.000000000000000000, 1.000000000000000000 ) ) ;
#24279 = ADVANCED_FACE ( 'NONE', ( #9727 ), #14698, .T. ) ;
#24280 = ORIENTED_EDGE ( 'NONE', *, *, #1662, .F. ) ;
#24281 = CARTESIAN_POINT ( 'NONE',  ( 14.34345188046069985, -51.57142019855179882, -75.41551559479479749 ) ) ;
#24282 = CARTESIAN_POINT ( 'NONE',  ( 47.36437953800110279, -54.67829754402429643, -54.76347716479679661 ) ) ;
#24283 = VECTOR ( 'NONE', #4311, 1000.000000000000000 ) ;
#24284 = CARTESIAN_POINT ( 'NONE',  ( 12.82231730657736257, 34.27273057154334879, -47.70638112244893136 ) ) ;
#24285 = CARTESIAN_POINT ( 'NONE',  ( 9.629521756913746344, -18.06914890294566689, -77.73182532936149869 ) ) ;
#24286 = CIRCLE ( 'NONE', #2548, 17.39999999999999503 ) ;
#24287 = CARTESIAN_POINT ( 'NONE',  ( 60.92101825946003402, -45.44428967124540009, -47.19725562356851611 ) ) ;
#24288 = AXIS2_PLACEMENT_3D ( 'NONE', #13790, #36850, #29747 ) ;
#24289 = VECTOR ( 'NONE', #27573, 1000.000000000000000 ) ;
#24291 = AXIS2_PLACEMENT_3D ( 'NONE', #14360, #41616, #29300 ) ;
#24290 = DIRECTION ( 'NONE',  ( 0.000000000000000000, 0.000000000000000000, -1.000000000000000000 ) ) ;
#24292 = CARTESIAN_POINT ( 'NONE',  ( 10.63085527536540020, 33.60671078422439706, -18.12439166827990178 ) ) ;
#24294 = CARTESIAN_POINT ( 'NONE',  ( 12.35956436866795727, -50.22963602464601962, -21.15000000006194369 ) ) ;
#24293 = CARTESIAN_POINT ( 'NONE',  ( 16.13393739769620083, -15.61618894467929941, -643.2998782751060389 ) ) ;
#24295 = CARTESIAN_POINT ( 'NONE',  ( 46.13393739769619373, 4.883811055320659733, -81.65000000000000568 ) ) ;
#24296 = CARTESIAN_POINT ( 'NONE',  ( 48.46943201930690037, 22.93089287882050087, -55.04752992213770568 ) ) ;
#24297 = ORIENTED_EDGE ( 'NONE', *, *, #36750, .T. ) ;
#24298 = CARTESIAN_POINT ( 'NONE',  ( 52.69326468654779205, -49.76107638029880320, -48.74393324173220066 ) ) ;
#24299 = EDGE_LOOP ( 'NONE', ( #9347, #26337 ) ) ;
#24300 = CARTESIAN_POINT ( 'NONE',  ( 18.67893569163094725, -51.93861847160620471, -75.09855816265704220 ) ) ;
#24301 = CARTESIAN_POINT ( 'NONE',  ( 8.223401571539490362, -15.61634053766229968, -58.50766849176299900 ) ) ;
#24302 = CARTESIAN_POINT ( 'NONE',  ( 16.13393739769620083, -15.61618894467929941, -5.690000000000000391 ) ) ;
#24304 = CARTESIAN_POINT ( 'NONE',  ( 54.31423360305029746, 16.85098597931899889, -26.53140032282190219 ) ) ;
#24303 = CARTESIAN_POINT ( 'NONE',  ( 82.49223220840640636, 13.86914553491480007, -46.59234684980529551 ) ) ;
#24305 = CARTESIAN_POINT ( 'NONE',  ( 19.58154494863300243, -9.463420391308439150, -68.11539470288319364 ) ) ;
#24306 = CARTESIAN_POINT ( 'NONE',  ( 52.67899906575139113, 18.54202610784680161, -48.75316747057349431 ) ) ;
#24307 = CARTESIAN_POINT ( 'NONE',  ( 56.44084032582000532, -45.18826010465620158, -16.10354642779179812 ) ) ;
#24308 = DIRECTION ( 'NONE',  ( 0.000000000000000000, 0.000000000000000000, 1.000000000000000000 ) ) ;
#24309 = ORIENTED_EDGE ( 'NONE', *, *, #10875, .F. ) ;
#24310 = CARTESIAN_POINT ( 'NONE',  ( 19.34621603495309827, -8.456020361482000425, -44.92174179178260118 ) ) ;
#24311 = ORIENTED_EDGE ( 'NONE', *, *, #620, .F. ) ;
#24312 = CARTESIAN_POINT ( 'NONE',  ( 11.27698470052689927, -65.16424334175378874, -17.25002958030430023 ) ) ;
#24313 = CARTESIAN_POINT ( 'NONE',  ( 12.60445274137229887, 34.24115893967649527, -47.46978735726350607 ) ) ;
#24314 = DIRECTION ( 'NONE',  ( 0.6911981449639439390, -0.7226652920947588266, 0.000000000000000000 ) ) ;
#24315 = CARTESIAN_POINT ( 'NONE',  ( 51.63616101854069740, -50.90272864159400257, -50.31291621231439848 ) ) ;
#24316 = CARTESIAN_POINT ( 'NONE',  ( 10.85712480788070167, -64.59421087333633693, -23.35787417042663705 ) ) ;
#24317 = CARTESIAN_POINT ( 'NONE',  ( 17.16957795298714018, -23.52717565502518937, -63.96600271670024540 ) ) ;
#24318 = ORIENTED_EDGE ( 'NONE', *, *, #4953, .T. ) ;
#24319 = CARTESIAN_POINT ( 'NONE',  ( 52.27483174160517621, -50.84964383646082808, -50.96525577083021830 ) ) ;
#24320 = CARTESIAN_POINT ( 'NONE',  ( 11.13393739769619906, -63.30396901272830945, -43.91553734765660266 ) ) ;
#24321 = EDGE_CURVE ( 'NONE', #26727, #10857, #33769, .T. ) ;
#24322 = DIRECTION ( 'NONE',  ( 1.000000000000000000, 0.000000000000000000, 0.000000000000000000 ) ) ;
#24323 = EDGE_LOOP ( 'NONE', ( #36450, #27984, #7627, #44855, #45054 ) ) ;
#24324 = CARTESIAN_POINT ( 'NONE',  ( 72.72056432233058842, 1.396834109478129804, -68.84999999999999432 ) ) ;
#24325 = CARTESIAN_POINT ( 'NONE',  ( 50.30621290460380379, -48.75259804172680589, -76.16272939178270462 ) ) ;
#24326 = EDGE_CURVE ( 'NONE', #42283, #25361, #25384, .T. ) ;
#24327 = CARTESIAN_POINT ( 'NONE',  ( 24.04461900158476340, -15.61617122039998051, -49.50766513674645353 ) ) ;
#24328 = ORIENTED_EDGE ( 'NONE', *, *, #13669, .F. ) ;
#24329 = CARTESIAN_POINT ( 'NONE',  ( 18.20459087906956341, -23.32129640834502737, -62.20899636545249933 ) ) ;
#24330 = CYLINDRICAL_SURFACE ( 'NONE', #5814, 1.000000000000000444 ) ;
#24331 = CARTESIAN_POINT ( 'NONE',  ( 56.93466175439829868, -50.26424374751940150, -52.70269902980160026 ) ) ;
#24332 = CARTESIAN_POINT ( 'NONE',  ( 60.29341046574950269, 14.73091211308410031, -47.84808156045389893 ) ) ;
#24333 = CIRCLE ( 'NONE', #1762, 20.29675463313339989 ) ;
#24334 = CARTESIAN_POINT ( 'NONE',  ( 24.23497581208709661, -14.08129589808019944, -71.73272827236569071 ) ) ;
#24335 = CARTESIAN_POINT ( 'NONE',  ( 52.82750202116550042, -49.69555339446630171, -48.94276309583950280 ) ) ;
#24336 = PLANE ( 'NONE',  #8777 ) ;
#24337 = DIRECTION ( 'NONE',  ( 0.000000000000000000, -1.000000000000000000, 0.000000000000000000 ) ) ;
#24338 =( LENGTH_UNIT ( ) NAMED_UNIT ( * ) SI_UNIT ( .MILLI., .METRE. ) );
#24339 = ORIENTED_EDGE ( 'NONE', *, *, #40321, .F. ) ;
#24340 = CARTESIAN_POINT ( 'NONE',  ( 18.03756209892690165, -8.413209921940879354, -59.81490083174298888 ) ) ;
#24341 = CARTESIAN_POINT ( 'NONE',  ( 12.93740664656274397, -49.25056949571164466, -34.64999999999999858 ) ) ;
#24342 = CARTESIAN_POINT ( 'NONE',  ( 12.48566319264315716, 34.18281312454822540, -23.53955123170710095 ) ) ;
#24343 = ADVANCED_FACE ( 'NONE', ( #5729 ), #11195, .F. ) ;
#24344 = B_SPLINE_CURVE_WITH_KNOTS ( 'NONE', 3,
 ( #44037, #40359, #29077, #36162, #39851, #3958, #270, #12857, #36671, #35910, #32209, #44550, #12327, #31955, #20424, #36412 ),
 .UNSPECIFIED., .F., .F.,
 ( 4, 2, 2, 2, 2, 2, 2, 4 ),
 ( -8.604228000000000152E-15, 0.07319275283555599920, 0.1391693187718399949, 0.1804046724820189962, 0.2061767685508799908, 0.2577209606886020077, 0.3401916681089580119, 0.4123535371017689743 ),
 .UNSPECIFIED. ) ;
#24345 = CARTESIAN_POINT ( 'NONE',  ( 46.87775759358779482, 22.67357701198350028, -75.82248416561151316 ) ) ;
#24346 = ADVANCED_FACE ( 'NONE', ( #13597 ), #2814, .T. ) ;
#24347 = DIRECTION ( 'NONE',  ( 0.000000000000000000, -1.000000000000000000, 0.000000000000000000 ) ) ;
#24348 = CARTESIAN_POINT ( 'NONE',  ( -2.623662905535780077, 17.43154064245049994, -4.296538310234220504 ) ) ;
#24349 = CARTESIAN_POINT ( 'NONE',  ( 12.29766918194670033, 33.39812178576170254, -15.84900139484649984 ) ) ;
#24350 = CARTESIAN_POINT ( 'NONE',  ( 7.889763993325539460, -15.48841732168549967, -76.51260139562688778 ) ) ;
#24351 = CARTESIAN_POINT ( 'NONE',  ( 56.30960098403389935, -50.61618702972189965, -75.76111591682739288 ) ) ;
#24353 = DIRECTION ( 'NONE',  ( 0.5877852522924733591, -0.8090169943749473402, 0.000000000000000000 ) ) ;
#24352 = CARTESIAN_POINT ( 'NONE',  ( 63.25402410758490390, 0.9098571636355720083, -69.14090909090960224 ) ) ;
#24354 = CARTESIAN_POINT ( 'NONE',  ( 63.46757340380580814, 1.384887413063060180, -68.61455525072810246 ) ) ;
#24355 = CARTESIAN_POINT ( 'NONE',  ( 61.08966237208559846, 14.10374299845339863, -46.92975878837979309 ) ) ;
#24356 = CARTESIAN_POINT ( 'NONE',  ( 6.312816564080409698, -63.12436966802319205, -47.22137548220880632 ) ) ;
#24357 = ORIENTED_EDGE ( 'NONE', *, *, #33098, .T. ) ;
#24358 = CARTESIAN_POINT ( 'NONE',  ( 52.86024057890890049, -49.64494889463909999, -48.64479820451980174 ) ) ;
#24359 = AXIS2_PLACEMENT_3D ( 'NONE', #39884, #23348, #3729 ) ;
#24360 = CARTESIAN_POINT ( 'NONE',  ( 61.03683084929289748, -45.19175033160959742, -27.29275181042889997 ) ) ;
#24361 = CARTESIAN_POINT ( 'NONE',  ( 8.428794512446437182, -17.68671268992946466, -72.70900503751509802 ) ) ;
#24362 = CARTESIAN_POINT ( 'NONE',  ( 13.08122484219290094, 19.68326368368759915, -21.57315878215120009 ) ) ;
#24363 = CARTESIAN_POINT ( 'NONE',  ( 56.44602573759370046, 15.00063885377410067, -26.25485097157960013 ) ) ;
#24364 = CIRCLE ( 'NONE', #15206, 0.5000000000000004441 ) ;
#24365 = CARTESIAN_POINT ( 'NONE',  ( 20.97695636306220024, -10.75840879809530115, -32.20281262070909634 ) ) ;
#24366 = CARTESIAN_POINT ( 'NONE',  ( 50.38251483118710183, 18.64895037491550056, -76.14999999999999147 ) ) ;
#24367 = CARTESIAN_POINT ( 'NONE',  ( 52.82298539538220439, 18.43416779221530177, -48.69818189231450134 ) ) ;
#24368 = CARTESIAN_POINT ( 'NONE',  ( 71.31451227301140250, 1.097895768572089814, -70.68669971647908312 ) ) ;
#24369 = CARTESIAN_POINT ( 'NONE',  ( 40.92757250301959715, -44.41382921904099845, -3.805845460188720164 ) ) ;
#24370 = CARTESIAN_POINT ( 'NONE',  ( 45.17943004775749927, -44.39222964805399840, -5.706577274949769851 ) ) ;
#24371 = ORIENTED_EDGE ( 'NONE', *, *, #7034, .F. ) ;
#24372 = DIRECTION ( 'NONE',  ( -0.9200120562340469155, 0.3918900565005459247, -8.326672684688669123E-17 ) ) ;
#24373 = CARTESIAN_POINT ( 'NONE',  ( 47.73667124825149699, -54.43832146008400485, -54.70375119057089819 ) ) ;
#24374 = FACE_BOUND ( 'NONE', #10175, .T. ) ;
#24375 = CARTESIAN_POINT ( 'NONE',  ( 21.54529203538514182, -19.77481408501185101, -70.66115603177810556 ) ) ;
#24376 = CARTESIAN_POINT ( 'NONE',  ( 60.85130585975760198, 14.27032567669020047, -47.46989369029309813 ) ) ;
#24377 = CARTESIAN_POINT ( 'NONE',  ( 71.47772926835831697, 0.9971903505820688407, -60.67679930835159752 ) ) ;
#24378 = DIRECTION ( 'NONE',  ( 0.000000000000000000, 0.000000000000000000, 1.000000000000000000 ) ) ;
#24379 = CARTESIAN_POINT ( 'NONE',  ( 71.36792781540339092, 1.399433130755050048, -61.07453677926569924 ) ) ;
#24380 = CARTESIAN_POINT ( 'NONE',  ( 22.46008150092894695, -20.47789627965039472, -71.71596240367421160 ) ) ;
#24381 = CARTESIAN_POINT ( 'NONE',  ( 65.14992021336850314, 1.382840740411480196, -70.34664320112889868 ) ) ;
#24382 = ORIENTED_EDGE ( 'NONE', *, *, #34787, .F. ) ;
#24383 = ORIENTED_EDGE ( 'NONE', *, *, #51653, .T. ) ;
#24384 = CARTESIAN_POINT ( 'NONE',  ( 3.633937397696199056, -15.61618894467929763, -2.149999999999999911 ) ) ;
#24385 = EDGE_CURVE ( 'NONE', #26354, #38464, #2021, .T. ) ;
#24386 = DIRECTION ( 'NONE',  ( 0.000000000000000000, -1.000000000000000000, 0.000000000000000000 ) ) ;
#24387 = VERTEX_POINT ( 'NONE', #32965 ) ;
#24388 = CARTESIAN_POINT ( 'NONE',  ( 11.18784989604460023, -64.00854436587380292, -43.96560154067280024 ) ) ;
#24389 = CARTESIAN_POINT ( 'NONE',  ( 12.39116026363089951, -65.38104286502799312, -46.54587326243779444 ) ) ;
#24390 = CARTESIAN_POINT ( 'NONE',  ( 17.75030770215581200, -9.027613932962333720, -50.02938860704751534 ) ) ;
#24391 = ORIENTED_EDGE ( 'NONE', *, *, #27594, .F. ) ;
#24392 = TOROIDAL_SURFACE ( 'NONE', #30994, 47.00000000000000000, 3.000000000000000000 ) ;
#24393 = CARTESIAN_POINT ( 'NONE',  ( 55.58353086675839450, 16.15099216771209001, 11.34999999999999964 ) ) ;
#24394 = CARTESIAN_POINT ( 'NONE',  ( 42.32037652162321706, 6.442361943507792787, -78.71780434772890089 ) ) ;
#24395 = CARTESIAN_POINT ( 'NONE',  ( 60.74502025776879321, 14.51238070346370002, -47.75426036517409756 ) ) ;
#24396 = CARTESIAN_POINT ( 'NONE',  ( 12.87384136754439901, -23.18946392516980026, -42.42172377882649670 ) ) ;
#24397 = DIRECTION ( 'NONE',  ( 0.000000000000000000, -1.000000000000000000, 0.000000000000000000 ) ) ;
#24398 = CARTESIAN_POINT ( 'NONE',  ( 62.03393739769618520, -30.31618894467939995, -65.65000000000000568 ) ) ;
#24399 = EDGE_LOOP ( 'NONE', ( #38347, #27179, #6648, #31997 ) ) ;
#24400 =( BOUNDED_CURVE ( )  B_SPLINE_CURVE ( 2, ( #2204, #21842, #18181 ),
 .UNSPECIFIED., .F., .T. ) 
 B_SPLINE_CURVE_WITH_KNOTS ( ( 3, 3 ),
 ( 1.104980434577240045, 2.168627590050199672 ),
 .UNSPECIFIED. ) 
 CURVE ( )  GEOMETRIC_REPRESENTATION_ITEM ( )  RATIONAL_B_SPLINE_CURVE ( ( 1.323085463760209857, 1.425426480542939967, 1.425426480542939967 ) ) 
 REPRESENTATION_ITEM ( '' )  );
#24401 = B_SPLINE_CURVE_WITH_KNOTS ( 'NONE', 3,
 ( #8855, #16450, #28229, #4648, #15940, #32149, #8331, #24805, #20365, #31898, #48166, #20888, #12527, #12017, #32402, #28750, #44232, #44749 ),
 .UNSPECIFIED., .F., .F.,
 ( 4, 2, 2, 2, 2, 2, 2, 2, 4 ),
 ( 0.000000000000000000, 0.06250019559800874813, 0.1250003911960174963, 0.1875005867940262583, 0.2500007823920349925, 0.3125009779900437268, 0.3750011735880525165, 0.4375013691860612508, 0.5000015647840699851 ),
 .UNSPECIFIED. ) ;
#24402 = CARTESIAN_POINT ( 'NONE',  ( 12.65814259846169954, -65.49670600571860746, -22.98480981823819747 ) ) ;
#24403 = CARTESIAN_POINT ( 'NONE',  ( 12.37279372661770083, -22.04740127911919956, -38.90110303094750321 ) ) ;
#24404 = TOROIDAL_SURFACE ( 'NONE', #43702, 25.00000000000000000, 1.000000000000000000 ) ;
#24405 = CARTESIAN_POINT ( 'NONE',  ( 20.99558314274035098, -9.289997993926764508, -33.21599877232336695 ) ) ;
#24406 = EDGE_CURVE ( 'NONE', #24462, #15604, #32071, .T. ) ;
#24407 = CARTESIAN_POINT ( 'NONE',  ( 13.84625307261759986, 20.91303491124859804, -75.51792558472199346 ) ) ;
#24408 = DIRECTION ( 'NONE',  ( 2.448986521869468475E-28, 2.813979115193090436E-11, -1.000000000000000000 ) ) ;
#24409 = CARTESIAN_POINT ( 'NONE',  ( 17.71568183981793609, 20.46959823935371503, -75.56421430877649925 ) ) ;
#24410 = CARTESIAN_POINT ( 'NONE',  ( 16.13393739769620083, -15.61618894467929941, -32.14999999999999858 ) ) ;
#24411 = CARTESIAN_POINT ( 'NONE',  ( 9.152839663105250878, -20.00332868818690102, -38.32907662296240403 ) ) ;
#24412 = EDGE_LOOP ( 'NONE', ( #14245, #20997 ) ) ;
#24413 = CARTESIAN_POINT ( 'NONE',  ( 53.82042919933849845, -48.69340853470760067, -26.93473920014709933 ) ) ;
#24414 = CARTESIAN_POINT ( 'NONE',  ( 15.93086454162260068, -51.01877534386230195, -20.59235730855489876 ) ) ;
#24415 = CARTESIAN_POINT ( 'NONE',  ( 23.53669455186048864, 17.69319178430572137, -34.79644561402099612 ) ) ;
#24416 = CARTESIAN_POINT ( 'NONE',  ( 8.222787824498201559, -15.61638397318239946, -64.79233150823698395 ) ) ;
#24417 = DIRECTION ( 'NONE',  ( -0.4156269377774580720, 0.5720614028176802535, 0.7071067811865481278 ) ) ;
#24418 = CARTESIAN_POINT ( 'NONE',  ( 44.13393739769620083, -36.11618894467930119, -44.64999999999999858 ) ) ;
#24419 = ORIENTED_EDGE ( 'NONE', *, *, #5633, .T. ) ;
#24420 = CARTESIAN_POINT ( 'NONE',  ( -9.066986571212598989, -44.13582524313829936, -5.880785460427049749 ) ) ;
#24421 = CARTESIAN_POINT ( 'NONE',  ( 47.32718728057039925, 23.47016710949800000, -54.75130141235280234 ) ) ;
#24422 = CARTESIAN_POINT ( 'NONE',  ( 17.55180121426148077, 18.38379139978320609, -83.19610070254232426 ) ) ;
#24423 = CARTESIAN_POINT ( 'NONE',  ( 63.17514626975080461, 1.276058558775519991, -62.60937635806730839 ) ) ;
#24424 = CARTESIAN_POINT ( 'NONE',  ( 56.55522360613520760, 14.97957722649010037, -26.26695323647559732 ) ) ;
#24425 = CARTESIAN_POINT ( 'NONE',  ( 42.99451563395630416, 11.89542822664250110, -4.474847206224069396 ) ) ;
#24426 = FACE_OUTER_BOUND ( 'NONE', #24982, .T. ) ;
#24427 = CARTESIAN_POINT ( 'NONE',  ( 12.72604533180880182, -21.52915663163615534, -65.11948762230144894 ) ) ;
#24428 = DIRECTION ( 'NONE',  ( 1.000000000000000000, 0.000000000000000000, 0.000000000000000000 ) ) ;
#24429 = CARTESIAN_POINT ( 'NONE',  ( 57.08228080684060046, -47.57523781541689800, -48.30570546696120005 ) ) ;
#24430 = CARTESIAN_POINT ( 'NONE',  ( 24.04476365437513152, -15.55955762548125243, -75.79004789881723525 ) ) ;
#24431 = CARTESIAN_POINT ( 'NONE',  ( 9.366881967297588929, -15.61636073738300112, -79.84717978380999170 ) ) ;
#24432 = CARTESIAN_POINT ( 'NONE',  ( 17.60467135870129951, -52.01451994755070274, -75.82251062550821530 ) ) ;
#24433 = DIRECTION ( 'NONE',  ( 0.000000000000000000, 0.000000000000000000, 1.000000000000000000 ) ) ;
#24434 = CARTESIAN_POINT ( 'NONE',  ( 54.44697901455320022, 13.88381105532070059, -13.49511142752179893 ) ) ;
#24435 = ORIENTED_EDGE ( 'NONE', *, *, #28201, .T. ) ;
#24436 = PLANE ( 'NONE',  #14554 ) ;
#24437 = CARTESIAN_POINT ( 'NONE',  ( 10.13821898889280071, 31.93693633726830328, -45.99533705415459650 ) ) ;
#24438 = AXIS2_PLACEMENT_3D ( 'NONE', #36997, #21770, #18112 ) ;
#24439 = CARTESIAN_POINT ( 'NONE',  ( 43.46649277351350094, 13.81022299180570023, -6.433241829987640159 ) ) ;
#24440 = CARTESIAN_POINT ( 'NONE',  ( 68.16054639260629244, -30.33163972796129926, -18.00105978623409797 ) ) ;
#24441 = ORIENTED_EDGE ( 'NONE', *, *, #43882, .F. ) ;
#24442 = CARTESIAN_POINT ( 'NONE',  ( 17.79306446254500074, 20.39333564065439930, -75.48537863783369062 ) ) ;
#24443 = ORIENTED_EDGE ( 'NONE', *, *, #39684, .F. ) ;
#24444 = ORIENTED_EDGE ( 'NONE', *, *, #27186, .F. ) ;
#24445 = ADVANCED_FACE ( 'NONE', ( #20923 ), #40477, .F. ) ;
#24446 = B_SPLINE_CURVE_WITH_KNOTS ( 'NONE', 3,
 ( #2181, #30460, #6631, #33619, #10824, #33872, #46481, #18674, #10570, #45952, #22336, #26526, #2700, #42541 ),
 .UNSPECIFIED., .F., .F.,
 ( 4, 2, 2, 2, 1, 1, 2, 4 ),
 ( 0.000000000000000000, 0.2471173528950013354, 0.3706760293425083730, 0.4324553675662667906, 0.4633450366781509122, 0.4787898712340928897, 0.4865122885120643503, 0.4942347057900358109 ),
 .UNSPECIFIED. ) ;
#24447 = ORIENTED_EDGE ( 'NONE', *, *, #452, .T. ) ;
#24448 = CYLINDRICAL_SURFACE ( 'NONE', #37763, 1.999999999999997335 ) ;
#24449 = CARTESIAN_POINT ( 'NONE',  ( 18.51896206369700337, -21.96195333999060040, -81.23899999999999011 ) ) ;
#24450 = EDGE_CURVE ( 'NONE', #41828, #43880, #17880, .T. ) ;
#24451 = CARTESIAN_POINT ( 'NONE',  ( 59.34499803081109803, -28.11618894467929763, -15.68015151901639825 ) ) ;
#24452 = EDGE_CURVE ( 'NONE', #18483, #21555, #9518, .T. ) ;
#24453 = ORIENTED_EDGE ( 'NONE', *, *, #28727, .F. ) ;
#24454 = DIRECTION ( 'NONE',  ( 1.000000000000000000, -0.000000000000000000, 1.224646799147353207E-16 ) ) ;
#24455 = EDGE_CURVE ( 'NONE', #12281, #29876, #47201, .T. ) ;
#24456 = B_SPLINE_SURFACE_WITH_KNOTS ( 'NONE', 3, 3, ( 
 ( #29667, #38071, #49104, #46208, #10293, #2167, #25472, #33606, #13205, #13461, #1390, #9268, #5335, #45420, #5592, #9525, #41476, #21546, #5842, #25729, #41737, #1648, #49620, #13713, #45676, #10812, #11073, #3204, #30706, #39364 ),
 ( #26256, #51419, #50389, #50639, #42262, #47238, #3466, #2688, #34634, #19437, #6361, #38327, #15513, #14473, #43302, #51163, #18660, #26771, #46988, #35417, #10555, #35155, #46467, #26512, #42789, #27039, #43044, #14990, #7140, #31467 ),
 ( #30956, #31211, #22321, #47491, #2417, #27293, #6884, #2944, #7393, #14735, #22580, #18398, #34377, #30446, #22834, #46728, #42528, #23341, #23092, #39111, #19176, #6616, #38597, #34898, #15256, #38855, #11329, #18915, #50898, #24626 ),
 ( #35929, #20703, #32744, #40637, #12608, #36183, #4736, #35685, #44570, #36694, #8162, #4476, #31978, #44310, #48251, #19693, #794, #16796, #12345, #28311, #24367, #19939, #16275, #44056, #11587, #27548, #28054, #8419, #24105, #28571 ),
 ( #40380, #46, #16023, #47998, #20445, #8671, #39617, #12098, #36433, #7656, #541, #3720, #51670, #40126, #15764, #27807, #16527, #4219, #32477, #20193, #48507, #31717, #32228, #43554, #23599, #47742, #11850, #43804, #7904, #290 ),
 ( #23851, #39875, #3974, #6039, #13394, #29607, #41156, #29093, #12875, #24884, #9460, #17822, #9964, #13898, #40896, #18080, #5269, #25669, #9199, #21220, #37484, #13144, #5777, #44836, #25409, #33796, #25151, #48771, #21996, #20966 ),
 ( #49805, #21485, #41939, #36967, #29856, #25924, #45358, #41671, #17317, #45610, #33542, #5006, #38006, #2104, #49560, #13647, #9709, #37232, #1585, #29352, #28831, #8941, #41412, #21739, #5530, #45877, #33281, #1329, #33013, #1064 ),
 ( #37746, #17060, #49036, #49297, #1844, #45092, #17573, #10232, #22257, #34574, #38264, #50325, #30892, #38527, #14927, #42464, #23027, #2357, #2883, #46919, #11005, #35090, #26973, #18333, #34312, #22518, #42724, #26703, #27225, #42982 ),
 ( #50579, #7077, #26448, #14411, #50058, #26190, #46663, #3143, #47175, #51091, #42201, #3404, #6551, #39049, #11264, #19111, #2626, #15189, #31150, #43239, #7330, #30639, #6818, #30379, #6299, #23277, #18598, #39299, #46404, #22772 ),
 ( #10492, #14669, #14154, #10746, #30122, #34048, #46141, #38791, #18851, #34834, #50835, #480, #51863, #20134, #48446, #15702, #48185, #19879, #4418, #27993, #47938, #24306, #24045, #31658, #11785, #32169, #32423, #36125, #16468, #51353 ),
 ( #20384, #12289, #3658, #19630, #7844, #43996, #12039, #12548, #16212, #24563, #36373, #19371, #28514, #23792, #229, #8102, #39808, #47682, #40066, #8356, #4159, #35353, #28250, #44511, #44248, #3916, #40323, #8615, #35620, #40576 ) ),
 .UNSPECIFIED., .F., .F., .F.,
 ( 4, 1, 1, 1, 1, 1, 1, 1, 4 ),
 ( 4, 2, 2, 2, 2, 2, 2, 2, 2, 2, 2, 2, 2, 2, 4 ),
 ( 0.000000000000000000, 0.1250000000000000000, 0.2500000000000000000, 0.3750000000000000000, 0.5000000000000000000, 0.6250000000000000000, 0.7500000000000000000, 0.8750000000000000000, 1.000000000000000000 ),
 ( -1.979714999999999961E-13, 0.09067117207851999039, 0.2140248969013430203, 0.2911209749156069559, 0.3773790415573270440, 0.4312903332084020436, 0.4852016248594769876, 0.5283306581803369761, 0.5714596915011970202, 0.6404661448145729796, 0.6753595992144020288, 0.7102530536142309670, 0.7544417240960439308, 0.8251435968669439402, 0.8625806664170020399 ),
 .UNSPECIFIED. ) ;
#24457 = CARTESIAN_POINT ( 'NONE',  ( 22.48949605721776379, -18.55301542404961523, -34.98530465220235897 ) ) ;
#24458 = VERTEX_POINT ( 'NONE', #20660 ) ;
#24459 = CARTESIAN_POINT ( 'NONE',  ( 11.66595244850846314, -64.88074487536820811, -23.89163317478661241 ) ) ;
#24460 = LINE ( 'NONE', #4834, #24283 ) ;
#24461 = EDGE_LOOP ( 'NONE', ( #15343, #6706, #40254, #49065 ) ) ;
#24462 = VERTEX_POINT ( 'NONE', #41889 ) ;
#24463 = DIRECTION ( 'NONE',  ( 1.000000000000000000, 0.000000000000000000, 0.000000000000000000 ) ) ;
#24464 = CARTESIAN_POINT ( 'NONE',  ( 11.09249001376588240, -65.15264562256584213, -17.64371731244277441 ) ) ;
#24465 = CARTESIAN_POINT ( 'NONE',  ( 60.91971420063490683, 14.46337360283989959, -47.74179738751160329 ) ) ;
#24466 = CARTESIAN_POINT ( 'NONE',  ( 46.21098136784690524, 13.96635512142479918, -8.540225283467140827 ) ) ;
#24467 = EDGE_CURVE ( 'NONE', #37382, #26336, #39630, .T. ) ;
#24468 = CARTESIAN_POINT ( 'NONE',  ( 20.99563241385233070, -21.94234062699898402, -68.08399647260520737 ) ) ;
#24469 = CARTESIAN_POINT ( 'NONE',  ( -10.89697165533940115, 11.09930551684650091, -6.204277548033930501 ) ) ;
#24470 = CIRCLE ( 'NONE', #5298, 1.999999999999998668 ) ;
#24471 = CARTESIAN_POINT ( 'NONE',  ( 22.87714163486811358, -16.92332580520769625, -62.90867644139516557 ) ) ;
#24472 = CARTESIAN_POINT ( 'NONE',  ( 57.58395499372409887, 14.48151100416250081, -26.27729977557869745 ) ) ;
#24473 = CARTESIAN_POINT ( 'NONE',  ( 16.92883245282440186, -23.42355021687080097, -57.75520862408900058 ) ) ;
#24474 = EDGE_LOOP ( 'NONE', ( #7992, #50599 ) ) ;
#24475 = CARTESIAN_POINT ( 'NONE',  ( 59.98335056725809977, 14.70517998043040109, -47.53560967005149962 ) ) ;
#24476 = LINE ( 'NONE', #24214, #22728 ) ;
#24477 = CARTESIAN_POINT ( 'NONE',  ( 52.56521937542130019, 18.62941943741099848, -48.47378147059570352 ) ) ;
#24478 = CARTESIAN_POINT ( 'NONE',  ( 72.23325239345169280, 1.348268854479550027, -69.88207728865640433 ) ) ;
#24479 = CARTESIAN_POINT ( 'NONE',  ( 42.34736991110049331, -39.80156373499493583, -74.65291150510742568 ) ) ;
#24481 = EDGE_CURVE ( 'NONE', #45923, #28860, #13101, .T. ) ;
#24480 = CARTESIAN_POINT ( 'NONE',  ( 12.14982920353035567, -22.52872525748182042, -36.45899726116088146 ) ) ;
#24482 = CARTESIAN_POINT ( 'NONE',  ( 46.37015983751390280, 21.71648543033839829, -76.14999999999999147 ) ) ;
#24483 = CARTESIAN_POINT ( 'NONE',  ( 49.60483365582589954, -53.69855377821179587, -55.15230005116299594 ) ) ;
#24484 = CARTESIAN_POINT ( 'NONE',  ( -10.41557261171689852, 11.58869671994870032, -6.169019698314530231 ) ) ;
#24485 = AXIS2_PLACEMENT_3D ( 'NONE', #9827, #33394, #6154 ) ;
#24486 = DIRECTION ( 'NONE',  ( -0.8090169943749478954, -0.5877852522924724710, 0.000000000000000000 ) ) ;
#24487 = CARTESIAN_POINT ( 'NONE',  ( 18.13393739769630031, 1.391621760993470014, -35.14999999999999858 ) ) ;
#24488 = CARTESIAN_POINT ( 'NONE',  ( 55.82175251386000525, 13.88381105532070059, -14.52096918537739967 ) ) ;
#24489 = ORIENTED_EDGE ( 'NONE', *, *, #6927, .F. ) ;
#24490 = CARTESIAN_POINT ( 'NONE',  ( 18.32870867059520137, -8.496520876714420467, -48.66252544231259236 ) ) ;
#24491 = CARTESIAN_POINT ( 'NONE',  ( 64.93393739769578588, 1.396834109478129804, -61.06337307536569625 ) ) ;
#24492 = CARTESIAN_POINT ( 'NONE',  ( 12.65447590535301892, -9.481377877827592116, -34.18295494821030900 ) ) ;
#24493 = CARTESIAN_POINT ( 'NONE',  ( 60.86554014449199457, -45.45472802933989698, -47.11666279147539882 ) ) ;
#24494 = CARTESIAN_POINT ( 'NONE',  ( 11.55666225148396720, -9.119571253868539173, -81.09705367392385256 ) ) ;
#24495 = CARTESIAN_POINT ( 'NONE',  ( 58.84616880385656401, -43.44694404977806812, -8.775629712027942730 ) ) ;
#24497 = CARTESIAN_POINT ( 'NONE',  ( 8.223571189834400386, -15.61612039429540033, -78.79233150823698395 ) ) ;
#24496 = CARTESIAN_POINT ( 'NONE',  ( 41.08545287463531537, 8.428089156136307381, -80.74272105195825588 ) ) ;
#24498 = CARTESIAN_POINT ( 'NONE',  ( 68.13393739769630031, 16.88381105532069881, -71.50000000000000000 ) ) ;
#24499 = DIRECTION ( 'NONE',  ( 1.000000000000000000, 0.000000000000000000, 0.000000000000000000 ) ) ;
#24500 = ORIENTED_EDGE ( 'NONE', *, *, #12374, .T. ) ;
#24501 = CARTESIAN_POINT ( 'NONE',  ( 84.44784216359251161, -43.11618894467930119, -47.47585302082339354 ) ) ;
#24502 = ORIENTED_EDGE ( 'NONE', *, *, #33917, .T. ) ;
#24503 = VERTEX_POINT ( 'NONE', #29051 ) ;
#24504 = CARTESIAN_POINT ( 'NONE',  ( 61.40055391219659953, -45.31037351547990255, -47.20955474051870482 ) ) ;
#24505 = CARTESIAN_POINT ( 'NONE',  ( 53.82998062364706726, -50.59960046679898937, -77.06221267959426768 ) ) ;
#24506 = CIRCLE ( 'NONE', #38771, 38.99999999999998579 ) ;
#24507 = CARTESIAN_POINT ( 'NONE',  ( 76.40158688816870836, -19.74821089629645243, -12.80337776394537030 ) ) ;
#24508 = CARTESIAN_POINT ( 'NONE',  ( 51.29528453023580425, -52.95704580151759444, -54.37422039053849687 ) ) ;
#24509 = EDGE_CURVE ( 'NONE', #16879, #38586, #47069, .T. ) ;
#24510 = AXIS2_PLACEMENT_3D ( 'NONE', #16746, #48994, #9912 ) ;
#24511 = EDGE_LOOP ( 'NONE', ( #21890, #30905, #33428, #35787, #15586 ) ) ;
#24512 = VERTEX_POINT ( 'NONE', #2838 ) ;
#24513 = EDGE_CURVE ( 'NONE', #46034, #43570, #50791, .T. ) ;
#24514 = CARTESIAN_POINT ( 'NONE',  ( 8.222911052588615988, -16.65154387527992341, -56.46599083452874623 ) ) ;
#24515 = CARTESIAN_POINT ( 'NONE',  ( -15.39330862682666101, 7.341020780706740467, -48.46231058698690219 ) ) ;
#24516 = CARTESIAN_POINT ( 'NONE',  ( 14.42149519498352106, 18.38378315315731371, -83.17357193473726795 ) ) ;
#24517 = CARTESIAN_POINT ( 'NONE',  ( 22.90106509282977854, -15.61618896609811458, -36.45282238757207693 ) ) ;
#24518 = CARTESIAN_POINT ( 'NONE',  ( -21.36606260230379917, 30.88381105532059934, 11.84999999999999964 ) ) ;
#24519 = LINE ( 'NONE', #36593, #25074 ) ;
#24520 = ORIENTED_EDGE ( 'NONE', *, *, #23461, .T. ) ;
#24521 = DIRECTION ( 'NONE',  ( 0.000000000000000000, 0.000000000000000000, -1.000000000000000000 ) ) ;
#24522 = CARTESIAN_POINT ( 'NONE',  ( 52.38386414254079426, -49.88582441666579825, -77.22931079715800706 ) ) ;
#24523 = CARTESIAN_POINT ( 'NONE',  ( 22.90065656494205726, -15.61616387038935017, -34.45281736178981902 ) ) ;
#24524 = CARTESIAN_POINT ( 'NONE',  ( 8.428873804167068329, -17.68700099338225940, -54.42433541308667344 ) ) ;
#24525 = ADVANCED_FACE ( 'NONE', ( #15144 ), #3098, .T. ) ;
#24526 = CARTESIAN_POINT ( 'NONE',  ( 12.52169745332239970, -22.58314453344630124, -64.66474951716369901 ) ) ;
#24527 = CARTESIAN_POINT ( 'NONE',  ( -0.4410626023037880206, -3.737207156102679839, -35.14999999999999858 ) ) ;
#24528 = CIRCLE ( 'NONE', #1968, 6.999999999999999112 ) ;
#24529 = FACE_OUTER_BOUND ( 'NONE', #50381, .T. ) ;
#24530 = EDGE_CURVE ( 'NONE', #5619, #49749, #11415, .T. ) ;
#24531 = CARTESIAN_POINT ( 'NONE',  ( 41.60772359302610113, -44.62161519139999655, -5.233302501927670214 ) ) ;
#24532 = CARTESIAN_POINT ( 'NONE',  ( 18.03855228839456970, -51.11618894468890062, -15.68043506693139832 ) ) ;
#24533 = CARTESIAN_POINT ( 'NONE',  ( 11.63393739769619906, -41.61618894467930119, -35.14999999999999858 ) ) ;
#24534 = CARTESIAN_POINT ( 'NONE',  ( 63.86970618309410952, 1.277726045464569804, -69.78446896035558211 ) ) ;
#24535 = CARTESIAN_POINT ( 'NONE',  ( 17.16957476740626021, -7.705201780575073656, -41.33399786311579760 ) ) ;
#24536 = ORIENTED_EDGE ( 'NONE', *, *, #20255, .T. ) ;
#24537 = CARTESIAN_POINT ( 'NONE',  ( 14.24806556045970041, -51.98087455372210286, -75.71853508996549920 ) ) ;
#24538 = CARTESIAN_POINT ( 'NONE',  ( 47.35028767480929446, -54.68244725382609772, -54.65313065648980029 ) ) ;
#24539 = B_SPLINE_CURVE_WITH_KNOTS ( 'NONE', 3,
 ( #15721, #24065, #5, #18873, #3936, #7349, #19649, #7610 ),
 .UNSPECIFIED., .F., .F.,
 ( 4, 2, 2, 4 ),
 ( 0.05031563485841133304, 0.06814349192364040075, 0.08666255477330790657, 0.09307761161196949351 ),
 .UNSPECIFIED. ) ;
#24540 = CARTESIAN_POINT ( 'NONE',  ( 24.04493738470190323, -14.58064157137056860, -37.46600467335122175 ) ) ;
#24541 = AXIS2_PLACEMENT_3D ( 'NONE', #2289, #42389, #2031 ) ;
#24542 = CYLINDRICAL_SURFACE ( 'NONE', #24607, 7.910999999999997812 ) ;
#24543 = AXIS2_PLACEMENT_3D ( 'NONE', #45565, #29560, #21436 ) ;
#24544 = CARTESIAN_POINT ( 'NONE',  ( 61.00027414223083611, -45.45014343267921930, -47.32927810435275262 ) ) ;
#24545 = EDGE_CURVE ( 'NONE', #7985, #2432, #46612, .T. ) ;
#24546 = DIRECTION ( 'NONE',  ( 0.000000000000000000, 0.000000000000000000, 1.000000000000000000 ) ) ;
#24548 = ADVANCED_FACE ( 'NONE', ( #22206 ), #46875, .T. ) ;
#24547 = CARTESIAN_POINT ( 'NONE',  ( 11.73422653530680115, 34.19011593798479964, -18.16216258077279733 ) ) ;
#24550 = CARTESIAN_POINT ( 'NONE',  ( 14.06328036766014122, -23.32129468089506830, -52.37566376501965237 ) ) ;
#24549 = CARTESIAN_POINT ( 'NONE',  ( 0.4371248283888460318, -8.845792823550640449, -35.02873218748179340 ) ) ;
#24551 = CARTESIAN_POINT ( 'NONE',  ( -11.32734370190460105, -41.88171845330919751, -6.430192534648670133 ) ) ;
#24552 = CARTESIAN_POINT ( 'NONE',  ( 43.09344256680816443, 12.72802089079580412, -5.051331040473342249 ) ) ;
#24553 = CARTESIAN_POINT ( 'NONE',  ( 48.40697635570069934, 22.96883648311629855, -55.14150811720919876 ) ) ;
#24554 = ORIENTED_EDGE ( 'NONE', *, *, #7759, .F. ) ;
#24555 = CARTESIAN_POINT ( 'NONE',  ( 23.18087123250600357, -15.90477637036519987, -62.86020799324039388 ) ) ;
#24556 = ORIENTED_EDGE ( 'NONE', *, *, #43902, .F. ) ;
#24557 = CARTESIAN_POINT ( 'NONE',  ( 18.74892447570123366, -51.88237913653802735, -74.91995119709325479 ) ) ;
#24558 = CARTESIAN_POINT ( 'NONE',  ( 53.41693480158270546, -49.35328119387190071, -48.75416851881869462 ) ) ;
#24559 = DIRECTION ( 'NONE',  ( 0.000000000000000000, 0.000000000000000000, 1.000000000000000000 ) ) ;
#24561 = CARTESIAN_POINT ( 'NONE',  ( 53.01071900028409800, 18.17451771224559920, -27.28273396498699910 ) ) ;
#24560 = CARTESIAN_POINT ( 'NONE',  ( 83.27189663703491362, 13.64797996652180068, -46.76788818508799750 ) ) ;
#24562 = CARTESIAN_POINT ( 'NONE',  ( 10.81957041042960022, -20.25300490191509795, -69.22445973777388417 ) ) ;
#24563 = CARTESIAN_POINT ( 'NONE',  ( 53.05489977530229595, 18.36750851102400262, -49.10811586475909962 ) ) ;
#24564 = CARTESIAN_POINT ( 'NONE',  ( 56.73667420261889305, -45.26434326652640294, -17.93020191283299880 ) ) ;
#24565 = CARTESIAN_POINT ( 'NONE',  ( 20.11812065015670825, -22.52868107655917029, -80.12566639359206988 ) ) ;
#24566 = TOROIDAL_SURFACE ( 'NONE', #12910, 34.47562460986249988, 0.5000000000000000000 ) ;
#24567 = VERTEX_POINT ( 'NONE', #38744 ) ;
#24568 = ORIENTED_EDGE ( 'NONE', *, *, #7249, .F. ) ;
#24569 = CARTESIAN_POINT ( 'NONE',  ( 11.98171981665329966, -65.04908998879550097, -16.46086821535179823 ) ) ;
#24570 = CARTESIAN_POINT ( 'NONE',  ( 12.03939575523859951, 34.11084159468560273, -47.24132823177560425 ) ) ;
#24571 = LINE ( 'NONE', #20918, #19833 ) ;
#24572 = ADVANCED_FACE ( 'NONE', ( #38216 ), #22023, .T. ) ;
#24573 = CARTESIAN_POINT ( 'NONE',  ( 52.60056159696439693, -50.12372689670589665, -49.79359568308569806 ) ) ;
#24574 = CARTESIAN_POINT ( 'NONE',  ( 15.09849988506595686, -23.52720223303058944, -64.04933591286372518 ) ) ;
#24575 = VERTEX_POINT ( 'NONE', #5987 ) ;
#24576 = ADVANCED_FACE ( 'NONE', ( #14879 ), #50159, .F. ) ;
#24577 = FACE_OUTER_BOUND ( 'NONE', #35611, .T. ) ;
#24578 = CARTESIAN_POINT ( 'NONE',  ( 11.13393739769619906, -63.31057960318910460, -43.74730822310910128 ) ) ;
#24579 = AXIS2_PLACEMENT_3D ( 'NONE', #30649, #2636, #15464 ) ;
#24580 = CARTESIAN_POINT ( 'NONE',  ( 23.83903480973297562, -17.68687855746657789, -59.59100454946410252 ) ) ;
#24581 = CARTESIAN_POINT ( 'NONE',  ( 47.55940100909866430, 23.33745173926940453, -55.06178025467780657 ) ) ;
#24582 = CARTESIAN_POINT ( 'NONE',  ( 50.93004497053770052, -50.92639964791920448, -76.14999999999999147 ) ) ;
#24583 = CARTESIAN_POINT ( 'NONE',  ( 14.06324741486789875, -23.32128614899894714, -44.09103022834820962 ) ) ;
#24584 = VECTOR ( 'NONE', #407, 1000.000000000000000 ) ;
#24585 = VERTEX_POINT ( 'NONE', #42931 ) ;
#24586 = CARTESIAN_POINT ( 'NONE',  ( -28.43713041416927823, -60.18725675654476959, 11.84999999999999964 ) ) ;
#24587 = CARTESIAN_POINT ( 'NONE',  ( 10.07635536168570489, 22.78899166960868072, -34.82441657595547468 ) ) ;
#24588 = CARTESIAN_POINT ( 'NONE',  ( 56.73072851771979686, -50.34974087631989903, -52.75329813171639870 ) ) ;
#24589 = CARTESIAN_POINT ( 'NONE',  ( 54.24589373054839569, 17.44605741449650083, -48.34735630146840180 ) ) ;
#24590 = CARTESIAN_POINT ( 'NONE',  ( 23.98623646584669800, -13.10140875542660055, -75.69367482554660853 ) ) ;
#24591 = CARTESIAN_POINT ( 'NONE',  ( 13.68997055383310091, -51.35827251140110405, -23.13969639952529889 ) ) ;
#24592 = CARTESIAN_POINT ( 'NONE',  ( 53.64448049682719954, 20.03493786279390321, -75.63065916943469347 ) ) ;
#24593 = DIRECTION ( 'NONE',  ( 1.000000000000000000, 0.000000000000000000, 0.000000000000000000 ) ) ;
#24594 = CARTESIAN_POINT ( 'NONE',  ( 47.16864635708999742, -54.20974419499959396, -75.46775895608709561 ) ) ;
#24595 = EDGE_LOOP ( 'NONE', ( #9219, #14947 ) ) ;
#24596 = CARTESIAN_POINT ( 'NONE',  ( 46.63393739769619373, -15.61618894467929941, -35.14999999999999858 ) ) ;
#24597 = CARTESIAN_POINT ( 'NONE',  ( 10.52009571295500123, -20.51429830889400208, -69.00429683512291490 ) ) ;
#24598 = CARTESIAN_POINT ( 'NONE',  ( 53.42000044619080512, -49.46448084836430326, -49.21358545526090467 ) ) ;
#24599 = DIRECTION ( 'NONE',  ( 1.000000000000000000, 0.000000000000000000, 0.000000000000000000 ) ) ;
#24600 = CARTESIAN_POINT ( 'NONE',  ( 12.54176915115859181, 34.20132235598342874, -23.51595098417593022 ) ) ;
#24601 = CIRCLE ( 'NONE', #7062, 10.49999999999999822 ) ;
#24602 = CARTESIAN_POINT ( 'NONE',  ( 47.24349440877020356, 23.09672500570559706, -75.29141078596350667 ) ) ;
#24603 = CARTESIAN_POINT ( 'NONE',  ( 19.74336188031776373, -54.29616745937406108, -17.45721575027601347 ) ) ;
#24604 = DIRECTION ( 'NONE',  ( 1.000000000000000000, 0.000000000000000000, 0.000000000000000000 ) ) ;
#24605 = CARTESIAN_POINT ( 'NONE',  ( 12.30205595647769989, 33.50594860225369587, -15.96528926831930129 ) ) ;
#24606 = ADVANCED_FACE ( 'NONE', ( #42150 ), #10441, .T. ) ;
#24607 = AXIS2_PLACEMENT_3D ( 'NONE', #33197, #9113, #44494 ) ;
#24608 = CARTESIAN_POINT ( 'NONE',  ( 16.97276188636960015, -43.80059717415329601, -59.64999999999999147 ) ) ;
#24609 = EDGE_CURVE ( 'NONE', #3072, #19396, #8333, .T. ) ;
#24610 = CARTESIAN_POINT ( 'NONE',  ( 16.13393739769620083, -15.61618894467929941, -32.14999999999999858 ) ) ;
#24612 = LINE ( 'NONE', #16261, #3878 ) ;
#24611 = CARTESIAN_POINT ( 'NONE',  ( -10.74337798235499974, 10.09066047292260038, -4.376538325821149655 ) ) ;
#24613 = AXIS2_PLACEMENT_3D ( 'NONE', #18344, #31928, #16225 ) ;
#24614 = CARTESIAN_POINT ( 'NONE',  ( 63.20402522475220053, 1.187237555532410171, -68.90390165256179955 ) ) ;
#24615 = CARTESIAN_POINT ( 'NONE',  ( 61.45021783597690046, 13.92999906544429933, -46.45636237004219993 ) ) ;
#24616 = DIRECTION ( 'NONE',  ( 0.2267461507312891755, 0.9739538916850959405, 3.885780586188060513E-13 ) ) ;
#24617 = CARTESIAN_POINT ( 'NONE',  ( -12.40573950840640016, -56.00019996439819892, -51.46982831076100240 ) ) ;
#24618 = EDGE_CURVE ( 'NONE', #11278, #36315, #45192, .T. ) ;
#24619 = ORIENTED_EDGE ( 'NONE', *, *, #157, .T. ) ;
#24620 = CARTESIAN_POINT ( 'NONE',  ( 52.97622290741030326, -49.58418250313399511, -48.78091471321639716 ) ) ;
#24621 = LINE ( 'NONE', #24879, #22839 ) ;
#24622 = CARTESIAN_POINT ( 'NONE',  ( 8.222920464335484070, -16.32242060214289836, -66.76390504089123112 ) ) ;
#24623 = CARTESIAN_POINT ( 'NONE',  ( 56.83722719842539561, 14.19618794446390098, -25.88848200734760141 ) ) ;
#24624 = CARTESIAN_POINT ( 'NONE',  ( 18.28036160049749981, -8.897899018898199230, -34.05125434552689967 ) ) ;
#24625 = CARTESIAN_POINT ( 'NONE',  ( 50.48048356710739881, 18.85947689767530377, -76.14999999999999147 ) ) ;
#24626 = CARTESIAN_POINT ( 'NONE',  ( 52.79307622657449883, 18.44841517198999625, -48.47378032971769812 ) ) ;
#24627 = FACE_OUTER_BOUND ( 'NONE', #8058, .T. ) ;
#24628 = DIRECTION ( 'NONE',  ( 4.486507500526829843E-12, 3.054623595244970244E-12, -1.000000000000000000 ) ) ;
#24629 = CARTESIAN_POINT ( 'NONE',  ( 68.13393739769618662, -30.31618894467939995, -65.65000000000000568 ) ) ;
#24630 = VERTEX_POINT ( 'NONE', #48398 ) ;
#24631 = DIRECTION ( 'NONE',  ( 0.000000000000000000, 0.000000000000000000, 1.000000000000000000 ) ) ;
#24632 = CARTESIAN_POINT ( 'NONE',  ( 73.06384957064030061, 1.187237555532410171, -68.90390165256179955 ) ) ;
#24633 = CARTESIAN_POINT ( 'NONE',  ( 47.73232013880370772, -54.44372343144849680, -54.71634908794329277 ) ) ;
#24634 = FACE_OUTER_BOUND ( 'NONE', #28070, .T. ) ;
#24635 = CARTESIAN_POINT ( 'NONE',  ( 73.01236646462280078, 1.336371993404949832, -62.65916430077300703 ) ) ;
#24636 = CARTESIAN_POINT ( 'NONE',  ( 41.55663457306080488, 12.62725083537310056, -3.466044030332980252 ) ) ;
#24637 = CARTESIAN_POINT ( 'NONE',  ( 60.80486542312029741, 14.95141560336979936, -48.31465950696279776 ) ) ;
#24638 = CARTESIAN_POINT ( 'NONE',  ( 71.25801539443460797, 1.385702546077159925, -61.00218178904909649 ) ) ;
#24639 = CARTESIAN_POINT ( 'NONE',  ( 12.95491128060869990, -49.88685839599860117, -82.14319696191608955 ) ) ;
#24640 = CARTESIAN_POINT ( 'NONE',  ( 72.03766074089830340, 1.404167647216139958, -61.33120565596220075 ) ) ;
#24641 = DIRECTION ( 'NONE',  ( 0.000000000000000000, 0.7071067811865475727, 0.7071067811865475727 ) ) ;
#24642 = EDGE_CURVE ( 'NONE', #27249, #7182, #15658, .T. ) ;
#24643 = CARTESIAN_POINT ( 'NONE',  ( 64.90740703336619788, 0.9940423591679298232, -70.69940569364969463 ) ) ;
#24644 = ORIENTED_EDGE ( 'NONE', *, *, #3666, .F. ) ;
#24645 = ORIENTED_EDGE ( 'NONE', *, *, #21391, .F. ) ;
#24646 = AXIS2_PLACEMENT_3D ( 'NONE', #26345, #50733, #6977 ) ;
#24647 = CARTESIAN_POINT ( 'NONE',  ( 57.07894513400979974, 18.98008675654529753, -52.67137582195630330 ) ) ;
#24648 = CARTESIAN_POINT ( 'NONE',  ( 16.15069521921704165, -51.05177107958204630, -15.66900421577824254 ) ) ;
#24649 = ORIENTED_EDGE ( 'NONE', *, *, #45123, .T. ) ;
#24650 = FACE_OUTER_BOUND ( 'NONE', #31334, .T. ) ;
#24651 = CARTESIAN_POINT ( 'NONE',  ( 60.23130391296999875, -45.78304229081430066, -47.24246919202539630 ) ) ;
#24652 = CARTESIAN_POINT ( 'NONE',  ( 57.50723798014340105, 13.88381064843590096, -25.33268340738889890 ) ) ;
#24653 = CARTESIAN_POINT ( 'NONE',  ( 51.30756405184769875, 19.59276739940289858, -76.17053259469020077 ) ) ;
#24654 = ORIENTED_EDGE ( 'NONE', *, *, #40847, .F. ) ;
#24655 = LINE ( 'NONE', #40407, #9141 ) ;
#24656 = CARTESIAN_POINT ( 'NONE',  ( 24.03661765299927922, -21.35782223538524960, -18.08174999999999955 ) ) ;
#24657 = CARTESIAN_POINT ( 'NONE',  ( 60.41031540318880388, 14.61374793670090000, -47.73939764751050063 ) ) ;
#24658 = CARTESIAN_POINT ( 'NONE',  ( 10.71758635354190048, -21.83276850440699945, -40.52046943329969508 ) ) ;
#24659 = CARTESIAN_POINT ( 'NONE',  ( 45.15345886371729733, 2.073553906859470164, -35.03944707979399453 ) ) ;
#24660 = CIRCLE ( 'NONE', #2091, 2.745152743487029756 ) ;
#24661 = CARTESIAN_POINT ( 'NONE',  ( 42.99085965337582138, -37.77634669025830050, -75.36538833490237721 ) ) ;
#24662 = VERTEX_POINT ( 'NONE', #47383 ) ;
#24663 = CARTESIAN_POINT ( 'NONE',  ( 24.04493738597581753, -16.65172954098637348, -41.83399762327896809 ) ) ;
#24664 = CARTESIAN_POINT ( 'NONE',  ( 9.334730646583459190, -18.66208476771889835, -35.09859433989379340 ) ) ;
#24665 = CARTESIAN_POINT ( 'NONE',  ( 40.82287771318460301, 14.16359845706069898, -5.804582292309759417 ) ) ;
#24666 = CARTESIAN_POINT ( 'NONE',  ( 52.26504646883520167, 18.55116755685089913, -77.19463087837650050 ) ) ;
#24667 = CARTESIAN_POINT ( 'NONE',  ( 13.39998208310050032, -51.78678246903520233, -74.14999999999999147 ) ) ;
#24668 = CARTESIAN_POINT ( 'NONE',  ( 56.13393739769620083, -15.61618894467859953, -3.187564294433463008 ) ) ;
#24669 = CARTESIAN_POINT ( 'NONE',  ( 10.84455767947489946, -9.291223892962099384, -48.78597552336009358 ) ) ;
#24670 = ORIENTED_EDGE ( 'NONE', *, *, #27044, .F. ) ;
#24671 = CARTESIAN_POINT ( 'NONE',  ( 54.50086469845559378, -48.02103409330769779, -26.62677904963780051 ) ) ;
#24672 = AXIS2_PLACEMENT_3D ( 'NONE', #516, #12324, #24599 ) ;
#24673 = EDGE_CURVE ( 'NONE', #37859, #31098, #28717, .T. ) ;
#24674 = CARTESIAN_POINT ( 'NONE',  ( 14.56142577300950158, -51.11619481415970512, -22.31059544230570069 ) ) ;
#24675 = CARTESIAN_POINT ( 'NONE',  ( 50.14053598161640224, -36.67694914693753105, -76.15143915218567372 ) ) ;
#24676 = CARTESIAN_POINT ( 'NONE',  ( 16.13393739769620083, -15.61618894467929941, -6.721843382729280059 ) ) ;
#24677 = CARTESIAN_POINT ( 'NONE',  ( 75.46929132602400614, 12.36451391831151270, -13.44110377523724509 ) ) ;
#24678 = DIRECTION ( 'NONE',  ( 0.000000000000000000, 0.000000000000000000, -1.000000000000000000 ) ) ;
#24679 = VERTEX_POINT ( 'NONE', #23747 ) ;
#24680 = CARTESIAN_POINT ( 'NONE',  ( -3.546948566059239916, -48.75848200741000227, -5.665576563160169776 ) ) ;
#24681 = CARTESIAN_POINT ( 'NONE',  ( 47.33041554461919986, 23.46292742803399989, -54.63195680419789824 ) ) ;
#24682 = CARTESIAN_POINT ( 'NONE',  ( 16.13393739769620083, -15.61618894467929941, -35.14999999999999858 ) ) ;
#24683 = CARTESIAN_POINT ( 'NONE',  ( 63.09723768121719445, 1.097895768572089814, -62.46942512468480402 ) ) ;
#24684 = CARTESIAN_POINT ( 'NONE',  ( 16.13393739769620083, -29.47259540523039689, -47.64999999999999858 ) ) ;
#24685 = CARTESIAN_POINT ( 'NONE',  ( 11.93488809551230112, 34.20717902861789383, -17.90291664076359979 ) ) ;
#24686 = DIRECTION ( 'NONE',  ( -0.000000000000000000, 1.000000000000000000, 0.000000000000000000 ) ) ;
#24687 = CARTESIAN_POINT ( 'NONE',  ( 68.13393739769708191, 17.98087126524919555, -68.79648330188413752 ) ) ;
#24688 = DIRECTION ( 'NONE',  ( -0.6911981449639438280, -0.7226652920947587155, -3.885780586188047891E-16 ) ) ;
#24689 = CARTESIAN_POINT ( 'NONE',  ( 54.36584921719999386, -48.99915756198799954, -48.99053282728779379 ) ) ;
#24690 = FACE_OUTER_BOUND ( 'NONE', #32308, .T. ) ;
#24691 = CARTESIAN_POINT ( 'NONE',  ( 64.66786723518751501, 0.9395704634982890990, -60.75234178971950172 ) ) ;
#24692 = CARTESIAN_POINT ( 'NONE',  ( 17.63739037456999981, -52.51931604725010061, -76.04695140691811162 ) ) ;
#24693 = CARTESIAN_POINT ( 'NONE',  ( 24.04493741173050481, -14.58064981991307008, -73.46600114540449056 ) ) ;
#24694 = CARTESIAN_POINT ( 'NONE',  ( 20.79454452025889921, -20.90970388501609989, -61.11739150984060132 ) ) ;
#24695 = VERTEX_POINT ( 'NONE', #16424 ) ;
#24696 = DIRECTION ( 'NONE',  ( 0.000000000000000000, 1.000000000000000000, 0.000000000000000000 ) ) ;
#24697 = CARTESIAN_POINT ( 'NONE',  ( 9.284658136444910781, 31.95765349661940036, -46.53066704864979641 ) ) ;
#24698 = CARTESIAN_POINT ( 'NONE',  ( 41.84489819291530210, 13.62916984612999904, -5.635697468575719959 ) ) ;
#24699 = CARTESIAN_POINT ( 'NONE',  ( 68.39017786503269747, -30.34043394131120408, -18.15414633457509908 ) ) ;
#24700 = ORIENTED_EDGE ( 'NONE', *, *, #7637, .T. ) ;
#24701 = EDGE_CURVE ( 'NONE', #8526, #37113, #27944, .T. ) ;
#24702 = CARTESIAN_POINT ( 'NONE',  ( 18.39354190614909967, 20.87662390947729918, -75.53341961486960088 ) ) ;
#24703 = ORIENTED_EDGE ( 'NONE', *, *, #575, .T. ) ;
#24704 = ORIENTED_EDGE ( 'NONE', *, *, #35968, .F. ) ;
#24705 = EDGE_CURVE ( 'NONE', #11240, #35016, #30406, .T. ) ;
#24706 = ORIENTED_EDGE ( 'NONE', *, *, #49462, .F. ) ;
#24707 = CARTESIAN_POINT ( 'NONE',  ( 10.72704221230929988, -63.83388919140170259, -45.49767852026099746 ) ) ;
#24708 = LINE ( 'NONE', #11930, #31044 ) ;
#24709 = CARTESIAN_POINT ( 'NONE',  ( 20.84116112335389914, -20.77990536183390091, -81.23899999999999011 ) ) ;
#24710 =( BOUNDED_CURVE ( )  B_SPLINE_CURVE ( 2, ( #7752, #16629, #41001 ),
 .UNSPECIFIED., .F., .T. ) 
 B_SPLINE_CURVE_WITH_KNOTS ( ( 3, 3 ),
 ( 2.168627590050209886, 3.232274745523169734 ),
 .UNSPECIFIED. ) 
 CURVE ( )  GEOMETRIC_REPRESENTATION_ITEM ( )  RATIONAL_B_SPLINE_CURVE ( ( 1.425426480542949959, 1.425426480542949959, 1.323085463760220071 ) ) 
 REPRESENTATION_ITEM ( '' )  );
#24711 = CARTESIAN_POINT ( 'NONE',  ( 61.51123563376980030, 13.94229735801039993, -46.77252351816970588 ) ) ;
#24712 = ORIENTED_EDGE ( 'NONE', *, *, #24210, .T. ) ;
#24713 = CARTESIAN_POINT ( 'NONE',  ( 75.24637618196231870, 2.935769708213510576, -12.27223567965690698 ) ) ;
#24714 = VECTOR ( 'NONE', #33454, 1000.000000000000000 ) ;
#24715 = CARTESIAN_POINT ( 'NONE',  ( 11.93488785502882799, 34.20717900760969599, -17.90291655963030237 ) ) ;
#24716 = ORIENTED_EDGE ( 'NONE', *, *, #19706, .T. ) ;
#24717 = CARTESIAN_POINT ( 'NONE',  ( 48.60192464956850245, -46.16790854508710140, -11.45750858288359808 ) ) ;
#24718 = CIRCLE ( 'NONE', #35638, 31.00000000000000000 ) ;
#24719 = LINE ( 'NONE', #47135, #12078 ) ;
#24720 = B_SPLINE_CURVE_WITH_KNOTS ( 'NONE', 3,
 ( #47586, #47335, #11430, #11681 ),
 .UNSPECIFIED., .F., .F.,
 ( 4, 4 ),
 ( 3.627924839442150162, 3.679879811498320219 ),
 .UNSPECIFIED. ) ;
#24721 = DIRECTION ( 'NONE',  ( 1.000000000000000000, 0.000000000000000000, 0.000000000000000000 ) ) ;
#24722 = ORIENTED_EDGE ( 'NONE', *, *, #45697, .F. ) ;
#24723 = ORIENTED_EDGE ( 'NONE', *, *, #16820, .F. ) ;
#24724 = CARTESIAN_POINT ( 'NONE',  ( 0.1457840918200039859, -10.50670027737364620, -34.68167776469301344 ) ) ;
#24725 = CARTESIAN_POINT ( 'NONE',  ( 11.78395124411410322, -65.42271807245853665, -17.88069317963548954 ) ) ;
#24726 = CARTESIAN_POINT ( 'NONE',  ( 73.29566088972229920, 12.14852325496580043, -12.77663947542729872 ) ) ;
#24727 = CARTESIAN_POINT ( 'NONE',  ( 49.66581511508110935, 14.35062369332880117, -11.70419715158129925 ) ) ;
#24728 = CARTESIAN_POINT ( 'NONE',  ( 16.13393739769620083, -15.61618894467929941, -19.14999999999999858 ) ) ;
#24729 = CARTESIAN_POINT ( 'NONE',  ( -4.848012345730049688, 16.07167109130610072, -4.416243733086949952 ) ) ;
#24731 = AXIS2_PLACEMENT_3D ( 'NONE', #40325, #21167, #20387 ) ;
#24730 = DIRECTION ( 'NONE',  ( -1.000000000000000000, 0.000000000000000000, 0.000000000000000000 ) ) ;
#24732 = CARTESIAN_POINT ( 'NONE',  ( 59.11062488304980178, 14.31961591063559958, -26.60245654262559967 ) ) ;
#24733 = CARTESIAN_POINT ( 'NONE',  ( 17.06159277801890184, -7.823486994871330147, -62.82522021216060892 ) ) ;
#24734 = VERTEX_POINT ( 'NONE', #7283 ) ;
#24735 = AXIS2_PLACEMENT_3D ( 'NONE', #19427, #27284, #37 ) ;
#24736 = CARTESIAN_POINT ( 'NONE',  ( 60.05889968639040433, 14.78467075934760011, -47.76686567462839861 ) ) ;
#24737 = B_SPLINE_CURVE_WITH_KNOTS ( 'NONE', 3,
 ( #7328, #27223, #18849, #46660, #27483, #11261 ),
 .UNSPECIFIED., .F., .F.,
 ( 4, 2, 4 ),
 ( 0.4942347057900358109, 0.7471173528950179055, 1.000000000000000000 ),
 .UNSPECIFIED. ) ;
#24738 = EDGE_CURVE ( 'NONE', #32778, #32833, #29581, .T. ) ;
#24739 = DIRECTION ( 'NONE',  ( -0.5720614028176835841, -0.4156269377774527984, 0.7071067811865484609 ) ) ;
#24740 = CARTESIAN_POINT ( 'NONE',  ( 11.14366242735480128, 32.52627267133070177, -44.02655122816489808 ) ) ;
#24741 = CARTESIAN_POINT ( 'NONE',  ( 72.33301759304930556, 1.348264851907009731, -69.78229850496350650 ) ) ;
#24742 = B_SPLINE_CURVE_WITH_KNOTS ( 'NONE', 3,
 ( #50230, #50486, #10394, #9871, #2267, #6465, #2529, #22422 ),
 .UNSPECIFIED., .F., .F.,
 ( 4, 2, 2, 4 ),
 ( 0.000000000000000000, 0.01259071533122118475, 0.6292267250244858445, 1.000000000000000000 ),
 .UNSPECIFIED. ) ;
#24743 = CARTESIAN_POINT ( 'NONE',  ( 42.75619885378542051, -39.84230250343536284, -72.67917449632909666 ) ) ;
#24744 = CARTESIAN_POINT ( 'NONE',  ( 10.86720904402820054, -64.97138516849830125, -17.53558607436760042 ) ) ;
#24745 = AXIS2_PLACEMENT_3D ( 'NONE', #18582, #23014, #39036 ) ;
#24746 = CARTESIAN_POINT ( 'NONE',  ( 47.18323847407950211, 23.57489298307800141, -74.14999581260398998 ) ) ;
#24747 = CARTESIAN_POINT ( 'NONE',  ( 49.24139269240150441, -53.85336577086550136, -55.19402337003639758 ) ) ;
#24748 = AXIS2_PLACEMENT_3D ( 'NONE', #50382, #23085, #30948 ) ;
#24749 = CARTESIAN_POINT ( 'NONE',  ( 16.13393739769620083, -15.61618894467929941, -13.15000000000000036 ) ) ;
#24750 = CARTESIAN_POINT ( 'NONE',  ( 63.02123093760216221, 0.4193442080440759612, -17.11446765124405900 ) ) ;
#24751 = CARTESIAN_POINT ( 'NONE',  ( 14.53139780415550142, -32.25138633525569531, -34.65800258959610147 ) ) ;
#24752 = CARTESIAN_POINT ( 'NONE',  ( 56.87728296015039575, 13.88381105532070059, -15.74456185640559980 ) ) ;
#24753 = ORIENTED_EDGE ( 'NONE', *, *, #14441, .F. ) ;
#24754 = CARTESIAN_POINT ( 'NONE',  ( 17.84071041520759948, -22.86833484813690021, -45.49376819976789932 ) ) ;
#24755 = CARTESIAN_POINT ( 'NONE',  ( 64.10467614833328298, 1.346167254499869959, -61.35479024022959749 ) ) ;
#24756 = VERTEX_POINT ( 'NONE', #4624 ) ;
#24757 = DIRECTION ( 'NONE',  ( 1.000000000000000000, 0.000000000000000000, 0.000000000000000000 ) ) ;
#24758 = CARTESIAN_POINT ( 'NONE',  ( 61.34213663493839874, -45.56221510017259391, -47.63657398781079877 ) ) ;
#24759 = CARTESIAN_POINT ( 'NONE',  ( 9.080923589672684315, -11.95388292134956565, -80.94469259108042536 ) ) ;
#24760 = CARTESIAN_POINT ( 'NONE',  ( 50.04022705241149538, 17.68250914423200015, -76.14999999999999147 ) ) ;
#24762 = FACE_BOUND ( 'NONE', #45816, .T. ) ;
#24761 = CARTESIAN_POINT ( 'NONE',  ( 40.91633283741396809, 8.407571910465815535, -81.55800397143316616 ) ) ;
#24763 = CARTESIAN_POINT ( 'NONE',  ( 51.76047954393799699, -51.31561834827489577, -76.04144536748918881 ) ) ;
#24764 = CARTESIAN_POINT ( 'NONE',  ( 18.20462978460193071, -23.32128541091630325, -51.92433345086598706 ) ) ;
#24765 = ORIENTED_EDGE ( 'NONE', *, *, #18111, .T. ) ;
#24766 = CARTESIAN_POINT ( 'NONE',  ( 84.32109122769391263, -43.95295802218129921, -47.41657241682840151 ) ) ;
#24767 = VERTEX_POINT ( 'NONE', #44723 ) ;
#24768 = VERTEX_POINT ( 'NONE', #44464 ) ;
#24769 = ADVANCED_FACE ( 'NONE', ( #8570 ), #21375, .T. ) ;
#24770 = VERTEX_POINT ( 'NONE', #959 ) ;
#24771 = CARTESIAN_POINT ( 'NONE',  ( 61.56767787646829504, -45.23020975912200470, -47.05004766648129788 ) ) ;
#24772 = CARTESIAN_POINT ( 'NONE',  ( 60.83133136721959744, 14.23629320661039976, -47.01992809069390233 ) ) ;
#24773 = CARTESIAN_POINT ( 'NONE',  ( 76.39788387924198787, -12.46578609194745013, -12.78738496680618120 ) ) ;
#24774 = CARTESIAN_POINT ( 'NONE',  ( 55.74551679396239479, -51.08285690157870107, -53.82168174107410152 ) ) ;
#24775 = ORIENTED_EDGE ( 'NONE', *, *, #15208, .T. ) ;
#24776 = ORIENTED_EDGE ( 'NONE', *, *, #46584, .F. ) ;
#24777 = CARTESIAN_POINT ( 'NONE',  ( 48.19306574706310897, 22.95973674188289948, -54.68274065309989851 ) ) ;
#24778 = AXIS2_PLACEMENT_3D ( 'NONE', #21346, #34172, #17948 ) ;
#24779 = CARTESIAN_POINT ( 'NONE',  ( -10.06254952539740799, 13.27891273067756828, -43.88582999887075431 ) ) ;
#24780 = CARTESIAN_POINT ( 'NONE',  ( 14.58828788332387383, 18.38379252020285648, -83.18681078541726492 ) ) ;
#24781 = DIRECTION ( 'NONE',  ( 0.000000000000000000, 1.000000000000000000, 0.000000000000000000 ) ) ;
#24782 = CARTESIAN_POINT ( 'NONE',  ( 23.04645064152602174, -11.63203833470640447, -59.62568821185394796 ) ) ;
#24783 = DIRECTION ( 'NONE',  ( -1.224646799147353207E-16, 1.000000000000000000, 0.000000000000000000 ) ) ;
#24784 = ORIENTED_EDGE ( 'NONE', *, *, #37343, .T. ) ;
#24785 = B_SPLINE_CURVE_WITH_KNOTS ( 'NONE', 3,
 ( #41309, #21377, #49194, #13288, #44724, #8571, #40532, #40789, #691, #32905, #21123 ),
 .UNSPECIFIED., .F., .F.,
 ( 4, 1, 1, 1, 1, 1, 1, 1, 4 ),
 ( 0.000000000000000000, 0.01167379492393827607, 0.09089272598764548683, 0.1701116570511966297, 0.2493305881149038561, 0.3285495191784527091, 0.4077684502420016455, 0.4869873813057088441, 0.5000036202821666054 ),
 .UNSPECIFIED. ) ;
#24786 = CARTESIAN_POINT ( 'NONE',  ( -64.19449136036989501, -52.49048880573185016, -62.88965083512580634 ) ) ;
#24787 = CARTESIAN_POINT ( 'NONE',  ( 53.89956272158779882, -50.63255278052579911, -76.79736712525030384 ) ) ;
#24788 = DIRECTION ( 'NONE',  ( 0.000000000000000000, 0.000000000000000000, 1.000000000000000000 ) ) ;
#24789 = CARTESIAN_POINT ( 'NONE',  ( 60.27298471930929225, 14.52882665919789851, -47.23662664135199662 ) ) ;
#24790 = AXIS2_PLACEMENT_3D ( 'NONE', #22638, #13317, #6420 ) ;
#24791 = CARTESIAN_POINT ( 'NONE',  ( 23.74604872763389807, -17.52472469027490121, -66.09069027630880555 ) ) ;
#24792 = VECTOR ( 'NONE', #49083, 1000.000000000000000 ) ;
#24793 = LINE ( 'NONE', #4902, #51464 ) ;
#24794 = CARTESIAN_POINT ( 'NONE',  ( 43.31938993087129575, -43.19129029557480237, -4.740111887245549660 ) ) ;
#24795 = DIRECTION ( 'NONE',  ( -1.000000000000000000, 0.000000000000000000, 0.000000000000000000 ) ) ;
#24796 = CARTESIAN_POINT ( 'NONE',  ( 71.62484648860579739, 0.9098571636355720083, -60.77008670988870165 ) ) ;
#24797 = CARTESIAN_POINT ( 'NONE',  ( 4.133937397696209715, -22.54439217495480108, -35.14999999999999858 ) ) ;
#24798 = CARTESIAN_POINT ( 'NONE',  ( 64.00031433471698961, 1.277124716467510135, -69.91379268075820619 ) ) ;
#24799 = CARTESIAN_POINT ( 'NONE',  ( 16.13393739769620083, -15.61618894467929941, -54.64999999999999858 ) ) ;
#24800 = CARTESIAN_POINT ( 'NONE',  ( 65.14567254404629182, 0.9617428959510800901, -17.75426655703740053 ) ) ;
#24801 = ORIENTED_EDGE ( 'NONE', *, *, #48629, .F. ) ;
#24802 = CARTESIAN_POINT ( 'NONE',  ( 14.25022214270639864, -51.72416169445279621, -75.53980707817230211 ) ) ;
#24803 = ADVANCED_FACE ( 'NONE', ( #9357 ), #16956, .T. ) ;
#24804 = CARTESIAN_POINT ( 'NONE',  ( 47.39659154339189939, -54.65216982619919861, -54.68228600026159825 ) ) ;
#24805 = CARTESIAN_POINT ( 'NONE',  ( 14.36267143126516821, -9.025320511040868965, -37.86948818684339813 ) ) ;
#24806 = CARTESIAN_POINT ( 'NONE',  ( 83.63329895952738013, 13.29802447021414658, -46.55718444776781695 ) ) ;
#24807 = EDGE_CURVE ( 'NONE', #50655, #46482, #21198, .T. ) ;
#24808 = FACE_OUTER_BOUND ( 'NONE', #46146, .T. ) ;
#24809 = TOROIDAL_SURFACE ( 'NONE', #13959, 23.49999999832119713, 0.5000000000814219803 ) ;
#24810 = CARTESIAN_POINT ( 'NONE',  ( 23.25051134834439992, -17.84844637390679978, -32.14999999999999858 ) ) ;
#24811 = CARTESIAN_POINT ( 'NONE',  ( 65.13393739769620083, -42.61618894467930119, -65.65000000000000568 ) ) ;
#24812 = EDGE_CURVE ( 'NONE', #14727, #29730, #22351, .T. ) ;
#24813 = CARTESIAN_POINT ( 'NONE',  ( 11.53916947328389853, 34.14449583656730169, -17.79819407340969661 ) ) ;
#24815 = CARTESIAN_POINT ( 'NONE',  ( 13.61938558719180037, -51.42721352359901488, -22.88820061572821274 ) ) ;
#24814 = CARTESIAN_POINT ( 'NONE',  ( 0.5522155295079101966, -8.807798953772319805, -34.84133294386911928 ) ) ;
#24816 = CARTESIAN_POINT ( 'NONE',  ( 19.17404118348583353, -55.50002796966285246, -75.86242720129490635 ) ) ;
#24817 = CARTESIAN_POINT ( 'NONE',  ( 42.35079399692714475, 13.08996448747064001, -5.113119481343584738 ) ) ;
#24818 = CARTESIAN_POINT ( 'NONE',  ( 48.70700827379929621, 22.78256351753950071, -54.80992293905860180 ) ) ;
#24819 = VERTEX_POINT ( 'NONE', #16680 ) ;
#24820 = CARTESIAN_POINT ( 'NONE',  ( 17.41965231446239670, -8.681529881159590900, -68.40553316769369019 ) ) ;
#24821 = ORIENTED_EDGE ( 'NONE', *, *, #28170, .F. ) ;
#24822 = CARTESIAN_POINT ( 'NONE',  ( 47.81335647225210295, 23.16511464041720103, -54.71582838624409817 ) ) ;
#24823 = CIRCLE ( 'NONE', #36543, 2.999999999999999112 ) ;
#24824 = CARTESIAN_POINT ( 'NONE',  ( 17.70545290926953541, -14.47441609210117086, -7.393828452885189861 ) ) ;
#24825 = CARTESIAN_POINT ( 'NONE',  ( 22.90093738767722797, -16.50198128633406469, -42.49448633122971586 ) ) ;
#24827 = CARTESIAN_POINT ( 'NONE',  ( 55.29029958675930345, 15.78228302045550002, -26.18850085621529900 ) ) ;
#24826 = CARTESIAN_POINT ( 'NONE',  ( 83.46510812583990457, 13.46894839930740062, -46.64393865386079341 ) ) ;
#24828 = CARTESIAN_POINT ( 'NONE',  ( 17.58314231216230183, -22.51853375007059910, -62.88694525268430624 ) ) ;
#24829 = CARTESIAN_POINT ( 'NONE',  ( 11.97330428935281432, 33.54929834488839901, -16.08313759590791037 ) ) ;
#24830 = CARTESIAN_POINT ( 'NONE',  ( 56.75109370957429888, -45.11618894467940066, -15.55230934101470197 ) ) ;
#24831 = PLANE ( 'NONE',  #37303 ) ;
#24832 = VERTEX_POINT ( 'NONE', #44986 ) ;
#24833 = EDGE_CURVE ( 'NONE', #47610, #19315, #10360, .T. ) ;
#24834 = VERTEX_POINT ( 'NONE', #48933 ) ;
#24835 = CARTESIAN_POINT ( 'NONE',  ( 11.95767227753720086, -64.99278100762269617, -16.37738641795650096 ) ) ;
#24836 = CARTESIAN_POINT ( 'NONE',  ( 12.90536311836260097, 34.27762790739640764, -47.59859303656190122 ) ) ;
#24837 = CARTESIAN_POINT ( 'NONE',  ( 61.50409964634459925, -45.37406455498979341, -47.35437808299670337 ) ) ;
#24838 = DIRECTION ( 'NONE',  ( -1.000000000000000000, 0.000000000000000000, 0.000000000000000000 ) ) ;
#24839 = CARTESIAN_POINT ( 'NONE',  ( 16.13393739769620083, -15.61618894467929941, -23.15000000000000213 ) ) ;
#24840 = ORIENTED_EDGE ( 'NONE', *, *, #42206, .T. ) ;
#24841 = CARTESIAN_POINT ( 'NONE',  ( 52.95538414884752143, 18.32046719859912542, -27.75247099191258826 ) ) ;
#24842 = AXIS2_PLACEMENT_3D ( 'NONE', #1748, #18241, #34209 ) ;
#24843 = CARTESIAN_POINT ( 'NONE',  ( 13.00893796619580023, 34.28605843179359880, -23.32157451048000141 ) ) ;
#24844 = CARTESIAN_POINT ( 'NONE',  ( 8.222934311419814790, -16.65171382147144996, -60.46600640966879325 ) ) ;
#24845 = CARTESIAN_POINT ( 'NONE',  ( 71.80939745721281042, 1.439519383694590093, -70.03165268182070236 ) ) ;
#24846 = CARTESIAN_POINT ( 'NONE',  ( 63.51391054266390768, 1.390208944942419755, -62.54542373973200142 ) ) ;
#24847 = CARTESIAN_POINT ( 'NONE',  ( 56.61928438282120624, 14.09173444410579989, -25.29356196242219923 ) ) ;
#24848 = ORIENTED_EDGE ( 'NONE', *, *, #7702, .F. ) ;
#24849 = CARTESIAN_POINT ( 'NONE',  ( 10.72267144924497018, -11.45744918686567360, -67.66115304884627335 ) ) ;
#24850 = CARTESIAN_POINT ( 'NONE',  ( 10.09871813756530123, 22.83973475445539947, -34.88336916441300417 ) ) ;
#24851 = ORIENTED_EDGE ( 'NONE', *, *, #21261, .F. ) ;
#24852 = CARTESIAN_POINT ( 'NONE',  ( 23.13393739769620083, -28.89524513604070322, -62.14999999999999858 ) ) ;
#24853 = CARTESIAN_POINT ( 'NONE',  ( 52.23246550063239368, -46.22135848195970453, -14.08618016001920026 ) ) ;
#24854 = EDGE_CURVE ( 'NONE', #12469, #2875, #41054, .T. ) ;
#24855 = CARTESIAN_POINT ( 'NONE',  ( 14.66333043824689852, -7.907488096807699485, -33.45249067809769628 ) ) ;
#24856 = CARTESIAN_POINT ( 'NONE',  ( 13.65323237260809996, -51.39160756126780427, -23.15000001653109862 ) ) ;
#24857 = CYLINDRICAL_SURFACE ( 'NONE', #16675, 22.00000000000000355 ) ;
#24858 = CARTESIAN_POINT ( 'NONE',  ( 46.95087536525909400, -53.78713274785700094, -75.86145147363799879 ) ) ;
#24859 = EDGE_LOOP ( 'NONE', ( #34250, #24922, #45440, #46483, #15411 ) ) ;
#24860 = CARTESIAN_POINT ( 'NONE',  ( 54.86086241772310501, 14.92554945543239953, -16.02041001650959728 ) ) ;
#24861 = CARTESIAN_POINT ( 'NONE',  ( 13.99783841214989977, -22.75367974531040360, -62.82522021216060892 ) ) ;
#24862 = CARTESIAN_POINT ( 'NONE',  ( 13.20791805462510027, -21.71788541402070294, -31.48951129204709787 ) ) ;
#24863 = CARTESIAN_POINT ( 'NONE',  ( 12.85792267939620181, 34.27659983687792078, -23.38353926081359191 ) ) ;
#24864 = CARTESIAN_POINT ( 'NONE',  ( 47.49951315049990086, 23.36196595494009998, -74.36100594765079563 ) ) ;
#24865 = CARTESIAN_POINT ( 'NONE',  ( 19.88800963098302788, -54.71077588610068432, -18.05472786948379493 ) ) ;
#24866 = DIRECTION ( 'NONE',  ( 1.000000000000000000, 1.681650659181820415E-11, -1.224643064585135000E-16 ) ) ;
#24867 = EDGE_CURVE ( 'NONE', #2213, #41372, #12064, .T. ) ;
#24868 = CARTESIAN_POINT ( 'NONE',  ( 28.67375133668729958, -4.663717383496379654, -34.65024193067809222 ) ) ;
#24869 = CARTESIAN_POINT ( 'NONE',  ( 16.13393739769639623, 7.383811055320659733, 4.943674098299959851 ) ) ;
#24870 = ADVANCED_FACE ( 'NONE', ( #21969 ), #9235, .T. ) ;
#24871 = CARTESIAN_POINT ( 'NONE',  ( 60.70500520956167634, -60.18725675654477669, 16.35000000000000142 ) ) ;
#24873 = CARTESIAN_POINT ( 'NONE',  ( 43.09923138757430650, -39.96440645322047658, -70.65236649871883401 ) ) ;
#24872 = CARTESIAN_POINT ( 'NONE',  ( 16.13393739769620083, -15.61618894467929941, -34.64999999999999858 ) ) ;
#24874 = CARTESIAN_POINT ( 'NONE',  ( 63.15779899367210248, 0.9281439705311279598, -69.00235340255139249 ) ) ;
#24875 = DIRECTION ( 'NONE',  ( 0.000000000000000000, 0.000000000000000000, -1.000000000000000000 ) ) ;
#24876 = CARTESIAN_POINT ( 'NONE',  ( -33.14628496358510290, -25.37751098170330266, -57.60188784292080300 ) ) ;
#24877 = VERTEX_POINT ( 'NONE', #39268 ) ;
#24878 = CARTESIAN_POINT ( 'NONE',  ( 53.13654541734729264, -49.50093312247239652, -48.84750851792770021 ) ) ;
#24879 = CARTESIAN_POINT ( 'NONE',  ( 13.39998208309999939, 20.55440457967890211, -74.14999999999999147 ) ) ;
#24880 = CARTESIAN_POINT ( 'NONE',  ( 24.03439145476966488, -16.03333523629986956, -65.80911902704585259 ) ) ;
#24881 = CARTESIAN_POINT ( 'NONE',  ( 56.08973322185949684, 14.74539909579659991, -25.91532893058719722 ) ) ;
#24882 = CARTESIAN_POINT ( 'NONE',  ( 9.088594551554871614, -15.94130873329680043, -39.43814165785299508 ) ) ;
#24883 = CARTESIAN_POINT ( 'NONE',  ( 50.83387907959539831, 18.50773185315869895, -76.22448499212009665 ) ) ;
#24884 = CARTESIAN_POINT ( 'NONE',  ( 53.05608040805520176, 18.32399154030060018, -48.95471305401200368 ) ) ;
#24885 = CARTESIAN_POINT ( 'NONE',  ( 71.40029138921259744, 0.9945465939392450494, -70.67393287070269992 ) ) ;
#24886 = DIRECTION ( 'NONE',  ( 0.1686178020941689892, -0.6660492713794449182, -0.7265992051412129005 ) ) ;
#24887 = CARTESIAN_POINT ( 'NONE',  ( 73.35428046702240579, -45.11618894467940066, -14.85668780614170004 ) ) ;
#24888 = ORIENTED_EDGE ( 'NONE', *, *, #14542, .F. ) ;
#24889 = CARTESIAN_POINT ( 'NONE',  ( 11.98394575196030054, -21.80361681728220091, -75.75539986607049059 ) ) ;
#24890 = CARTESIAN_POINT ( 'NONE',  ( 72.90248002265630589, 1.325715844996850024, -68.88725199158319867 ) ) ;
#24891 = CARTESIAN_POINT ( 'NONE',  ( 47.48995689174640233, -54.59520503108659994, -54.73871931135540336 ) ) ;
#24892 = CARTESIAN_POINT ( 'NONE',  ( 16.13393739769620083, -15.61618894467929941, -6.928362978644219794 ) ) ;
#24893 = CARTESIAN_POINT ( 'NONE',  ( 73.17080802144350571, 1.198183261254780030, -62.58868501588759869 ) ) ;
#24894 = CARTESIAN_POINT ( 'NONE',  ( 57.11681979626609973, 18.51971639153730109, -52.00830098209539898 ) ) ;
#24895 = CARTESIAN_POINT ( 'NONE',  ( 71.44150897753121399, 1.096153228089719933, -60.69147900812899366 ) ) ;
#24896 = CARTESIAN_POINT ( 'NONE',  ( 46.89857864678853616, 7.968436783889276676, -34.72191413131643145 ) ) ;
#24897 = CARTESIAN_POINT ( 'NONE',  ( 71.50039957044630512, 1.308983041454300000, -60.91458334016920162 ) ) ;
#24898 = AXIS2_PLACEMENT_3D ( 'NONE', #17560, #25911, #9695 ) ;
#24899 = CARTESIAN_POINT ( 'NONE',  ( 14.06314050699439733, -23.32125855261902103, -72.09094108337404805 ) ) ;
#24900 = CARTESIAN_POINT ( 'NONE',  ( 65.13185782384009315, 1.385888765344500007, -70.30422512560809878 ) ) ;
#24901 = EDGE_LOOP ( 'NONE', ( #25562, #12231 ) ) ;
#24902 = ORIENTED_EDGE ( 'NONE', *, *, #30844, .T. ) ;
#24903 = CARTESIAN_POINT ( 'NONE',  ( 9.286271486682959875, -63.20121777444870048, -46.53040463691939976 ) ) ;
#24904 = LINE ( 'NONE', #32500, #40262 ) ;
#24905 = B_SPLINE_CURVE_WITH_KNOTS ( 'NONE', 3,
 ( #38399, #22133, #31471, #47244, #43306, #2497, #14291, #18477, #10105, #21876, #5911, #25797, #11334, #19441, #33925, #14033, #35424, #5662, #17703, #15518, #29734, #42336, #49686, #46014, #6435, #26065, #39369, #15261, #42072, #46280, #38140, #47495, #3470, #6174, #31217, #51423, #2240, #27298, #7398, #41805, #45750, #18216, #11592, #41546, #33671, #34181, #21609 ),
 .UNSPECIFIED., .F., .F.,
 ( 4, 2, 2, 2, 2, 2, 2, 1, 1, 1, 1, 2, 2, 2, 2, 2, 2, 2, 1, 1, 1, 2, 2, 2, 2, 2, 4 ),
 ( 0.5000060683415493701, 0.5312556890702444523, 0.5625053097989395345, 0.5937549305276346168, 0.6093797408919819913, 0.6171921460741557341, 0.6210983486652426055, 0.6230514499607860968, 0.6240280006085577869, 0.6245162759324436319, 0.6247604135943864989, 0.6248824824253578214, 0.6250045512563292549, 0.6562541719849754873, 0.6875037927136217197, 0.7187534134422679521, 0.7343782238065911239, 0.7421906289887525432, 0.7460968315798330863, 0.7480499328753733579, 0.7490264835231437157, 0.7495147588470287836, 0.7500030341709139625, 0.8125022756281854441, 0.8750015170854569257, 0.9375007585427284074, 1.000000000000000000 ),
 .UNSPECIFIED. ) ;
#24906 = ORIENTED_EDGE ( 'NONE', *, *, #1070, .T. ) ;
#24907 = CARTESIAN_POINT ( 'NONE',  ( -19.23636731124815569, 18.87413034886438368, 16.21999999999999886 ) ) ;
#24908 = CARTESIAN_POINT ( 'NONE',  ( 21.54527551665228913, -11.45754112647657053, -70.24448936511146258 ) ) ;
#24909 = DIRECTION ( 'NONE',  ( 0.000000000000000000, 0.000000000000000000, 1.000000000000000000 ) ) ;
#24910 = CARTESIAN_POINT ( 'NONE',  ( 53.07814259748259644, 19.64173092165989942, -76.24016859401959323 ) ) ;
#24911 = ORIENTED_EDGE ( 'NONE', *, *, #7030, .T. ) ;
#24912 = FACE_OUTER_BOUND ( 'NONE', #8986, .T. ) ;
#24913 = CARTESIAN_POINT ( 'NONE',  ( 42.65279859904871529, 6.493598508889044219, -77.05562690612859456 ) ) ;
#24914 = CARTESIAN_POINT ( 'NONE',  ( 60.47553822975979898, 14.59310890814650108, -47.74689862192149548 ) ) ;
#24915 = ADVANCED_FACE ( 'NONE', ( #26417 ), #22053, .T. ) ;
#24916 = CARTESIAN_POINT ( 'NONE',  ( 22.48256449764289755, -10.35523332789670192, -55.57206633538729790 ) ) ;
#24917 = EDGE_CURVE ( 'NONE', #17232, #566, #44533, .T. ) ;
#24918 = CARTESIAN_POINT ( 'NONE',  ( 55.91595717589819259, 14.67227259378030091, -25.32543214355489880 ) ) ;
#24919 = CARTESIAN_POINT ( 'NONE',  ( 42.28978442694865691, -37.66980104272789731, -78.87076310448497907 ) ) ;
#24920 = B_SPLINE_CURVE_WITH_KNOTS ( 'NONE', 3,
 ( #48482, #24863, #29331, #24600, #24342, #45332, #12325, #20680, #29073, #32205, #9171, #28285, #40357, #36669, #36410 ),
 .UNSPECIFIED., .F., .F.,
 ( 4, 2, 2, 1, 1, 1, 2, 2, 4 ),
 ( 0.000000000000000000, 0.2500000000000059952, 0.3750000000000062172, 0.4375000000000073275, 0.4687500000000076050, 0.4843750000000044964, 0.4921875000000029976, 0.5000000000000014433, 1.000000000000000000 ),
 .UNSPECIFIED. ) ;
#24921 = EDGE_CURVE ( 'NONE', #51503, #29628, #17076, .T. ) ;
#24922 = ORIENTED_EDGE ( 'NONE', *, *, #169, .T. ) ;
#24923 = FACE_OUTER_BOUND ( 'NONE', #34965, .T. ) ;
#24924 = CARTESIAN_POINT ( 'NONE',  ( 23.57696182004550067, -15.94525348384249952, -32.24671282160349506 ) ) ;
#24925 = CARTESIAN_POINT ( 'NONE',  ( 10.96238827582470066, -11.05823734394309987, -32.14999999999999858 ) ) ;
#24926 = CARTESIAN_POINT ( 'NONE',  ( 14.31317264139750023, 20.84016670874339638, -75.79682998878489286 ) ) ;
#24927 = CARTESIAN_POINT ( 'NONE',  ( 68.13393739771808555, -29.66618894502720138, -65.65000000100739896 ) ) ;
#24928 = DIRECTION ( 'NONE',  ( 0.000000000000000000, 0.000000000000000000, 1.000000000000000000 ) ) ;
#24929 = CIRCLE ( 'NONE', #19124, 5.500000000000000000 ) ;
#24930 = CARTESIAN_POINT ( 'NONE',  ( 17.49881693170749841, -23.74759869739819962, -51.95473276590490030 ) ) ;
#24931 = EDGE_CURVE ( 'NONE', #7479, #4963, #17072, .T. ) ;
#24932 = ORIENTED_EDGE ( 'NONE', *, *, #11423, .T. ) ;
#24933 = CARTESIAN_POINT ( 'NONE',  ( 54.01638715310450323, -48.57868330340730267, -26.93638457783499973 ) ) ;
#24934 = CARTESIAN_POINT ( 'NONE',  ( 16.05893884861770005, -51.08980756358450037, -20.93640534643669682 ) ) ;
#24935 = CARTESIAN_POINT ( 'NONE',  ( 45.14919548887390022, 2.061487825409429764, -35.12503119152809461 ) ) ;
#24936 = CARTESIAN_POINT ( 'NONE',  ( 9.367540081427694787, -15.04338014694595316, -51.87411835802699045 ) ) ;
#24937 = DIRECTION ( 'NONE',  ( 0.000000000000000000, 0.000000000000000000, 1.000000000000000000 ) ) ;
#24938 = ORIENTED_EDGE ( 'NONE', *, *, #38639, .T. ) ;
#24939 = CARTESIAN_POINT ( 'NONE',  ( -6.533439702237169300, -46.24119595036209773, -5.313628346711630535 ) ) ;
#24940 = CARTESIAN_POINT ( 'NONE',  ( 47.20857549670580511, 23.55481961561859805, -54.63975978072630113 ) ) ;
#24941 = CARTESIAN_POINT ( 'NONE',  ( 22.13393739769589885, 22.91950879131610108, -35.14999999999999858 ) ) ;
#24942 = CARTESIAN_POINT ( 'NONE',  ( 63.49266932922240159, 1.386446979194299933, -62.50785065198430601 ) ) ;
#24943 = DIRECTION ( 'NONE',  ( 0.3294064756441428266, 0.9441882088883046809, -2.329877999999999163E-14 ) ) ;
#24944 = CARTESIAN_POINT ( 'NONE',  ( 11.78860067047029858, 34.19036438400789280, -17.85348613431190046 ) ) ;
#24945 = DIRECTION ( 'NONE',  ( 0.000000000000000000, 1.000000000000000000, 0.000000000000000000 ) ) ;
#24946 = CARTESIAN_POINT ( 'NONE',  ( 21.54530371564770519, -19.77479805983715977, -64.66115530570463932 ) ) ;
#24947 = CARTESIAN_POINT ( 'NONE',  ( 71.40255948545589604, 1.402336724396250123, -61.08651255177160522 ) ) ;
#24948 = CARTESIAN_POINT ( 'NONE',  ( 59.53533088614899782, -46.29190482577769927, -47.84669194743329967 ) ) ;
#24949 = CARTESIAN_POINT ( 'NONE',  ( 20.92357090894525840, -20.46386084668973027, -66.70452729442683903 ) ) ;
#24950 = CARTESIAN_POINT ( 'NONE',  ( 17.40399715363529864, -52.78596775754549952, -76.12812327221449493 ) ) ;
#24951 = DIRECTION ( 'NONE',  ( 0.000000000000000000, -1.000000000000000000, 0.000000000000000000 ) ) ;
#24952 = PLANE ( 'NONE',  #28564 ) ;
#24953 = CARTESIAN_POINT ( 'NONE',  ( 24.04473007462266310, -15.61618926727986789, -75.50766188105974663 ) ) ;
#24954 = ORIENTED_EDGE ( 'NONE', *, *, #20791, .T. ) ;
#24955 = DIRECTION ( 'NONE',  ( -3.907280855591541680E-22, -1.000000000000000000, -8.281540456132319756E-12 ) ) ;
#24956 = CARTESIAN_POINT ( 'NONE',  ( 8.953364294532669021, 31.90297171738869864, -46.63441339637809335 ) ) ;
#24957 = CYLINDRICAL_SURFACE ( 'NONE', #32591, 7.910999999999997812 ) ;
#24958 = DIRECTION ( 'NONE',  ( -1.000000000000000000, 0.000000000000000000, 0.000000000000000000 ) ) ;
#24959 = ORIENTED_EDGE ( 'NONE', *, *, #30748, .F. ) ;
#24960 = CARTESIAN_POINT ( 'NONE',  ( 18.68424525891759913, 20.62786770048280260, -75.03330975078269205 ) ) ;
#24961 = EDGE_LOOP ( 'NONE', ( #19009, #2644, #35889, #49267 ) ) ;
#24962 = VERTEX_POINT ( 'NONE', #4388 ) ;
#24963 = ORIENTED_EDGE ( 'NONE', *, *, #20937, .F. ) ;
#24964 = CARTESIAN_POINT ( 'NONE',  ( 10.31171152940200031, -63.41871857732729723, -45.84829271550790253 ) ) ;
#24965 = CARTESIAN_POINT ( 'NONE',  ( 56.92366313695160329, -45.73164766762909750, -26.16831549262139944 ) ) ;
#24966 = CARTESIAN_POINT ( 'NONE',  ( 23.12137736902419860, -17.69276842965039975, -81.23899999999999011 ) ) ;
#24967 = CARTESIAN_POINT ( 'NONE',  ( 61.49572070650139466, 14.06442238722440052, -47.20084786350769690 ) ) ;
#24968 = CARTESIAN_POINT ( 'NONE',  ( 63.91114391772079273, 1.454949836291180132, -61.73964252679819964 ) ) ;
#24969 = EDGE_LOOP ( 'NONE', ( #43369, #42386, #49324, #42661 ) ) ;
#24970 = AXIS2_PLACEMENT_3D ( 'NONE', #43081, #26812, #42825 ) ;
#24971 = CARTESIAN_POINT ( 'NONE',  ( -20.36606260230379917, -15.61618894467949836, -69.65000000000000568 ) ) ;
#24972 = AXIS2_PLACEMENT_3D ( 'NONE', #33555, #46415, #6564 ) ;
#24973 = CARTESIAN_POINT ( 'NONE',  ( 12.30205592777625334, 33.50594859046132257, -15.96528925779647601 ) ) ;
#24974 = EDGE_LOOP ( 'NONE', ( #36776, #1099, #27820, #41886, #1029 ) ) ;
#24975 = CARTESIAN_POINT ( 'NONE',  ( 11.13393739525318438, -63.64729783289567422, -24.14585929178920054 ) ) ;
#24976 = EDGE_CURVE ( 'NONE', #11158, #15142, #44222, .T. ) ;
#24977 = CARTESIAN_POINT ( 'NONE',  ( 24.04493618318231185, -15.62127662466025235, -33.79253448095708023 ) ) ;
#24978 = AXIS2_PLACEMENT_3D ( 'NONE', #353, #37292, #12678 ) ;
#24979 = CARTESIAN_POINT ( 'NONE',  ( 5.633937397696199056, -15.61618894439688532, -18.58999999999999986 ) ) ;
#24980 = ADVANCED_FACE ( 'NONE', ( #48157 ), #16442, .T. ) ;
#24981 = ORIENTED_EDGE ( 'NONE', *, *, #48316, .T. ) ;
#24982 = EDGE_LOOP ( 'NONE', ( #13220, #29493, #1402, #43894 ) ) ;
#24983 = CARTESIAN_POINT ( 'NONE',  ( 47.17210187534929844, -54.78212032244810104, -74.50474471063260751 ) ) ;
#24984 = FACE_OUTER_BOUND ( 'NONE', #3195, .T. ) ;
#24985 = CARTESIAN_POINT ( 'NONE',  ( 46.42739470264289992, 14.32699058590440089, -9.432284590658529311 ) ) ;
#24986 = CARTESIAN_POINT ( 'NONE',  ( 16.13393739769620083, -15.61618894467929941, -3.187564294433600232 ) ) ;
#24987 = CARTESIAN_POINT ( 'NONE',  ( -6.123496779401830459, 15.19157518532879969, -4.783664570069790400 ) ) ;
#24988 = CARTESIAN_POINT ( 'NONE',  ( 45.42616726031420882, 2.762490711761018236, -58.70844597252361297 ) ) ;
#24989 = CARTESIAN_POINT ( 'NONE',  ( 54.86087699991983868, 14.92551754678483711, -16.02040008515932712 ) ) ;
#24990 = CARTESIAN_POINT ( 'NONE',  ( 20.51459614682930166, -22.12745434449419690, -73.59899483681280685 ) ) ;
#24991 = EDGE_CURVE ( 'NONE', #30210, #14297, #1164, .T. ) ;
#24992 = ORIENTED_EDGE ( 'NONE', *, *, #37996, .T. ) ;
#24993 = CARTESIAN_POINT ( 'NONE',  ( 11.67620015026735203, -64.89165383396532150, -23.88711004025349283 ) ) ;
#24994 = CARTESIAN_POINT ( 'NONE',  ( -8.601845089184939397, -44.24493450895539581, -5.161620436049600080 ) ) ;
#24995 = CARTESIAN_POINT ( 'NONE',  ( 11.79211174369839910, 33.77432752974699781, -45.32950553526499959 ) ) ;
#24996 = EDGE_CURVE ( 'NONE', #7027, #35178, #32933, .T. ) ;
#24997 = CARTESIAN_POINT ( 'NONE',  ( 72.70940061843029412, 1.399433130755119992, -68.88399041770809106 ) ) ;
#24998 = AXIS2_PLACEMENT_3D ( 'NONE', #50873, #14962, #30928 ) ;
#24999 = CARTESIAN_POINT ( 'NONE',  ( 11.88460916115749910, -64.82510961609500555, -16.16716782998640056 ) ) ;
#25000 = VECTOR ( 'NONE', #12024, 1000.000000000000000 ) ;
#25001 = CARTESIAN_POINT ( 'NONE',  ( 11.73319001782157933, 34.19002770849662198, -18.17421237843034731 ) ) ;
#25002 = AXIS2_PLACEMENT_3D ( 'NONE', #44332, #37253, #40402 ) ;
#25003 = CARTESIAN_POINT ( 'NONE',  ( 49.36631007174879926, -53.73686886467790202, -54.70819196421620489 ) ) ;
#25004 = CARTESIAN_POINT ( 'NONE',  ( 42.53968774367980643, -44.23115725350800176, -5.088323970340629998 ) ) ;
#25005 = CARTESIAN_POINT ( 'NONE',  ( 61.72540128749741228, -0.04346031282550247982, -16.65167021730934493 ) ) ;
#25006 = CARTESIAN_POINT ( 'NONE',  ( 14.58123197128150039, -32.20606442350140242, -34.65032322548079691 ) ) ;
#25007 = CARTESIAN_POINT ( 'NONE',  ( 12.14986774143145887, -22.52874705890221918, -54.45899922363309997 ) ) ;
#25008 = EDGE_LOOP ( 'NONE', ( #39271, #16888, #50138, #41930, #14371 ) ) ;
#25009 = CARTESIAN_POINT ( 'NONE',  ( 16.45875955084829911, -23.05938616812849773, -47.55346040742190183 ) ) ;
#25010 =( BOUNDED_CURVE ( )  B_SPLINE_CURVE ( 3, ( #15054, #34696, #18465, #14282 ),
 .UNSPECIFIED., .F., .T. ) 
 B_SPLINE_CURVE_WITH_KNOTS ( ( 4, 4 ),
 ( 3.293969860817171025, 3.377821128487717317 ),
 .UNSPECIFIED. ) 
 CURVE ( )  GEOMETRIC_REPRESENTATION_ITEM ( )  RATIONAL_B_SPLINE_CURVE ( ( 1.000000000000000000, 0.9994141662295833450, 0.9994141662295833450, 1.000000000000000000 ) ) 
 REPRESENTATION_ITEM ( '' )  );
#25011 = CARTESIAN_POINT ( 'NONE',  ( 64.11008412164950698, 1.443559558797649967, -61.49008420214889981 ) ) ;
#25012 = ORIENTED_EDGE ( 'NONE', *, *, #32872, .T. ) ;
#25013 = CARTESIAN_POINT ( 'NONE',  ( 16.13393739769620083, -15.61618894467929941, 8.349999999999999645 ) ) ;
#25014 = CARTESIAN_POINT ( 'NONE',  ( 60.71052973799270092, -45.66926968361909900, -47.62087077360929754 ) ) ;
#25015 = CARTESIAN_POINT ( 'NONE',  ( 56.84932596551109185, -50.65659107673559447, -53.85230338955700091 ) ) ;
#25016 = CARTESIAN_POINT ( 'NONE',  ( 61.62036109055981115, 14.01986140997038888, -47.09707863094710945 ) ) ;
#25018 = FACE_OUTER_BOUND ( 'NONE', #40729, .T. ) ;
#25017 = CARTESIAN_POINT ( 'NONE',  ( 45.00717534271083053, 8.798628770718870840, -61.77800503858115633 ) ) ;
#25019 = CARTESIAN_POINT ( 'NONE',  ( 19.06574088075160134, -9.201589384987739706, -60.48364006133169823 ) ) ;
#25020 = CARTESIAN_POINT ( 'NONE',  ( 16.13393739769620083, -15.61618894467929941, -22.14999999999999858 ) ) ;
#25021 = ORIENTED_EDGE ( 'NONE', *, *, #44385, .T. ) ;
#25022 = CARTESIAN_POINT ( 'NONE',  ( 84.05638291250160421, -44.46509440729400353, -47.35165316785450074 ) ) ;
#25023 = ORIENTED_EDGE ( 'NONE', *, *, #46144, .T. ) ;
#25024 = ORIENTED_EDGE ( 'NONE', *, *, #51438, .F. ) ;
#25025 = EDGE_LOOP ( 'NONE', ( #29060, #18118, #40275, #37609, #7879 ) ) ;
#25026 = FACE_OUTER_BOUND ( 'NONE', #883, .T. ) ;
#25027 = CARTESIAN_POINT ( 'NONE',  ( 52.63768092904719964, -49.80353151416749569, -48.69670982295910022 ) ) ;
#25028 = CARTESIAN_POINT ( 'NONE',  ( 55.94681035962474880, 14.65618203914781859, -25.53316267917964311 ) ) ;
#25029 = CARTESIAN_POINT ( 'NONE',  ( 76.39306992833101617, -14.04342351347505513, -12.76664126219467121 ) ) ;
#25030 = CARTESIAN_POINT ( 'NONE',  ( 23.08073416742070094, -9.873403152104399894, -35.14999999999999858 ) ) ;
#25031 = EDGE_LOOP ( 'NONE', ( #19114, #28225 ) ) ;
#25032 = ORIENTED_EDGE ( 'NONE', *, *, #1805, .F. ) ;
#25033 = CARTESIAN_POINT ( 'NONE',  ( 16.13393739769620083, -15.61618894467929941, -24.90346750000000142 ) ) ;
#25034 = CARTESIAN_POINT ( 'NONE',  ( 56.84210776121830122, 19.42547441397019981, -53.85131221055259942 ) ) ;
#25035 = CARTESIAN_POINT ( 'NONE',  ( 23.06214062797170072, -27.61618894467930119, -24.14999999999999858 ) ) ;
#25036 = FACE_OUTER_BOUND ( 'NONE', #47569, .T. ) ;
#25037 = EDGE_CURVE ( 'NONE', #14960, #44411, #10376, .T. ) ;
#25038 = CARTESIAN_POINT ( 'NONE',  ( 8.797781558458089179, -63.18317285479920997, -46.67022811708060459 ) ) ;
#25039 = CYLINDRICAL_SURFACE ( 'NONE', #5032, 7.910999999999997812 ) ;
#25040 = VECTOR ( 'NONE', #40825, 1000.000000000000000 ) ;
#25041 = ORIENTED_EDGE ( 'NONE', *, *, #13510, .F. ) ;
#25042 = DIRECTION ( 'NONE',  ( 0.3294064756441309472, 0.9441882088883087887, -3.053113317719179500E-16 ) ) ;
#25043 = CARTESIAN_POINT ( 'NONE',  ( 83.89200044194980421, -48.61618894467930119, -53.92796738110899923 ) ) ;
#25044 = CARTESIAN_POINT ( 'NONE',  ( 68.13393739769618662, -30.31618894467939995, -80.15000000000000568 ) ) ;
#25045 = VECTOR ( 'NONE', #23577, 1000.000000000000000 ) ;
#25046 = CARTESIAN_POINT ( 'NONE',  ( 60.82575030619229750, 14.23921728079439930, -47.02326931679620259 ) ) ;
#25047 = AXIS2_PLACEMENT_3D ( 'NONE', #2226, #18203, #50187 ) ;
#25048 = CARTESIAN_POINT ( 'NONE',  ( 11.24659819205199973, -9.476102375211780782, -65.29850096567270157 ) ) ;
#25049 = CARTESIAN_POINT ( 'NONE',  ( 8.711199217769639347, 17.65459752315663877, -34.82978046822305629 ) ) ;
#25050 = AXIS2_PLACEMENT_3D ( 'NONE', #44132, #15587, #35497 ) ;
#25051 = CARTESIAN_POINT ( 'NONE',  ( 42.25512407184699981, -43.69544688865530446, -4.476913605124590134 ) ) ;
#25052 = FACE_OUTER_BOUND ( 'NONE', #35470, .T. ) ;
#25053 = CARTESIAN_POINT ( 'NONE',  ( 73.01385068780759013, 0.9098571636355720083, -62.15909090909049439 ) ) ;
#25054 = CARTESIAN_POINT ( 'NONE',  ( 68.13393739824140027, -1.666188945520784337, -49.15000000187050233 ) ) ;
#25055 = CARTESIAN_POINT ( 'NONE',  ( 64.20565978367740456, 1.440336511345229997, -69.88995585498329888 ) ) ;
#25056 = DIRECTION ( 'NONE',  ( 0.000000000000000000, -1.000000000000000000, 0.000000000000000000 ) ) ;
#25057 = CARTESIAN_POINT ( 'NONE',  ( 67.08848200792850491, -0.1544538032429550178, -17.50642677597119956 ) ) ;
#25058 = ORIENTED_EDGE ( 'NONE', *, *, #22600, .F. ) ;
#25059 = CARTESIAN_POINT ( 'NONE',  ( 13.76720245349099869, -52.01740915708810320, -75.38689171750549178 ) ) ;
#25060 = CARTESIAN_POINT ( 'NONE',  ( 57.37029956467470271, 18.93460159902399909, -52.65659740218330143 ) ) ;
#25061 = EDGE_CURVE ( 'NONE', #1527, #29389, #12891, .T. ) ;
#25062 = CARTESIAN_POINT ( 'NONE',  ( 83.30738730474247689, 10.97725729733029532, -44.69194689374966600 ) ) ;
#25063 = CARTESIAN_POINT ( 'NONE',  ( -3.866062602303800499, -15.61618894467929763, -16.88999999999999702 ) ) ;
#25064 = CARTESIAN_POINT ( 'NONE',  ( 15.18614069519726151, -7.687728170468655975, -54.97012589771951951 ) ) ;
#25065 = CARTESIAN_POINT ( 'NONE',  ( 23.20356372514779864, -14.30628808687479925, -32.14999999999999858 ) ) ;
#25066 = DIRECTION ( 'NONE',  ( -1.000000000000000000, 0.000000000000000000, 0.000000000000000000 ) ) ;
#25067 = CARTESIAN_POINT ( 'NONE',  ( 47.71760965017880096, -54.49863051568969752, -55.05225816380090009 ) ) ;
#25069 = CARTESIAN_POINT ( 'NONE',  ( 8.428879373767653505, -17.68702123896981249, -74.42433509932602931 ) ) ;
#25068 = DIRECTION ( 'NONE',  ( 0.000000000000000000, 1.000000000000000000, 0.000000000000000000 ) ) ;
#25070 = AXIS2_PLACEMENT_3D ( 'NONE', #29775, #45792, #26104 ) ;
#25071 = CARTESIAN_POINT ( 'NONE',  ( 16.13393739769620083, -38.61618894467930119, -62.64999999999999858 ) ) ;
#25072 = CARTESIAN_POINT ( 'NONE',  ( 2.918607032519620947, -25.21768847662068325, 5.856814007409659517 ) ) ;
#25073 = CARTESIAN_POINT ( 'NONE',  ( 48.80215967364860319, 22.76357081333170029, -54.88693110859010460 ) ) ;
#25074 = VECTOR ( 'NONE', #44728, 1000.000000000000000 ) ;
#25075 = ORIENTED_EDGE ( 'NONE', *, *, #23512, .F. ) ;
#25076 = AXIS2_PLACEMENT_3D ( 'NONE', #3875, #27190, #18812 ) ;
#25077 = CARTESIAN_POINT ( 'NONE',  ( 9.100060599342889134, -15.09933658661340239, -65.87052737365789312 ) ) ;
#25078 = VERTEX_POINT ( 'NONE', #43458 ) ;
#25079 = TOROIDAL_SURFACE ( 'NONE', #15088, 34.99999974117479695, 4.999999999402000128 ) ;
#25080 = CARTESIAN_POINT ( 'NONE',  ( 62.63393739769619373, -53.11618894467930119, 10.84999999999999964 ) ) ;
#25081 = CARTESIAN_POINT ( 'NONE',  ( -1.057045607928901232, -15.61618894398127999, 14.34999999999999964 ) ) ;
#25082 = DIRECTION ( 'NONE',  ( -1.224646799147353207E-16, 1.000000000000000000, 0.000000000000000000 ) ) ;
#25084 = CARTESIAN_POINT ( 'NONE',  ( 56.05190775535580627, 14.68378006638939937, -25.80821134207000256 ) ) ;
#25083 = CARTESIAN_POINT ( 'NONE',  ( 83.99291904213089310, 13.14199879970889917, -47.15152633430140838 ) ) ;
#25085 = AXIS2_PLACEMENT_3D ( 'NONE', #4623, #48397, #11990 ) ;
#25086 = CARTESIAN_POINT ( 'NONE',  ( 17.53874363813559967, -8.704671157431098649, -70.01664904841010184 ) ) ;
#25087 = AXIS2_PLACEMENT_3D ( 'NONE', #29291, #4936, #28771 ) ;
#25088 = CARTESIAN_POINT ( 'NONE',  ( 82.34864690492774741, -45.64188066427791313, -47.72348187592566404 ) ) ;
#25089 = CARTESIAN_POINT ( 'NONE',  ( 72.82137280411760116, 1.383928098097870096, -68.54761322559109260 ) ) ;
#25090 = B_SPLINE_SURFACE_WITH_KNOTS ( 'NONE', 3, 3, ( 
 ( #37731, #37470, #17559, #32461, #36949, #13131, #25138, #45076, #9185, #51738 ),
 ( #27622, #15064, #18730, #46795, #27112, #42861, #19249, #3539, #23674, #47315 ),
 ( #34968, #15833, #38673, #34709, #47816, #10887, #39691, #47562, #50965, #43372 ),
 ( #39178, #12616, #23161, #23418, #22906, #51238, #44576, #11657, #38924, #3273 ),
 ( #2758, #14808, #43115, #11142, #47058, #7206, #19509, #3796, #50709, #35231 ),
 ( #30773, #51489, #26850, #6956, #15329, #3016, #18987, #35499, #15589, #31282 ),
 ( #11403, #31032, #7464, #31543, #43628, #27365, #39439, #19765, #7731, #35756 ),
 ( #31798, #28576, #22653, #13905, #25675, #8680, #45616, #49045, #9468, #33289 ),
 ( #40903, #40645, #29358, #49305, #24632, #45364, #41677, #25416, #45099, #41418 ),
 ( #13652, #5785, #9716, #5277, #1336, #28840, #16803, #1851, #13151, #17829 ),
 ( #13400, #29613, #4743, #29863, #21745, #32752, #37753, #33802, #49813, #17068 ),
 ( #41165, #20710, #36701, #25158, #5536, #803, #36974, #17579, #33549, #44843 ),
 ( #21491, #33020, #17326, #48778, #12884, #8948, #24890, #29101, #5013, #37491 ),
 ( #37238, #20975, #1591, #1071, #9206, #49566, #21228, #46668, #26982, #25932 ),
 ( #2892, #11011, #50842, #6046, #30128, #42731, #42207, #42989, #30386, #46410 ),
 ( #10498, #26712, #38271, #26196, #9970, #14933, #6305, #34581, #7085, #23035 ) ),
 .UNSPECIFIED., .F., .F., .F.,
 ( 4, 2, 2, 2, 2, 2, 2, 4 ),
 ( 4, 1, 1, 1, 1, 1, 1, 4 ),
 ( -1.183080999999999906E-15, 0.07216186899280699341, 0.1546325764131580016, 0.2061767685508779924, 0.2319488646197380155, 0.2731842183299139637, 0.3391607842661950034, 0.4123535371017569839 ),
 ( 0.000000000000000000, 0.1428571428571430157, 0.2857142857142860315, 0.4285714285714289917, 0.5714285714285709528, 0.7142857142857139685, 0.8571428571428569843, 1.000000000000000000 ),
 .UNSPECIFIED. ) ;
#25091 = CARTESIAN_POINT ( 'NONE',  ( 22.46012480422232471, -20.47783645966823585, -80.00066668459615471 ) ) ;
#25092 = ORIENTED_EDGE ( 'NONE', *, *, #48676, .F. ) ;
#25093 = ORIENTED_EDGE ( 'NONE', *, *, #51402, .F. ) ;
#25094 = CARTESIAN_POINT ( 'NONE',  ( 12.12757547495970023, -65.18777574590600921, -16.69244762554430039 ) ) ;
#25095 = CARTESIAN_POINT ( 'NONE',  ( 11.44396443873849911, 33.41480605604599674, -45.21635737664340127 ) ) ;
#25096 = DIRECTION ( 'NONE',  ( -0.5685928097855377228, 0.5944782866685497380, 0.5685928097855377228 ) ) ;
#25097 = CARTESIAN_POINT ( 'NONE',  ( 49.34600860551959300, -53.00476810193420363, -52.46789648595490263 ) ) ;
#25098 = CARTESIAN_POINT ( 'NONE',  ( 9.221499452342687420, -19.60046601118327914, -64.34100209943599680 ) ) ;
#25099 = ORIENTED_EDGE ( 'NONE', *, *, #4655, .F. ) ;
#25100 = CARTESIAN_POINT ( 'NONE',  ( 57.10963496851019272, 14.63735811038339918, -26.25116453996779953 ) ) ;
#25101 = EDGE_CURVE ( 'NONE', #26370, #49152, #16181, .T. ) ;
#25102 = CARTESIAN_POINT ( 'NONE',  ( 11.27224481477622575, -21.94234313428745153, -60.21602416443509753 ) ) ;
#25103 = CARTESIAN_POINT ( 'NONE',  ( 29.06214062797170072, -15.61618894467929941, -23.15000000000000213 ) ) ;
#25104 = CARTESIAN_POINT ( 'NONE',  ( 50.12211799414340163, -48.76092583931080071, -76.14999999999999147 ) ) ;
#25105 = B_SPLINE_CURVE_WITH_KNOTS ( 'NONE', 3,
 ( #35023, #14089, #38985, #19048, #38456, #34766, #10426, #22710, #26638, #49998, #51027 ),
 .UNSPECIFIED., .F., .F.,
 ( 4, 1, 1, 1, 1, 1, 1, 1, 4 ),
 ( 0.4999975329053952255, 0.5076261421407139984, 0.5868450732042660434, 0.6660640042678135364, 0.7452829353315238992, 0.8245018663950713922, 0.9037207974587817549, 0.9829397285223337999, 1.000000000000000000 ),
 .UNSPECIFIED. ) ;
#25106 = EDGE_CURVE ( 'NONE', #48357, #13535, #47651, .T. ) ;
#25107 = FACE_OUTER_BOUND ( 'NONE', #4098, .T. ) ;
#25108 = ORIENTED_EDGE ( 'NONE', *, *, #30689, .T. ) ;
#25109 = EDGE_CURVE ( 'NONE', #33352, #18872, #49570, .T. ) ;
#25110 = CARTESIAN_POINT ( 'NONE',  ( 11.97539229837822106, -10.20477340020057611, -67.74448618190876914 ) ) ;
#25111 = DIRECTION ( 'NONE',  ( 0.000000000000000000, -1.000000000000000000, 0.000000000000000000 ) ) ;
#25112 = EDGE_LOOP ( 'NONE', ( #9713, #35903, #12630, #13351, #46134, #15285, #1032, #14415, #20072 ) ) ;
#25113 = CARTESIAN_POINT ( 'NONE',  ( 18.20460328303584419, -7.911084987229377141, -53.37566667684684774 ) ) ;
#25114 = LINE ( 'NONE', #50023, #42927 ) ;
#25115 = EDGE_CURVE ( 'NONE', #37505, #51131, #7816, .T. ) ;
#25116 = CARTESIAN_POINT ( 'NONE',  ( 8.087912829374468870, -13.81502027023469914, -78.86243206809139394 ) ) ;
#25117 = CARTESIAN_POINT ( 'NONE',  ( 68.13393739769630031, 16.88381105531836823, -74.20000000000023022 ) ) ;
#25118 = FACE_OUTER_BOUND ( 'NONE', #14568, .T. ) ;
#25119 = CARTESIAN_POINT ( 'NONE',  ( 47.45602544390119704, -54.53030583225749695, -74.72363872023309739 ) ) ;
#25120 = ORIENTED_EDGE ( 'NONE', *, *, #18092, .T. ) ;
#25121 = VECTOR ( 'NONE', #39195, 1000.000000000000000 ) ;
#25122 = CARTESIAN_POINT ( 'NONE',  ( 55.40887998857099461, 14.39935875450660063, -16.01783516407289909 ) ) ;
#25123 = CIRCLE ( 'NONE', #8390, 10.27649999999999864 ) ;
#25124 = CARTESIAN_POINT ( 'NONE',  ( 57.24507234829509628, -50.61619228912019963, -53.91419826682510319 ) ) ;
#25126 = CARTESIAN_POINT ( 'NONE',  ( 52.60158096327749888, -49.82903481347529606, -48.60922413768609829 ) ) ;
#25125 = CIRCLE ( 'NONE', #13453, 0.5000000000000004441 ) ;
#25127 = EDGE_CURVE ( 'NONE', #12629, #50723, #8071, .T. ) ;
#25128 = CARTESIAN_POINT ( 'NONE',  ( 21.98073010695399887, -11.67187985524660121, -34.65826853459179802 ) ) ;
#25129 = AXIS2_PLACEMENT_3D ( 'NONE', #2443, #22087, #6389 ) ;
#25130 = DIRECTION ( 'NONE',  ( -1.000000000000000000, 0.000000000000000000, 0.000000000000000000 ) ) ;
#25131 = VECTOR ( 'NONE', #49132, 1000.000000000000000 ) ;
#25132 = CARTESIAN_POINT ( 'NONE',  ( 47.34254393078440160, 23.13085423282609909, -75.17206278554509424 ) ) ;
#25133 = FACE_OUTER_BOUND ( 'NONE', #30588, .T. ) ;
#25134 = EDGE_CURVE ( 'NONE', #28015, #1802, #7048, .T. ) ;
#25135 = CARTESIAN_POINT ( 'NONE',  ( 61.14444386409353882, -45.63613486214893555, -47.70810082891851067 ) ) ;
#25136 = CARTESIAN_POINT ( 'NONE',  ( 12.30638105235319912, 33.40191250400779666, -15.85198194120730086 ) ) ;
#25137 = DIRECTION ( 'NONE',  ( -0.8090169943749471182, 0.5877852522924732481, 0.000000000000000000 ) ) ;
#25138 = CARTESIAN_POINT ( 'NONE',  ( 73.02088654388471411, 1.338092079250050137, -68.62019553714330300 ) ) ;
#25140 = CARTESIAN_POINT ( 'NONE',  ( 29.35282966121437553, -35.71037171799162735, -84.62344484690784441 ) ) ;
#25139 = CARTESIAN_POINT ( 'NONE',  ( 14.13393739769630031, 1.391621760993509982, -35.14999999999999858 ) ) ;
#25141 = CARTESIAN_POINT ( 'NONE',  ( 61.26948014433400402, 14.00673465877100021, -46.56955475535669819 ) ) ;
#25142 = CARTESIAN_POINT ( 'NONE',  ( -18.43754721997909840, -52.44194012997609633, -54.46408928706210162 ) ) ;
#25143 = ORIENTED_EDGE ( 'NONE', *, *, #39989, .F. ) ;
#25144 = CARTESIAN_POINT ( 'NONE',  ( 53.06129598958289506, -49.54289835688069843, -48.87622692776139388 ) ) ;
#25145 = EDGE_CURVE ( 'NONE', #21555, #18765, #28752, .T. ) ;
#25146 = CARTESIAN_POINT ( 'NONE',  ( 61.56839264358480079, -45.12835126257370177, -27.89781785035500050 ) ) ;
#25147 = CARTESIAN_POINT ( 'NONE',  ( 12.14991548571375368, -22.52877406651395376, -74.45899817883974947 ) ) ;
#25148 = CARTESIAN_POINT ( 'NONE',  ( 56.79768778468150003, 14.70793938441589965, -26.22464504602800162 ) ) ;
#25149 = CARTESIAN_POINT ( 'NONE',  ( 19.77219298086049903, -22.11770738490020349, -80.57026077041129497 ) ) ;
#25150 = CARTESIAN_POINT ( 'NONE',  ( 50.65222607392030341, 18.77326448281979765, -76.16386725149659753 ) ) ;
#25151 = CARTESIAN_POINT ( 'NONE',  ( 52.70437010560439717, 18.50693821689120000, -48.55295696688259710 ) ) ;
#25152 = CARTESIAN_POINT ( 'NONE',  ( 71.01106396815980304, 1.383811055320669947, -70.34375346881599000 ) ) ;
#25153 = DIRECTION ( 'NONE',  ( 0.000000000000000000, 0.000000000000000000, 1.000000000000000000 ) ) ;
#25154 = CARTESIAN_POINT ( 'NONE',  ( 73.90096124267101629, -43.37807912905199714, -12.95075084354250095 ) ) ;
#25155 = VERTEX_POINT ( 'NONE', #2504 ) ;
#25156 = CARTESIAN_POINT ( 'NONE',  ( 16.58539016039730285, -8.179598009217608379, -72.58664262352569096 ) ) ;
#25157 = EDGE_LOOP ( 'NONE', ( #22426, #15393, #35759, #39928 ) ) ;
#25158 = CARTESIAN_POINT ( 'NONE',  ( 73.06536971133249381, 1.096932441169210071, -69.00001114258428458 ) ) ;
#25159 = CARTESIAN_POINT ( 'NONE',  ( 47.43216622799359783, -54.63853425152050391, -54.88096955750960149 ) ) ;
#25160 = CARTESIAN_POINT ( 'NONE',  ( 17.45133669559110956, -7.792397174005662563, -49.34550584340571788 ) ) ;
#25161 = CARTESIAN_POINT ( 'NONE',  ( 73.02088654388471411, 1.338092079250050137, -62.67980446285670126 ) ) ;
#25162 = CARTESIAN_POINT ( 'NONE',  ( 8.222313118464692039, -15.61611924975770016, -60.79233150823699816 ) ) ;
#25163 = B_SPLINE_CURVE_WITH_KNOTS ( 'NONE', 3,
 ( #24497, #674, #20578, #20840, #24235, #13013, #36837, #32882, #36062, #40515, #48124, #48916, #4604, #8287, #44967, #12748, #36571, #28703 ),
 .UNSPECIFIED., .F., .F.,
 ( 4, 2, 2, 2, 2, 2, 2, 2, 4 ),
 ( 0.000000000000000000, 0.06250019609009530019, 0.1250003921801906004, 0.1875005882702859006, 0.2500007843603812008, 0.3125009804504764732, 0.3750011765405718012, 0.4375013726306671291, 0.5000015687207624016 ),
 .UNSPECIFIED. ) ;
#25164 = CARTESIAN_POINT ( 'NONE',  ( 71.33393739769660158, 1.396834109478129804, -61.06337307536559678 ) ) ;
#25165 = LINE ( 'NONE', #16809, #27498 ) ;
#25166 = CARTESIAN_POINT ( 'NONE',  ( 71.99615133745550111, 1.261444690199579943, -61.15177544325119641 ) ) ;
#25167 = AXIS2_PLACEMENT_3D ( 'NONE', #20409, #28019, #40599 ) ;
#25168 = CARTESIAN_POINT ( 'NONE',  ( 24.04493739769619864, -15.61618894467929941, -32.14999999999999858 ) ) ;
#25169 = ORIENTED_EDGE ( 'NONE', *, *, #7509, .F. ) ;
#25170 = CARTESIAN_POINT ( 'NONE',  ( 65.25681082723269810, 1.383811055320669947, -70.34375346881599000 ) ) ;
#25171 = VERTEX_POINT ( 'NONE', #39446 ) ;
#25172 = ORIENTED_EDGE ( 'NONE', *, *, #36175, .F. ) ;
#25173 = CARTESIAN_POINT ( 'NONE',  ( 9.273487956746848226, -63.11543068638779630, -46.53410025525219851 ) ) ;
#25174 = LINE ( 'NONE', #13167, #30229 ) ;
#25175 = VERTEX_POINT ( 'NONE', #50719 ) ;
#25176 = FACE_OUTER_BOUND ( 'NONE', #17843, .T. ) ;
#25177 = CARTESIAN_POINT ( 'NONE',  ( 84.02702888049316243, 13.40383544920428172, -47.45289756459199992 ) ) ;
#25178 = PLANE ( 'NONE',  #48752 ) ;
#25179 = EDGE_CURVE ( 'NONE', #483, #32383, #22914, .T. ) ;
#25180 = CARTESIAN_POINT ( 'NONE',  ( 53.39545258799459759, 19.65859595880879951, -76.18303073696110062 ) ) ;
#25181 = VERTEX_POINT ( 'NONE', #11153 ) ;
#25182 = CARTESIAN_POINT ( 'NONE',  ( 14.63393739769630031, 0.9255523191757060175, -34.64999999999999858 ) ) ;
#25183 = CARTESIAN_POINT ( 'NONE',  ( 51.13393739769659874, -50.61618894467899565, 16.85000000000000142 ) ) ;
#25184 = CARTESIAN_POINT ( 'NONE',  ( 8.654140298178170099, -18.27765407811988752, -66.39876892714730161 ) ) ;
#25185 = ADVANCED_FACE ( 'NONE', ( #2767 ), #3547, .T. ) ;
#25186 = CARTESIAN_POINT ( 'NONE',  ( 15.17406030731610045, -7.427089114582080320, -55.25519061113279662 ) ) ;
#25187 = CARTESIAN_POINT ( 'NONE',  ( 26.13393739769619728, -15.61618894467929941, -2.149999999999999911 ) ) ;
#25188 = CARTESIAN_POINT ( 'NONE',  ( 42.29796674348754948, -37.67109563684581985, -78.82985224857310413 ) ) ;
#25189 = ORIENTED_EDGE ( 'NONE', *, *, #48803, .F. ) ;
#25190 = CARTESIAN_POINT ( 'NONE',  ( 56.55522355860080097, -46.21195502513410247, -26.26695352263039851 ) ) ;
#25191 = CARTESIAN_POINT ( 'NONE',  ( 15.69588917291320129, -8.178796420554320434, -45.71393110241879754 ) ) ;
#25192 = ADVANCED_FACE ( 'NONE', ( #38933 ), #16839, .T. ) ;
#25193 = DIRECTION ( 'NONE',  ( 1.000000000000000000, 0.000000000000000000, 0.000000000000000000 ) ) ;
#25194 = CARTESIAN_POINT ( 'NONE',  ( 14.54665750016330072, 20.57774151326000123, -75.67041253543301593 ) ) ;
#25195 = EDGE_CURVE ( 'NONE', #7027, #9837, #43379, .T. ) ;
#25196 = CARTESIAN_POINT ( 'NONE',  ( 51.99247536373789558, 18.26518850788540149, -77.11022606388370093 ) ) ;
#25197 = DIRECTION ( 'NONE',  ( -1.000000000000000000, 0.000000000000000000, 0.000000000000000000 ) ) ;
#25198 = VECTOR ( 'NONE', #51369, 1000.000000000000000 ) ;
#25199 = CARTESIAN_POINT ( 'NONE',  ( 13.45088311011700100, -23.41259455232169984, -52.11317062803209410 ) ) ;
#25200 = VERTEX_POINT ( 'NONE', #18998 ) ;
#25201 = CARTESIAN_POINT ( 'NONE',  ( 55.83353943854869783, -46.18894462837869952, -25.84382037829299961 ) ) ;
#25202 = CARTESIAN_POINT ( 'NONE',  ( 14.48916582606740100, -51.10390356942439638, -22.14433180932410039 ) ) ;
#25203 = DIRECTION ( 'NONE',  ( -0.7071067811865475727, 0.7071067811865475727, 0.000000000000000000 ) ) ;
#25204 = DIRECTION ( 'NONE',  ( 0.000000000000000000, 0.000000000000000000, 1.000000000000000000 ) ) ;
#25205 = DIRECTION ( 'NONE',  ( 0.000000000000000000, 0.000000000000000000, -1.000000000000000000 ) ) ;
#25206 = EDGE_LOOP ( 'NONE', ( #22596, #18337, #50276, #23230, #9192 ) ) ;
#25207 = CARTESIAN_POINT ( 'NONE',  ( -5.145629218704510066, -47.11336362869789696, -4.652761024381289801 ) ) ;
#25208 = CARTESIAN_POINT ( 'NONE',  ( 47.20789225325369642, 23.55536091824439637, -54.64146362385890399 ) ) ;
#25209 = ADVANCED_FACE ( 'NONE', ( #6444 ), #18738, .T. ) ;
#25210 = CARTESIAN_POINT ( 'NONE',  ( 55.91595722987329964, -45.90465052577939531, -25.32543029193989881 ) ) ;
#25211 = CARTESIAN_POINT ( 'NONE',  ( 63.36539477273620236, 1.325715844996850024, -62.41274800841679848 ) ) ;
#25212 = CARTESIAN_POINT ( 'NONE',  ( 17.98749078828947745, -41.76263555408611694, -34.79644660940672907 ) ) ;
#25213 = CARTESIAN_POINT ( 'NONE',  ( 11.50291098922579991, 34.11720288171970594, -17.75618560011610114 ) ) ;
#25214 = CARTESIAN_POINT ( 'NONE',  ( 16.13393739769620083, -15.61618894467929941, -7.139181489322110608 ) ) ;
#25215 = DIRECTION ( 'NONE',  ( 0.000000000000000000, -1.000000000000000000, 0.000000000000000000 ) ) ;
#25216 = CARTESIAN_POINT ( 'NONE',  ( 72.33986051001160433, 1.456055805561079941, -61.71730126733579169 ) ) ;
#25217 = CARTESIAN_POINT ( 'NONE',  ( 58.76768575440100051, -46.69271212826609485, -47.97336379875430623 ) ) ;
#25218 = CARTESIAN_POINT ( 'NONE',  ( 22.21960090659290188, -18.66279415813841069, -66.60040840573597620 ) ) ;
#25219 = ADVANCED_FACE ( 'NONE', ( #7476 ), #937, .F. ) ;
#25220 = CARTESIAN_POINT ( 'NONE',  ( 52.78762917051419379, 21.08910179861619838, -54.06354383229390237 ) ) ;
#25221 = CARTESIAN_POINT ( 'NONE',  ( 63.30597626835550784, 1.134959972145540119, -69.13433375889879073 ) ) ;
#25222 = CARTESIAN_POINT ( 'NONE',  ( 12.72599752907515658, -9.703248301412761734, -47.78615421569977428 ) ) ;
#25223 = ORIENTED_EDGE ( 'NONE', *, *, #2851, .T. ) ;
#25224 = LINE ( 'NONE', #33353, #12919 ) ;
#25225 = CARTESIAN_POINT ( 'NONE',  ( 9.739018438830168378, 32.00108083321330099, -46.29762906764769781 ) ) ;
#25226 = CARTESIAN_POINT ( 'NONE',  ( 66.10673863877181589, -29.76883965895079953, -16.72118890776879852 ) ) ;
#25227 = CARTESIAN_POINT ( 'NONE',  ( 33.38393739769599478, 10.53025766472752522, -34.79644660940672907 ) ) ;
#25228 = VERTEX_POINT ( 'NONE', #51497 ) ;
#25229 = CARTESIAN_POINT ( 'NONE',  ( 18.21797964295990013, 20.46947493835569887, -75.41867332334460627 ) ) ;
#25230 = EDGE_LOOP ( 'NONE', ( #20591, #8374, #43260, #36623 ) ) ;
#25231 = VERTEX_POINT ( 'NONE', #43125 ) ;
#25232 = LINE ( 'NONE', #21825, #10305 ) ;
#25233 = EDGE_LOOP ( 'NONE', ( #32416, #21363, #17089, #13738 ) ) ;
#25234 = CARTESIAN_POINT ( 'NONE',  ( 12.33080418725089977, -65.41125055805170518, -47.27598567016929820 ) ) ;
#25235 = CARTESIAN_POINT ( 'NONE',  ( 56.48760883520149889, -46.18664620669910192, -26.24751697164999698 ) ) ;
#25236 = CARTESIAN_POINT ( 'NONE',  ( 21.36642042239409989, -20.32905245748499823, -81.23899999999999011 ) ) ;
#25237 = LINE ( 'NONE', #9801, #44042 ) ;
#25238 = EDGE_CURVE ( 'NONE', #39742, #50075, #14329, .T. ) ;
#25239 = AXIS2_PLACEMENT_3D ( 'NONE', #12221, #44186, #19565 ) ;
#25240 = CARTESIAN_POINT ( 'NONE',  ( 61.51623078522280252, 13.93866689514799972, -46.75536389823849959 ) ) ;
#25241 = DIRECTION ( 'NONE',  ( 0.000000000000000000, 0.000000000000000000, 1.000000000000000000 ) ) ;
#25242 = ORIENTED_EDGE ( 'NONE', *, *, #20221, .F. ) ;
#25243 = CIRCLE ( 'NONE', #15205, 0.5000000000000045519 ) ;
#25244 = CARTESIAN_POINT ( 'NONE',  ( 22.90125369822447610, -15.85481226531381616, -68.85839675053532005 ) ) ;
#25245 = AXIS2_PLACEMENT_3D ( 'NONE', #1996, #10381, #9608 ) ;
#25246 = EDGE_CURVE ( 'NONE', #18765, #11901, #38634, .T. ) ;
#25247 = ORIENTED_EDGE ( 'NONE', *, *, #35323, .F. ) ;
#25248 = CARTESIAN_POINT ( 'NONE',  ( 49.47280132910630357, -45.11618894461000195, -10.20974854288130018 ) ) ;
#25249 = CARTESIAN_POINT ( 'NONE',  ( 22.90093739769620029, -15.61618894467913243, -28.45282021618999835 ) ) ;
#25250 = CARTESIAN_POINT ( 'NONE',  ( 11.73137203405248385, 10.53025766472752522, -34.79644660940672907 ) ) ;
#25251 = EDGE_LOOP ( 'NONE', ( #2752, #47813, #44264, #38679 ) ) ;
#25252 = LINE ( 'NONE', #45193, #14113 ) ;
#25253 = CARTESIAN_POINT ( 'NONE',  ( 47.19185019601420095, -54.76658792525179820, -74.50414561666529778 ) ) ;
#25254 = CARTESIAN_POINT ( 'NONE',  ( 47.13393739769619373, 4.883811055320659733, -54.64999999999999858 ) ) ;
#25255 = CARTESIAN_POINT ( 'NONE',  ( 54.47259994055220034, 15.01996530865999979, -15.76423849626599960 ) ) ;
#25256 = DIRECTION ( 'NONE',  ( 0.6911981449639427177, -0.7226652920947596037, 0.000000000000000000 ) ) ;
#25257 = DIRECTION ( 'NONE',  ( 1.000000000000000000, 0.000000000000000000, 0.000000000000000000 ) ) ;
#25258 = CARTESIAN_POINT ( 'NONE',  ( 9.367050196127319595, -15.61601677469269944, -55.84717978380999881 ) ) ;
#25259 = CARTESIAN_POINT ( 'NONE',  ( 57.71856222965350014, 13.89769183763849902, -25.57520695384850029 ) ) ;
#25260 = CARTESIAN_POINT ( 'NONE',  ( 22.29316687837529898, -20.47938135168080009, -75.50024918233970084 ) ) ;
#25261 = VERTEX_POINT ( 'NONE', #34976 ) ;
#25262 = CARTESIAN_POINT ( 'NONE',  ( 59.95384340470150164, 14.69603373565070115, -47.36701927546829438 ) ) ;
#25263 = LINE ( 'NONE', #37862, #15237 ) ;
#25264 = CARTESIAN_POINT ( 'NONE',  ( 46.82538613462318722, -34.56499699448699658, -54.61944740401202125 ) ) ;
#25265 = FACE_OUTER_BOUND ( 'NONE', #28058, .T. ) ;
#25266 = AXIS2_PLACEMENT_3D ( 'NONE', #49384, #22603, #22344 ) ;
#25267 = AXIS2_PLACEMENT_3D ( 'NONE', #7527, #31599, #50776 ) ;
#25269 = CARTESIAN_POINT ( 'NONE',  ( 14.63393739769640156, 10.88381105532070059, -34.64999999999999858 ) ) ;
#25268 = AXIS2_PLACEMENT_3D ( 'NONE', #89, #32790, #3764 ) ;
#25270 = CARTESIAN_POINT ( 'NONE',  ( 22.48834434154391104, -10.88577583731355425, -65.30397204142286682 ) ) ;
#25271 = CARTESIAN_POINT ( 'NONE',  ( 9.367479537931210132, -15.61613030728229923, -79.45282021618999124 ) ) ;
#25272 = CARTESIAN_POINT ( 'NONE',  ( 49.13043947778380272, -53.90062760971940037, -55.21565379135309826 ) ) ;
#25273 = CARTESIAN_POINT ( 'NONE',  ( 51.19324896229723976, -31.68074559396569256, -17.14371393497826901 ) ) ;
#25274 = EDGE_CURVE ( 'NONE', #35178, #18174, #6963, .T. ) ;
#25275 = CARTESIAN_POINT ( 'NONE',  ( 8.713805725719740991, -18.46962709096431254, -34.39090680685740153 ) ) ;
#25276 = DIRECTION ( 'NONE',  ( 1.000000000000000000, 0.000000000000000000, 0.000000000000000000 ) ) ;
#25277 = EDGE_CURVE ( 'NONE', #12905, #41446, #20159, .T. ) ;
#25278 = ORIENTED_EDGE ( 'NONE', *, *, #49418, .T. ) ;
#25279 = CARTESIAN_POINT ( 'NONE',  ( 23.49651994093389717, -14.47642026974889795, -45.01845461338599819 ) ) ;
#25280 = CARTESIAN_POINT ( 'NONE',  ( 64.50758838025409148, 1.321111291668120025, -61.05922999307440335 ) ) ;
#25281 = ORIENTED_EDGE ( 'NONE', *, *, #6662, .F. ) ;
#25282 = CARTESIAN_POINT ( 'NONE',  ( 10.97210468079044610, 32.23756417331421176, -23.98816728309424917 ) ) ;
#25283 = CARTESIAN_POINT ( 'NONE',  ( 60.88289654404759688, -45.68840397722050284, -47.72275522894760513 ) ) ;
#25284 = CARTESIAN_POINT ( 'NONE',  ( 23.37006864188870026, 18.01372606128889942, -34.65445009297679491 ) ) ;
#25285 = CARTESIAN_POINT ( 'NONE',  ( 12.89656437789989951, 18.76901986582059934, -21.06838189635490011 ) ) ;
#25287 = DIRECTION ( 'NONE',  ( -1.000000000000000000, -1.040834085586084257E-16, 0.000000000000000000 ) ) ;
#25286 = CARTESIAN_POINT ( 'NONE',  ( 45.24585991142964048, 8.815101637006968360, -60.61901997089581329 ) ) ;
#25288 = DIRECTION ( 'NONE',  ( -0.3863301728269175062, -0.9223605572462019175, 3.330669073875470114E-16 ) ) ;
#25289 = DIRECTION ( 'NONE',  ( 0.000000000000000000, 1.000000000000000000, 0.000000000000000000 ) ) ;
#25290 = VERTEX_POINT ( 'NONE', #19776 ) ;
#25291 = ORIENTED_EDGE ( 'NONE', *, *, #46926, .F. ) ;
#25292 = ORIENTED_EDGE ( 'NONE', *, *, #17794, .F. ) ;
#25293 = ORIENTED_EDGE ( 'NONE', *, *, #36750, .F. ) ;
#25294 = CARTESIAN_POINT ( 'NONE',  ( 61.50647473645999952, -45.22354326066130170, -47.00768424768439502 ) ) ;
#25295 = DIRECTION ( 'NONE',  ( 0.000000000000000000, 0.000000000000000000, 1.000000000000000000 ) ) ;
#25296 = CARTESIAN_POINT ( 'NONE',  ( 54.39599759010950208, -51.37714874329250136, -53.12073448206439963 ) ) ;
#25297 = ORIENTED_EDGE ( 'NONE', *, *, #33775, .T. ) ;
#25298 = ORIENTED_EDGE ( 'NONE', *, *, #8877, .T. ) ;
#25299 = EDGE_CURVE ( 'NONE', #9595, #42519, #24708, .T. ) ;
#25300 = CARTESIAN_POINT ( 'NONE',  ( 23.06214062797170072, -3.616188944679349593, -24.15000000000000213 ) ) ;
#25301 = ORIENTED_EDGE ( 'NONE', *, *, #42829, .F. ) ;
#25302 = CARTESIAN_POINT ( 'NONE',  ( 22.90071998467804804, -15.61618839864605057, -72.45282571548244732 ) ) ;
#25303 = CARTESIAN_POINT ( 'NONE',  ( 9.511343591802949859, -13.64028796437523461, -45.94011037906290085 ) ) ;
#25304 = DIRECTION ( 'NONE',  ( 0.000000000000000000, 0.000000000000000000, 1.000000000000000000 ) ) ;
#25305 = CARTESIAN_POINT ( 'NONE',  ( 56.46551779669420057, -50.77616595281960343, -53.85225392423020452 ) ) ;
#25306 = CARTESIAN_POINT ( 'NONE',  ( 62.88393739769619373, 4.883811055320659733, -84.94863984844531046 ) ) ;
#25307 = VERTEX_POINT ( 'NONE', #12962 ) ;
#25308 = B_SPLINE_CURVE_WITH_KNOTS ( 'NONE', 3,
 ( #3750, #43070, #19201, #28863, #51695, #32004, #47771, #15789, #11877, #32774, #32256, #570, #44867, #48024, #28598, #318, #36724, #8449 ),
 .UNSPECIFIED., .F., .F.,
 ( 4, 2, 2, 2, 2, 2, 2, 2, 4 ),
 ( 0.000000000000000000, 0.06249981108821953124, 0.1249996221764390625, 0.1874994332646585937, 0.2499992443528781250, 0.3124990554410977950, 0.3749988665293174095, 0.4374986776175370795, 0.4999984887057566940 ),
 .UNSPECIFIED. ) ;
#25309 = DIRECTION ( 'NONE',  ( 0.000000000000000000, 0.7071067811865463515, -0.7071067811865487940 ) ) ;
#25311 = CARTESIAN_POINT ( 'NONE',  ( 53.51849515060609974, -51.02420518644899516, -75.95517920710381077 ) ) ;
#25310 = AXIS2_PLACEMENT_3D ( 'NONE', #37195, #21699, #21959 ) ;
#25312 = CARTESIAN_POINT ( 'NONE',  ( 20.98630067873081728, -20.33298601347895129, -46.69830337009432952 ) ) ;
#25313 = CARTESIAN_POINT ( 'NONE',  ( 60.39786843514819736, 14.46339658146679952, -47.23199723846380493 ) ) ;
#25314 = CARTESIAN_POINT ( 'NONE',  ( 10.22062101548030100, -20.77559171587279963, -68.78413393247190299 ) ) ;
#25315 = DIRECTION ( 'NONE',  ( -1.010747651509595448E-22, -1.000000000000000000, 3.858400438143729530E-12 ) ) ;
#25316 = CARTESIAN_POINT ( 'NONE',  ( 41.74196416991780012, 13.83302381481709986, -5.934307256532159514 ) ) ;
#25317 = CARTESIAN_POINT ( 'NONE',  ( 42.47447998003330127, -44.18050766653550454, -5.039225367523919807 ) ) ;
#25318 = CARTESIAN_POINT ( 'NONE',  ( 69.22748654599971019, -50.70395984887900909, -74.34354914830332461 ) ) ;
#25319 = CARTESIAN_POINT ( 'NONE',  ( 67.45368034285870351, 1.609458251574180432, -19.55784009146304214 ) ) ;
#25320 = CARTESIAN_POINT ( 'NONE',  ( 64.40830624361899481, 1.428532738834869864, -70.03330250477451102 ) ) ;
#25321 = DIRECTION ( 'NONE',  ( 0.000000000000000000, 0.000000000000000000, -1.000000000000000000 ) ) ;
#25322 = CARTESIAN_POINT ( 'NONE',  ( 65.36113773965780638, 1.378962859947149955, -18.37587875859610165 ) ) ;
#25323 = ORIENTED_EDGE ( 'NONE', *, *, #51511, .T. ) ;
#25324 = CARTESIAN_POINT ( 'NONE',  ( 14.36865994475110142, -51.35369855970039765, -75.11575902016450357 ) ) ;
#25325 = AXIS2_PLACEMENT_3D ( 'NONE', #46669, #50331, #26455 ) ;
#25326 = CARTESIAN_POINT ( 'NONE',  ( 47.21621394679169725, -54.78114590934789874, -54.62203065971809934 ) ) ;
#25327 = DIRECTION ( 'NONE',  ( 0.000000000000000000, 0.000000000000000000, -1.000000000000000000 ) ) ;
#25328 = FACE_BOUND ( 'NONE', #24901, .T. ) ;
#25329 =( BOUNDED_SURFACE ( )  B_SPLINE_SURFACE ( 2, 2, ( 
 ( #7347, #11025, #19894, #23295, #3934, #31420, #31676, #31166, #7608 ),
 ( #35888, #47194, #11542, #15469, #31934, #3, #7861, #246, #19130 ),
 ( #30910, #43506, #23809, #35640, #43759, #26994, #39827, #7097, #35109 ),
 ( #51109, #11281, #27764, #46940, #23048, #3160, #43000, #15212, #51625 ),
 ( #15980, #8117, #47955, #19391, #11801, #12058, #28009, #44016, #27504 ) ),
 .UNSPECIFIED., .F., .T., .T. ) 
 B_SPLINE_SURFACE_WITH_KNOTS ( ( 3, 2, 3 ),
 ( 3, 2, 2, 2, 3 ),
 ( -0.003205554297748039981, 0.8238407534185530068, 1.650887061134849843 ),
 ( -3.141592653589790007, -1.570796326794899889, 0.000000000000000000, 1.570796326794899889, 3.141592653589790007 ),
 .UNSPECIFIED. ) 
 GEOMETRIC_REPRESENTATION_ITEM ( )  RATIONAL_B_SPLINE_SURFACE ( (
 ( 1.000000000000000000, 0.7071067811865480168, 1.000000000000000000, 0.7071067811865480168, 1.000000000000000000, 0.7071067811865480168, 1.000000000000000000, 0.7071067811865480168, 1.000000000000000000),
 ( 0.9157107718030679244, 0.6475052963475169676, 0.9157107718030679244, 0.6475052963475169676, 0.9157107718030679244, 0.6475052963475169676, 0.9157107718030679244, 0.6475052963475169676, 0.9157107718030679244),
 ( 1.000000000000000000, 0.7071067811865480168, 1.000000000000000000, 0.7071067811865480168, 1.000000000000000000, 0.7071067811865480168, 1.000000000000000000, 0.7071067811865480168, 1.000000000000000000),
 ( 0.9157107718030469412, 0.6475052963475019796, 0.9157107718030469412, 0.6475052963475019796, 0.9157107718030469412, 0.6475052963475019796, 0.9157107718030469412, 0.6475052963475019796, 0.9157107718030469412),
 ( 1.000000000000000000, 0.7071067811865480168, 1.000000000000000000, 0.7071067811865480168, 1.000000000000000000, 0.7071067811865480168, 1.000000000000000000, 0.7071067811865480168, 1.000000000000000000) ) ) 
 REPRESENTATION_ITEM ( '' )  SURFACE ( )  );
#25330 = CARTESIAN_POINT ( 'NONE',  ( 23.28706766060589928, -17.69237313545239942, -32.14999999999999858 ) ) ;
#25331 = LINE ( 'NONE', #4654, #25580 ) ;
#25332 = DIRECTION ( 'NONE',  ( 0.000000000000000000, 0.000000000000000000, -1.000000000000000000 ) ) ;
#25334 = CARTESIAN_POINT ( 'NONE',  ( 16.65420337845429799, 19.88381105532299742, -20.15000000000000213 ) ) ;
#25333 = CARTESIAN_POINT ( 'NONE',  ( 4.133937397696209715, -22.54439217495480108, -47.64999999999999858 ) ) ;
#25335 = EDGE_CURVE ( 'NONE', #40528, #47610, #20015, .T. ) ;
#25336 = CARTESIAN_POINT ( 'NONE',  ( 56.38082786511019862, 19.49268417552400123, -53.29063683202039670 ) ) ;
#25337 = CARTESIAN_POINT ( 'NONE',  ( 20.63393739769620083, -41.61618894467930119, -54.64999999999999858 ) ) ;
#25338 = CARTESIAN_POINT ( 'NONE',  ( 48.55128749046469494, 22.77231967830010007, -54.59786143027240257 ) ) ;
#25339 = ORIENTED_EDGE ( 'NONE', *, *, #4107, .T. ) ;
#25340 = AXIS2_PLACEMENT_3D ( 'NONE', #16681, #28988, #33172 ) ;
#25341 = CARTESIAN_POINT ( 'NONE',  ( 9.319736165278609263, -13.79706257782909873, -67.93021958131210170 ) ) ;
#25342 = CIRCLE ( 'NONE', #9490, 2.000000000000000000 ) ;
#25343 = VERTEX_POINT ( 'NONE', #12176 ) ;
#25344 = PLANE ( 'NONE',  #39589 ) ;
#25345 = CARTESIAN_POINT ( 'NONE',  ( 53.55347996444381664, -49.37856166211688702, -49.15350056090469621 ) ) ;
#25346 = DIRECTION ( 'NONE',  ( 0.3445670372598628184, 0.6174735272333260472, -0.7071067811865442421 ) ) ;
#25348 = CARTESIAN_POINT ( 'NONE',  ( 54.40762147712389663, 16.55776885928690234, -25.97561773943489882 ) ) ;
#25347 = CARTESIAN_POINT ( 'NONE',  ( 84.44303304399450383, 12.08919773384380036, -47.45512980871949793 ) ) ;
#25349 = CARTESIAN_POINT ( 'NONE',  ( 18.37403219540230026, -8.928548554084470013, -66.05570249522909876 ) ) ;
#25350 = PLANE ( 'NONE',  #32889 ) ;
#25351 = CARTESIAN_POINT ( 'NONE',  ( 72.74776047649530142, 1.391252479931859964, -68.77264296518760034 ) ) ;
#25352 = CARTESIAN_POINT ( 'NONE',  ( 44.13393739769620083, -33.11618894467930829, -54.27132075603720551 ) ) ;
#25353 = ORIENTED_EDGE ( 'NONE', *, *, #22572, .F. ) ;
#25354 = ORIENTED_EDGE ( 'NONE', *, *, #30300, .T. ) ;
#25355 = CARTESIAN_POINT ( 'NONE',  ( 11.79921494304270091, -65.04093993986319333, -16.52202905013960077 ) ) ;
#25357 = ADVANCED_FACE ( 'NONE', ( #32312 ), #7982, .T. ) ;
#25356 = CARTESIAN_POINT ( 'NONE',  ( 11.13393739775729863, 32.27424679965390197, -43.95119008811450101 ) ) ;
#25358 = CARTESIAN_POINT ( 'NONE',  ( -11.39236625349550103, 2.585530954890270294, -54.64999999999999858 ) ) ;
#25359 = CARTESIAN_POINT ( 'NONE',  ( 19.54195246423347854, -21.52908623084648099, -54.78615564698215223 ) ) ;
#25360 = CARTESIAN_POINT ( 'NONE',  ( 10.13693646489610067, -64.73981908445260558, -47.01156321116880576 ) ) ;
#25361 = VERTEX_POINT ( 'NONE', #36263 ) ;
#25362 = ADVANCED_FACE ( 'NONE', ( #372 ), #8760, .T. ) ;
#25363 = CARTESIAN_POINT ( 'NONE',  ( -22.72534110410520114, -11.79254667875349938, -54.70989275527219320 ) ) ;
#25364 = CARTESIAN_POINT ( 'NONE',  ( 53.71518589158228707, 17.65496981945476662, -27.13660862535111562 ) ) ;
#25365 = AXIS2_PLACEMENT_3D ( 'NONE', #41346, #13326, #8872 ) ;
#25366 = CARTESIAN_POINT ( 'NONE',  ( 22.46009878491385336, -20.47787216187520087, -59.71601578695964463 ) ) ;
#25367 = ADVANCED_FACE ( 'NONE', ( #16353 ), #24448, .T. ) ;
#25368 = DIRECTION ( 'NONE',  ( 0.5516667872527449834, -0.8340645993220396903, -3.885780586188043947E-16 ) ) ;
#25369 = CARTESIAN_POINT ( 'NONE',  ( 50.67690155642070238, -50.61106055578139973, -76.14999999999999147 ) ) ;
#25370 = LINE ( 'NONE', #29565, #17094 ) ;
#25371 = ORIENTED_EDGE ( 'NONE', *, *, #5199, .F. ) ;
#25372 = CARTESIAN_POINT ( 'NONE',  ( 53.55220836886790181, -48.78100643530040514, -26.47327747818699706 ) ) ;
#25373 = CARTESIAN_POINT ( 'NONE',  ( 68.13393739769814772, 19.38381105532029736, -71.50000000000200373 ) ) ;
#25374 = VERTEX_POINT ( 'NONE', #20789 ) ;
#25375 = CARTESIAN_POINT ( 'NONE',  ( 23.04645729084084493, -11.63205128005230193, -53.62566746339389567 ) ) ;
#25376 = CARTESIAN_POINT ( 'NONE',  ( 47.27830536510050052, -46.14749639572039541, -10.52818769379789821 ) ) ;
#25377 = CARTESIAN_POINT ( 'NONE',  ( 11.04448286797610024, -9.129022697162250566, -81.08056213787290289 ) ) ;
#25378 = CARTESIAN_POINT ( 'NONE',  ( 9.366647546311250849, -15.61604444486649967, -65.84717978381009118 ) ) ;
#25379 = CARTESIAN_POINT ( 'NONE',  ( 53.91674685403769729, 19.61716007771000037, -76.09466592280320185 ) ) ;
#25380 = CARTESIAN_POINT ( 'NONE',  ( 47.40869509741950338, -54.46061727596239876, -74.94674070344109396 ) ) ;
#25381 = ORIENTED_EDGE ( 'NONE', *, *, #38703, .F. ) ;
#25382 = CARTESIAN_POINT ( 'NONE',  ( 55.98930672876529968, 14.33000371823360020, -16.77916391804700069 ) ) ;
#25383 = CARTESIAN_POINT ( 'NONE',  ( 57.35856959117180054, -50.13596281943610222, -52.61941485247680106 ) ) ;
#25384 = CIRCLE ( 'NONE', #41303, 6.000000000000000000 ) ;
#25385 = CARTESIAN_POINT ( 'NONE',  ( 22.62449386613170077, -18.37576063303379925, -34.97514425884629929 ) ) ;
#25386 = DIRECTION ( 'NONE',  ( 0.8660254037844384856, -0.5000000000000003331, -2.775557561562892337E-16 ) ) ;
#25387 = ORIENTED_EDGE ( 'NONE', *, *, #6371, .F. ) ;
#25388 = CARTESIAN_POINT ( 'NONE',  ( 46.76255008597159701, 22.27812416600520251, -76.02679354016848379 ) ) ;
#25389 = CARTESIAN_POINT ( 'NONE',  ( 64.98600614086828386, 1.191644800533210091, -60.65994692684869705 ) ) ;
#25390 = CARTESIAN_POINT ( 'NONE',  ( 75.16204195899146612, -29.53650206104261500, -11.85619338644309551 ) ) ;
#25391 = CARTESIAN_POINT ( 'NONE',  ( 63.63393739769619373, 21.88381105532059934, 16.35000000000000142 ) ) ;
#25392 = CARTESIAN_POINT ( 'NONE',  ( 22.11006429370840110, -9.935574188519110450, -81.26573725944388116 ) ) ;
#25393 = AXIS2_PLACEMENT_3D ( 'NONE', #23560, #11806, #7351 ) ;
#25394 = CARTESIAN_POINT ( 'NONE',  ( 84.44784216359251161, -43.11618894467930119, -47.47585302082339354 ) ) ;
#25396 = CARTESIAN_POINT ( 'NONE',  ( 47.17883912218999853, -39.34270251064258161, -54.71052591825291245 ) ) ;
#25395 = CARTESIAN_POINT ( 'NONE',  ( 68.13393739769620083, -15.61618894467929941, -65.65000000000000568 ) ) ;
#25397 = ADVANCED_FACE ( 'NONE', ( #43635 ), #23934, .F. ) ;
#25398 = DIRECTION ( 'NONE',  ( -0.6676418852213052979, 0.2329255526947255628, -0.7071067811865461294 ) ) ;
#25399 = CARTESIAN_POINT ( 'NONE',  ( 6.300025116801259983, -65.10110191454670314, -48.92608059699489331 ) ) ;
#25400 = ADVANCED_FACE ( 'NONE', ( #27883 ), #28394, .F. ) ;
#25401 = ORIENTED_EDGE ( 'NONE', *, *, #14274, .T. ) ;
#25402 = CARTESIAN_POINT ( 'NONE',  ( 52.77257543143819873, -49.69364411959510619, -48.57105728902469366 ) ) ;
#25403 = ORIENTED_EDGE ( 'NONE', *, *, #37018, .T. ) ;
#25404 = CARTESIAN_POINT ( 'NONE',  ( 61.75043129679379916, -45.11618897208669665, -28.15142663286150437 ) ) ;
#25405 = CARTESIAN_POINT ( 'NONE',  ( 49.60483365582589954, -53.69855377821169640, -55.15230005116299594 ) ) ;
#25406 = LINE ( 'NONE', #21482, #23119 ) ;
#25407 = CARTESIAN_POINT ( 'NONE',  ( 9.697439554173731935, -18.49959911504659971, -35.31875724254479820 ) ) ;
#25408 = CARTESIAN_POINT ( 'NONE',  ( 50.47459370284359892, 19.05485954424960227, -76.14999999999999147 ) ) ;
#25409 = CARTESIAN_POINT ( 'NONE',  ( 52.73033965374710164, 18.49117935840850180, -48.63393906880330775 ) ) ;
#25410 = CARTESIAN_POINT ( 'NONE',  ( 60.45746832332759624, -45.66454841953329691, -47.21482551237440362 ) ) ;
#25411 = CARTESIAN_POINT ( 'NONE',  ( 46.61750669586271556, 22.00845647503780000, -76.11314270326337805 ) ) ;
#25412 = ORIENTED_EDGE ( 'NONE', *, *, #34899, .F. ) ;
#25413 = VECTOR ( 'NONE', #46217, 999.9999999999998863 ) ;
#25414 = CARTESIAN_POINT ( 'NONE',  ( 17.96388931505610387, -8.394141429016420020, -74.64633483117968638 ) ) ;
#25416 = CARTESIAN_POINT ( 'NONE',  ( 72.85976395805219852, 1.369613126987639928, -68.75357062980060618 ) ) ;
#25415 = AXIS2_PLACEMENT_3D ( 'NONE', #49795, #42189, #34563 ) ;
#25417 = CARTESIAN_POINT ( 'NONE',  ( 47.50476691646419880, -54.58925063325320082, -54.77393688460149690 ) ) ;
#25418 = CARTESIAN_POINT ( 'NONE',  ( 19.58480251134974282, -8.478714239322904689, -49.43568005544015875 ) ) ;
#25419 = CARTESIAN_POINT ( 'NONE',  ( 11.53606103740170674, 24.11867657901759188, -21.73577486392030167 ) ) ;
#25420 = CARTESIAN_POINT ( 'NONE',  ( 56.45552857517409961, 19.30196012738109701, -52.91205108279270775 ) ) ;
#25421 = CARTESIAN_POINT ( 'NONE',  ( 71.35301946752790059, 1.370853092582090094, -60.97060118797210038 ) ) ;
#25422 = DIRECTION ( 'NONE',  ( 0.000000000000000000, 0.000000000000000000, 1.000000000000000000 ) ) ;
#25423 = CARTESIAN_POINT ( 'NONE',  ( 71.51437757259260763, 1.412203896155519889, -61.12765129660999719 ) ) ;
#25424 = ADVANCED_FACE ( 'NONE', ( #44399 ), #36781, .T. ) ;
#25425 = DIRECTION ( 'NONE',  ( 0.000000000000000000, 0.000000000000000000, -1.000000000000000000 ) ) ;
#25426 = CARTESIAN_POINT ( 'NONE',  ( 64.88733809717990653, 1.187415670095769871, -70.58414947367060677 ) ) ;
#25427 = VERTEX_POINT ( 'NONE', #16608 ) ;
#25428 = CARTESIAN_POINT ( 'NONE',  ( 9.291657151117041380, -63.23923423081338768, -46.52991438213880571 ) ) ;
#25429 = DIRECTION ( 'NONE',  ( 0.000000000000000000, -1.000000000000000000, 0.000000000000000000 ) ) ;
#25430 = ORIENTED_EDGE ( 'NONE', *, *, #45689, .F. ) ;
#25431 = ADVANCED_FACE ( 'NONE', ( #8499 ), #34342, .T. ) ;
#25432 = CARTESIAN_POINT ( 'NONE',  ( 53.63393739769619373, 21.88381105532059934, 11.84999999999999964 ) ) ;
#25433 = CARTESIAN_POINT ( 'NONE',  ( 10.72256258572000220, -11.45758887280185156, -69.66115420274824999 ) ) ;
#25434 = CARTESIAN_POINT ( 'NONE',  ( 15.98424424538390198, -22.66744068707240345, -53.35393626560600211 ) ) ;
#25435 = CARTESIAN_POINT ( 'NONE',  ( 51.83018428346819206, 19.54284939159689927, -76.24313691477149746 ) ) ;
#25436 = ORIENTED_EDGE ( 'NONE', *, *, #9593, .F. ) ;
#25437 = DIRECTION ( 'NONE',  ( 1.000000000000000000, 0.000000000000000000, 0.000000000000000000 ) ) ;
#25438 = DIRECTION ( 'NONE',  ( -1.000000000000000000, 0.000000000000000000, 0.000000000000000000 ) ) ;
#25439 = CARTESIAN_POINT ( 'NONE',  ( 24.04493740453103712, -15.60937728281429848, -43.79205105475155335 ) ) ;
#25440 = CARTESIAN_POINT ( 'NONE',  ( 7.917544350917670393, -14.92799903136709894, -50.81893047157019794 ) ) ;
#25441 = AXIS2_PLACEMENT_3D ( 'NONE', #22611, #38627, #34666 ) ;
#25442 = CARTESIAN_POINT ( 'NONE',  ( 20.45795268026760638, -10.33956678657632722, -56.17117403034256995 ) ) ;
#25443 = CARTESIAN_POINT ( 'NONE',  ( 41.94238982860078835, -37.61441522663087511, -80.60767011578155916 ) ) ;
#25444 = B_SPLINE_CURVE_WITH_KNOTS ( 'NONE', 3,
 ( #21599, #40759, #928, #21344, #32869, #17691, #37350, #9578, #33404, #40500, #1189, #16926, #4861, #44692, #48902, #13001, #12466, #28954, #45219, #48635, #8542, #41020, #28434, #8796, #4590, #49164, #20565, #36560, #9327, #661, #13258, #44955, #25275, #16650, #37093, #5389, #12735, #1449, #9056 ),
 .UNSPECIFIED., .F., .F.,
 ( 4, 2, 1, 1, 1, 1, 1, 2, 2, 2, 2, 2, 2, 2, 2, 2, 2, 2, 2, 2, 2, 4 ),
 ( 0.4999999442541762096, 0.5001220145802860451, 0.5002440849063958250, 0.5004882255586154960, 0.5009765068630547269, 0.5019530694719332997, 0.5039061946896904454, 0.5078124451252047367, 0.5156249459962332082, 0.5312499477382901514, 0.5624999512224040377, 0.5937499547065180350, 0.6249999581906319213, 0.6562499616747458075, 0.6874999651588598049, 0.7187499686429736911, 0.7499999721270875774, 0.7812499756112015747, 0.8124999790953154610, 0.8749999860635435667, 0.9374999930317717833, 1.000000000000000000 ),
 .UNSPECIFIED. ) ;
#25445 = ORIENTED_EDGE ( 'NONE', *, *, #39873, .F. ) ;
#25446 = CARTESIAN_POINT ( 'NONE',  ( 18.59699486872473884, 20.77208395163040322, -75.25166008050844368 ) ) ;
#25447 = CARTESIAN_POINT ( 'NONE',  ( 20.99980520150160146, -21.25799932088259681, -46.50612041305500099 ) ) ;
#25448 = CARTESIAN_POINT ( 'NONE',  ( 11.10779186475480174, -10.92055609319979936, -32.14999999999999858 ) ) ;
#25449 = AXIS2_PLACEMENT_3D ( 'NONE', #33868, #9787, #13213 ) ;
#25450 = CARTESIAN_POINT ( 'NONE',  ( 13.92353701934610122, 20.57110240350969832, -75.40982873507010709 ) ) ;
#25451 = AXIS2_PLACEMENT_3D ( 'NONE', #32233, #40386, #40130 ) ;
#25452 = CARTESIAN_POINT ( 'NONE',  ( 9.367478339302499180, -15.61624867646989756, -69.45282021618999124 ) ) ;
#25453 = CARTESIAN_POINT ( 'NONE',  ( -9.953010648345507860, -19.86500842468492323, -59.64999999999999147 ) ) ;
#25454 = CARTESIAN_POINT ( 'NONE',  ( 19.98923256093490153, -8.327881876965719243, -51.16254345526869685 ) ) ;
#25455 = ORIENTED_EDGE ( 'NONE', *, *, #38498, .T. ) ;
#25456 = CARTESIAN_POINT ( 'NONE',  ( 52.77799953798270138, -49.65042343486720000, -27.64301666048340067 ) ) ;
#25457 = CARTESIAN_POINT ( 'NONE',  ( 16.60579442219119883, -51.11619062814370551, -20.30246704093690013 ) ) ;
#25458 = CARTESIAN_POINT ( 'NONE',  ( 3.953188568412389969, 25.49695625375460040, -9.854466049057851507 ) ) ;
#25459 = ADVANCED_FACE ( 'NONE', ( #20468 ), #7675, .T. ) ;
#25460 = DIRECTION ( 'NONE',  ( 0.000000000000000000, 0.000000000000000000, 1.000000000000000000 ) ) ;
#25461 = CARTESIAN_POINT ( 'NONE',  ( -23.31565607136582230, -53.84900783228816579, 16.85000000000000142 ) ) ;
#25462 = ORIENTED_EDGE ( 'NONE', *, *, #2799, .T. ) ;
#25463 = CARTESIAN_POINT ( 'NONE',  ( -6.527821822757669423, -46.15177778084200355, -5.007725705170800623 ) ) ;
#25464 = EDGE_CURVE ( 'NONE', #19643, #45513, #10756, .T. ) ;
#25465 = CARTESIAN_POINT ( 'NONE',  ( 47.41560371684850139, 23.41602560681479872, -54.88584520135799494 ) ) ;
#25466 = CARTESIAN_POINT ( 'NONE',  ( 22.20417850065061671, 22.76024865223504889, -34.79644414665609986 ) ) ;
#25467 = CARTESIAN_POINT ( 'NONE',  ( 63.18115153217100755, 0.8966068345641580173, -62.26318953425310099 ) ) ;
#25468 = CARTESIAN_POINT ( 'NONE',  ( 60.85038404897530029, 14.22631097275989909, -47.01191575018489743 ) ) ;
#25469 = CARTESIAN_POINT ( 'NONE',  ( 43.27084646332170337, 12.63989574393310100, -5.051381114894940794 ) ) ;
#25470 = EDGE_CURVE ( 'NONE', #36729, #36007, #11607, .T. ) ;
#25471 = CARTESIAN_POINT ( 'NONE',  ( 16.13393739769620083, -15.61618894467929941, 4.450000000000000178 ) ) ;
#25472 = CARTESIAN_POINT ( 'NONE',  ( 53.18486760013709613, 18.24248981343010101, -48.80133335483809986 ) ) ;
#25473 = LINE ( 'NONE', #17641, #27503 ) ;
#25474 = CARTESIAN_POINT ( 'NONE',  ( 56.62774750731059470, -47.76694016067460069, -48.32660976114450335 ) ) ;
#25475 = CARTESIAN_POINT ( 'NONE',  ( 12.03708665661662636, -21.02749597990143116, -67.15911188335698512 ) ) ;
#25476 = AXIS2_PLACEMENT_3D ( 'NONE', #8191, #48539, #19964 ) ;
#25477 = CARTESIAN_POINT ( 'NONE',  ( 54.26151850782470376, 20.26306358825659970, -53.24447792474390440 ) ) ;
#25478 = B_SPLINE_CURVE_WITH_KNOTS ( 'NONE', 3,
 ( #27508, #36148, #47960, #7866, #15985, #35113, #28014, #20156, #40089, #3939, #12063, #47704, #47453, #48209, #19899, #27768, #43763, #47198, #15216, #35644, #250, #8123, #23814, #51115, #11286, #43510, #31939, #24327 ),
 .UNSPECIFIED., .F., .F.,
 ( 4, 2, 2, 2, 2, 2, 2, 2, 2, 2, 2, 2, 2, 4 ),
 ( 0.000000000000000000, 0.03124971541833476002, 0.06249943083666952004, 0.09374914625500427312, 0.1249988616733390401, 0.1562485770916738070, 0.1874982925100085462, 0.2187480079283433132, 0.2499977233466780802, 0.2812474387650128471, 0.3124971541833476141, 0.3749965850200170925, 0.4374960158566866264, 0.4999954466933561603 ),
 .UNSPECIFIED. ) ;
#25479 = CARTESIAN_POINT ( 'NONE',  ( 63.31978766800369840, 1.229084191802120030, -69.04069905742069579 ) ) ;
#25480 = DIRECTION ( 'NONE',  ( 1.000000000000000000, 0.000000000000000000, 0.000000000000000000 ) ) ;
#25481 = CARTESIAN_POINT ( 'NONE',  ( 22.56376508447987561, -18.32376100367250515, -60.97451088762495885 ) ) ;
#25482 = EDGE_LOOP ( 'NONE', ( #50788, #21478, #44360, #28255 ) ) ;
#25483 = CARTESIAN_POINT ( 'NONE',  ( 14.13393739769619906, -31.61618894467930474, -34.64999999999999858 ) ) ;
#25484 = CARTESIAN_POINT ( 'NONE',  ( 9.293570193019839110, 32.02070994195079834, -46.52994104399439834 ) ) ;
#25485 = CARTESIAN_POINT ( 'NONE',  ( 45.93002705875483827, 13.88381105130597604, -7.538620839776520199 ) ) ;
#25486 = EDGE_CURVE ( 'NONE', #26724, #43577, #29399, .T. ) ;
#25487 = CARTESIAN_POINT ( 'NONE',  ( 68.03809913820030886, -32.00255854605169503, -18.68243752497800259 ) ) ;
#25488 = CARTESIAN_POINT ( 'NONE',  ( 17.99108685348040026, 20.53764257940400029, -75.58342519351550948 ) ) ;
#25489 = ORIENTED_EDGE ( 'NONE', *, *, #21980, .F. ) ;
#25490 = ORIENTED_EDGE ( 'NONE', *, *, #47734, .F. ) ;
#25491 = PLANE ( 'NONE',  #39591 ) ;
#25492 = AXIS2_PLACEMENT_3D ( 'NONE', #30236, #25520, #37586 ) ;
#25493 = ORIENTED_EDGE ( 'NONE', *, *, #44254, .T. ) ;
#25494 = EDGE_CURVE ( 'NONE', #16045, #31153, #11843, .T. ) ;
#25495 = CARTESIAN_POINT ( 'NONE',  ( 10.66704074881489994, -63.38769094126030268, -45.39606956719949693 ) ) ;
#25496 = CARTESIAN_POINT ( 'NONE',  ( 57.00815868861789681, -45.37048793376839484, -25.89347327989339931 ) ) ;
#25497 = CARTESIAN_POINT ( 'NONE',  ( 24.04483537888494382, -15.65978551039709110, -77.50942050008035267 ) ) ;
#25498 = CARTESIAN_POINT ( 'NONE',  ( 61.48519961305099457, 14.00861713270729858, -47.04493765378530412 ) ) ;
#25499 = CARTESIAN_POINT ( 'NONE',  ( 63.72368862820488999, 1.434949534324519993, -62.02708488646099738 ) ) ;
#25500 = ORIENTED_EDGE ( 'NONE', *, *, #35622, .F. ) ;
#25501 = CARTESIAN_POINT ( 'NONE',  ( 45.95394279055306441, 6.916571454256072116, -60.54993553558288255 ) ) ;
#25502 = ORIENTED_EDGE ( 'NONE', *, *, #33851, .F. ) ;
#25503 = CARTESIAN_POINT ( 'NONE',  ( 54.56301516078890046, -45.21020833436829633, -14.51131706652730102 ) ) ;
#25504 = DIRECTION ( 'NONE',  ( 0.000000000000000000, 0.000000000000000000, -1.000000000000000000 ) ) ;
#25505 = CARTESIAN_POINT ( 'NONE',  ( 9.824348392058000812, -18.68523042451224114, -49.70282426501482576 ) ) ;
#25506 = ORIENTED_EDGE ( 'NONE', *, *, #43822, .F. ) ;
#25507 = CARTESIAN_POINT ( 'NONE',  ( 73.02919596257699197, 0.9065823421260940096, -69.11945805671248877 ) ) ;
#25508 = CARTESIAN_POINT ( 'NONE',  ( 47.02944151445359466, -54.40995658191120299, -75.36157798374209449 ) ) ;
#25509 = CARTESIAN_POINT ( 'NONE',  ( 61.30950358004140099, 14.36220717851900019, -47.67188667985269745 ) ) ;
#25510 = EDGE_CURVE ( 'NONE', #41523, #8412, #12657, .T. ) ;
#25511 = CARTESIAN_POINT ( 'NONE',  ( 50.30650830823179120, 13.88381105525040127, -10.79667524648609955 ) ) ;
#25512 = AXIS2_PLACEMENT_3D ( 'NONE', #49460, #9615, #5431 ) ;
#25513 = DIRECTION ( 'NONE',  ( 1.000000000000000000, 0.000000000000000000, 0.000000000000000000 ) ) ;
#25514 = CARTESIAN_POINT ( 'NONE',  ( -18.86606260230390220, 24.88381105532059934, 16.85000000000000142 ) ) ;
#25515 = CARTESIAN_POINT ( 'NONE',  ( 57.89943171185210247, 14.04932663211479849, -25.97857316395900185 ) ) ;
#25516 = CARTESIAN_POINT ( 'NONE',  ( 13.05426711372570026, -22.83438672010860060, -73.91587056106729392 ) ) ;
#25517 = B_SPLINE_SURFACE_WITH_KNOTS ( 'NONE', 3, 3, ( 
 ( #37148, #49472, #25582, #17488, #5697, #25835, #26102, #1246, #21650, #21910, #41077, #33961 ),
 ( #33195, #37655, #49214, #9382, #49977, #14069, #17740, #34217, #30031, #41329, #6213, #18248 ),
 ( #21400, #25060, #50238, #45009, #5190, #17234, #22942, #23449, #27146, #35534, #47345, #30296 ),
 ( #18769, #31065, #3054, #14584, #34740, #30550, #14844, #19024, #46314, #15103, #11442, #51005 ),
 ( #47091, #39473, #46574, #39209, #50493, #10662, #30806, #11180, #43149, #35000, #7245, #3574 ),
 ( #6471, #34488, #42895, #26619, #2535, #23192, #2796, #38961, #6990, #10404, #42634, #26356 ) ),
 .UNSPECIFIED., .F., .F., .F.,
 ( 4, 2, 4 ),
 ( 4, 1, 1, 1, 1, 1, 1, 1, 1, 4 ),
 ( -0.3078040425649150036, -0.2786161072492089885, 1.435456000000000037E-29 ),
 ( 0.000000000000000000, 0.1111111111111110078, 0.2222222222222219878, 0.3333333333333329818, 0.4444444444444439757, 0.5555555555555560243, 0.6666666666666670737, 0.7777777777777779011, 0.8888888888888889506, 1.000000000000000000 ),
 .UNSPECIFIED. ) ;
#25518 = ORIENTED_EDGE ( 'NONE', *, *, #19976, .F. ) ;
#25519 = VECTOR ( 'NONE', #22937, 1000.000000000000000 ) ;
#25520 = DIRECTION ( 'NONE',  ( 0.000000000000000000, 1.000000000000000000, 0.000000000000000000 ) ) ;
#25521 = CIRCLE ( 'NONE', #30538, 18.50000000000000000 ) ;
#25522 = DIRECTION ( 'NONE',  ( 0.000000000000000000, 0.000000000000000000, -1.000000000000000000 ) ) ;
#25523 = DIRECTION ( 'NONE',  ( -1.000000000000000000, 0.000000000000000000, 0.000000000000000000 ) ) ;
#25524 = CARTESIAN_POINT ( 'NONE',  ( 72.90864092247801409, 1.230946250268279973, -69.10734940427019524 ) ) ;
#25525 = EDGE_CURVE ( 'NONE', #8290, #5276, #28593, .T. ) ;
#25526 = B_SPLINE_CURVE_WITH_KNOTS ( 'NONE', 3,
 ( #8893, #33235, #24580, #12566, #25366, #37438, #36389, #32700, #44528, #497, #13347, #32969, #25102, #41114, #21439, #16485, #24844, #5227 ),
 .UNSPECIFIED., .F., .F.,
 ( 4, 2, 2, 2, 2, 2, 2, 2, 4 ),
 ( 0.5000000030890958680, 0.5625000027029588567, 0.6250000023168218455, 0.6875000019306849453, 0.7500000015445479340, 0.8125000011584109227, 0.8750000007722740225, 0.9375000003861370113, 1.000000000000000000 ),
 .UNSPECIFIED. ) ;
#25527 = DIRECTION ( 'NONE',  ( 1.000000000000000000, 0.000000000000000000, 0.000000000000000000 ) ) ;
#25528 = CARTESIAN_POINT ( 'NONE',  ( 21.57906565130501875, -9.858451563110987692, -65.24878181863623183 ) ) ;
#25529 = EDGE_CURVE ( 'NONE', #10190, #40528, #40403, .T. ) ;
#25530 = CARTESIAN_POINT ( 'NONE',  ( 17.16940787898279197, -7.705177864455698966, -59.33404506873640827 ) ) ;
#25531 = CARTESIAN_POINT ( 'NONE',  ( 48.94088206813629682, -53.97935211052140403, -55.17481584361439673 ) ) ;
#25532 = CARTESIAN_POINT ( 'NONE',  ( 9.807679542830243236, -20.47774811832251629, -56.58400988324318348 ) ) ;
#25533 = CARTESIAN_POINT ( 'NONE',  ( 76.85544920018013215, -43.13137431541007061, -14.75910591941364380 ) ) ;
#25534 = FACE_OUTER_BOUND ( 'NONE', #20328, .T. ) ;
#25535 = VERTEX_POINT ( 'NONE', #24651 ) ;
#25536 = CARTESIAN_POINT ( 'NONE',  ( 21.44577556945500163, -20.84027446995419908, -39.31469157680550097 ) ) ;
#25537 = CARTESIAN_POINT ( 'NONE',  ( 64.14653846951229355, 1.039769764133499974, -61.16551630736319822 ) ) ;
#25538 = ORIENTED_EDGE ( 'NONE', *, *, #48697, .T. ) ;
#25539 = CARTESIAN_POINT ( 'NONE',  ( 9.402977987163499307, -14.22576715605993769, -33.91259203128302602 ) ) ;
#25540 = CARTESIAN_POINT ( 'NONE',  ( 60.52868080801660255, -45.70706635237720405, -47.56219373738379375 ) ) ;
#25541 = DIRECTION ( 'NONE',  ( -1.000000000000000000, 0.000000000000000000, 0.000000000000000000 ) ) ;
#25542 = CARTESIAN_POINT ( 'NONE',  ( 50.23538082579219832, 18.53774256725959901, -76.14999999999999147 ) ) ;
#25544 = CARTESIAN_POINT ( 'NONE',  ( 22.90090927591486292, -15.61618926791037687, -70.45281771081829447 ) ) ;
#25543 = CARTESIAN_POINT ( 'NONE',  ( 43.97715045787865762, 8.720472785296667695, -66.77010945423391775 ) ) ;
#25545 = DIRECTION ( 'NONE',  ( 1.000000000000000000, 0.000000000000000000, 0.000000000000000000 ) ) ;
#25546 = DIRECTION ( 'NONE',  ( 0.000000000000000000, 0.000000000000000000, 1.000000000000000000 ) ) ;
#25547 = ORIENTED_EDGE ( 'NONE', *, *, #40612, .F. ) ;
#25548 = AXIS2_PLACEMENT_3D ( 'NONE', #31439, #28284, #47468 ) ;
#25549 = ORIENTED_EDGE ( 'NONE', *, *, #17863, .T. ) ;
#25550 = EDGE_LOOP ( 'NONE', ( #49505, #39383, #18321, #36524 ) ) ;
#25551 = ORIENTED_EDGE ( 'NONE', *, *, #10432, .T. ) ;
#25552 = CARTESIAN_POINT ( 'NONE',  ( 61.34009987415589649, -45.20348205694470067, -46.37197372483269930 ) ) ;
#25553 = DIRECTION ( 'NONE',  ( 1.000000000000000000, 0.000000000000000000, 0.000000000000000000 ) ) ;
#25554 = AXIS2_PLACEMENT_3D ( 'NONE', #6736, #51525, #47598 ) ;
#25555 = CARTESIAN_POINT ( 'NONE',  ( 54.86738137264109838, -51.34065982945939766, -53.37025816224030450 ) ) ;
#25556 = ORIENTED_EDGE ( 'NONE', *, *, #41356, .F. ) ;
#25557 = ORIENTED_EDGE ( 'NONE', *, *, #4300, .T. ) ;
#25558 = CIRCLE ( 'NONE', #32243, 5.999999999999998224 ) ;
#25559 = CARTESIAN_POINT ( 'NONE',  ( 9.366916810851629194, -16.50183646529157144, -73.41114475139522710 ) ) ;
#25560 = CARTESIAN_POINT ( 'NONE',  ( 50.51702630346309775, -53.30999449162459314, -54.91376886094779763 ) ) ;
#25561 = CARTESIAN_POINT ( 'NONE',  ( 16.13393739769620083, -15.61618894467929941, -35.14999999999999858 ) ) ;
#25562 = ORIENTED_EDGE ( 'NONE', *, *, #19927, .T. ) ;
#25563 = DIRECTION ( 'NONE',  ( 0.000000000000000000, 0.000000000000000000, 1.000000000000000000 ) ) ;
#25564 = CARTESIAN_POINT ( 'NONE',  ( 52.30043102847849923, -50.70004990181330129, -76.35983844118280217 ) ) ;
#25565 = DIRECTION ( 'NONE',  ( -0.3294064756440929220, 0.9441882088883218893, 0.000000000000000000 ) ) ;
#25566 = EDGE_CURVE ( 'NONE', #16548, #32624, #40075, .T. ) ;
#25567 = CARTESIAN_POINT ( 'NONE',  ( 8.463963385727261368, -13.95539207350469901, -63.08037089589139867 ) ) ;
#25568 = ADVANCED_FACE ( 'NONE', ( #21245 ), #29878, .T. ) ;
#25569 = CARTESIAN_POINT ( 'NONE',  ( 22.14946380439831941, -18.71488146266838370, -32.99858898373786076 ) ) ;
#25570 = CARTESIAN_POINT ( 'NONE',  ( 41.58741077758180182, 13.58021230090170128, -5.496105773154369878 ) ) ;
#25571 = CARTESIAN_POINT ( 'NONE',  ( 41.99652581331089607, -44.42478526866589306, -5.118462684484269332 ) ) ;
#25572 = EDGE_CURVE ( 'NONE', #29653, #20020, #9731, .T. ) ;
#25573 = CARTESIAN_POINT ( 'NONE',  ( 68.13393739769840352, -50.61618894467879670, -73.25000000000220268 ) ) ;
#25574 = CYLINDRICAL_SURFACE ( 'NONE', #24842, 7.910999999999997812 ) ;
#25575 = CARTESIAN_POINT ( 'NONE',  ( 63.65729443213299987, 1.185469602160369895, -69.60194394625881387 ) ) ;
#25576 = CIRCLE ( 'NONE', #20558, 0.4934525379635912867 ) ;
#25577 = CARTESIAN_POINT ( 'NONE',  ( 47.08272461591150204, 8.115112359209708970, -53.89515469992119989 ) ) ;
#25578 = CARTESIAN_POINT ( 'NONE',  ( 66.50410218238459947, 1.883581543589160079, -20.28081949647409843 ) ) ;
#25579 = ORIENTED_EDGE ( 'NONE', *, *, #36468, .F. ) ;
#25580 = VECTOR ( 'NONE', #17492, 999.9999999999998863 ) ;
#25581 = CARTESIAN_POINT ( 'NONE',  ( 14.74689323179859990, -52.86909850055779714, -76.12391999848780699 ) ) ;
#25582 = CARTESIAN_POINT ( 'NONE',  ( 57.35071420090630312, 19.00220926952300005, -52.74072019877679907 ) ) ;
#25583 = CARTESIAN_POINT ( 'NONE',  ( -19.37574330875981232, -50.24588423573533902, 16.21999999999999886 ) ) ;
#25584 = CARTESIAN_POINT ( 'NONE',  ( 46.98749078828947034, -36.11618894467930119, -34.79644660940672907 ) ) ;
#25585 = CARTESIAN_POINT ( 'NONE',  ( 23.22693331446999920, -14.39611290704790036, -32.14999999999999858 ) ) ;
#25586 = DIRECTION ( 'NONE',  ( 0.8660254037844380415, -0.5000000000000012212, -2.498001805406606160E-16 ) ) ;
#25587 = EDGE_CURVE ( 'NONE', #36317, #51255, #5098, .T. ) ;
#25588 = CARTESIAN_POINT ( 'NONE',  ( 8.038038740883386879, -60.26370295294966439, -21.05410134318717041 ) ) ;
#25589 = CARTESIAN_POINT ( 'NONE',  ( 19.60264381368218878, -8.482739570013125174, -45.15181677121430681 ) ) ;
#25590 = CARTESIAN_POINT ( 'NONE',  ( 56.48240791863720744, 19.53654756573429907, -53.80987478700529891 ) ) ;
#25591 = CARTESIAN_POINT ( 'NONE',  ( 48.03280260593719930, 23.13580117559470040, -55.25606283016369957 ) ) ;
#25592 = ORIENTED_EDGE ( 'NONE', *, *, #627, .F. ) ;
#25593 = CARTESIAN_POINT ( 'NONE',  ( 23.00352250046740110, -17.21348656573650260, -64.91990020089450297 ) ) ;
#25594 = ORIENTED_EDGE ( 'NONE', *, *, #28778, .T. ) ;
#25595 = CONICAL_SURFACE ( 'NONE', #13077, 14.87302494707580180, 1.249045772398249987 ) ;
#25596 = DIRECTION ( 'NONE',  ( 0.5951849179585205762, 0.4324271549242467705, 0.6773194734531339245 ) ) ;
#25597 = CARTESIAN_POINT ( 'NONE',  ( 57.24929578232330130, -50.61618894764249887, -53.91492796143979405 ) ) ;
#25599 = CARTESIAN_POINT ( 'NONE',  ( 52.61984545813539427, 18.57124442378099971, -27.71374801268460075 ) ) ;
#25598 = CARTESIAN_POINT ( 'NONE',  ( 84.40405423732200063, 12.27453954208750098, -47.38850513265820297 ) ) ;
#25600 = CARTESIAN_POINT ( 'NONE',  ( 11.42992024409580054, -10.36121213071920089, -75.72041208499069853 ) ) ;
#25601 = CYLINDRICAL_SURFACE ( 'NONE', #47720, 6.766999999999998572 ) ;
#25602 = CARTESIAN_POINT ( 'NONE',  ( 56.59132469845479818, -45.11618894467940066, -15.49288788266510153 ) ) ;
#25603 = CARTESIAN_POINT ( 'NONE',  ( 16.13393739769620083, -15.61618894467929941, -6.189999999999999503 ) ) ;
#25604 = DIRECTION ( 'NONE',  ( 0.000000000000000000, 0.000000000000000000, -1.000000000000000000 ) ) ;
#25605 = VECTOR ( 'NONE', #22259, 1000.000000000000000 ) ;
#25606 = VERTEX_POINT ( 'NONE', #12902 ) ;
#25607 = ORIENTED_EDGE ( 'NONE', *, *, #22888, .T. ) ;
#25608 = CARTESIAN_POINT ( 'NONE',  ( 12.10371154477140010, -65.18136423378868471, -16.68259577209380140 ) ) ;
#25609 = CARTESIAN_POINT ( 'NONE',  ( 12.11391230005439823, 34.07748982303999696, -46.92647627143619360 ) ) ;
#25610 = DIRECTION ( 'NONE',  ( 0.000000000000000000, -1.000000000000000000, 0.000000000000000000 ) ) ;
#25611 = CARTESIAN_POINT ( 'NONE',  ( 3.133937397696200389, -15.61618894467929763, -6.189999999999999503 ) ) ;
#25612 = B_SPLINE_CURVE_WITH_KNOTS ( 'NONE', 3,
 ( #15433, #7569, #11244, #7057, #31384, #36107, #35852, #23260, #23008, #3123 ),
 .UNSPECIFIED., .F., .F.,
 ( 4, 2, 2, 2, 4 ),
 ( 0.000000000000000000, 0.1775000000004226253, 0.3375000000003006706, 0.4375000000002248757, 0.5000003605123823913 ),
 .UNSPECIFIED. ) ;
#25613 = DIRECTION ( 'NONE',  ( 0.9200120562340469155, -0.3918900565005459247, 0.000000000000000000 ) ) ;
#25614 = TOROIDAL_SURFACE ( 'NONE', #6418, 12.50000000000000000, 1.000000000000000000 ) ;
#25615 = VERTEX_POINT ( 'NONE', #9985 ) ;
#25616 = CARTESIAN_POINT ( 'NONE',  ( -13.76961861560299916, -41.00297359184299495, -46.76611145355789745 ) ) ;
#25617 = AXIS2_PLACEMENT_3D ( 'NONE', #41759, #3489, #43065 ) ;
#25618 = CARTESIAN_POINT ( 'NONE',  ( 54.63655771189059607, 16.82059223505549994, -26.73578643762699869 ) ) ;
#25619 = CARTESIAN_POINT ( 'NONE',  ( 53.26167791221869408, -49.50159509410539727, -49.13884078695329549 ) ) ;
#25620 = CARTESIAN_POINT ( 'NONE',  ( 51.50035696899490034, 19.75281252459599912, -50.15572549081029052 ) ) ;
#25621 = CARTESIAN_POINT ( 'NONE',  ( 59.83128115804950653, -2.247120905410399772, -15.76168587106839958 ) ) ;
#25622 = CARTESIAN_POINT ( 'NONE',  ( 51.01140995548900037, -49.48507500592920394, -76.32135044086720654 ) ) ;
#25623 = DIRECTION ( 'NONE',  ( 0.000000000000000000, -1.000000000000000000, 0.000000000000000000 ) ) ;
#25624 = ORIENTED_EDGE ( 'NONE', *, *, #45984, .T. ) ;
#25625 = CARTESIAN_POINT ( 'NONE',  ( 22.90111010729205177, -15.61618905465553553, -68.45282213299155671 ) ) ;
#25626 = DIRECTION ( 'NONE',  ( -0.5951849179585204652, -0.4324271549242469925, 0.6773194734531338135 ) ) ;
#25627 = ORIENTED_EDGE ( 'NONE', *, *, #4317, .T. ) ;
#25628 = CARTESIAN_POINT ( 'NONE',  ( 23.04647745593273811, -11.63208902550109336, -57.34100099693699093 ) ) ;
#25629 = DIRECTION ( 'NONE',  ( -0.8660254037844379305, 0.5000000000000011102, -1.387778780781449373E-16 ) ) ;
#25630 = CARTESIAN_POINT ( 'NONE',  ( 22.85730003971410085, -19.66369351922019959, -32.18498778107969116 ) ) ;
#25631 = EDGE_CURVE ( 'NONE', #47003, #10013, #50337, .T. ) ;
#25632 = CARTESIAN_POINT ( 'NONE',  ( 13.99297327411639991, -51.17866263145759831, -22.74640880580200175 ) ) ;
#25633 = CARTESIAN_POINT ( 'NONE',  ( 54.34362824239659773, 19.58923895723300035, -75.97910198928759939 ) ) ;
#25634 = CARTESIAN_POINT ( 'NONE',  ( 46.87137491217979601, -53.55967532393449915, -75.98463753095340678 ) ) ;
#25635 = ORIENTED_EDGE ( 'NONE', *, *, #33157, .F. ) ;
#25636 = ADVANCED_FACE ( 'NONE', ( #45117 ), #49831, .F. ) ;
#25637 = CARTESIAN_POINT ( 'NONE',  ( 56.26232872805620389, 14.29808925844480072, -17.58200819105400114 ) ) ;
#25638 = CARTESIAN_POINT ( 'NONE',  ( 20.29259217163623319, -10.20485708858880436, -78.16115132716946334 ) ) ;
#25639 =( BOUNDED_CURVE ( )  B_SPLINE_CURVE ( 3, ( #18617, #50600, #26728, #5800 ),
 .UNSPECIFIED., .F., .T. ) 
 B_SPLINE_CURVE_WITH_KNOTS ( ( 4, 4 ),
 ( 4.712388980384694115, 5.070260775219138871 ),
 .UNSPECIFIED. ) 
 CURVE ( )  GEOMETRIC_REPRESENTATION_ITEM ( )  RATIONAL_B_SPLINE_CURVE ( ( 1.000000000000000000, 0.9893557610490356646, 0.9893557610490356646, 1.000000000000000000 ) ) 
 REPRESENTATION_ITEM ( '' )  );
#25640 = CARTESIAN_POINT ( 'NONE',  ( 57.35094531453579947, -50.23772356244409565, -52.73804475687759918 ) ) ;
#25641 = AXIS2_PLACEMENT_3D ( 'NONE', #38650, #10347, #34947 ) ;
#25642 = CARTESIAN_POINT ( 'NONE',  ( 18.62387150434389937, -22.21488518936680023, -33.23232777544669148 ) ) ;
#25643 = CARTESIAN_POINT ( 'NONE',  ( 66.53393739769619231, 11.23736444591397543, -69.70355339059327093 ) ) ;
#25644 = B_SPLINE_CURVE_WITH_KNOTS ( 'NONE', 3,
 ( #22373, #22113, #31011, #10085 ),
 .UNSPECIFIED., .F., .F.,
 ( 4, 4 ),
 ( 3.898674657257720000, 4.021955696373110456 ),
 .UNSPECIFIED. ) ;
#25645 = VERTEX_POINT ( 'NONE', #5801 ) ;
#25646 = CARTESIAN_POINT ( 'NONE',  ( 47.42191000389319555, 23.38128243525070360, -74.50100479479878857 ) ) ;
#25647 = CARTESIAN_POINT ( 'NONE',  ( 65.01767771978660448, 0.8838110553206759423, -60.52272727272730179 ) ) ;
#25648 = CARTESIAN_POINT ( 'NONE',  ( 75.16212372845173206, -29.54155010626721634, -11.85658773837712054 ) ) ;
#25649 = CARTESIAN_POINT ( 'NONE',  ( 31.58225770014180256, -2.032350560840031406, -102.2016796975540274 ) ) ;
#25650 = DIRECTION ( 'NONE',  ( 0.2771081164311157696, -0.6505467637364703570, -0.7071067811865504593 ) ) ;
#25651 = CARTESIAN_POINT ( 'NONE',  ( 17.72982031756377808, -49.61616882370213943, -83.18296600389349749 ) ) ;
#25652 = EDGE_CURVE ( 'NONE', #14404, #39471, #17594, .T. ) ;
#25653 = AXIS2_PLACEMENT_3D ( 'NONE', #33057, #40420, #28351 ) ;
#25654 = LINE ( 'NONE', #40623, #39478 ) ;
#25656 = CARTESIAN_POINT ( 'NONE',  ( 47.18678629383617107, -39.34334098796522738, -54.67089428642063353 ) ) ;
#25655 = DIRECTION ( 'NONE',  ( 0.000000000000000000, 0.000000000000000000, 1.000000000000000000 ) ) ;
#25657 = ADVANCED_FACE ( 'NONE', ( #49062 ), #29119, .T. ) ;
#25658 = CARTESIAN_POINT ( 'NONE',  ( 61.14427338081150509, 14.07233411761519903, -46.75185522880649813 ) ) ;
#25659 = CARTESIAN_POINT ( 'NONE',  ( -33.14628496358510290, -5.854866907655339681, -57.60188784292080300 ) ) ;
#25660 = ORIENTED_EDGE ( 'NONE', *, *, #10048, .T. ) ;
#25661 = CARTESIAN_POINT ( 'NONE',  ( 52.76045300953009587, -49.70056559441360378, -48.50241422118810419 ) ) ;
#25662 = ORIENTED_EDGE ( 'NONE', *, *, #23960, .T. ) ;
#25663 = CARTESIAN_POINT ( 'NONE',  ( 57.75416591588980708, -45.11614852472010284, -25.44313242021300070 ) ) ;
#25664 = DIRECTION ( 'NONE',  ( 0.000000000000000000, -1.000000000000000000, 0.000000000000000000 ) ) ;
#25665 = CARTESIAN_POINT ( 'NONE',  ( 13.61473149145860084, 19.77355128491650049, -21.87339239449909911 ) ) ;
#25666 = CARTESIAN_POINT ( 'NONE',  ( 56.52876338304670156, 14.13686770687309924, -25.36325227249279735 ) ) ;
#25667 = CARTESIAN_POINT ( 'NONE',  ( 17.03912355353180175, -8.621677044631578468, -47.99378621272389722 ) ) ;
#25668 = CARTESIAN_POINT ( 'NONE',  ( 28.81656660489900190, -26.62211590400339745, -34.68308842254609914 ) ) ;
#25669 = CARTESIAN_POINT ( 'NONE',  ( 52.83705229977910278, 18.43325409324560127, -48.81125896478140191 ) ) ;
#25670 = CARTESIAN_POINT ( 'NONE',  ( 47.13393739769619373, 4.883811055320659733, -54.64999999999999858 ) ) ;
#25671 = CARTESIAN_POINT ( 'NONE',  ( 60.32392629779650406, -45.73451482830140691, -47.22595585683189512 ) ) ;
#25672 = CARTESIAN_POINT ( 'NONE',  ( 64.81322693590129802, -44.32916768243990191, -10.69846699143639945 ) ) ;
#25673 = ORIENTED_EDGE ( 'NONE', *, *, #41564, .T. ) ;
#25674 = CARTESIAN_POINT ( 'NONE',  ( 13.21023430151019973, -22.46882745431149786, -73.69570765841629623 ) ) ;
#25675 = CARTESIAN_POINT ( 'NONE',  ( 73.06808687136680192, 1.187415670095769871, -68.89659930051639947 ) ) ;
#25676 = CARTESIAN_POINT ( 'NONE',  ( 47.39616816378460129, -54.65991725903980125, -54.86393396055039773 ) ) ;
#25677 = CARTESIAN_POINT ( 'NONE',  ( 8.222915784689270424, -14.75862311762373835, -48.82684667488993568 ) ) ;
#25678 = CARTESIAN_POINT ( 'NONE',  ( 73.13041444294920268, 0.8910129994591549085, -62.32805707658469885 ) ) ;
#25679 = CARTESIAN_POINT ( 'NONE',  ( 10.91841378337480073, -65.04619103187860674, -17.66395372721920154 ) ) ;
#25680 = CARTESIAN_POINT ( 'NONE',  ( 71.54590618381259048, 1.188860127980290171, -60.81548205241750082 ) ) ;
#25681 = CARTESIAN_POINT ( 'NONE',  ( 8.222926011208455677, -16.64759936946806462, -76.75081796745894280 ) ) ;
#25682 = CARTESIAN_POINT ( 'NONE',  ( 24.04485091158800003, -15.61618876680915236, -45.79233931912149558 ) ) ;
#25683 = AXIS2_PLACEMENT_3D ( 'NONE', #853, #49350, #21276 ) ;
#25684 = CARTESIAN_POINT ( 'NONE',  ( 8.222919918104569348, -16.64776285459041816, -46.46616330941802175 ) ) ;
#25685 = CARTESIAN_POINT ( 'NONE',  ( 65.05904174327520195, 1.369885150286800135, -70.38694600888931063 ) ) ;
#25686 = VERTEX_POINT ( 'NONE', #29378 ) ;
#25687 = CARTESIAN_POINT ( 'NONE',  ( 8.802047646820330584, -63.20618355599279425, -46.67014429624759941 ) ) ;
#25688 = CARTESIAN_POINT ( 'NONE',  ( 8.428863955492316151, -13.54541270948961262, -46.87566500811402648 ) ) ;
#25689 = ORIENTED_EDGE ( 'NONE', *, *, #26077, .F. ) ;
#25690 = CARTESIAN_POINT ( 'NONE',  ( 33.13393739769620083, -38.61618894467930119, -84.65000000000000568 ) ) ;
#25691 = CARTESIAN_POINT ( 'NONE',  ( 23.06214062797170072, -27.61618894467930119, -32.14999999999999858 ) ) ;
#25692 = CARTESIAN_POINT ( 'NONE',  ( 9.807834611244294010, -20.47794709156341852, -70.29933580689034045 ) ) ;
#25693 = CARTESIAN_POINT ( 'NONE',  ( 53.29069657418769879, 19.80760425434010230, -75.99878262601679069 ) ) ;
#25694 = ORIENTED_EDGE ( 'NONE', *, *, #33968, .F. ) ;
#25695 = CARTESIAN_POINT ( 'NONE',  ( 61.31807987947320271, 14.40950277385760003, -47.72348187476750070 ) ) ;
#25696 = DIRECTION ( 'NONE',  ( 0.000000000000000000, -1.000000000000000000, 0.000000000000000000 ) ) ;
#25697 = AXIS2_PLACEMENT_3D ( 'NONE', #8469, #48299, #25203 ) ;
#25698 = CARTESIAN_POINT ( 'NONE',  ( 16.82787181412869870, -23.83209882013590075, -58.26550999155039534 ) ) ;
#25699 = EDGE_CURVE ( 'NONE', #9424, #44314, #41184, .T. ) ;
#25700 = CARTESIAN_POINT ( 'NONE',  ( 22.89230595604955099, -15.24705981027367052, -56.43546068824361583 ) ) ;
#25701 = CARTESIAN_POINT ( 'NONE',  ( 45.63740510567983932, -38.11460057359725795, -62.13264583676811981 ) ) ;
#25702 = ORIENTED_EDGE ( 'NONE', *, *, #23955, .T. ) ;
#25703 = CARTESIAN_POINT ( 'NONE',  ( 57.25349264864389909, -45.82938052622620262, -26.26171515177349747 ) ) ;
#25704 = CARTESIAN_POINT ( 'NONE',  ( 11.45349785648839891, -9.819622762339609068, -49.51643979347259261 ) ) ;
#25705 = CARTESIAN_POINT ( 'NONE',  ( 52.66149646884399971, -49.78765645775949622, -48.73888008360700042 ) ) ;
#25706 = CARTESIAN_POINT ( 'NONE',  ( 8.988681696069670934, -17.72250670475619927, -32.14999999999999858 ) ) ;
#25707 = CARTESIAN_POINT ( 'NONE',  ( 14.04989515242449905, 20.46947493835569887, -75.41867332334470575 ) ) ;
#25708 = DIRECTION ( 'NONE',  ( 0.000000000000000000, -1.000000000000000000, 0.000000000000000000 ) ) ;
#25709 = CARTESIAN_POINT ( 'NONE',  ( 41.50830747127400144, -45.30505886361360268, -6.113803590135650445 ) ) ;
#25710 = LINE ( 'NONE', #6342, #20590 ) ;
#25711 = CARTESIAN_POINT ( 'NONE',  ( 8.132716167238188021, -17.60696254563019991, -52.43004635228650301 ) ) ;
#25712 = ORIENTED_EDGE ( 'NONE', *, *, #22925, .F. ) ;
#25713 = CARTESIAN_POINT ( 'NONE',  ( 52.69755715977279920, -49.73393510400349982, -27.86573118051390097 ) ) ;
#25714 = CARTESIAN_POINT ( 'NONE',  ( 16.50880182598979573, -51.11266520550329773, -20.14980157100569969 ) ) ;
#25716 = CARTESIAN_POINT ( 'NONE',  ( 46.63499162694400724, -39.11122816143360126, -34.64999999999999858 ) ) ;
#25715 = CARTESIAN_POINT ( 'NONE',  ( 11.23966493344340023, 33.90699900300699454, -17.15436069251279605 ) ) ;
#25718 = EDGE_CURVE ( 'NONE', #39379, #39152, #10099, .T. ) ;
#25717 = CARTESIAN_POINT ( 'NONE',  ( 15.24135970174500088, -8.620056853935023966, -70.30678751322059838 ) ) ;
#25719 = CARTESIAN_POINT ( 'NONE',  ( 47.38131247932619772, 14.91674438995409879, -10.59906179801200032 ) ) ;
#25720 = ORIENTED_EDGE ( 'NONE', *, *, #15322, .F. ) ;
#25721 = CARTESIAN_POINT ( 'NONE',  ( -10.88827818861070185, -42.34077264742860081, -6.211465758528559533 ) ) ;
#25722 = CARTESIAN_POINT ( 'NONE',  ( 47.62712401335679857, 23.26915926184220140, -54.68830161141420376 ) ) ;
#25723 = AXIS2_PLACEMENT_3D ( 'NONE', #29843, #6023, #37217 ) ;
#25724 = CARTESIAN_POINT ( 'NONE',  ( 56.46551779669420057, -50.77616595281960343, -53.85225392423020452 ) ) ;
#25725 = CARTESIAN_POINT ( 'NONE',  ( 63.24043675930629860, 1.099344084866029858, -62.24193811877859162 ) ) ;
#25726 = CARTESIAN_POINT ( 'NONE',  ( 60.86520825975330240, 14.21854415338730071, -47.04175779766590182 ) ) ;
#25727 = CARTESIAN_POINT ( 'NONE',  ( 42.80890084553470132, 12.86785355579670131, -5.063862466711140264 ) ) ;
#25728 = CARTESIAN_POINT ( 'NONE',  ( 52.15298324570800048, 18.44951579869039904, -77.15976990859368811 ) ) ;
#25729 = CARTESIAN_POINT ( 'NONE',  ( 52.87578304523380268, 18.40442787170260175, -48.67531064471670277 ) ) ;
#25730 = CARTESIAN_POINT ( 'NONE',  ( 18.68073206901139471, 24.30204422277620324, -76.07915437898316213 ) ) ;
#25731 = CARTESIAN_POINT ( 'NONE',  ( 60.34543612929479650, -45.86997884962860184, -47.73174601672569395 ) ) ;
#25732 = CARTESIAN_POINT ( 'NONE',  ( 19.65243233025719860, -21.45234396756585582, -66.78026749941459173 ) ) ;
#25733 = VECTOR ( 'NONE', #7518, 1000.000000000000000 ) ;
#25734 = CARTESIAN_POINT ( 'NONE',  ( 52.23074715003530599, 21.34763686467589849, -54.40819828980639983 ) ) ;
#25735 = CARTESIAN_POINT ( 'NONE',  ( 63.78870119449619835, 1.432915709213359978, -69.43629025642729857 ) ) ;
#25736 = CARTESIAN_POINT ( 'NONE',  ( 63.88393739769619373, 4.883811055320659733, -61.34712802272770915 ) ) ;
#25737 = CARTESIAN_POINT ( 'NONE',  ( -11.36606260230380094, -15.61618894467929941, -54.64999999999999858 ) ) ;
#25738 = ORIENTED_EDGE ( 'NONE', *, *, #328, .T. ) ;
#25739 = DIRECTION ( 'NONE',  ( 0.000000000000000000, 0.000000000000000000, -1.000000000000000000 ) ) ;
#25740 = CARTESIAN_POINT ( 'NONE',  ( 10.77396489004810043, 32.13674430547519734, -45.20697498780340595 ) ) ;
#25741 = FACE_OUTER_BOUND ( 'NONE', #12101, .T. ) ;
#25742 = CARTESIAN_POINT ( 'NONE',  ( 65.61159321741499184, -31.73702401370160331, -17.31747073895240163 ) ) ;
#25743 = CARTESIAN_POINT ( 'NONE',  ( 18.12954445334329989, 19.89798265472740013, -74.14993923597710079 ) ) ;
#25744 = VERTEX_POINT ( 'NONE', #1606 ) ;
#25745 = ORIENTED_EDGE ( 'NONE', *, *, #26755, .F. ) ;
#25746 = CARTESIAN_POINT ( 'NONE',  ( 49.48559182206740559, 22.51696836342139818, -55.18124709514480486 ) ) ;
#25747 = ORIENTED_EDGE ( 'NONE', *, *, #35434, .F. ) ;
#25748 = CARTESIAN_POINT ( 'NONE',  ( 12.56728399523450079, -65.44523288411160422, -46.96404464519110178 ) ) ;
#25749 = CARTESIAN_POINT ( 'NONE',  ( 56.44632044434209917, -46.23264868926420235, -26.25478470813849796 ) ) ;
#25750 = CARTESIAN_POINT ( 'NONE',  ( 76.21898748821377012, -48.61618894467930119, -83.94294850574455324 ) ) ;
#25751 = CARTESIAN_POINT ( 'NONE',  ( 9.124990099443129665, -48.86424491586210195, -35.14566363178129649 ) ) ;
#25752 = ORIENTED_EDGE ( 'NONE', *, *, #3853, .F. ) ;
#25753 = CARTESIAN_POINT ( 'NONE',  ( 45.42810023600526392, 6.859503157004126273, -63.17912806148366656 ) ) ;
#25754 = B_SPLINE_SURFACE_WITH_KNOTS ( 'NONE', 3, 3, ( 
 ( #24491, #4596, #23466, #32098, #43675, #46662, #16399, #48117, #28178 ),
 ( #40508, #31588, #44180, #24228, #19816, #40253, #20314, #35804, #28439 ),
 ( #30638, #50578, #42723, #41800, #49682, #21604, #45225, #13775, #44698 ),
 ( #29729, #17187, #13522, #41025, #1453, #5394, #28696, #45745, #25791 ),
 ( #21351, #33408, #28961, #25280, #1195, #9839, #33666, #37098, #37354 ),
 ( #37608, #5141, #32875, #934, #666, #44960, #45485, #41284, #49171 ),
 ( #13006, #1714, #9062, #17697, #49426, #48909, #13263, #25537, #17442 ),
 ( #12741, #8803, #20571, #24755, #29480, #9583, #41541, #36564, #5657 ),
 ( #4866, #25011, #29218, #9333, #16656, #32613, #48640, #40765, #20833 ),
 ( #21095, #36831, #16931, #33144, #34175, #50454, #46791, #46536, #5907 ),
 ( #38920, #26578, #42331, #42594, #15060, #42067, #14804, #26059, #6169 ),
 ( #22128, #14028, #50961, #10361, #31028, #38135, #10624, #10883, #37881 ),
 ( #47053, #6952, #21870, #18472, #50705, #6691, #18726, #1973, #34705 ),
 ( #46009, #6430, #10100, #2235, #2754, #17952, #49937, #29986, #27108 ),
 ( #22649, #30769, #26846, #22903, #42856, #18211, #50194, #46275, #14544 ),
 ( #11138, #3012, #33920, #18983, #14286, #34964, #26322, #38668, #30513 ),
 ( #30253, #22389, #38393, #2492, #34445, #27872, #24176, #11919, #27618 ),
 ( #361, #27361, #114, #11399, #43368, #43624, #43875, #7972, #31794 ),
 ( #36250, #40199, #19245, #47311, #3792, #23414, #15325, #7202, #31278 ),
 ( #43111, #23157, #39435, #39174, #3269, #35227, #4287, #23670, #23922 ) ),
 .UNSPECIFIED., .F., .F., .F.,
 ( 4, 2, 2, 2, 2, 2, 2, 2, 2, 4 ),
 ( 4, 1, 1, 1, 1, 1, 4 ),
 ( -1.826192301619919967, -1.664708266399350212, -1.413116924480830150, -1.141370188512450090, -0.9130961508099619817, -0.7989591319587170393, -0.6163399017967240434, -0.3681920442903470203, -0.1161770322012310036, 0.000000000000000000 ),
 ( 0.000000000000000000, 0.1666666666666670182, 0.3333333333333329818, 0.5000000000000000000, 0.6666666666666670737, 0.8333333333333330373, 1.000000000000000000 ),
 .UNSPECIFIED. ) ;
#25755 = ORIENTED_EDGE ( 'NONE', *, *, #20342, .T. ) ;
#25756 = CARTESIAN_POINT ( 'NONE',  ( 49.15516447654730570, -45.57934867088179942, -11.33945784234580145 ) ) ;
#25757 = EDGE_CURVE ( 'NONE', #43986, #1848, #26030, .T. ) ;
#25758 = CARTESIAN_POINT ( 'NONE',  ( 24.01797834635617335, -16.29077936918112002, -33.81949288947817678 ) ) ;
#25759 = CARTESIAN_POINT ( 'NONE',  ( 24.91854708852270406, -24.40079863550579020, -22.15000000000000924 ) ) ;
#25760 = CARTESIAN_POINT ( 'NONE',  ( 11.91260932085662638, -21.26622862968680039, -49.55142757455319469 ) ) ;
#25761 = ADVANCED_FACE ( 'NONE', ( #30913 ), #14691, .F. ) ;
#25762 = ORIENTED_EDGE ( 'NONE', *, *, #1600, .T. ) ;
#25763 = B_SPLINE_CURVE_WITH_KNOTS ( 'NONE', 3,
 ( #26793, #6900, #31483, #11604, #42544, #22851, #38871, #2434, #47507, #7157, #23110, #39128, #42280, #2960, #47004, #18933 ),
 .UNSPECIFIED., .F., .F.,
 ( 4, 2, 2, 2, 2, 2, 2, 4 ),
 ( -5.400124999999999671E-13, 0.7105627886305859731, 1.313424307618820119, 1.690212756986460008, 1.931671722270319913, 2.414589652838039946, 3.187258341746380008, 3.863343444541179839 ),
 .UNSPECIFIED. ) ;
#25764 = ADVANCED_FACE ( 'NONE', ( #10513 ), #10521, .T. ) ;
#25765 = CARTESIAN_POINT ( 'NONE',  ( 14.14886614762370165, 1.362847559348080217, -35.02873218748179340 ) ) ;
#25766 = CARTESIAN_POINT ( 'NONE',  ( 47.09611959407079951, -54.55650624126920434, -75.12137911381070410 ) ) ;
#25767 = CARTESIAN_POINT ( 'NONE',  ( 49.79848667668909457, 12.57015533470270086, -6.517774395972690371 ) ) ;
#25768 = AXIS2_PLACEMENT_3D ( 'NONE', #2089, #2343, #18317 ) ;
#25769 = EDGE_CURVE ( 'NONE', #28199, #21295, #26985, .T. ) ;
#25770 = CARTESIAN_POINT ( 'NONE',  ( 52.06789743720410257, 13.88381105532070059, -11.75767006276409887 ) ) ;
#25771 = CARTESIAN_POINT ( 'NONE',  ( 51.97963026116360652, 21.17322201635790080, -53.55374510773989982 ) ) ;
#25772 = CARTESIAN_POINT ( 'NONE',  ( 51.02815224725549825, 19.65062265738080072, -76.14999943445199904 ) ) ;
#25773 = CARTESIAN_POINT ( 'NONE',  ( 57.74431620579319713, 13.88376939222820106, -25.44123524798349933 ) ) ;
#25774 = CARTESIAN_POINT ( 'NONE',  ( 8.788063236854998905, -18.37750765070880021, -72.17305407766760084 ) ) ;
#25775 = VERTEX_POINT ( 'NONE', #21627 ) ;
#25776 = CARTESIAN_POINT ( 'NONE',  ( 25.72499013618932651, -0.9180541517691319653, -34.79644660940672907 ) ) ;
#25777 = CARTESIAN_POINT ( 'NONE',  ( -11.22462160640339945, -41.78302095251060422, -5.474790624452850807 ) ) ;
#25778 = CARTESIAN_POINT ( 'NONE',  ( 76.75364055736000068, -40.92245084168380487, -14.31887545395620087 ) ) ;
#25780 = ADVANCED_FACE ( 'NONE', ( #13794 ), #3459, .F. ) ;
#25779 = CARTESIAN_POINT ( 'NONE',  ( 0.5716597380707004739, -15.61618894405949831, -8.050000000008262546 ) ) ;
#25781 =( BOUNDED_CURVE ( )  B_SPLINE_CURVE ( 3, ( #9241, #1363, #49844, #33319 ),
 .UNSPECIFIED., .F., .T. ) 
 B_SPLINE_CURVE_WITH_KNOTS ( ( 4, 4 ),
 ( 2.269173848739415078, 2.375544669831940237 ),
 .UNSPECIFIED. ) 
 CURVE ( )  GEOMETRIC_REPRESENTATION_ITEM ( )  RATIONAL_B_SPLINE_CURVE ( ( 1.000000000000000000, 0.9990573262772525220, 0.9990573262772525220, 1.000000000000000000 ) ) 
 REPRESENTATION_ITEM ( '' )  );
#25782 = DIRECTION ( 'NONE',  ( 1.000000000000000000, 0.000000000000000000, 0.000000000000000000 ) ) ;
#25783 = CARTESIAN_POINT ( 'NONE',  ( 22.21722746122567571, -10.53735606139580838, -65.28627145430250778 ) ) ;
#25784 = CARTESIAN_POINT ( 'NONE',  ( 12.72591348253150123, -21.52908204588105434, -79.11948583704311488 ) ) ;
#25785 = CARTESIAN_POINT ( 'NONE',  ( 59.11308834892447805, 16.26059245213280136, -49.51867816856292137 ) ) ;
#25786 = CARTESIAN_POINT ( 'NONE',  ( 43.60412366894710345, -43.70472620657429985, -5.064848484333539957 ) ) ;
#25787 = CARTESIAN_POINT ( 'NONE',  ( 22.90088705258820667, -15.61618575905976414, -62.45282818884277276 ) ) ;
#25788 = FACE_OUTER_BOUND ( 'NONE', #16635, .T. ) ;
#25789 = ORIENTED_EDGE ( 'NONE', *, *, #10245, .F. ) ;
#25790 = CARTESIAN_POINT ( 'NONE',  ( 23.55489827341749987, -14.95586022399930037, -51.03909337422119563 ) ) ;
#25791 = CARTESIAN_POINT ( 'NONE',  ( 64.43108017310198932, 0.9486745332807529074, -60.92803123004440380 ) ) ;
#25792 = ORIENTED_EDGE ( 'NONE', *, *, #24450, .T. ) ;
#25793 = CARTESIAN_POINT ( 'NONE',  ( -2.611048155534260395, 19.76244989865589829, -8.524257365257900787 ) ) ;
#25794 = CARTESIAN_POINT ( 'NONE',  ( 60.78207366828240055, -45.60272865987860769, -47.53378783808489771 ) ) ;
#25795 = CARTESIAN_POINT ( 'NONE',  ( 14.39186542499959920, -8.781882511953600812, -74.26773406640160147 ) ) ;
#25796 =( GEOMETRIC_REPRESENTATION_CONTEXT ( 3 ) GLOBAL_UNCERTAINTY_ASSIGNED_CONTEXT ( ( #3310 ) ) GLOBAL_UNIT_ASSIGNED_CONTEXT ( ( #12066, #4961, #9422 ) ) REPRESENTATION_CONTEXT ( 'NONE', 'WORKASPACE' ) );
#25797 = CARTESIAN_POINT ( 'NONE',  ( 22.15209459710153084, -20.75234990211308173, -61.73254012881733388 ) ) ;
#25799 = CARTESIAN_POINT ( 'NONE',  ( 12.14990911837581145, -8.703607423280148581, -35.12566392782755287 ) ) ;
#25798 = CARTESIAN_POINT ( 'NONE',  ( 44.67293909344935798, 8.774802390190076906, -63.39842665425204871 ) ) ;
#25800 = ADVANCED_FACE ( 'NONE', ( #38413 ), #50212, .F. ) ;
#25801 = CIRCLE ( 'NONE', #24972, 1.999999999999995115 ) ;
#25802 = CARTESIAN_POINT ( 'NONE',  ( 56.84932592767829362, -50.65659099804129539, -63.99406948319280275 ) ) ;
#25803 = CARTESIAN_POINT ( 'NONE',  ( 40.69061954106139467, -45.32287878058329511, -5.669818197142030058 ) ) ;
#25804 = ORIENTED_EDGE ( 'NONE', *, *, #45599, .T. ) ;
#25805 = EDGE_LOOP ( 'NONE', ( #2835, #6245, #40385, #10829 ) ) ;
#25806 = ORIENTED_EDGE ( 'NONE', *, *, #35062, .T. ) ;
#25807 = CARTESIAN_POINT ( 'NONE',  ( -22.75970726311355108, -18.37500023713087671, -54.70196997798354488 ) ) ;
#25808 = CARTESIAN_POINT ( 'NONE',  ( 53.12256372476250021, -49.57422361163540359, -49.14106871637599738 ) ) ;
#25809 = DIRECTION ( 'NONE',  ( 0.000000000000000000, 0.000000000000000000, 1.000000000000000000 ) ) ;
#25810 = CARTESIAN_POINT ( 'NONE',  ( 55.98862517971360120, -50.75900301025659900, -53.00668962061499911 ) ) ;
#25811 = ORIENTED_EDGE ( 'NONE', *, *, #31664, .T. ) ;
#25812 = VERTEX_POINT ( 'NONE', #14047 ) ;
#25813 = CARTESIAN_POINT ( 'NONE',  ( 23.90924003817241683, -14.10962612633021607, -77.44674804159603809 ) ) ;
#25814 = CARTESIAN_POINT ( 'NONE',  ( 50.12109376404330163, -53.47864665676979712, -55.01406006385839476 ) ) ;
#25815 = CARTESIAN_POINT ( 'NONE',  ( 11.13393739769619906, -55.30245861064819479, -24.15000000000000213 ) ) ;
#25816 = ORIENTED_EDGE ( 'NONE', *, *, #15091, .T. ) ;
#25817 = CARTESIAN_POINT ( 'NONE',  ( 56.84932592767840021, 19.42421310868259354, -74.14999999999999147 ) ) ;
#25818 = CARTESIAN_POINT ( 'NONE',  ( 53.70323348958860521, -50.76982429470329805, -76.35188063097180589 ) ) ;
#25819 = CARTESIAN_POINT ( 'NONE',  ( 60.23130391297029718, 14.55066440145539985, -47.24246919202519734 ) ) ;
#25820 = EDGE_CURVE ( 'NONE', #41896, #12580, #32707, .T. ) ;
#25821 = CARTESIAN_POINT ( 'NONE',  ( 19.56784363952110084, -8.559629194120539353, -77.65665421159729931 ) ) ;
#25822 = CARTESIAN_POINT ( 'NONE',  ( 1.027904703268269992, 11.45423359053189927, -15.65000000000000036 ) ) ;
#25823 = CARTESIAN_POINT ( 'NONE',  ( 43.16865701737530259, 13.99521548782530012, -6.804304403661720180 ) ) ;
#25824 = CARTESIAN_POINT ( 'NONE',  ( 42.30536707268809948, -43.16822450031050096, -3.349718967764970134 ) ) ;
#25825 = CARTESIAN_POINT ( 'NONE',  ( 22.14971581627796482, -18.71501114327763915, -28.45282021618999835 ) ) ;
#25826 = CARTESIAN_POINT ( 'NONE',  ( 55.98228069898435422, 14.58868318825703092, -25.31776496031197610 ) ) ;
#25827 = AXIS2_PLACEMENT_3D ( 'NONE', #9813, #49395, #9556 ) ;
#25828 = CARTESIAN_POINT ( 'NONE',  ( 64.62407509413539231, 1.313826662893059938, -70.30919366152539851 ) ) ;
#25829 = CARTESIAN_POINT ( 'NONE',  ( 9.366560669795820360, -15.61606439180730099, -33.84717978380999881 ) ) ;
#25830 = VECTOR ( 'NONE', #38129, 1000.000000000000000 ) ;
#25831 = VECTOR ( 'NONE', #40852, 1000.000000000000000 ) ;
#25832 = CARTESIAN_POINT ( 'NONE',  ( 67.98303682264749170, 0.1477386350055570063, -18.18688548989880260 ) ) ;
#25833 = ORIENTED_EDGE ( 'NONE', *, *, #30670, .T. ) ;
#25834 = CARTESIAN_POINT ( 'NONE',  ( 15.05440318628160057, -53.11618894467930119, -76.14999999999999147 ) ) ;
#25835 = CARTESIAN_POINT ( 'NONE',  ( 57.31533494679120366, 19.23294600587710335, -53.15033584403609979 ) ) ;
#25836 = EDGE_CURVE ( 'NONE', #8281, #45496, #5930, .T. ) ;
#25837 = DIRECTION ( 'NONE',  ( 0.000000000000000000, 0.000000000000000000, -1.000000000000000000 ) ) ;
#25838 = PLANE ( 'NONE',  #14222 ) ;
#25839 = CARTESIAN_POINT ( 'NONE',  ( 46.97440434136990461, -54.33447984715540002, -75.47461153638509757 ) ) ;
#25840 = CARTESIAN_POINT ( 'NONE',  ( 63.35681832276381442, 1.325839985408290067, -68.86912414701170349 ) ) ;
#25841 = CARTESIAN_POINT ( 'NONE',  ( 11.49998292432769986, 34.13930433918829976, -17.88621716035489939 ) ) ;
#25842 = B_SPLINE_CURVE_WITH_KNOTS ( 'NONE', 3,
 ( #43893, #5104, #24973, #21059, #36526, #27887, #40731, #28921, #36268, #24193, #37058, #49133, #16103, #44406, #4308, #9027, #24715, #378 ),
 .UNSPECIFIED., .F., .F.,
 ( 4, 2, 2, 2, 2, 2, 2, 2, 4 ),
 ( 0.000000000000000000, 0.1774999104122986782, 0.3374998296571877221, 0.4374997791852425766, 0.4999997476402775476, 0.6249996845503474896, 0.7565686301423247828, 0.9670789430894899397, 1.000000000000000000 ),
 .UNSPECIFIED. ) ;
#25843 = CARTESIAN_POINT ( 'NONE',  ( 24.04493737574808776, -16.65173435148965808, -51.83399569883714975 ) ) ;
#25844 = CARTESIAN_POINT ( 'NONE',  ( 56.43926849312130400, 19.54193581886750053, -53.62500735189280476 ) ) ;
#25845 = CARTESIAN_POINT ( 'NONE',  ( 47.97791291234110389, 23.15825109668029924, -55.19708778542380401 ) ) ;
#25846 = ORIENTED_EDGE ( 'NONE', *, *, #35887, .F. ) ;
#25847 = CARTESIAN_POINT ( 'NONE',  ( 19.11048863820259669, -9.222230711542339421, -76.48586413618289725 ) ) ;
#25848 = ORIENTED_EDGE ( 'NONE', *, *, #16036, .F. ) ;
#25849 = DIRECTION ( 'NONE',  ( 0.000000000000000000, 0.000000000000000000, -1.000000000000000000 ) ) ;
#25850 = CARTESIAN_POINT ( 'NONE',  ( 16.13393739769620083, -15.61618894467929941, 7.349999999999999645 ) ) ;
#25851 = CARTESIAN_POINT ( 'NONE',  ( 9.367282414267279478, -15.61633198492950036, -43.45282021618999835 ) ) ;
#25853 = DIRECTION ( 'NONE',  ( 0.3569024281753349626, 0.000000000000000000, 0.9341416684649872515 ) ) ;
#25852 = CARTESIAN_POINT ( 'NONE',  ( 84.43710458089100257, 12.07919292302930181, -47.42958317885469910 ) ) ;
#25854 = ADVANCED_FACE ( 'NONE', ( #9356 ), #2510, .F. ) ;
#25855 = CARTESIAN_POINT ( 'NONE',  ( 12.10839719180959939, -9.825024575796660997, -71.75946553180959597 ) ) ;
#25856 = CARTESIAN_POINT ( 'NONE',  ( 11.13393739769619906, -55.30245861064819479, -24.15000000000000213 ) ) ;
#25857 = CARTESIAN_POINT ( 'NONE',  ( 0.5774960717374452157, -22.43288435223359656, -34.81767276520686494 ) ) ;
#25858 = CARTESIAN_POINT ( 'NONE',  ( 56.18972397053033063, -45.98241309864640414, -26.01119422816448079 ) ) ;
#25859 = CARTESIAN_POINT ( 'NONE',  ( 16.13393739769620083, -15.61618894467929941, -18.58999999999999986 ) ) ;
#25860 = EDGE_CURVE ( 'NONE', #35517, #37146, #48908, .T. ) ;
#25861 = VERTEX_POINT ( 'NONE', #22922 ) ;
#25862 = ORIENTED_EDGE ( 'NONE', *, *, #30093, .T. ) ;
#25863 = ADVANCED_FACE ( 'NONE', ( #6969 ), #34983, .T. ) ;
#25864 = DIRECTION ( 'NONE',  ( 1.000000000000000000, 0.000000000000000000, 0.000000000000000000 ) ) ;
#25865 = CARTESIAN_POINT ( 'NONE',  ( 12.72020591613260088, 34.25200402611910278, -47.31888902628400473 ) ) ;
#25866 = CARTESIAN_POINT ( 'NONE',  ( 23.89338532170834384, -14.02234939633399335, -39.44318785247980230 ) ) ;
#25867 = CIRCLE ( 'NONE', #3299, 2.999999999999997780 ) ;
#25868 = CARTESIAN_POINT ( 'NONE',  ( 8.222262383277058717, -15.61618471288229948, -44.50766849176299900 ) ) ;
#25869 = LINE ( 'NONE', #17519, #9962 ) ;
#25870 = AXIS2_PLACEMENT_3D ( 'NONE', #32583, #32331, #20810 ) ;
#25871 = AXIS2_PLACEMENT_3D ( 'NONE', #17955, #38923, #30772 ) ;
#25872 = AXIS2_PLACEMENT_3D ( 'NONE', #46783, #30503, #11644 ) ;
#25873 = VERTEX_POINT ( 'NONE', #30530 ) ;
#25874 = CARTESIAN_POINT ( 'NONE',  ( -1.431265392021220162, -50.53043258612900246, -36.47998747206590053 ) ) ;
#25875 = CARTESIAN_POINT ( 'NONE',  ( 57.33795248997969907, 14.58087673940109852, -26.27059240990359967 ) ) ;
#25876 = AXIS2_PLACEMENT_3D ( 'NONE', #414, #19303, #28441 ) ;
#25877 = CARTESIAN_POINT ( 'NONE',  ( 47.28886650904659206, 23.50118699693149793, -54.78430227607729819 ) ) ;
#25878 = CARTESIAN_POINT ( 'NONE',  ( 59.89120361409349869, -2.379225728188540501, -15.76033884563189957 ) ) ;
#25879 = CARTESIAN_POINT ( 'NONE',  ( 51.16024758163639774, -50.72509723359110012, -76.16561535978119934 ) ) ;
#25880 = CARTESIAN_POINT ( 'NONE',  ( 60.25366577380279409, -46.63518866124190509, -48.78944481778400188 ) ) ;
#25881 = EDGE_CURVE ( 'NONE', #50462, #25775, #47855, .T. ) ;
#25882 = VERTEX_POINT ( 'NONE', #18748 ) ;
#25883 = DIRECTION ( 'NONE',  ( 1.000000000000000000, 0.000000000000000000, 0.000000000000000000 ) ) ;
#25884 = CARTESIAN_POINT ( 'NONE',  ( 68.13393739769814772, 19.38381105532029736, -71.50000000000200373 ) ) ;
#25885 = EDGE_LOOP ( 'NONE', ( #16026, #4818, #12948, #11400 ) ) ;
#25886 = CARTESIAN_POINT ( 'NONE',  ( 12.33745008528437026, -55.43540947936329388, -75.02879301533954504 ) ) ;
#25887 = DIRECTION ( 'NONE',  ( -0.7956403955640117820, 0.6057692307692287281, 0.000000000000000000 ) ) ;
#25888 = EDGE_CURVE ( 'NONE', #28421, #39126, #2668, .T. ) ;
#25889 = CARTESIAN_POINT ( 'NONE',  ( 13.26742230928919852, -7.885353774765291313, -79.17930779234588101 ) ) ;
#25890 = CARTESIAN_POINT ( 'NONE',  ( 13.32592044370020012, -50.85448151712510167, -21.60957454853980053 ) ) ;
#25891 = CARTESIAN_POINT ( 'NONE',  ( 54.67606251842929765, 19.48951422470729966, -76.08857982990380719 ) ) ;
#25892 = CARTESIAN_POINT ( 'NONE',  ( 47.48063017875849567, -54.33024059387050642, -75.12266286288350159 ) ) ;
#25893 = ORIENTED_EDGE ( 'NONE', *, *, #4979, .T. ) ;
#25894 = CARTESIAN_POINT ( 'NONE',  ( 55.96902438450270978, 14.60256988625710051, -17.93020271988870107 ) ) ;
#25895 = CARTESIAN_POINT ( 'NONE',  ( 47.66479567111289839, 23.29271780185170115, -55.15155557582939849 ) ) ;
#25896 = CARTESIAN_POINT ( 'NONE',  ( 56.96867955654300175, -50.47610601613909864, -53.05103816245590309 ) ) ;
#25897 = CARTESIAN_POINT ( 'NONE',  ( -30.36606260230379917, -53.11618894467940066, 17.35000000000000142 ) ) ;
#25898 = CARTESIAN_POINT ( 'NONE',  ( 22.90099047617777472, -15.26966479008347299, -44.83088873439039190 ) ) ;
#25899 = CARTESIAN_POINT ( 'NONE',  ( 47.07698750752110328, 22.65904192746489798, -75.76367654143750485 ) ) ;
#25900 = DIRECTION ( 'NONE',  ( 0.8660254037844390407, -0.4999999999999995004, 0.000000000000000000 ) ) ;
#25901 = CONICAL_SURFACE ( 'NONE', #6712, 12.92820323027549989, 0.7481802937784480800 ) ;
#25902 = CARTESIAN_POINT ( 'NONE',  ( 40.76017235305160114, -45.36108721241059527, -5.740519108723990627 ) ) ;
#25903 = CARTESIAN_POINT ( 'NONE',  ( 31.58225770014180256, -2.032350560841368114, -29.09832030244561807 ) ) ;
#25904 = AXIS2_PLACEMENT_3D ( 'NONE', #28407, #20284, #40225 ) ;
#25905 = CARTESIAN_POINT ( 'NONE',  ( 29.10811623682189975, -4.501937149316799669, -34.99013415954829753 ) ) ;
#25906 = VECTOR ( 'NONE', #2729, 1000.000000000000000 ) ;
#25907 = AXIS2_PLACEMENT_3D ( 'NONE', #23160, #12420, #27364 ) ;
#25908 = CARTESIAN_POINT ( 'NONE',  ( 18.86789271228450104, 20.55440457967890211, -74.14999999999999147 ) ) ;
#25909 = CARTESIAN_POINT ( 'NONE',  ( 24.04503344477293680, -15.61618896013167479, -37.50766614148061251 ) ) ;
#25910 = CARTESIAN_POINT ( 'NONE',  ( -15.83221208767410282, 6.858269193346590242, -48.53302639233909588 ) ) ;
#25912 = CARTESIAN_POINT ( 'NONE',  ( 46.38067733160732331, -40.25943396676748876, -54.53019052586303417 ) ) ;
#25911 = DIRECTION ( 'NONE',  ( 0.000000000000000000, 0.000000000000000000, 1.000000000000000000 ) ) ;
#25913 = AXIS2_PLACEMENT_3D ( 'NONE', #41110, #48456, #12825 ) ;
#25914 = CARTESIAN_POINT ( 'NONE',  ( 61.22873865439940033, 14.02808039422199826, -46.61559125704629736 ) ) ;
#25915 = CARTESIAN_POINT ( 'NONE',  ( -26.90058206776729932, 10.62243301518619987, -56.03720707547429924 ) ) ;
#25916 = ORIENTED_EDGE ( 'NONE', *, *, #30272, .F. ) ;
#25917 = CARTESIAN_POINT ( 'NONE',  ( 52.82947468502609922, -49.66147222709160047, -48.64744666514059901 ) ) ;
#25918 = VERTEX_POINT ( 'NONE', #35515 ) ;
#25919 = CARTESIAN_POINT ( 'NONE',  ( 44.05838509154141036, 8.810486217098942419, -66.03926413344439084 ) ) ;
#25920 = CARTESIAN_POINT ( 'NONE',  ( 19.78667132190540201, -9.582939898486838359, -40.52046943329969508 ) ) ;
#25921 = CARTESIAN_POINT ( 'NONE',  ( 57.05026703580490022, 13.94318891463120025, -25.51228499960440388 ) ) ;
#25922 = CARTESIAN_POINT ( 'NONE',  ( 13.16891555493870136, -9.216876155902941292, -41.81470958976149177 ) ) ;
#25923 = CARTESIAN_POINT ( 'NONE',  ( 28.71032976354209865, -26.58237652039480281, -34.65450330891889763 ) ) ;
#25924 = CARTESIAN_POINT ( 'NONE',  ( 53.24078573210410070, 18.24730475180699685, -49.04425871532740189 ) ) ;
#25925 = CARTESIAN_POINT ( 'NONE',  ( 64.83879995576869248, 1.326134026835569912, -60.90937915352040477 ) ) ;
#25926 = CARTESIAN_POINT ( 'NONE',  ( 11.27234472087837780, -21.94241871684008771, -58.21600153524056509 ) ) ;
#25927 = CARTESIAN_POINT ( 'NONE',  ( 55.68173555688790088, -48.93614072104979584, -53.85224183628929495 ) ) ;
#25928 = EDGE_CURVE ( 'NONE', #8909, #40766, #14454, .T. ) ;
#25929 = ORIENTED_EDGE ( 'NONE', *, *, #5322, .T. ) ;
#25930 = CARTESIAN_POINT ( 'NONE',  ( 18.20721935276529990, -22.77217918175530187, -71.47757758863500044 ) ) ;
#25931 = EDGE_CURVE ( 'NONE', #51329, #30578, #22668, .T. ) ;
#25932 = CARTESIAN_POINT ( 'NONE',  ( 72.73458218292580568, 1.393731187554809958, -68.81053500035210391 ) ) ;
#25933 = CARTESIAN_POINT ( 'NONE',  ( 21.61678711427710553, -9.893587190645865448, -49.53557109157861049 ) ) ;
#25934 = CARTESIAN_POINT ( 'NONE',  ( 73.18782247527531126, 0.8859637708054489691, -62.41593972647849853 ) ) ;
#25935 = CARTESIAN_POINT ( 'NONE',  ( 11.01613591012540105, -65.16628805936319679, -18.04558894943079750 ) ) ;
#25936 = CARTESIAN_POINT ( 'NONE',  ( 52.82975622904280755, 18.42854261028849905, -48.48625935290110078 ) ) ;
#25937 = DIRECTION ( 'NONE',  ( 0.3569024281753415129, 0.000000000000000000, 0.9341416684649846980 ) ) ;
#25938 = CARTESIAN_POINT ( 'NONE',  ( 71.40893329644849530, 0.8879664753683469414, -60.62259972594619484 ) ) ;
#25939 = CARTESIAN_POINT ( 'NONE',  ( 17.48127988501421370, -23.44392173378956556, -45.95340561908123078 ) ) ;
#25940 = CARTESIAN_POINT ( 'NONE',  ( 64.78392625511199299, 1.096932441169210071, -70.58143231363629866 ) ) ;
#25941 = ORIENTED_EDGE ( 'NONE', *, *, #4974, .T. ) ;
#25942 = CARTESIAN_POINT ( 'NONE',  ( 8.967302953424740153, -63.21494621409839709, -46.63268177960510030 ) ) ;
#25943 = LINE ( 'NONE', #14946, #5957 ) ;
#25944 = ORIENTED_EDGE ( 'NONE', *, *, #26854, .T. ) ;
#25945 = CARTESIAN_POINT ( 'NONE',  ( 10.13393739769589885, 22.91950879131600161, -34.64999999999999858 ) ) ;
#25946 = CARTESIAN_POINT ( 'NONE',  ( 9.366929578439700421, -14.73044796243286747, -69.49448701350169699 ) ) ;
#25947 = DIRECTION ( 'NONE',  ( 0.000000000000000000, 0.000000000000000000, -1.000000000000000000 ) ) ;
#25948 = AXIS2_PLACEMENT_3D ( 'NONE', #21319, #18179, #1423 ) ;
#25949 = CARTESIAN_POINT ( 'NONE',  ( 52.35198200795250045, 18.81557687444639981, -76.97988190764880301 ) ) ;
#25950 = VECTOR ( 'NONE', #15978, 1000.000000000000114 ) ;
#25951 = ORIENTED_EDGE ( 'NONE', *, *, #328, .F. ) ;
#25952 = DIRECTION ( 'NONE',  ( 0.000000000000000000, 0.000000000000000000, -1.000000000000000000 ) ) ;
#25953 = CARTESIAN_POINT ( 'NONE',  ( 44.07452568954059302, 1.883811055320659955, -54.64999999999999858 ) ) ;
#25954 = VECTOR ( 'NONE', #36572, 1000.000000000000114 ) ;
#25955 = CARTESIAN_POINT ( 'NONE',  ( 22.89852080129521283, -15.42085789721739708, -72.44363893989624614 ) ) ;
#25956 = CARTESIAN_POINT ( 'NONE',  ( 24.04472027134544021, -15.61619704117925522, -43.79232540400376905 ) ) ;
#25957 = CIRCLE ( 'NONE', #2560, 34.55616290057869833 ) ;
#25958 = EDGE_CURVE ( 'NONE', #11224, #29423, #49515, .T. ) ;
#25959 = B_SPLINE_SURFACE_WITH_KNOTS ( 'NONE', 3, 3, ( 
 ( #13648, #42911, #25671, #27159, #29858, #45879, #29354, #9966, #22958, #37749, #9711, #45360, #41941, #18784, #6042, #38980 ),
 ( #1586, #9462, #1846, #51022, #25410, #31081, #38008, #43167, #41413, #17575, #33543, #2817, #34762, #29608, #41673, #5779 ),
 ( #46851, #31591, #4090, #20316, #47362, #20574, #36305, #39492, #415, #12474, #16402, #23728, #11713, #24493, #36567, #3590 ),
 ( #43678, #27416, #48377, #32101, #36058, #167, #40511, #19563, #23977, #32359, #28442, #44444, #20064, #39744, #8027, #43930 ),
 ( #47612, #11459, #15383, #43421, #8550, #47870, #16141, #4599, #27676, #44183, #15894, #31336, #40001, #7778, #3846, #12219 ),
 ( #7521, #23469, #48120, #35552, #19819, #51542, #15639, #35807, #51791, #31851, #11973, #27928, #28181, #8283, #24231, #40256 ),
 ( #4348, #40768, #17701, #25540, #28964, #21354, #13265, #17190, #25794, #1198, #1456, #938, #29221, #21874, #41544, #16934 ),
 ( #45488, #16659, #44701, #5144, #41028, #25014, #21098, #33411, #33669, #28699, #37101, #13526, #48644, #29483, #8806, #4869 ),
 ( #20836, #32878, #49429, #9586, #33147, #41803, #49174, #36834, #37357, #5660, #21607, #48912, #32616, #1717, #37611, #45228 ),
 ( #9336, #45748, #49684, #5909, #13778, #669, #29732, #25283, #17445, #41287, #13009, #5397, #44963, #9842, #12744, #24758 ),
 ( #9065, #6694, #22392, #22652, #47057, #22131, #46794, #6172, #38138, #38396, #38672, #2757, #26581, #18729, #31031, #34967 ) ),
 .UNSPECIFIED., .F., .F., .F.,
 ( 4, 1, 1, 1, 1, 1, 1, 1, 4 ),
 ( 4, 2, 2, 2, 2, 2, 2, 4 ),
 ( 0.000000000000000000, 0.1250000000000000000, 0.2500000000000000000, 0.3750000000000000000, 0.5000000000000000000, 0.6250000000000000000, 0.7500000000000000000, 0.8750000000000000000, 1.000000000000000000 ),
 ( 6.048176999999999513E-14, 0.1586790292817849835, 0.3005262815670050047, 0.4007017087559869850, 0.4507894223504779752, 0.5309297641016630376, 0.6591543109035590264, 0.8014034175119129078 ),
 .UNSPECIFIED. ) ;
#25960 = CARTESIAN_POINT ( 'NONE',  ( 14.64547964051690165, -7.506490210384190398, -49.23455185029779813 ) ) ;
#25961 = B_SPLINE_CURVE_WITH_KNOTS ( 'NONE', 3,
 ( #24424, #5331, #40438, #4530, #17374, #33341, #20502, #36495, #599, #16584, #32537, #48571 ),
 .UNSPECIFIED., .F., .F.,
 ( 4, 2, 2, 2, 2, 4 ),
 ( 0.000000000000000000, 0.05115848177113838796, 0.3903315494385208306, 0.7421782045515662452, 0.9620823639972201358, 1.000000000000000000 ),
 .UNSPECIFIED. ) ;
#25962 = CARTESIAN_POINT ( 'NONE',  ( 10.82647640503957120, -11.32133379854484900, -55.66916738645966944 ) ) ;
#25963 = CARTESIAN_POINT ( 'NONE',  ( 44.35481541144333306, -37.96333356703264883, -68.54560956798736981 ) ) ;
#25964 = ADVANCED_FACE ( 'NONE', ( #47580 ), #27385, .T. ) ;
#25965 = VERTEX_POINT ( 'NONE', #50982 ) ;
#25966 = CARTESIAN_POINT ( 'NONE',  ( 57.23048878589050048, -45.83455400380619693, -26.25958840414919848 ) ) ;
#25967 = CARTESIAN_POINT ( 'NONE',  ( 17.71571533420349809, -22.89661972621449948, -46.66455827518219479 ) ) ;
#25968 = CARTESIAN_POINT ( 'NONE',  ( 9.116705508467720875, -14.11849739422179972, -32.14999999999999858 ) ) ;
#25969 = CARTESIAN_POINT ( 'NONE',  ( 13.42257066052990133, 20.48963383789619996, -74.34036667011370980 ) ) ;
#25970 = CARTESIAN_POINT ( 'NONE',  ( 11.13393739769619906, 24.07008072128950005, -43.74348518090240390 ) ) ;
#25971 = CARTESIAN_POINT ( 'NONE',  ( 41.13179987942019977, -45.04922869730629742, -5.658934828260900218 ) ) ;
#25972 = CARTESIAN_POINT ( 'NONE',  ( 24.04481203031673076, -15.61619115162449312, -61.50767625960597229 ) ) ;
#25973 = CARTESIAN_POINT ( 'NONE',  ( 24.37219564613430123, -15.95356372295639957, -63.52069670119330169 ) ) ;
#25974 = ORIENTED_EDGE ( 'NONE', *, *, #12785, .T. ) ;
#25975 = CARTESIAN_POINT ( 'NONE',  ( 53.35940782512449942, -48.99705445778459278, -26.69012152621940359 ) ) ;
#25976 = CARTESIAN_POINT ( 'NONE',  ( 54.76812893638570046, -50.71857552302670058, -76.05693996196100670 ) ) ;
#25977 = CARTESIAN_POINT ( 'NONE',  ( 10.83502951711263940, -21.55863658954535822, -40.23930580441716387 ) ) ;
#25979 = CARTESIAN_POINT ( 'NONE',  ( 41.87382049790848271, -39.75083843982427112, -76.94057980257345264 ) ) ;
#25978 = CARTESIAN_POINT ( 'NONE',  ( 70.26204857723202224, 12.15939804013194880, -11.90373897417649829 ) ) ;
#25980 = CARTESIAN_POINT ( 'NONE',  ( 13.90590011285059902, -8.924521810714191261, -52.24487123071539685 ) ) ;
#25981 = PLANE ( 'NONE',  #8880 ) ;
#25982 = AXIS2_PLACEMENT_3D ( 'NONE', #7938, #4005, #48032 ) ;
#25983 = ORIENTED_EDGE ( 'NONE', *, *, #25881, .T. ) ;
#25984 = CARTESIAN_POINT ( 'NONE',  ( -11.32734370190460105, -41.88171845330919751, -6.430192534648670133 ) ) ;
#25985 = AXIS2_PLACEMENT_3D ( 'NONE', #49285, #24875, #40884 ) ;
#25986 = CARTESIAN_POINT ( 'NONE',  ( 47.53188093336569864, 23.33481414632970186, -54.72542454593359906 ) ) ;
#25987 = DIRECTION ( 'NONE',  ( 0.000000000000000000, 0.000000000000000000, 1.000000000000000000 ) ) ;
#25988 = CARTESIAN_POINT ( 'NONE',  ( 63.20250508406000023, 1.096932441169210071, -62.29998885741579784 ) ) ;
#25989 = CARTESIAN_POINT ( 'NONE',  ( 12.99333467301740086, 19.39160263449290156, -21.36722376697930059 ) ) ;
#25990 = CARTESIAN_POINT ( 'NONE',  ( 68.13393739769618662, -30.31618894467939995, -65.65000000000000568 ) ) ;
#25991 = CIRCLE ( 'NONE', #13498, 15.29999999999999716 ) ;
#25992 = CARTESIAN_POINT ( 'NONE',  ( 11.62127288507080003, 34.09666180512939349, -17.36671666713459672 ) ) ;
#25993 = CARTESIAN_POINT ( 'NONE',  ( 22.90100109812010842, -16.68472418553394476, -56.89745730083780018 ) ) ;
#25994 = DIRECTION ( 'NONE',  ( 0.000000000000000000, -1.000000000000000000, 0.000000000000000000 ) ) ;
#25995 = CARTESIAN_POINT ( 'NONE',  ( 53.63393739769619373, -53.11618894467930119, 17.35000000000000142 ) ) ;
#25996 = CARTESIAN_POINT ( 'NONE',  ( 57.59125325346249724, -47.31051068446480201, -48.20109099143959952 ) ) ;
#25997 = CARTESIAN_POINT ( 'NONE',  ( 22.86391141925847492, -16.33902761098219614, -66.48686977775619766 ) ) ;
#25998 = ADVANCED_FACE ( 'NONE', ( #39194, #43386 ), #15081, .T. ) ;
#25999 = CARTESIAN_POINT ( 'NONE',  ( 54.45614327494340046, 20.39970296835699770, -54.11881936521780290 ) ) ;
#26000 = CARTESIAN_POINT ( 'NONE',  ( 63.62896973943209389, 1.416241615474740145, -69.07296579632759403 ) ) ;
#26001 = DIRECTION ( 'NONE',  ( 1.000000000000000000, 0.000000000000000000, 0.000000000000000000 ) ) ;
#26002 = LINE ( 'NONE', #45684, #45854 ) ;
#26003 = CARTESIAN_POINT ( 'NONE',  ( 19.94077147091733337, 23.62963092878765536, -18.33136226284473125 ) ) ;
#26004 = CARTESIAN_POINT ( 'NONE',  ( 10.77166614911110187, 32.01493747166969683, -45.20465578477089963 ) ) ;
#26005 = CARTESIAN_POINT ( 'NONE',  ( 72.71069314568710240, 1.377110276564839975, -62.16153651468360408 ) ) ;
#26006 = B_SPLINE_CURVE_WITH_KNOTS ( 'NONE', 3,
 ( #19564, #39231, #7522, #43422, #30824, #47110, #10940, #46852, #42912, #8028, #11461, #47613, #4091, #27160, #23729, #15384 ),
 .UNSPECIFIED., .F., .F.,
 ( 4, 2, 2, 2, 2, 2, 2, 4 ),
 ( 0.000000000000000000, 1.392512724848399941, 2.647735462739909895, 3.432249673922110222, 3.922571055910980320, 4.903213819888729397, 6.472242242253120281, 7.845142111821970410 ),
 .UNSPECIFIED. ) ;
#26007 = CARTESIAN_POINT ( 'NONE',  ( 66.14674587413610141, -31.04161172517479983, -17.02975172920780267 ) ) ;
#26008 = CARTESIAN_POINT ( 'NONE',  ( 9.366705026548178381, -15.88967530897099678, -47.83432355292423210 ) ) ;
#26009 = ORIENTED_EDGE ( 'NONE', *, *, #24921, .F. ) ;
#26010 = ORIENTED_EDGE ( 'NONE', *, *, #27200, .F. ) ;
#26011 = CARTESIAN_POINT ( 'NONE',  ( 49.60654698967459808, 22.46544607396180027, -55.15184126837920076 ) ) ;
#26012 = CARTESIAN_POINT ( 'NONE',  ( 50.77833043287579073, -0.1940347697328212717, -16.58944421967073524 ) ) ;
#26013 = ORIENTED_EDGE ( 'NONE', *, *, #48371, .T. ) ;
#26014 = CARTESIAN_POINT ( 'NONE',  ( 12.05814235705390125, -65.22170215249130365, -46.28435471616069918 ) ) ;
#26015 = CARTESIAN_POINT ( 'NONE',  ( 56.86392865038990152, -45.57086430673709998, -26.04468540372219820 ) ) ;
#26016 = CARTESIAN_POINT ( 'NONE',  ( 24.04493736746855959, -15.61700137643269315, -77.50770766772195941 ) ) ;
#26017 = CARTESIAN_POINT ( 'NONE',  ( 63.54731047306190561, 1.396834109478129804, -62.44999999999999574 ) ) ;
#26018 = ORIENTED_EDGE ( 'NONE', *, *, #47852, .F. ) ;
#26019 = CARTESIAN_POINT ( 'NONE',  ( 46.47824713337531932, 6.969044071021170517, -57.92844982156870515 ) ) ;
#26020 = VERTEX_POINT ( 'NONE', #31049 ) ;
#26021 = EDGE_CURVE ( 'NONE', #11422, #6409, #46188, .T. ) ;
#26022 = CARTESIAN_POINT ( 'NONE',  ( 51.85399221484009757, -45.59830427757680127, -13.29383979432519958 ) ) ;
#26023 = CARTESIAN_POINT ( 'NONE',  ( 16.25866331035335222, -23.60640883099551601, -34.28700762286280934 ) ) ;
#26024 = CARTESIAN_POINT ( 'NONE',  ( 14.56142577301880081, 19.88381692480329832, -22.31059544230340208 ) ) ;
#26025 = EDGE_CURVE ( 'NONE', #42086, #13057, #31930, .T. ) ;
#26026 = FACE_OUTER_BOUND ( 'NONE', #825, .T. ) ;
#26027 = AXIS2_PLACEMENT_3D ( 'NONE', #51604, #35616, #3400 ) ;
#26028 = CARTESIAN_POINT ( 'NONE',  ( 13.63393739769599833, 14.38381105532070059, -34.64999999999999858 ) ) ;
#26029 = CARTESIAN_POINT ( 'NONE',  ( 46.74845599210109981, -53.81985652269789711, -75.90842213619210099 ) ) ;
#26030 = CIRCLE ( 'NONE', #18519, 20.00000000000000355 ) ;
#26031 = CARTESIAN_POINT ( 'NONE',  ( 49.73684662565250392, 13.14257322138860040, -6.768569892874900518 ) ) ;
#26032 = TOROIDAL_SURFACE ( 'NONE', #36101, 23.49999999832119713, 0.5000000000814219803 ) ;
#26033 = CARTESIAN_POINT ( 'NONE',  ( 50.47459759387780309, -50.28724450852030259, -76.14999999999999147 ) ) ;
#26034 = LINE ( 'NONE', #38638, #25906 ) ;
#26035 = CARTESIAN_POINT ( 'NONE',  ( 51.42797782268849716, 19.97168430531710115, -76.10787250224271361 ) ) ;
#26036 = CARTESIAN_POINT ( 'NONE',  ( 58.51605347960990144, 13.88377689860699959, -25.61130927043330274 ) ) ;
#26037 = CARTESIAN_POINT ( 'NONE',  ( 17.37891786306619935, -23.36452888456510024, -67.73679393810499505 ) ) ;
#26038 = ORIENTED_EDGE ( 'NONE', *, *, #845, .F. ) ;
#26039 = DIRECTION ( 'NONE',  ( 0.000000000000000000, 0.000000000000000000, 1.000000000000000000 ) ) ;
#26040 = CARTESIAN_POINT ( 'NONE',  ( -9.207529314482119531, -42.75858213421489751, -4.288095148114170030 ) ) ;
#26041 = DIRECTION ( 'NONE',  ( 0.000000000000000000, 0.000000000000000000, 1.000000000000000000 ) ) ;
#26042 = CARTESIAN_POINT ( 'NONE',  ( 72.64733618323120368, 1.408710407022059963, -69.13189173240590435 ) ) ;
#26043 = PRODUCT_RELATED_PRODUCT_CATEGORY ( 'part', '', ( #35664 ) ) ;
#26044 = CARTESIAN_POINT ( 'NONE',  ( 20.13393739768955726, -55.41568642894477392, -74.40622738393629731 ) ) ;
#26045 = CARTESIAN_POINT ( 'NONE',  ( 7.523314408995540603, 29.85141564380720069, -20.29480228628009542 ) ) ;
#26046 = CARTESIAN_POINT ( 'NONE',  ( 24.04493741622511749, -14.58065722670617248, -43.46598914385031520 ) ) ;
#26047 = CARTESIAN_POINT ( 'NONE',  ( 41.52331217820510290, 12.65721966367290108, -3.580227199495849888 ) ) ;
#26048 = CARTESIAN_POINT ( 'NONE',  ( 64.95360084570988590, 1.395196698723379924, -70.24366017557039754 ) ) ;
#26049 = DIRECTION ( 'NONE',  ( -0.7071067811865511255, -0.7071067811865440200, 0.000000000000000000 ) ) ;
#26050 = DIRECTION ( 'NONE',  ( 0.9486832980505123247, 0.000000000000000000, 0.3162277660168421045 ) ) ;
#26051 = EDGE_CURVE ( 'NONE', #24834, #46021, #33751, .T. ) ;
#26052 = CARTESIAN_POINT ( 'NONE',  ( 26.13393739769619728, -2.337132753317950229, -39.64999999999999858 ) ) ;
#26053 = CARTESIAN_POINT ( 'NONE',  ( 18.74893938429089957, -51.88241111309920228, -74.91994212300119216 ) ) ;
#26054 = CYLINDRICAL_SURFACE ( 'NONE', #2214, 10.00000000000000711 ) ;
#26055 = EDGE_LOOP ( 'NONE', ( #13540, #41048, #49454, #26645 ) ) ;
#26056 = ADVANCED_FACE ( 'NONE', ( #23431, #32320 ), #43895, .T. ) ;
#26057 = CARTESIAN_POINT ( 'NONE',  ( 12.50377125389449873, -9.110146514235310633, -50.40534192571220018 ) ) ;
#26058 = EDGE_CURVE ( 'NONE', #20782, #29727, #3504, .T. ) ;
#26059 = CARTESIAN_POINT ( 'NONE',  ( 63.83199809114920242, 1.060191324942699964, -61.46728771041559725 ) ) ;
#26060 = ORIENTED_EDGE ( 'NONE', *, *, #4133, .F. ) ;
#26061 = CARTESIAN_POINT ( 'NONE',  ( 22.04685453431686071, -19.02416987423216455, -68.61948488014840564 ) ) ;
#26062 = AXIS2_PLACEMENT_3D ( 'NONE', #35252, #38942, #31557 ) ;
#26063 = CARTESIAN_POINT ( 'NONE',  ( 29.13393739769619728, -33.11618894467940066, -34.64999999999999858 ) ) ;
#26064 = CARTESIAN_POINT ( 'NONE',  ( 22.90122453025153249, -15.61618899996915211, -58.45282045073077626 ) ) ;
#26065 = CARTESIAN_POINT ( 'NONE',  ( 18.27335346058083232, -23.24998756582152382, -61.92073563639246458 ) ) ;
#26067 = DIRECTION ( 'NONE',  ( -1.000000000000000000, -0.000000000000000000, -0.000000000000000000 ) ) ;
#26066 = CARTESIAN_POINT ( 'NONE',  ( 44.29800273259771615, 8.746227658329765120, -65.21609057545674659 ) ) ;
#26068 = EDGE_CURVE ( 'NONE', #9489, #41896, #3236, .T. ) ;
#26069 = CARTESIAN_POINT ( 'NONE',  ( 10.00711282696240012, -18.74238904653320148, -81.23899999999999011 ) ) ;
#26070 = DIRECTION ( 'NONE',  ( 0.7800418122827239564, 0.000000000000000000, -0.6257273935913973961 ) ) ;
#26071 = ORIENTED_EDGE ( 'NONE', *, *, #1763, .F. ) ;
#26072 = ORIENTED_EDGE ( 'NONE', *, *, #35822, .F. ) ;
#26073 = ORIENTED_EDGE ( 'NONE', *, *, #45206, .T. ) ;
#26074 = CARTESIAN_POINT ( 'NONE',  ( 61.18552659700819873, -45.29711232550319266, -46.94415545492860531 ) ) ;
#26075 = CARTESIAN_POINT ( 'NONE',  ( 60.97477285130578650, 14.20885590850662261, -47.29314152441210695 ) ) ;
#26076 = CARTESIAN_POINT ( 'NONE',  ( 82.75389963950320293, -45.59493862562369770, -47.67227237921210303 ) ) ;
#26077 = EDGE_CURVE ( 'NONE', #13824, #39880, #37010, .T. ) ;
#26078 = ORIENTED_EDGE ( 'NONE', *, *, #41164, .F. ) ;
#26079 = ORIENTED_EDGE ( 'NONE', *, *, #30788, .F. ) ;
#26080 = CARTESIAN_POINT ( 'NONE',  ( 21.54526366514968316, -19.77485305479494215, -72.66112179359276979 ) ) ;
#26081 = CARTESIAN_POINT ( 'NONE',  ( 28.13393739769619728, -8.687985714403843929, -35.01561944896766221 ) ) ;
#26082 = ADVANCED_FACE ( 'NONE', ( #32064 ), #24195, .F. ) ;
#26083 = CARTESIAN_POINT ( 'NONE',  ( -6.866062602303790285, -15.61618894467929941, -59.64999999999999147 ) ) ;
#26084 = VERTEX_POINT ( 'NONE', #8509 ) ;
#26085 = CARTESIAN_POINT ( 'NONE',  ( 23.07061256195587617, -19.52359038917101941, -49.67076867670061802 ) ) ;
#26086 = CARTESIAN_POINT ( 'NONE',  ( 51.63598217325660045, -50.37061234098579376, -76.35349662556009775 ) ) ;
#26087 = CARTESIAN_POINT ( 'NONE',  ( 60.77503050668930484, 14.28448999696009913, -47.26114755906990439 ) ) ;
#26088 = CARTESIAN_POINT ( 'NONE',  ( 16.73976790070870280, -23.44049191639519947, -74.48789696905249968 ) ) ;
#26089 = DIRECTION ( 'NONE',  ( 0.000000000000000000, -1.000000000000000000, 0.000000000000000000 ) ) ;
#26090 = CARTESIAN_POINT ( 'NONE',  ( 45.82863908892869631, 13.88351059623800055, -7.494183445420209644 ) ) ;
#26091 = CARTESIAN_POINT ( 'NONE',  ( 42.33768682256320659, -43.16216139800930307, -3.566431340445090026 ) ) ;
#26092 = CARTESIAN_POINT ( 'NONE',  ( 7.517033938252880354, 30.35161808146150264, -19.14999999999999858 ) ) ;
#26093 = CIRCLE ( 'NONE', #16084, 5.499999999999998224 ) ;
#26094 =( BOUNDED_CURVE ( )  B_SPLINE_CURVE ( 3, ( #33205, #9389, #5960, #25334 ),
 .UNSPECIFIED., .F., .T. ) 
 B_SPLINE_CURVE_WITH_KNOTS ( ( 4, 4 ),
 ( 5.387239059104177663, 6.283185307179586232 ),
 .UNSPECIFIED. ) 
 CURVE ( )  GEOMETRIC_REPRESENTATION_ITEM ( )  RATIONAL_B_SPLINE_CURVE ( ( 1.000000000000000000, 0.9342179155433358861, 0.9342179155433358861, 1.000000000000000000 ) ) 
 REPRESENTATION_ITEM ( '' )  );
#26095 = CIRCLE ( 'NONE', #21083, 4.649999999999999467 ) ;
#26096 = EDGE_CURVE ( 'NONE', #16045, #45245, #23940, .T. ) ;
#26097 = CARTESIAN_POINT ( 'NONE',  ( 64.93393739769619799, 1.396834109478129804, -70.23662692463440749 ) ) ;
#26098 = CARTESIAN_POINT ( 'NONE',  ( -28.43713041416928178, 28.95487886718607839, 17.35000000000000142 ) ) ;
#26099 = FACE_OUTER_BOUND ( 'NONE', #47654, .T. ) ;
#26100 = EDGE_LOOP ( 'NONE', ( #32957, #27217, #42142, #1935 ) ) ;
#26101 = DIRECTION ( 'NONE',  ( -0.8696770943991732894, 0.4936210606096660958, -7.688651000000001506E-17 ) ) ;
#26102 = CARTESIAN_POINT ( 'NONE',  ( 57.30262419534599871, 19.28754421135300134, -53.29749903242779396 ) ) ;
#26103 = CARTESIAN_POINT ( 'NONE',  ( 9.618181908336627117, 33.17626444789963358, -46.87734673171561184 ) ) ;
#26104 = DIRECTION ( 'NONE',  ( 0.000000000000000000, -0.7371541403039566509, 0.6757246284047478957 ) ) ;
#26105 = CARTESIAN_POINT ( 'NONE',  ( 46.44868656089280279, -53.13167745678150311, -76.13981661584659832 ) ) ;
#26106 = CARTESIAN_POINT ( 'NONE',  ( 63.46249669555339779, 1.383767307422960169, -68.70744520365728647 ) ) ;
#26107 = CARTESIAN_POINT ( 'NONE',  ( 47.82090655655320433, -54.45843870253389696, -55.22757576880370323 ) ) ;
#26108 = CARTESIAN_POINT ( 'NONE',  ( 9.407816849586122743, -14.19422756809612274, -49.91407474786834086 ) ) ;
#26109 = CARTESIAN_POINT ( 'NONE',  ( 17.20688454841970128, 14.56395709402249850, -35.14999999999999858 ) ) ;
#26110 = CARTESIAN_POINT ( 'NONE',  ( 48.17643508576089317, 23.07461921580190278, -55.27613280443460297 ) ) ;
#26111 = ORIENTED_EDGE ( 'NONE', *, *, #23895, .T. ) ;
#26112 = ADVANCED_FACE ( 'NONE', ( #897 ), #11885, .T. ) ;
#26113 = CARTESIAN_POINT ( 'NONE',  ( 21.09281434348019602, -20.63137574190060164, -71.09897682385668816 ) ) ;
#26114 = ADVANCED_FACE ( 'NONE', ( #4057 ), #1269, .T. ) ;
#26115 = VERTEX_POINT ( 'NONE', #47518 ) ;
#26117 = CARTESIAN_POINT ( 'NONE',  ( 71.42298070439039748, 0.9242073871622918935, -70.66822101033309877 ) ) ;
#26116 = PRODUCT_DEFINITION_SHAPE ( 'NONE', 'NONE',  #45296 ) ;
#26118 = SPHERICAL_SURFACE ( 'NONE', #24541, 0.5000000000000000000 ) ;
#26119 = CARTESIAN_POINT ( 'NONE',  ( 82.75389963950189554, 14.36256073625980001, -47.67227237920639737 ) ) ;
#26120 = CARTESIAN_POINT ( 'NONE',  ( 47.04404845359650267, 8.017726918288019533, -34.85732842610089932 ) ) ;
#26121 = CARTESIAN_POINT ( 'NONE',  ( 83.78435757737699419, 13.39064817555830089, -47.11582429421620333 ) ) ;
#26122 = CARTESIAN_POINT ( 'NONE',  ( 17.53487969994000295, -22.52849097422360103, -78.88916932753549816 ) ) ;
#26124 = ADVANCED_FACE ( 'NONE', ( #2974 ), #45207, .F. ) ;
#26123 = LINE ( 'NONE', #42135, #13698 ) ;
#26125 = CARTESIAN_POINT ( 'NONE',  ( 71.47612964547808190, 0.8925687589132609290, -70.63296852923029689 ) ) ;
#26126 = DIRECTION ( 'NONE',  ( -1.000000000000000000, 0.000000000000000000, 0.000000000000000000 ) ) ;
#26127 = EDGE_LOOP ( 'NONE', ( #43685, #38203, #12704, #32261 ) ) ;
#26128 = DIRECTION ( 'NONE',  ( 0.000000000000000000, 0.000000000000000000, -1.000000000000000000 ) ) ;
#26129 = ORIENTED_EDGE ( 'NONE', *, *, #51230, .F. ) ;
#26130 = ORIENTED_EDGE ( 'NONE', *, *, #29395, .F. ) ;
#26131 = CARTESIAN_POINT ( 'NONE',  ( 12.36320305068320025, -64.54682834576858852, -15.76422791927960176 ) ) ;
#26132 = CARTESIAN_POINT ( 'NONE',  ( 24.04491295644446680, -15.59492720088391948, -39.50681616597011470 ) ) ;
#26133 = CIRCLE ( 'NONE', #3565, 2.000000000000000000 ) ;
#26134 = DIRECTION ( 'NONE',  ( 1.224646799147353207E-16, 1.000000000000000000, -0.000000000000000000 ) ) ;
#26135 = CARTESIAN_POINT ( 'NONE',  ( 12.39246200226850014, -65.46010474692718617, -47.59569286893109563 ) ) ;
#26136 = CIRCLE ( 'NONE', #1049, 18.86180339887500068 ) ;
#26137 = ORIENTED_EDGE ( 'NONE', *, *, #29900, .F. ) ;
#26138 = ORIENTED_EDGE ( 'NONE', *, *, #43117, .T. ) ;
#26139 = CARTESIAN_POINT ( 'NONE',  ( -22.46120355510790034, -21.45481835963710182, -54.31569267914190391 ) ) ;
#26140 = CARTESIAN_POINT ( 'NONE',  ( 64.43393739769679485, 11.38381105532070059, -68.84999999999999432 ) ) ;
#26141 = CARTESIAN_POINT ( 'NONE',  ( 52.73337885104540135, 18.44966310541049737, -48.25078709180450431 ) ) ;
#26142 = CARTESIAN_POINT ( 'NONE',  ( 65.47927597481400142, -1.466436190217940139, -16.55648068461299971 ) ) ;
#26143 = ADVANCED_FACE ( 'NONE', ( #33350, #48842 ), #24952, .T. ) ;
#26144 = CARTESIAN_POINT ( 'NONE',  ( 51.14620533116269741, -49.75767105349819985, -76.32769630694630791 ) ) ;
#26145 = CARTESIAN_POINT ( 'NONE',  ( 59.38599522353990068, -47.70324967091819701, -49.95552091575579823 ) ) ;
#26146 = VERTEX_POINT ( 'NONE', #25736 ) ;
#26147 = CARTESIAN_POINT ( 'NONE',  ( 22.02282920616732653, -10.31289947776867955, -33.55901135124811674 ) ) ;
#26148 = CARTESIAN_POINT ( 'NONE',  ( 70.83393739769690001, 16.88381105531530579, -74.20000000000047180 ) ) ;
#26149 = EDGE_LOOP ( 'NONE', ( #20776, #30250 ) ) ;
#26150 = CARTESIAN_POINT ( 'NONE',  ( 20.99566274868214322, -9.290061469335373801, -57.21600112116089321 ) ) ;
#26151 = CARTESIAN_POINT ( 'NONE',  ( 55.64908854110159808, -48.32622745761450034, -48.64133301306080170 ) ) ;
#26152 = CARTESIAN_POINT ( 'NONE',  ( 13.93647208143119975, -23.14997244139559740, -46.60283323465849747 ) ) ;
#26153 = CARTESIAN_POINT ( 'NONE',  ( 52.97768859602520308, -49.62760585955020076, -49.05519427004490041 ) ) ;
#26154 = CARTESIAN_POINT ( 'NONE',  ( 14.04300386716569982, -50.94367055530580757, -21.72002249117950257 ) ) ;
#26155 = CARTESIAN_POINT ( 'NONE',  ( 57.01957022279430021, 19.39593752494300105, -74.14897285927730763 ) ) ;
#26156 = CARTESIAN_POINT ( 'NONE',  ( 46.69907961121389661, -53.35444326668270065, -76.07703971530399656 ) ) ;
#26157 = ORIENTED_EDGE ( 'NONE', *, *, #3185, .F. ) ;
#26158 = CARTESIAN_POINT ( 'NONE',  ( 55.95110166314709943, 14.60640795197440056, -17.62158316991920159 ) ) ;
#26159 = FACE_OUTER_BOUND ( 'NONE', #26180, .T. ) ;
#26160 = CARTESIAN_POINT ( 'NONE',  ( 56.57206750191940614, -50.73353241686610460, -53.72158482581370009 ) ) ;
#26161 = EDGE_CURVE ( 'NONE', #4963, #10362, #14373, .T. ) ;
#26162 = CARTESIAN_POINT ( 'NONE',  ( 19.00123712817629951, -22.05987976827099928, -43.21391308946270016 ) ) ;
#26163 = CARTESIAN_POINT ( 'NONE',  ( 9.366359964801500126, -15.61275108346748119, -43.84734136853051467 ) ) ;
#26164 = ORIENTED_EDGE ( 'NONE', *, *, #38268, .F. ) ;
#26165 = EDGE_CURVE ( 'NONE', #34653, #13586, #38222, .T. ) ;
#26166 = CARTESIAN_POINT ( 'NONE',  ( 47.32559383855520707, 22.99766105135049798, -75.35927704317229825 ) ) ;
#26167 = CARTESIAN_POINT ( 'NONE',  ( 65.16374186055298878, 1.338092079250050137, -60.76305085381149951 ) ) ;
#26168 = CARTESIAN_POINT ( 'NONE',  ( 75.16211347727251280, -29.54091756298097948, -11.85653830296175926 ) ) ;
#26169 = CARTESIAN_POINT ( 'NONE',  ( 104.6856170952499809, -2.032350560839140119, -65.65000000000000568 ) ) ;
#26170 = CIRCLE ( 'NONE', #1092, 28.31678667024650409 ) ;
#26171 = CARTESIAN_POINT ( 'NONE',  ( 57.50723795381379944, -45.11618894467940066, -25.33268388717609909 ) ) ;
#26172 = DIRECTION ( 'NONE',  ( 0.3805321250008310008, 0.000000000000000000, -0.9247677015566404535 ) ) ;
#26173 = CARTESIAN_POINT ( 'NONE',  ( 82.68210891836909582, 14.16981534136089849, -47.42732332448029808 ) ) ;
#26174 = CARTESIAN_POINT ( 'NONE',  ( -9.374724833670061486, 14.33830887257789932, -43.22289157268509996 ) ) ;
#26176 = CARTESIAN_POINT ( 'NONE',  ( 40.88670949972279089, -39.06981162304028032, -85.10457558764954911 ) ) ;
#26175 = CARTESIAN_POINT ( 'NONE',  ( -18.86606260230390220, 19.38381105532060289, 11.34999999999999964 ) ) ;
#26177 = CARTESIAN_POINT ( 'NONE',  ( 8.222918819271470170, -14.44621895267512990, -70.55475847918624765 ) ) ;
#26178 = PLANE ( 'NONE',  #25415 ) ;
#26179 = CARTESIAN_POINT ( 'NONE',  ( 12.76594342643739921, 33.07036822156479872, -45.89070534480030261 ) ) ;
#26180 = EDGE_LOOP ( 'NONE', ( #26900, #47628, #44992, #27171 ) ) ;
#26181 = ADVANCED_FACE ( 'NONE', ( #14742 ), #22587, .T. ) ;
#26182 = CARTESIAN_POINT ( 'NONE',  ( 52.76604523481000086, -49.70803434126499809, -48.76247711586999856 ) ) ;
#26183 = ORIENTED_EDGE ( 'NONE', *, *, #7969, .F. ) ;
#26184 = CARTESIAN_POINT ( 'NONE',  ( 47.22257521636639410, 8.040674068322497092, -54.75197889428296349 ) ) ;
#26185 = CARTESIAN_POINT ( 'NONE',  ( 9.366937397696199596, -15.61618894467949836, -28.45282021618999835 ) ) ;
#26186 = CARTESIAN_POINT ( 'NONE',  ( 13.79402747301139875, 19.88244612326230154, -22.16946263372249959 ) ) ;
#26187 = CARTESIAN_POINT ( 'NONE',  ( 57.25554329504040396, 13.89079948325800018, -25.31272174971099886 ) ) ;
#26188 = CARTESIAN_POINT ( 'NONE',  ( 10.47335541784519997, -11.40900813729630059, -41.65627172763429797 ) ) ;
#26189 = CARTESIAN_POINT ( 'NONE',  ( 36.93393739769619799, -15.61618894467929941, -12.65000000000000036 ) ) ;
#26191 = EDGE_CURVE ( 'NONE', #31099, #34663, #38671, .T. ) ;
#26190 = CARTESIAN_POINT ( 'NONE',  ( 53.26169323521300214, 18.26921110352349942, -49.13884436845789594 ) ) ;
#26192 = CARTESIAN_POINT ( 'NONE',  ( 64.78711365736010919, 1.264121749638659864, -60.84994802006399794 ) ) ;
#26193 = DIRECTION ( 'NONE',  ( -1.000000000000000000, 0.000000000000000000, 0.000000000000000000 ) ) ;
#26194 = EDGE_LOOP ( 'NONE', ( #8388, #20729, #6499, #1770 ) ) ;
#26195 = CARTESIAN_POINT ( 'NONE',  ( 10.36331059341320149, -10.29767275415630046, -36.52453509903889994 ) ) ;
#26196 = CARTESIAN_POINT ( 'NONE',  ( 73.00002125581650603, 1.102139304147779830, -69.09899266709390986 ) ) ;
#26197 = CARTESIAN_POINT ( 'NONE',  ( 24.04485446177871921, -15.57701860679610562, -49.79075491074868864 ) ) ;
#26198 = CARTESIAN_POINT ( 'NONE',  ( 72.79634974714259954, 1.384378348444520013, -62.56683295884919715 ) ) ;
#26199 = CARTESIAN_POINT ( 'NONE',  ( 11.89321892218980103, -65.43602743108449715, -18.17421237902440012 ) ) ;
#26200 = DIRECTION ( 'NONE',  ( 0.000000000000000000, 0.000000000000000000, -1.000000000000000000 ) ) ;
#26201 = CARTESIAN_POINT ( 'NONE',  ( 24.04493739753763748, -15.62200579106754184, -75.79256001894520978 ) ) ;
#26202 = CARTESIAN_POINT ( 'NONE',  ( 14.52552095220001327, -9.025673756071128651, -61.87668528295537129 ) ) ;
#26203 = CARTESIAN_POINT ( 'NONE',  ( 23.09841952678586807, -19.38864957793463617, -45.66577835145771047 ) ) ;
#26204 = CARTESIAN_POINT ( 'NONE',  ( 65.07649219403899110, 1.383767307422960169, -70.32144070214289400 ) ) ;
#26205 = ORIENTED_EDGE ( 'NONE', *, *, #453, .T. ) ;
#26206 = CARTESIAN_POINT ( 'NONE',  ( 10.14016983710170017, -63.19813366497749030, -45.99431160738090085 ) ) ;
#26207 = CIRCLE ( 'NONE', #42119, 21.50000000000000000 ) ;
#26208 = LINE ( 'NONE', #5798, #42830 ) ;
#26209 = ORIENTED_EDGE ( 'NONE', *, *, #3266, .F. ) ;
#26210 = CARTESIAN_POINT ( 'NONE',  ( 22.90121638405171467, -15.61618906730874734, -72.84718036870921765 ) ) ;
#26211 = CARTESIAN_POINT ( 'NONE',  ( 57.27159524557450254, 19.01963230153999973, -52.75109250000340211 ) ) ;
#26212 = CARTESIAN_POINT ( 'NONE',  ( 53.83004547088629721, 19.36722000321880088, -77.06233108604320137 ) ) ;
#26213 = TOROIDAL_SURFACE ( 'NONE', #46326, 5.500000000000000000, 0.5000000000000000000 ) ;
#26214 = VERTEX_POINT ( 'NONE', #6891 ) ;
#26215 = VECTOR ( 'NONE', #14102, 1000.000000000000000 ) ;
#26216 = CARTESIAN_POINT ( 'NONE',  ( 12.77233515538412512, -65.50098146119171361, -47.69352623444314787 ) ) ;
#26217 = DIRECTION ( 'NONE',  ( 0.000000000000000000, 1.000000000000000000, 0.000000000000000000 ) ) ;
#26218 = DIRECTION ( 'NONE',  ( -0.8660254037844387076, -0.4999999999999998890, 1.110223024625155678E-16 ) ) ;
#26219 = DIRECTION ( 'NONE',  ( 0.7071067811865475727, 0.000000000000000000, -0.7071067811865475727 ) ) ;
#26220 = CARTESIAN_POINT ( 'NONE',  ( 23.96847382039350194, -13.04660549645949885, -59.69145075069550188 ) ) ;
#26221 = DIRECTION ( 'NONE',  ( 1.000000000000000000, 0.000000000000000000, 0.000000000000000000 ) ) ;
#26222 = CARTESIAN_POINT ( 'NONE',  ( 45.83898684223488829, -38.13670450189240313, -61.12474413365445969 ) ) ;
#26223 = B_SPLINE_CURVE_WITH_KNOTS ( 'NONE', 3,
 ( #28524, #32962, #490, #44261, #16226, #241 ),
 .UNSPECIFIED., .F., .F.,
 ( 4, 2, 4 ),
 ( -0.1400863131347609980, -0.1374219544292619999, -0.1219760492225880066 ),
 .UNSPECIFIED. ) ;
#26224 = ORIENTED_EDGE ( 'NONE', *, *, #16379, .F. ) ;
#26225 = CARTESIAN_POINT ( 'NONE',  ( 57.28506249589020172, -45.82228059267649911, -26.26463383974999743 ) ) ;
#26226 = CARTESIAN_POINT ( 'NONE',  ( 9.083108146633041002, -13.20942749461869958, -43.33736317051029374 ) ) ;
#26227 = CARTESIAN_POINT ( 'NONE',  ( 53.58092488835709588, -49.39931725161739706, -49.20716744093340367 ) ) ;
#26228 = EDGE_CURVE ( 'NONE', #29727, #20782, #13557, .T. ) ;
#26229 = CARTESIAN_POINT ( 'NONE',  ( 8.831522587211491526, -16.55713555864529951, -32.14999999999999858 ) ) ;
#26230 = ADVANCED_FACE ( 'NONE', ( #14481 ), #22068, .T. ) ;
#26231 = CIRCLE ( 'NONE', #30419, 39.00000000000001421 ) ;
#26232 = DIRECTION ( 'NONE',  ( 0.000000000000000000, 0.000000000000000000, -1.000000000000000000 ) ) ;
#26233 = CARTESIAN_POINT ( 'NONE',  ( 14.15215969969850107, 19.92749982851029955, -74.54610039094001195 ) ) ;
#26234 = EDGE_CURVE ( 'NONE', #34442, #34264, #4304, .T. ) ;
#26235 = CARTESIAN_POINT ( 'NONE',  ( 23.83903834229127128, -13.54551676074863309, -51.70899580649221861 ) ) ;
#26236 = CARTESIAN_POINT ( 'NONE',  ( 44.72927470446840204, -45.40228777558419893, -7.990864045375530189 ) ) ;
#26237 = CARTESIAN_POINT ( 'NONE',  ( 52.13393739769618662, -1.166188944679350081, -65.65000000000000568 ) ) ;
#26238 = CARTESIAN_POINT ( 'NONE',  ( 14.56272227730649860, -7.522116807958889595, -64.94663746033839402 ) ) ;
#26239 = ORIENTED_EDGE ( 'NONE', *, *, #42884, .F. ) ;
#26240 = CARTESIAN_POINT ( 'NONE',  ( 55.05504109302290061, -47.02930131300339411, -25.82589578894450000 ) ) ;
#26241 = CARTESIAN_POINT ( 'NONE',  ( 55.16108428730660052, -50.93339917627999824, -75.32514449214200170 ) ) ;
#26243 = CARTESIAN_POINT ( 'NONE',  ( 41.53258628612942971, -39.71279169438616918, -78.58678531550816615 ) ) ;
#26242 = CARTESIAN_POINT ( 'NONE',  ( 1.761208164887659855, 24.33375541177040091, -11.00324065032750021 ) ) ;
#26244 = PLANE ( 'NONE',  #8786 ) ;
#26245 = DIRECTION ( 'NONE',  ( -0.6803061734058448717, -3.854301087740865499E-16, -0.7329280390501489162 ) ) ;
#26246 = AXIS2_PLACEMENT_3D ( 'NONE', #48968, #32674, #12535 ) ;
#26247 = EDGE_LOOP ( 'NONE', ( #24821, #40341, #38462, #8868 ) ) ;
#26248 = CARTESIAN_POINT ( 'NONE',  ( 12.89365889624202133, -8.399591182479161589, -80.87333339708158064 ) ) ;
#26249 = AXIS2_PLACEMENT_3D ( 'NONE', #15677, #12261, #51579 ) ;
#26250 = CARTESIAN_POINT ( 'NONE',  ( 47.38645038732749981, 23.43329625106930081, -54.85297834023369745 ) ) ;
#26251 = CARTESIAN_POINT ( 'NONE',  ( 16.79572468873124791, -7.713964170122347142, -65.31892447852293060 ) ) ;
#26252 = CARTESIAN_POINT ( 'NONE',  ( 8.223606718150689332, -15.61618413875730127, -36.50766849176289952 ) ) ;
#26253 = DIRECTION ( 'NONE',  ( 0.000000000000000000, 0.000000000000000000, 1.000000000000000000 ) ) ;
#26254 = CARTESIAN_POINT ( 'NONE',  ( 11.99500145082170022, 34.02547674131670163, -16.88883237367399914 ) ) ;
#26255 = CARTESIAN_POINT ( 'NONE',  ( 22.37291293269603898, -18.87617199571374016, -57.00054481839593734 ) ) ;
#26257 = EDGE_CURVE ( 'NONE', #22762, #33088, #9452, .T. ) ;
#26256 = CARTESIAN_POINT ( 'NONE',  ( 53.42190059089289633, 18.11830158836169957, -48.77466594534000421 ) ) ;
#26258 = CARTESIAN_POINT ( 'NONE',  ( -22.09888148991250389, 23.83340452438281076, 16.85000000000000142 ) ) ;
#26259 = CARTESIAN_POINT ( 'NONE',  ( 57.81792062896100504, -47.19274128029930182, -48.15693251440850275 ) ) ;
#26260 = CARTESIAN_POINT ( 'NONE',  ( 56.48924519203420402, 14.93416829053070138, -26.24160504693750084 ) ) ;
#26261 = FACE_OUTER_BOUND ( 'NONE', #3694, .T. ) ;
#26262 = DIRECTION ( 'NONE',  ( -0.2517544074889990768, 0.9677911542837447367, 0.000000000000000000 ) ) ;
#26263 = CARTESIAN_POINT ( 'NONE',  ( 12.30205595647329986, -64.73832649162540065, -15.96528926833489948 ) ) ;
#26264 = CARTESIAN_POINT ( 'NONE',  ( 23.04645808148667996, -19.60032511754615925, -75.67434416289975729 ) ) ;
#26265 = CARTESIAN_POINT ( 'NONE',  ( 19.78696991733798427, 23.18878466699404939, -17.61868324447104328 ) ) ;
#26266 = CARTESIAN_POINT ( 'NONE',  ( 10.77308341670910075, 32.08904557254610523, -45.20552704545990252 ) ) ;
#26267 = FACE_OUTER_BOUND ( 'NONE', #181, .T. ) ;
#26268 = CARTESIAN_POINT ( 'NONE',  ( 67.45418707017489623, -32.84195721915489941, -19.55846886189739919 ) ) ;
#26269 = ORIENTED_EDGE ( 'NONE', *, *, #17049, .F. ) ;
#26270 = CARTESIAN_POINT ( 'NONE',  ( 18.84530413485449785, 20.48963383789619996, -74.34036667011370980 ) ) ;
#26271 = ORIENTED_EDGE ( 'NONE', *, *, #23800, .T. ) ;
#26272 = ORIENTED_EDGE ( 'NONE', *, *, #9190, .F. ) ;
#26273 = AXIS2_PLACEMENT_3D ( 'NONE', #39007, #7548, #44664 ) ;
#26274 = CARTESIAN_POINT ( 'NONE',  ( 9.221498594704018004, -19.60046454519304504, -80.34100214027874642 ) ) ;
#26275 = CARTESIAN_POINT ( 'NONE',  ( 76.60792998803806597, 2.469312492038889140, -13.69250461759032866 ) ) ;
#26276 = VERTEX_POINT ( 'NONE', #26518 ) ;
#26277 = CARTESIAN_POINT ( 'NONE',  ( 11.98107198743070079, -65.17237640307759250, -46.15866685343029729 ) ) ;
#26278 = CARTESIAN_POINT ( 'NONE',  ( 57.57641373505710192, -45.19636825784430556, -25.75112877952900092 ) ) ;
#26279 = DIRECTION ( 'NONE',  ( -1.000000000000000000, 0.000000000000000000, 0.000000000000000000 ) ) ;
#26280 = CARTESIAN_POINT ( 'NONE',  ( 63.46018632244250313, 1.384447124000270035, -68.59133994763901399 ) ) ;
#26281 = ORIENTED_EDGE ( 'NONE', *, *, #22407, .T. ) ;
#26282 = CARTESIAN_POINT ( 'NONE',  ( 11.65850508138839992, 34.15500248326146959, -22.48931345404534099 ) ) ;
#26283 = CARTESIAN_POINT ( 'NONE',  ( -30.36606260230379917, 21.88381105532059934, 10.84999999999999964 ) ) ;
#26284 = CARTESIAN_POINT ( 'NONE',  ( 0.1155610841158959956, 19.94237700917059897, -35.14999985728680088 ) ) ;
#26285 = ORIENTED_EDGE ( 'NONE', *, *, #43084, .F. ) ;
#26286 = CARTESIAN_POINT ( 'NONE',  ( 54.01992009194989919, -45.20950787019129535, -14.10456388246860016 ) ) ;
#26287 = CARTESIAN_POINT ( 'NONE',  ( 51.94632098643839413, 1.634516250066370135, -19.08862713762362517 ) ) ;
#26288 = AXIS2_PLACEMENT_3D ( 'NONE', #46931, #51364, #3154 ) ;
#26289 = CARTESIAN_POINT ( 'NONE',  ( 16.50882131665489894, 19.88028741127540044, -20.29200666522829977 ) ) ;
#26290 = CARTESIAN_POINT ( 'NONE',  ( 52.68908936341578908, 18.51792035577400242, -28.15000000000000213 ) ) ;
#26291 = CARTESIAN_POINT ( 'NONE',  ( 22.90362342996845513, -15.73105605196614754, -46.45820667783088709 ) ) ;
#26292 = FACE_OUTER_BOUND ( 'NONE', #5669, .T. ) ;
#26293 = CARTESIAN_POINT ( 'NONE',  ( 47.11902681095349976, -54.23932985581029698, -75.46775895608709561 ) ) ;
#26294 = CARTESIAN_POINT ( 'NONE',  ( 45.32018539748889907, 12.59810024214380064, -5.468941159389729911 ) ) ;
#26295 = ADVANCED_FACE ( 'NONE', ( #42535 ), #2694, .T. ) ;
#26296 = CARTESIAN_POINT ( 'NONE',  ( 50.95179065742699720, 19.71850122818939965, -76.14999999969789712 ) ) ;
#26297 = CARTESIAN_POINT ( 'NONE',  ( 58.76638950021190055, 13.88377925009550040, -25.68003433735720265 ) ) ;
#26298 = CARTESIAN_POINT ( 'NONE',  ( 17.52357721215789610, -7.488974053030859501, -37.06157372594439181 ) ) ;
#26299 = VERTEX_POINT ( 'NONE', #35693 ) ;
#26300 = CARTESIAN_POINT ( 'NONE',  ( 50.15542239739440333, 21.61238791475396326, -53.37026996103012522 ) ) ;
#26301 = AXIS2_PLACEMENT_3D ( 'NONE', #33108, #45708, #45188 ) ;
#26302 = CARTESIAN_POINT ( 'NONE',  ( 7.077899642728071150, -59.90137670018390281, -12.08739966597480020 ) ) ;
#26303 = DIRECTION ( 'NONE',  ( 1.000000000000000000, 0.000000000000000000, 0.000000000000000000 ) ) ;
#26304 = DIRECTION ( 'NONE',  ( 1.000000000000000000, 0.000000000000000000, 0.000000000000000000 ) ) ;
#26305 = CARTESIAN_POINT ( 'NONE',  ( 16.13393739769620083, -15.61618894467929941, -69.65000000000000568 ) ) ;
#26306 = CARTESIAN_POINT ( 'NONE',  ( 14.06331050438567409, -7.911075405847579844, -78.92433594638590932 ) ) ;
#26307 = CARTESIAN_POINT ( 'NONE',  ( 7.492845759203720313, 29.94784237631284896, -20.13893727953968948 ) ) ;
#26308 = CARTESIAN_POINT ( 'NONE',  ( 82.27845038698740154, -45.17869114109299744, -46.87713570531570184 ) ) ;
#26309 = DIRECTION ( 'NONE',  ( 0.000000000000000000, 0.000000000000000000, -1.000000000000000000 ) ) ;
#26310 = CARTESIAN_POINT ( 'NONE',  ( 42.53933707111890783, 12.02846082064439948, -4.182107870958490459 ) ) ;
#26312 = ADVANCED_FACE ( 'NONE', ( #48006 ), #44065, .T. ) ;
#26311 = CARTESIAN_POINT ( 'NONE',  ( 65.27736602627911111, 1.383811055320669947, -70.34999999999999432 ) ) ;
#26313 = CARTESIAN_POINT ( 'NONE',  ( 57.79494562534669200, 17.81506593150905360, -51.23192195986732855 ) ) ;
#26314 = CARTESIAN_POINT ( 'NONE',  ( 24.04493739769619864, -15.61618894467929941, -32.14999999999999858 ) ) ;
#26315 = CIRCLE ( 'NONE', #18805, 2.999999999999998224 ) ;
#26316 = DIRECTION ( 'NONE',  ( 0.000000000000000000, 0.000000000000000000, -1.000000000000000000 ) ) ;
#26317 = EDGE_CURVE ( 'NONE', #39152, #20377, #29479, .T. ) ;
#26318 = B_SPLINE_CURVE_WITH_KNOTS ( 'NONE', 3,
 ( #34630, #26767, #24361, #36429, #32471, #44306, #8415, #47738, #51414, #27544, #7900, #23595, #42, #36179, #4472, #28049, #48502, #43550 ),
 .UNSPECIFIED., .F., .F.,
 ( 4, 2, 2, 2, 2, 2, 2, 2, 4 ),
 ( 0.000000000000000000, 0.06250000040831246717, 0.1250000008166249343, 0.1875000012249374015, 0.2500000016332498687, 0.3125000020415623636, 0.3750000024498748030, 0.4375000028581872424, 0.5000000032664997374 ),
 .UNSPECIFIED. ) ;
#26319 = LINE ( 'NONE', #45481, #45724 ) ;
#26320 = ORIENTED_EDGE ( 'NONE', *, *, #15491, .F. ) ;
#26321 = CARTESIAN_POINT ( 'NONE',  ( 10.32568081865999865, -20.28211327437259826, -57.85192144569249706 ) ) ;
#26322 = CARTESIAN_POINT ( 'NONE',  ( 63.43155684671108929, 1.056975075120689889, -61.93355797292380061 ) ) ;
#26323 = EDGE_LOOP ( 'NONE', ( #29381, #26847, #43821, #43377 ) ) ;
#26324 = CARTESIAN_POINT ( 'NONE',  ( 10.22105026692229046, -19.02422193446483689, -69.28615314898171107 ) ) ;
#26325 = CARTESIAN_POINT ( 'NONE',  ( 57.50723796702470025, 13.88381105532070059, -17.93019253464870033 ) ) ;
#26326 = FACE_OUTER_BOUND ( 'NONE', #19773, .T. ) ;
#26327 = DIRECTION ( 'NONE',  ( 1.964275807512749840E-11, -1.000000000000000000, -5.103645611290830066E-11 ) ) ;
#26328 = CARTESIAN_POINT ( 'NONE',  ( 45.95638572195198179, 8.859046655822801597, -57.17003146777447142 ) ) ;
#26329 = CARTESIAN_POINT ( 'NONE',  ( 10.13877654970559838, -18.94649479092700162, -81.23899999999999011 ) ) ;
#26330 = FACE_OUTER_BOUND ( 'NONE', #33841, .T. ) ;
#26331 = ORIENTED_EDGE ( 'NONE', *, *, #28953, .T. ) ;
#26332 = ORIENTED_EDGE ( 'NONE', *, *, #32904, .F. ) ;
#26333 = ORIENTED_EDGE ( 'NONE', *, *, #18025, .F. ) ;
#26334 = CARTESIAN_POINT ( 'NONE',  ( -22.65176864815480329, -19.69794255023575857, -54.65770472193846530 ) ) ;
#26335 = DIRECTION ( 'NONE',  ( 1.000000000000000000, 0.000000000000000000, 0.000000000000000000 ) ) ;
#26336 = VERTEX_POINT ( 'NONE', #12105 ) ;
#26337 = ORIENTED_EDGE ( 'NONE', *, *, #41887, .T. ) ;
#26338 = CARTESIAN_POINT ( 'NONE',  ( 23.82939211681739522, -13.74556092313518718, -77.43178944251761209 ) ) ;
#26339 = CARTESIAN_POINT ( 'NONE',  ( 53.63393739769619373, 31.88381105532059934, 16.35000000000000142 ) ) ;
#26340 = VERTEX_POINT ( 'NONE', #7912 ) ;
#26341 = CARTESIAN_POINT ( 'NONE',  ( 24.04493545821624068, -15.62192134604925897, -49.50789643335303936 ) ) ;
#26342 = CARTESIAN_POINT ( 'NONE',  ( 51.82948403312330754, -50.48701590866159705, -76.37482631807910138 ) ) ;
#26343 = CARTESIAN_POINT ( 'NONE',  ( 60.65208747370029840, 14.36635548808680163, -47.38958427977119925 ) ) ;
#26344 = CARTESIAN_POINT ( 'NONE',  ( 9.364637171664139004, -11.64588391339660056, -77.18134062521558292 ) ) ;
#26345 = CARTESIAN_POINT ( 'NONE',  ( -18.86606260230360022, -50.61618894467959962, 11.34999999999999964 ) ) ;
#26346 = FACE_OUTER_BOUND ( 'NONE', #40268, .T. ) ;
#26347 = EDGE_CURVE ( 'NONE', #44397, #27321, #11336, .T. ) ;
#26348 = CARTESIAN_POINT ( 'NONE',  ( 41.80294712679280167, -43.87265997789249639, -4.284453813682689294 ) ) ;
#26349 = CARTESIAN_POINT ( 'NONE',  ( 74.93037156228848517, -45.11618894467250129, -15.31097063366330069 ) ) ;
#26350 = CARTESIAN_POINT ( 'NONE',  ( 56.52818367932749766, 14.13713193161779991, -25.29323032974989971 ) ) ;
#26351 = CARTESIAN_POINT ( 'NONE',  ( 64.80088823274410004, 1.308647200627879981, -70.40208447574109130 ) ) ;
#26352 = CARTESIAN_POINT ( 'NONE',  ( 20.97406584291865173, -20.57336686969118489, -33.10160192024077475 ) ) ;
#26353 = CARTESIAN_POINT ( 'NONE',  ( 23.95077513244409673, -14.92063448110079982, -51.25925627687220043 ) ) ;
#26354 = VERTEX_POINT ( 'NONE', #19946 ) ;
#26355 = SURFACE_STYLE_USAGE ( .BOTH. , #50237 ) ;
#26356 = CARTESIAN_POINT ( 'NONE',  ( 57.55751162087899786, 19.38381105532060289, -53.92796738110899923 ) ) ;
#26357 = CARTESIAN_POINT ( 'NONE',  ( 44.47540486623933020, -39.99256076608075716, -64.35539580940769611 ) ) ;
#26358 = CARTESIAN_POINT ( 'NONE',  ( 22.90093739769620029, -15.61618894467913243, -28.45282021618999835 ) ) ;
#26359 = CARTESIAN_POINT ( 'NONE',  ( 21.52140218880130007, -11.27449214404849975, -32.14999999999999858 ) ) ;
#26360 = CARTESIAN_POINT ( 'NONE',  ( 63.49266932922240159, 1.386446979194299933, -68.79214934801569825 ) ) ;
#26361 = CARTESIAN_POINT ( 'NONE',  ( 47.82833025861889809, -54.39460764734859310, -54.73692062665020330 ) ) ;
#26362 = CIRCLE ( 'NONE', #29705, 13.50000000000000178 ) ;
#26363 = CARTESIAN_POINT ( 'NONE',  ( 24.04511355972104170, -15.61618909363076924, -51.79233356384455078 ) ) ;
#26364 = CARTESIAN_POINT ( 'NONE',  ( 9.572633603277138192, -13.37907996729690829, -35.95238683638561383 ) ) ;
#26365 = CARTESIAN_POINT ( 'NONE',  ( 41.53147733619440629, 13.48015055873413992, -5.331435673538858389 ) ) ;
#26366 = ADVANCED_FACE ( 'NONE', ( #11858 ), #7663, .F. ) ;
#26367 = CARTESIAN_POINT ( 'NONE',  ( 47.92670010532269487, 23.13728742016890294, -54.84775024399120014 ) ) ;
#26368 = VERTEX_POINT ( 'NONE', #28062 ) ;
#26369 = CARTESIAN_POINT ( 'NONE',  ( 13.56856140308030056, -9.046454919155269891, -78.22868061958250507 ) ) ;
#26370 = VERTEX_POINT ( 'NONE', #32236 ) ;
#26371 = CARTESIAN_POINT ( 'NONE',  ( 71.36299175555980412, 1.264791438333819906, -70.51396375885850887 ) ) ;
#26372 = CARTESIAN_POINT ( 'NONE',  ( 60.34379258661509482, -45.86802437805019395, -47.72732609191810127 ) ) ;
#26373 = CARTESIAN_POINT ( 'NONE',  ( 16.13393739769620083, -15.61618894467929941, 36.77166666666649775 ) ) ;
#26374 = CARTESIAN_POINT ( 'NONE',  ( 44.13393739769620083, 1.883811055320659955, -54.27132075603810080 ) ) ;
#26376 = CARTESIAN_POINT ( 'NONE',  ( 55.64728501505769742, 15.02354991311229959, -25.47826257345920098 ) ) ;
#26375 = CARTESIAN_POINT ( 'NONE',  ( 63.63393739769619373, -63.11618894467939356, 17.35000000000000142 ) ) ;
#26377 = CARTESIAN_POINT ( 'NONE',  ( 23.13352024345619995, -16.48128933305549992, -70.49196263479178981 ) ) ;
#26378 = CARTESIAN_POINT ( 'NONE',  ( 16.13393739769620083, -15.61618894467929941, -22.14999999999999858 ) ) ;
#26379 = CARTESIAN_POINT ( 'NONE',  ( 8.222734977135019108, -15.61599928274970139, -66.79233150823698395 ) ) ;
#26380 = CARTESIAN_POINT ( 'NONE',  ( 11.97520588862272817, -21.02746353419226821, -41.16110300765930674 ) ) ;
#26381 = B_SPLINE_SURFACE_WITH_KNOTS ( 'NONE', 1, 3, ( 
 ( #32195, #27773, #7873, #48736, #4443, #12841, #24589, #23565, #28798, #47965, #44026, #24074, #39581, #40093, #3687, #8382 ),
 ( #35649, #24332, #40600, #40348, #4186, #505, #51635, #20162, #16494, #36153, #48215, #32446, #48473, #12574, #28537, #8637 ) ),
 .UNSPECIFIED., .F., .F., .F.,
 ( 2, 2 ),
 ( 4, 2, 2, 2, 2, 2, 2, 4 ),
 ( 0.1258684489467890022, 0.9339464778236650222 ),
 ( -9.143185466370150394, -8.666071118672251217, -5.863520046276620157, -3.060968973880999755, -0.2584179014853750234, 2.544133170910249930, 5.346684243305870332, 5.524684653693860525 ),
 .UNSPECIFIED. ) ;
#26382 = VERTEX_POINT ( 'NONE', #12353 ) ;
#26383 = DIRECTION ( 'NONE',  ( 0.000000000000000000, 0.000000000000000000, 1.000000000000000000 ) ) ;
#26384 = ORIENTED_EDGE ( 'NONE', *, *, #12738, .T. ) ;
#26385 = ORIENTED_EDGE ( 'NONE', *, *, #4717, .T. ) ;
#26386 = CARTESIAN_POINT ( 'NONE',  ( 12.17681940037459931, -64.87407314697640004, -16.15032133963409677 ) ) ;
#26387 = CARTESIAN_POINT ( 'NONE',  ( 24.03024257791251372, -15.12402444006626467, -39.48786302714248109 ) ) ;
#26388 = CARTESIAN_POINT ( 'NONE',  ( 17.01977592779661919, -22.38318318947497687, -54.91115525370862827 ) ) ;
#26389 = DIRECTION ( 'NONE',  ( 0.000000000000000000, 0.000000000000000000, -1.000000000000000000 ) ) ;
#26390 = CIRCLE ( 'NONE', #27264, 1.999999999999996669 ) ;
#26391 = VERTEX_POINT ( 'NONE', #8169 ) ;
#26392 = ORIENTED_EDGE ( 'NONE', *, *, #28864, .F. ) ;
#26393 = CARTESIAN_POINT ( 'NONE',  ( -22.86606125915950116, -18.55922616655630009, -54.87897021767069106 ) ) ;
#26394 = CARTESIAN_POINT ( 'NONE',  ( 16.13393739769620083, -15.61618894467929941, -32.14999999999999858 ) ) ;
#26395 = CARTESIAN_POINT ( 'NONE',  ( 52.57474326386780206, -49.85166559037340761, -48.47378032971909789 ) ) ;
#26396 = CARTESIAN_POINT ( 'NONE',  ( 52.79235666617839939, 18.38620345821869861, -48.27343973962159396 ) ) ;
#26397 = CARTESIAN_POINT ( 'NONE',  ( 59.22263297176129981, -2.907530923697950076, -15.66492698287460072 ) ) ;
#26398 = CARTESIAN_POINT ( 'NONE',  ( 51.09074886990410391, -48.81936691653330485, -76.44262319005039785 ) ) ;
#26399 = CARTESIAN_POINT ( 'NONE',  ( 57.78985979110940008, -48.99901549808799928, -51.17840550953660284 ) ) ;
#26400 =( BOUNDED_CURVE ( )  B_SPLINE_CURVE ( 3, ( #23590, #47482, #19929, #27799 ),
 .UNSPECIFIED., .F., .T. ) 
 B_SPLINE_CURVE_WITH_KNOTS ( ( 4, 4 ),
 ( 1.570796326794895004, 2.169041209213995014 ),
 .UNSPECIFIED. ) 
 CURVE ( )  GEOMETRIC_REPRESENTATION_ITEM ( )  RATIONAL_B_SPLINE_CURVE ( ( 1.000000000000000000, 0.9703969717270899409, 0.9703969717270899409, 1.000000000000000000 ) ) 
 REPRESENTATION_ITEM ( '' )  );
#26401 = ORIENTED_EDGE ( 'NONE', *, *, #4383, .F. ) ;
#26402 = CARTESIAN_POINT ( 'NONE',  ( 14.15298794937745619, -7.924134237888455168, -33.21219548599496107 ) ) ;
#26403 = CARTESIAN_POINT ( 'NONE',  ( 68.13393739769769297, 18.72622661238300168, -73.39853292320978539 ) ) ;
#26404 = ORIENTED_EDGE ( 'NONE', *, *, #11230, .F. ) ;
#26405 = CARTESIAN_POINT ( 'NONE',  ( 16.13393739769620083, -15.61618894467929941, -15.65000000000000036 ) ) ;
#26406 = CARTESIAN_POINT ( 'NONE',  ( 55.20159258013029557, -48.56083622538359634, -48.75785604020860120 ) ) ;
#26407 = CARTESIAN_POINT ( 'NONE',  ( 20.73481432542239844, -9.258620298766089718, -47.71189826954910274 ) ) ;
#26408 = CIRCLE ( 'NONE', #48201, 20.00000000000001421 ) ;
#26409 = CARTESIAN_POINT ( 'NONE',  ( 14.13534289311499847, -51.11424938965239306, -22.31792951338179876 ) ) ;
#26410 = CARTESIAN_POINT ( 'NONE',  ( 54.95426265229980345, 19.54999294923799980, -75.77179759279050586 ) ) ;
#26411 = EDGE_CURVE ( 'NONE', #22570, #6190, #24113, .T. ) ;
#26412 = B_SPLINE_CURVE_WITH_KNOTS ( 'NONE', 3,
 ( #11489, #43198, #14631, #7291, #34792, #35317, #43449, #23495, #30851, #46619 ),
 .UNSPECIFIED., .F., .F.,
 ( 4, 1, 1, 1, 1, 1, 1, 4 ),
 ( 0.5000037738926587094, 0.5650942749437076751, 0.6443132060073258893, 0.7235321370709463240, 0.8027510681345644272, 0.8819699991981826415, 0.9611889302618030761, 1.000000000000000000 ),
 .UNSPECIFIED. ) ;
#26413 = CARTESIAN_POINT ( 'NONE',  ( 47.57068389873440140, -54.44477986132550029, -74.81178025453719727 ) ) ;
#26414 = CARTESIAN_POINT ( 'NONE',  ( 56.96608301822320186, 13.88381105532070059, -16.09650052231710404 ) ) ;
#26415 = CARTESIAN_POINT ( 'NONE',  ( -11.32734370190460105, -41.88171845330919751, -6.430192534648659475 ) ) ;
#26416 = EDGE_CURVE ( 'NONE', #51495, #32888, #39479, .T. ) ;
#26417 = FACE_OUTER_BOUND ( 'NONE', #30395, .T. ) ;
#26418 = CARTESIAN_POINT ( 'NONE',  ( 13.03996251179859911, -21.95416011689880165, -47.49173536689809794 ) ) ;
#26419 = LINE ( 'NONE', #38495, #18926 ) ;
#26420 = EDGE_CURVE ( 'NONE', #49388, #41237, #21056, .T. ) ;
#26421 = EDGE_LOOP ( 'NONE', ( #28387, #46065 ) ) ;
#26422 = CARTESIAN_POINT ( 'NONE',  ( 47.39163994235539690, 23.01787381642170160, -75.29714945969119810 ) ) ;
#26423 = CIRCLE ( 'NONE', #49058, 17.63819660112499932 ) ;
#26424 = CARTESIAN_POINT ( 'NONE',  ( 65.06933737855371191, 1.383922910988889976, -60.98106092919370269 ) ) ;
#26425 = LINE ( 'NONE', #42443, #42338 ) ;
#26426 = CARTESIAN_POINT ( 'NONE',  ( 12.04795396861086942, -65.20652679592811296, -23.72527635874608265 ) ) ;
#26427 = CARTESIAN_POINT ( 'NONE',  ( 29.06532888865359965, -4.517767789041739590, -34.89721277419619838 ) ) ;
#26428 = CIRCLE ( 'NONE', #37334, 2.000000000000000000 ) ;
#26429 = CARTESIAN_POINT ( 'NONE',  ( 53.63393739769619373, -62.11618894467930119, 17.35000000000000142 ) ) ;
#26430 = CARTESIAN_POINT ( 'NONE',  ( 82.25188034893719191, 13.88444637376409929, -46.44925509022990440 ) ) ;
#26431 = CARTESIAN_POINT ( 'NONE',  ( 0.3560139052572889873, 20.05003001002749841, -34.85296064851209508 ) ) ;
#26433 = CARTESIAN_POINT ( 'NONE',  ( 41.43972917658179256, -38.75047512967100971, -83.14010518295869190 ) ) ;
#26432 = CARTESIAN_POINT ( 'NONE',  ( 52.26504646883520167, 18.55116755685089913, -77.19463087837650050 ) ) ;
#26434 = CARTESIAN_POINT ( 'NONE',  ( 21.50885149835741572, -9.731310480211288194, -71.24312159355089591 ) ) ;
#26435 = CARTESIAN_POINT ( 'NONE',  ( 23.83903474352796437, -13.54549896641242945, -69.42433801165668683 ) ) ;
#26436 = EDGE_CURVE ( 'NONE', #48656, #43880, #48156, .T. ) ;
#26437 = CARTESIAN_POINT ( 'NONE',  ( -0.1608700869847050074, 30.41078316111070023, -48.65898601561190162 ) ) ;
#26438 = ORIENTED_EDGE ( 'NONE', *, *, #26257, .T. ) ;
#26439 = CARTESIAN_POINT ( 'NONE',  ( 53.05831035746550128, -49.54894111999600170, -48.91556382526960078 ) ) ;
#26440 = VERTEX_POINT ( 'NONE', #300 ) ;
#26441 = CARTESIAN_POINT ( 'NONE',  ( 43.11186292497671246, 8.718372030718779087, -70.65452844614090111 ) ) ;
#26442 = CIRCLE ( 'NONE', #10584, 20.00000000000001421 ) ;
#26443 = CARTESIAN_POINT ( 'NONE',  ( 18.20469938706415292, -23.32126574151624254, -74.20899818179171348 ) ) ;
#26444 = CARTESIAN_POINT ( 'NONE',  ( 14.01810477701600099, 19.82185230895960260, -22.03884457292680210 ) ) ;
#26445 = CARTESIAN_POINT ( 'NONE',  ( 57.04818975476379705, 14.01160997093949945, -25.71237456541479816 ) ) ;
#26446 = CARTESIAN_POINT ( 'NONE',  ( 21.53292167905440024, -11.07817975272370070, -40.23033096848919854 ) ) ;
#26447 = CARTESIAN_POINT ( 'NONE',  ( 50.93003901630650176, 19.69401506034679983, -76.14999999999999147 ) ) ;
#26448 = CARTESIAN_POINT ( 'NONE',  ( 53.48932715621429423, 18.18157440465409991, -49.16886947772060523 ) ) ;
#26449 = CARTESIAN_POINT ( 'NONE',  ( 55.43335310247359615, -45.81514513605549865, -16.33642346105520105 ) ) ;
#26450 = CARTESIAN_POINT ( 'NONE',  ( 16.15069188244332210, 19.81939201856824795, -15.66900176635303232 ) ) ;
#26451 = CIRCLE ( 'NONE', #38178, 2.576499999999998902 ) ;
#26452 = EDGE_LOOP ( 'NONE', ( #44454, #38415, #5707, #49060, #11982 ) ) ;
#26453 = CARTESIAN_POINT ( 'NONE',  ( 23.67750195217940146, -17.77983910020999758, -39.37641661732929776 ) ) ;
#26454 = CARTESIAN_POINT ( 'NONE',  ( 11.63826667102989987, -65.39198021057481469, -17.83149736357540149 ) ) ;
#26455 = DIRECTION ( 'NONE',  ( 0.7071067811865475727, 0.000000000000000000, 0.7071067811865475727 ) ) ;
#26456 = CARTESIAN_POINT ( 'NONE',  ( 72.76779797359338886, 1.388189907116970101, -62.58632377286669879 ) ) ;
#26457 = CARTESIAN_POINT ( 'NONE',  ( 10.98409431994489971, -65.15011576587480135, -18.15364188641290255 ) ) ;
#26458 = CARTESIAN_POINT ( 'NONE',  ( -0.4410626023037880206, -27.49517073325580085, -35.14999999999999858 ) ) ;
#26459 = CARTESIAN_POINT ( 'NONE',  ( 47.64143405400680109, 23.30250925609140111, -74.14999999999999147 ) ) ;
#26460 = CARTESIAN_POINT ( 'NONE',  ( 15.01509412889560124, -8.922449039472333254, -61.90007767931285798 ) ) ;
#26461 = EDGE_CURVE ( 'NONE', #35304, #29727, #8504, .T. ) ;
#26462 = CARTESIAN_POINT ( 'NONE',  ( 18.14859056469791554, -23.29360679183883676, -45.92611244253869529 ) ) ;
#26463 = VERTEX_POINT ( 'NONE', #27554 ) ;
#26464 = CARTESIAN_POINT ( 'NONE',  ( 64.97085660027880749, 1.369719003397489976, -70.35226930031740267 ) ) ;
#26465 = VERTEX_POINT ( 'NONE', #27813 ) ;
#26466 = CARTESIAN_POINT ( 'NONE',  ( 10.48815925059109944, -63.18736884412081167, -45.62666951642670199 ) ) ;
#26467 = DIRECTION ( 'NONE',  ( 0.000000000000000000, -1.000000000000000000, 0.000000000000000000 ) ) ;
#26468 = VERTEX_POINT ( 'NONE', #44319 ) ;
#26469 = DIRECTION ( 'NONE',  ( 0.000000000000000000, -8.281569874363147012E-12, 1.000000000000000000 ) ) ;
#26470 = CARTESIAN_POINT ( 'NONE',  ( 56.96867952315420069, 19.24372813523060088, -53.05103816797900151 ) ) ;
#26471 = CARTESIAN_POINT ( 'NONE',  ( 52.91674791423729829, 19.03363345784520178, -77.24667101748759990 ) ) ;
#26472 = EDGE_LOOP ( 'NONE', ( #28146, #26936, #15213 ) ) ;
#26473 = FACE_OUTER_BOUND ( 'NONE', #4164, .T. ) ;
#26474 = DIRECTION ( 'NONE',  ( 0.000000000000000000, 0.000000000000000000, 1.000000000000000000 ) ) ;
#26476 = CARTESIAN_POINT ( 'NONE',  ( 14.92425238142254784, 21.51730928977700685, -76.12465453342672106 ) ) ;
#26475 = AXIS2_PLACEMENT_3D ( 'NONE', #17237, #16452, #13063 ) ;
#26477 = CARTESIAN_POINT ( 'NONE',  ( 9.221383621697642141, -11.63210989131640360, -68.95899869748384958 ) ) ;
#26478 = CARTESIAN_POINT ( 'NONE',  ( 17.82813868014650183, -23.68541456244950183, -62.22645654473139842 ) ) ;
#26479 = CIRCLE ( 'NONE', #24778, 18.00000000000000355 ) ;
#26480 = CARTESIAN_POINT ( 'NONE',  ( 16.13393739769620083, -15.61618894467929941, 6.349999999999999645 ) ) ;
#26481 = CARTESIAN_POINT ( 'NONE',  ( 45.10181048658294145, -38.05446154858772445, -64.81063413519126470 ) ) ;
#26482 = ORIENTED_EDGE ( 'NONE', *, *, #24210, .F. ) ;
#26483 = CARTESIAN_POINT ( 'NONE',  ( 47.13393649688870113, -39.28050833195659663, -53.76790015415899404 ) ) ;
#26484 = CARTESIAN_POINT ( 'NONE',  ( 22.91773806209070230, -18.69624452062379660, -52.36832131176279859 ) ) ;
#26485 = CARTESIAN_POINT ( 'NONE',  ( 53.12218299100999985, -49.57312743958999590, -49.13784299743709738 ) ) ;
#26486 = AXIS2_PLACEMENT_3D ( 'NONE', #50120, #49869, #1905 ) ;
#26487 = CARTESIAN_POINT ( 'NONE',  ( 8.870425115289640061, -15.32709397560249975, -32.14999999999999858 ) ) ;
#26488 = ADVANCED_FACE ( 'NONE', ( #20453 ), #21773, .T. ) ;
#26489 = CARTESIAN_POINT ( 'NONE',  ( 9.366940089669899550, -15.31057181698914071, -61.46719675360134971 ) ) ;
#26490 = CARTESIAN_POINT ( 'NONE',  ( 13.76640160517550093, 20.38774172224130155, -75.08736963500949457 ) ) ;
#26491 = DIRECTION ( 'NONE',  ( 1.000000000000000000, 0.000000000000000000, 0.000000000000000000 ) ) ;
#26492 = CARTESIAN_POINT ( 'NONE',  ( 41.24359221735250003, -44.95166412314729598, -5.592253627833279950 ) ) ;
#26493 = CARTESIAN_POINT ( 'NONE',  ( 54.47259832750690123, 15.01994964729280113, -15.76422791930239953 ) ) ;
#26494 = CARTESIAN_POINT ( 'NONE',  ( 9.197206178375568086, -11.15923026191389944, -66.68945394373800184 ) ) ;
#26495 = ORIENTED_EDGE ( 'NONE', *, *, #28410, .F. ) ;
#26496 = CARTESIAN_POINT ( 'NONE',  ( 52.72378859808819840, -49.69239786187580421, -27.46381703610870062 ) ) ;
#26497 = AXIS2_PLACEMENT_3D ( 'NONE', #21706, #42169, #30862 ) ;
#26498 = CARTESIAN_POINT ( 'NONE',  ( 54.11678715959330077, -50.95118505024800015, -75.83232676159579455 ) ) ;
#26500 = CARTESIAN_POINT ( 'NONE',  ( 41.51070890355069309, -39.71021112747065729, -78.69265187567246755 ) ) ;
#26499 = CARTESIAN_POINT ( 'NONE',  ( 9.593021974030840227, 30.53981953105449776, -13.35990672362370013 ) ) ;
#26501 = CARTESIAN_POINT ( 'NONE',  ( 15.05440318628110141, 21.88381105532300097, -76.14999999999999147 ) ) ;
#26502 = DIRECTION ( 'NONE',  ( -1.000000000000000000, 0.000000000000000000, 0.000000000000000000 ) ) ;
#26503 = ORIENTED_EDGE ( 'NONE', *, *, #28121, .T. ) ;
#26504 = CARTESIAN_POINT ( 'NONE',  ( 14.32008737414983024, -7.878783737859143876, -80.93427853967327223 ) ) ;
#26505 = CARTESIAN_POINT ( 'NONE',  ( 47.52205594386720122, 23.34398621139530050, -54.75138854905920027 ) ) ;
#26506 = AXIS2_PLACEMENT_3D ( 'NONE', #2679, #38584, #6095 ) ;
#26507 = CARTESIAN_POINT ( 'NONE',  ( 19.85100399889286749, -8.556464285641796508, -65.44686368286718903 ) ) ;
#26508 = CARTESIAN_POINT ( 'NONE',  ( 72.33393739769618946, 1.883811055320669947, -68.84999999999999432 ) ) ;
#26509 = CARTESIAN_POINT ( 'NONE',  ( -21.36606260230379917, 30.88381105532059934, 17.35000000000000142 ) ) ;
#26510 = CARTESIAN_POINT ( 'NONE',  ( 11.70612132434609975, 33.78984264953350447, -16.54010580622759718 ) ) ;
#26511 = CARTESIAN_POINT ( 'NONE',  ( 51.81004865379589575, 18.07991840855869725, -76.98867843095119667 ) ) ;
#26512 = CARTESIAN_POINT ( 'NONE',  ( 52.83783336071989822, 18.42431077469710132, -48.61329614525410392 ) ) ;
#26513 = CARTESIAN_POINT ( 'NONE',  ( 69.63393739769620083, 11.88381105532070059, -71.50000000000000000 ) ) ;
#26514 = CARTESIAN_POINT ( 'NONE',  ( 57.34991680843397432, -50.61618894467929408, -53.92361874565386159 ) ) ;
#26515 = CARTESIAN_POINT ( 'NONE',  ( 54.99095794367999446, 16.49186176109470026, -26.61809928030959682 ) ) ;
#26516 = FACE_OUTER_BOUND ( 'NONE', #34598, .T. ) ;
#26517 = CARTESIAN_POINT ( 'NONE',  ( 11.13393739769619906, -63.50859000450320480, -43.92731420739779225 ) ) ;
#26518 = CARTESIAN_POINT ( 'NONE',  ( 20.13393739769620083, -28.89524513604070322, -84.65000000000000568 ) ) ;
#26519 = CARTESIAN_POINT ( 'NONE',  ( 46.62909198040490111, -45.11618894467940066, -7.723523852232909270 ) ) ;
#26520 = CARTESIAN_POINT ( 'NONE',  ( 71.34180821298970443, 0.9214125008369580261, -60.57945272938810177 ) ) ;
#26521 = CARTESIAN_POINT ( 'NONE',  ( 10.97902921384109831, 32.05945366115350481, -44.74278564644669842 ) ) ;
#26522 = CARTESIAN_POINT ( 'NONE',  ( 72.76657796014310975, 1.245299373075410054, -61.97143377409609855 ) ) ;
#26523 = CIRCLE ( 'NONE', #7277, 1.000000000000000888 ) ;
#26524 = ADVANCED_FACE ( 'NONE', ( #20503 ), #37261, .T. ) ;
#26525 = FACE_OUTER_BOUND ( 'NONE', #25482, .T. ) ;
#26526 = CARTESIAN_POINT ( 'NONE',  ( 12.72276870064157883, 24.23809552752231866, -75.55236793428871067 ) ) ;
#26527 = ORIENTED_EDGE ( 'NONE', *, *, #23410, .T. ) ;
#26528 = ADVANCED_FACE ( 'NONE', ( #40107 ), #1050, .T. ) ;
#26529 = VERTEX_POINT ( 'NONE', #13373 ) ;
#26530 = CARTESIAN_POINT ( 'NONE',  ( -1.266062602478600141, -15.61618894541809865, -10.44999999990159623 ) ) ;
#26531 = CARTESIAN_POINT ( 'NONE',  ( 49.34719147343828638, -2.352134976191016857, -15.70858444975636559 ) ) ;
#26532 = EDGE_LOOP ( 'NONE', ( #40785, #37949, #49647, #34851 ) ) ;
#26533 = CARTESIAN_POINT ( 'NONE',  ( 11.80055863122290027, -65.03891413853099834, -45.85802714334909780 ) ) ;
#26534 = CARTESIAN_POINT ( 'NONE',  ( 56.53807458594769741, -45.58081011514489944, -25.88778928241779909 ) ) ;
#26535 = DIRECTION ( 'NONE',  ( 0.9316796806450557966, 0.000000000000000000, 0.3632808454531109565 ) ) ;
#26536 = EDGE_CURVE ( 'NONE', #40950, #41446, #27759, .T. ) ;
#26537 = DIRECTION ( 'NONE',  ( 9.341879000000000579E-17, -6.787273000000000785E-17, 1.000000000000000000 ) ) ;
#26538 = ORIENTED_EDGE ( 'NONE', *, *, #22249, .F. ) ;
#26539 = CARTESIAN_POINT ( 'NONE',  ( 59.52869175205803032, 14.25746298374641441, -26.73578769780420572 ) ) ;
#26540 = CARTESIAN_POINT ( 'NONE',  ( 45.66610078067787981, 6.885504573898759695, -61.98917487139547688 ) ) ;
#26541 = CARTESIAN_POINT ( 'NONE',  ( 12.18056949873179917, 33.83315300093070022, -24.20126506825790003 ) ) ;
#26542 = EDGE_LOOP ( 'NONE', ( #49259, #16184, #45831, #42499, #557, #12311 ) ) ;
#26543 = CARTESIAN_POINT ( 'NONE',  ( 53.28808755247190021, -45.11618894467940066, -12.64220374931200119 ) ) ;
#26544 = FACE_OUTER_BOUND ( 'NONE', #30979, .T. ) ;
#26545 = CARTESIAN_POINT ( 'NONE',  ( 16.33846296857170088, 19.88381105367919943, -21.13414048024790048 ) ) ;
#26546 = CARTESIAN_POINT ( 'NONE',  ( 0.000000000000000000, 0.000000000000000000, 0.000000000000000000 ) ) ;
#26547 = CARTESIAN_POINT ( 'NONE',  ( 9.366926243097925209, -16.50190438893503853, -47.41114289273251359 ) ) ;
#26548 = DIRECTION ( 'NONE',  ( 0.000000000000000000, 0.000000000000000000, -1.000000000000000000 ) ) ;
#26549 = CARTESIAN_POINT ( 'NONE',  ( 47.36711723512720340, -54.66958679686550227, -74.36142533359220863 ) ) ;
#26550 = CARTESIAN_POINT ( 'NONE',  ( 64.61729235537799809, 13.73161753659590012, -11.40814173470289994 ) ) ;
#26551 = ADVANCED_FACE ( 'NONE', ( #4984 ), #12859, .T. ) ;
#26552 = CARTESIAN_POINT ( 'NONE',  ( 68.13393739769620083, -38.11618894467930119, -73.25000000000000000 ) ) ;
#26553 = B_SPLINE_SURFACE_WITH_KNOTS ( 'NONE', 3, 3, ( 
 ( #38068, #10290, #46205, #25468, #38324, #41473 ),
 ( #5589, #49617, #1645, #25726, #17635, #33603 ),
 ( #13710, #29664, #45672, #41734, #5839, #21804 ),
 ( #37811, #17884, #23596, #7390, #7137, #19936 ),
 ( #11846, #7901, #6881, #26768, #47235, #43041 ),
 ( #16019, #34895, #11326, #23089, #47739, #11584 ),
 ( #47488, #51159, #27545, #15253, #43299, #27036 ),
 ( #31206, #35926, #51667, #39108, #42784, #18912 ),
 ( #27290, #39871, #2941, #43, #10809, #30953 ),
 ( #43551, #3971, #50895, #46725, #3201, #51415 ),
 ( #46984, #38852, #19689, #3463, #22831, #14987 ) ),
 .UNSPECIFIED., .F., .F., .F.,
 ( 4, 1, 1, 1, 1, 1, 1, 1, 4 ),
 ( 4, 2, 4 ),
 ( 0.000000000000000000, 0.1250000000000000000, 0.2500000000000000000, 0.3750000000000000000, 0.5000000000000000000, 0.6250000000000000000, 0.7500000000000000000, 0.8750000000000000000, 1.000001242265009971 ),
 ( 0.5133021419581690337, 0.6217601802413029732, 0.8336663735762139815 ),
 .UNSPECIFIED. ) ;
#26554 = DIRECTION ( 'NONE',  ( 0.000000000000000000, 1.000000000000000000, 0.000000000000000000 ) ) ;
#26555 = MECHANICAL_DESIGN_GEOMETRIC_PRESENTATION_REPRESENTATION (  '', ( #32375 ), #39122 ) ;
#26556 = CARTESIAN_POINT ( 'NONE',  ( 11.63826681150182374, 34.15960232215161341, -17.83149674234766380 ) ) ;
#26557 = CARTESIAN_POINT ( 'NONE',  ( 24.34438809016150174, -16.37198001076230014, -37.53688731232609399 ) ) ;
#26558 = ORIENTED_EDGE ( 'NONE', *, *, #26608, .F. ) ;
#26559 = CARTESIAN_POINT ( 'NONE',  ( 52.92565939194879832, 18.90186872980919830, -50.10275203585430148 ) ) ;
#26560 = CARTESIAN_POINT ( 'NONE',  ( 8.120607361937230095, -62.21505069536980415, -15.66636916474939767 ) ) ;
#26561 = CARTESIAN_POINT ( 'NONE',  ( 75.47375904900299304, -35.00320737813580507, -12.36911740208540067 ) ) ;
#26562 = DIRECTION ( 'NONE',  ( 0.3863301728269261659, 0.9223605572461982538, 0.000000000000000000 ) ) ;
#26563 = DIRECTION ( 'NONE',  ( 0.000000000000000000, 0.000000000000000000, 1.000000000000000000 ) ) ;
#26564 = DIRECTION ( 'NONE',  ( 1.000000000000000000, 0.000000000000000000, 0.000000000000000000 ) ) ;
#26565 = CARTESIAN_POINT ( 'NONE',  ( 18.20463974528131601, -23.32128259539753046, -36.20899657585380993 ) ) ;
#26566 = CARTESIAN_POINT ( 'NONE',  ( 82.64666749252569389, -45.32231744321139644, -47.29311289609230329 ) ) ;
#26567 = CARTESIAN_POINT ( 'NONE',  ( 12.76333982178410054, 19.08640070912930042, -21.19734824621640001 ) ) ;
#26568 = CARTESIAN_POINT ( 'NONE',  ( 14.12259461928470117, 19.90775691817940185, -22.75706044212220291 ) ) ;
#26569 = CARTESIAN_POINT ( 'NONE',  ( 41.30230023304270048, 12.85426430236040041, -3.681965864469090022 ) ) ;
#26570 = DIRECTION ( 'NONE',  ( -1.000000000000000000, 0.000000000000000000, 0.000000000000000000 ) ) ;
#26571 = DIRECTION ( 'NONE',  ( -0.5818181818182643905, 0.000000000000000000, 0.8133188816852151559 ) ) ;
#26572 = CARTESIAN_POINT ( 'NONE',  ( 70.03247032090770574, -49.95860450174168221, -71.35146707679193412 ) ) ;
#26573 = CARTESIAN_POINT ( 'NONE',  ( 75.55177307622278704, -43.36778670056347806, -13.42519430266176528 ) ) ;
#26574 = CARTESIAN_POINT ( 'NONE',  ( 17.93421870997589807, -52.10138505899109873, -75.81674732426940011 ) ) ;
#26575 = CARTESIAN_POINT ( 'NONE',  ( 58.41816864604760440, -45.11618894467940066, -10.37988043371890079 ) ) ;
#26576 = EDGE_LOOP ( 'NONE', ( #4293, #45931, #21626, #22400, #4266, #35385 ) ) ;
#26577 = CARTESIAN_POINT ( 'NONE',  ( 18.25716822292040220, -22.75751831680320336, -55.47535351378389379 ) ) ;
#26578 = CARTESIAN_POINT ( 'NONE',  ( 63.97507082502400522, 1.443019669817199979, -61.62767282824479764 ) ) ;
#26579 = ORIENTED_EDGE ( 'NONE', *, *, #19502, .T. ) ;
#26580 = CARTESIAN_POINT ( 'NONE',  ( 17.90520935967482785, -22.20705525476682141, -68.86948548096090406 ) ) ;
#26581 = CARTESIAN_POINT ( 'NONE',  ( 61.14444386409360277, -45.63613486214899950, -47.70810082891859594 ) ) ;
#26582 = CARTESIAN_POINT ( 'NONE',  ( -30.36606260230379917, 21.88381105532059934, 16.35000000000000142 ) ) ;
#26583 = CARTESIAN_POINT ( 'NONE',  ( 16.13393739769620083, -30.04994567442000175, -34.64999999999999858 ) ) ;
#26584 = CARTESIAN_POINT ( 'NONE',  ( 9.341559668391759885, -17.31601013018309843, -81.23899999999999011 ) ) ;
#26585 = CARTESIAN_POINT ( 'NONE',  ( 10.06369629473941352, -53.99262654158863484, -34.79644414665150975 ) ) ;
#26586 = ORIENTED_EDGE ( 'NONE', *, *, #5319, .T. ) ;
#26587 = EDGE_CURVE ( 'NONE', #17335, #9073, #25243, .T. ) ;
#26588 = ORIENTED_EDGE ( 'NONE', *, *, #2060, .F. ) ;
#26589 = EDGE_LOOP ( 'NONE', ( #45115, #29769, #40069 ) ) ;
#26590 = CARTESIAN_POINT ( 'NONE',  ( 55.94726098010619353, -45.11618894467940066, -14.63509752318040036 ) ) ;
#26591 = CARTESIAN_POINT ( 'NONE',  ( 61.32820939606469324, -45.23504818669070460, -46.87279288174590164 ) ) ;
#26592 = EDGE_CURVE ( 'NONE', #17966, #39558, #21873, .T. ) ;
#26593 = DIRECTION ( 'NONE',  ( 1.000000000000000000, 0.000000000000000000, 0.000000000000000000 ) ) ;
#26594 = FACE_OUTER_BOUND ( 'NONE', #23158, .T. ) ;
#26595 = AXIS2_PLACEMENT_3D ( 'NONE', #43643, #50980, #39705 ) ;
#26596 = ORIENTED_EDGE ( 'NONE', *, *, #16917, .F. ) ;
#26597 = VERTEX_POINT ( 'NONE', #40363 ) ;
#26598 = CARTESIAN_POINT ( 'NONE',  ( 8.428860219786908914, -13.54542629176921587, -62.87566502643110766 ) ) ;
#26599 = CONICAL_SURFACE ( 'NONE', #4022, 55.50000000000000711, 1.262743545771120246 ) ;
#26600 = DIRECTION ( 'NONE',  ( 0.000000000000000000, 0.000000000000000000, -1.000000000000000000 ) ) ;
#26601 = ORIENTED_EDGE ( 'NONE', *, *, #47296, .F. ) ;
#26602 = CARTESIAN_POINT ( 'NONE',  ( 24.04345669879266723, -15.78160371113625260, -49.51431991849604231 ) ) ;
#26603 = CARTESIAN_POINT ( 'NONE',  ( 52.36927103260880045, -51.34176544043950230, -75.93037472320008874 ) ) ;
#26604 = CARTESIAN_POINT ( 'NONE',  ( 60.82331437658589834, 14.26027801509150095, -47.24344971340510568 ) ) ;
#26605 = EDGE_CURVE ( 'NONE', #34084, #7703, #5996, .T. ) ;
#26606 = DIRECTION ( 'NONE',  ( 0.000000000000000000, 0.000000000000000000, -1.000000000000000000 ) ) ;
#26607 = B_SPLINE_CURVE_WITH_KNOTS ( 'NONE', 3,
 ( #7075, #43485, #23025, #27743, #7589, #19627, #23535, #14666, #43236, #39047, #46917, #34832, #3141, #19109, #43741, #35086, #51351, #50833 ),
 .UNSPECIFIED., .F., .F.,
 ( 4, 2, 2, 2, 2, 2, 2, 2, 4 ),
 ( 0.000000000000000000, 0.4467108845949059881, 0.9572376098462268557, 1.276316813128300032, 1.435856414769340006, 1.633224234453040324, 1.949012745946970160, 2.454274364337259762, 2.552633626256600063 ),
 .UNSPECIFIED. ) ;
#26608 = EDGE_CURVE ( 'NONE', #40328, #51786, #48754, .T. ) ;
#26609 = CARTESIAN_POINT ( 'NONE',  ( 41.82061695157300818, -44.02105789449079509, -4.552229691682260437 ) ) ;
#26610 = B_SPLINE_CURVE_WITH_KNOTS ( 'NONE', 3,
 ( #26672, #30089, #30349, #6789, #41908, #22486, #38492, #49778, #33766, #18302 ),
 .UNSPECIFIED., .F., .F.,
 ( 4, 1, 1, 1, 1, 1, 1, 4 ),
 ( 0.000000000000000000, 0.03231255575895254639, 0.1115314868226600781, 0.1907504178862047817, 0.2699693489497539400, 0.3491882800134615272, 0.4284072110770061892, 0.4999975329053952255 ),
 .UNSPECIFIED. ) ;
#26611 = CARTESIAN_POINT ( 'NONE',  ( 65.24498226310142002, 0.1269486509447112499, -16.97693471835480850 ) ) ;
#26612 = CARTESIAN_POINT ( 'NONE',  ( 56.61789568001263007, 14.09242255766770491, -25.29355634365396099 ) ) ;
#26613 = CARTESIAN_POINT ( 'NONE',  ( 64.73247919242599835, 1.309849225219359869, -70.36735971887151209 ) ) ;
#26614 = CARTESIAN_POINT ( 'NONE',  ( 27.13393739769620083, -38.61618894467930119, -72.14999999999999147 ) ) ;
#26615 = FACE_OUTER_BOUND ( 'NONE', #30642, .T. ) ;
#26616 = CARTESIAN_POINT ( 'NONE',  ( 19.73361416582759986, -22.58964399566790249, -53.63582420878069001 ) ) ;
#26617 = ORIENTED_EDGE ( 'NONE', *, *, #50464, .T. ) ;
#26618 = CARTESIAN_POINT ( 'NONE',  ( 14.63048442081539946, -52.51931604725010061, -76.04695140691811162 ) ) ;
#26619 = CARTESIAN_POINT ( 'NONE',  ( 57.55751162087899786, 19.06184008987549916, -52.83558909271580006 ) ) ;
#26620 = CARTESIAN_POINT ( 'NONE',  ( 71.57216560976189612, 1.132579237369250036, -70.50812303354520338 ) ) ;
#26621 = CARTESIAN_POINT ( 'NONE',  ( 46.12376833368420392, -40.10057103694796155, -56.35806153124856621 ) ) ;
#26622 = CARTESIAN_POINT ( 'NONE',  ( 41.23393739769619515, -15.61618894467929408, 4.450000000000000178 ) ) ;
#26623 = CIRCLE ( 'NONE', #10761, 151.6440921975380434 ) ;
#26624 = CARTESIAN_POINT ( 'NONE',  ( 47.03253577542010078, -54.46635581206609800, -75.29851419728690587 ) ) ;
#26625 = CARTESIAN_POINT ( 'NONE',  ( 63.38363568028490391, 1.325841671674429900, -68.92527065596381419 ) ) ;
#26626 = CARTESIAN_POINT ( 'NONE',  ( 47.82811749538019797, -54.43775025877560836, -54.96145351061949924 ) ) ;
#26627 = CARTESIAN_POINT ( 'NONE',  ( 24.00183349690676948, -14.77473046282855584, -45.47376742038415642 ) ) ;
#26628 = CARTESIAN_POINT ( 'NONE',  ( -9.553724527077868345, -43.62474080932184251, -5.594726726022510199 ) ) ;
#26629 = CARTESIAN_POINT ( 'NONE',  ( 48.26465138126300758, 22.99219893776650281, -54.90320022043339776 ) ) ;
#26630 = ORIENTED_EDGE ( 'NONE', *, *, #46935, .F. ) ;
#26631 = CARTESIAN_POINT ( 'NONE',  ( 9.385193573649580401, -17.66485093986310062, -77.75336703320080289 ) ) ;
#26632 = ORIENTED_EDGE ( 'NONE', *, *, #37335, .F. ) ;
#26633 = CARTESIAN_POINT ( 'NONE',  ( 71.38783905025809418, 1.187237555532410171, -70.57991217294409125 ) ) ;
#26634 = CYLINDRICAL_SURFACE ( 'NONE', #40474, 6.766999999999998572 ) ;
#26635 = CARTESIAN_POINT ( 'NONE',  ( 83.49396093841654931, 14.01989379893576881, -47.52772051671507114 ) ) ;
#26636 = CARTESIAN_POINT ( 'NONE',  ( 11.30419729876839874, -10.47652263729510125, -58.10707212942319444 ) ) ;
#26637 = CARTESIAN_POINT ( 'NONE',  ( 21.00581555762000008, -20.71593030003079861, -72.71009270457319928 ) ) ;
#26638 = CARTESIAN_POINT ( 'NONE',  ( 9.438349570632869501, -17.22248095868435769, -79.77162013446428546 ) ) ;
#26639 = CARTESIAN_POINT ( 'NONE',  ( 14.06335810825438060, -7.911063077082181927, -67.20899717355162295 ) ) ;
#26640 = DIRECTION ( 'NONE',  ( 0.000000000000000000, 0.000000000000000000, -1.000000000000000000 ) ) ;
#26641 = VERTEX_POINT ( 'NONE', #44554 ) ;
#26642 = CARTESIAN_POINT ( 'NONE',  ( 51.67587649748470113, -33.96749857170579645, -77.01363636363508647 ) ) ;
#26643 = VERTEX_POINT ( 'NONE', #44813 ) ;
#26644 = EDGE_CURVE ( 'NONE', #12924, #37859, #46968, .T. ) ;
#26645 = ORIENTED_EDGE ( 'NONE', *, *, #42884, .T. ) ;
#26646 = CARTESIAN_POINT ( 'NONE',  ( 12.19720189295309964, -64.69332835163750417, -15.92873818751279913 ) ) ;
#26647 = CARTESIAN_POINT ( 'NONE',  ( 56.39253198848358295, 14.87044060624309871, -26.18964637225387193 ) ) ;
#26648 = CARTESIAN_POINT ( 'NONE',  ( 76.47316685153059268, -26.61964061097626555, -13.11179020515832150 ) ) ;
#26649 = CARTESIAN_POINT ( 'NONE',  ( 9.013808781100760115, -63.78940033112238694, -46.72196778451930044 ) ) ;
#26650 = EDGE_LOOP ( 'NONE', ( #12762, #27877, #34011, #19783 ) ) ;
#26651 = B_SPLINE_CURVE_WITH_KNOTS ( 'NONE', 3,
 ( #19306, #3329, #35288, #51286, #11714, #22959 ),
 .UNSPECIFIED., .F., .F.,
 ( 4, 2, 4 ),
 ( 0.000000000000000000, 0.3218804212953693678, 0.6437608425907387355 ),
 .UNSPECIFIED. ) ;
#26652 = ORIENTED_EDGE ( 'NONE', *, *, #43137, .F. ) ;
#26653 = LINE ( 'NONE', #31101, #47718 ) ;
#26654 = CARTESIAN_POINT ( 'NONE',  ( 83.89200044194980421, -48.61618894467930119, -53.92796738110899923 ) ) ;
#26655 = CARTESIAN_POINT ( 'NONE',  ( 48.94415371571059836, 22.39326048681330050, -54.05322516865759752 ) ) ;
#26656 = CARTESIAN_POINT ( 'NONE',  ( 61.45969919439730234, -1.272705315759670164, -16.07655046430879864 ) ) ;
#26657 = CARTESIAN_POINT ( 'NONE',  ( 51.61772101699829562, -50.35897448521090070, -76.35065455175050886 ) ) ;
#26658 = CARTESIAN_POINT ( 'NONE',  ( 60.85130813898859969, -45.50269846729229783, -47.46988763436880276 ) ) ;
#26659 = ORIENTED_EDGE ( 'NONE', *, *, #32784, .T. ) ;
#26660 = CARTESIAN_POINT ( 'NONE',  ( 23.37058690749169187, -12.35555072797064646, -33.65753852466926332 ) ) ;
#26661 = CARTESIAN_POINT ( 'NONE',  ( 76.87859648677320479, 11.88381402801379849, -14.85884684523960075 ) ) ;
#26662 = VERTEX_POINT ( 'NONE', #37728 ) ;
#26663 = PLANE ( 'NONE',  #51124 ) ;
#26664 = CIRCLE ( 'NONE', #30854, 50.00000000000000000 ) ;
#26665 = CARTESIAN_POINT ( 'NONE',  ( 50.44516630505179933, -45.11618894467940066, -10.60027150234669868 ) ) ;
#26666 = CIRCLE ( 'NONE', #16644, 39.39359268544610870 ) ;
#26667 = CARTESIAN_POINT ( 'NONE',  ( 22.14140776524460108, -10.56672883743910063, -39.79000516318719605 ) ) ;
#26668 = CARTESIAN_POINT ( 'NONE',  ( 13.20471009389370032, -50.60438166373199920, -21.36609921343159968 ) ) ;
#26669 = ADVANCED_FACE ( 'NONE', ( #21466 ), #10188, .F. ) ;
#26670 = CARTESIAN_POINT ( 'NONE',  ( 47.02070054993090054, -53.74782267376620126, -75.86501933388160523 ) ) ;
#26671 = CARTESIAN_POINT ( 'NONE',  ( 56.40060982945949775, 13.95655126064509943, -16.03711971019910010 ) ) ;
#26672 = CARTESIAN_POINT ( 'NONE',  ( 9.367432603602109609, -15.61609789975089946, -77.84717978380999170 ) ) ;
#26673 = CARTESIAN_POINT ( 'NONE',  ( 56.76664445295860872, -50.67471734267469685, -53.84360320749780016 ) ) ;
#26674 = CARTESIAN_POINT ( 'NONE',  ( 19.02084999298380197, -9.181261218463509621, -44.48141598648069106 ) ) ;
#26675 = CARTESIAN_POINT ( 'NONE',  ( 16.13393739769620083, -15.61618894467929941, -12.13039854958090125 ) ) ;
#26676 = ORIENTED_EDGE ( 'NONE', *, *, #13964, .F. ) ;
#26677 = CARTESIAN_POINT ( 'NONE',  ( 46.51664131682890257, 21.89886130434609868, -76.13722091169989881 ) ) ;
#26678 = CARTESIAN_POINT ( 'NONE',  ( 64.88003574513449223, 1.187237555532410171, -60.72008782705600538 ) ) ;
#26679 = CARTESIAN_POINT ( 'NONE',  ( 44.88827463677240104, -46.10881073926530149, -8.898903786617220035 ) ) ;
#26680 = CARTESIAN_POINT ( 'NONE',  ( 8.223201290577328848, -15.61599831009169925, -56.79233150823699816 ) ) ;
#26681 = CARTESIAN_POINT ( 'NONE',  ( 49.34439669087809932, 13.88381105532070059, -8.366249983091170961 ) ) ;
#26682 = VECTOR ( 'NONE', #27516, 1000.000000000000000 ) ;
#26683 = CARTESIAN_POINT ( 'NONE',  ( 38.67452568954060155, -33.11618894467940066, -81.65000000000000568 ) ) ;
#26684 = CARTESIAN_POINT ( 'NONE',  ( 82.13853704237929776, 13.88381105532070059, -46.42699167578030028 ) ) ;
#26685 = CARTESIAN_POINT ( 'NONE',  ( 11.19961559249191652, 34.01497085325235759, -46.39999999999999858 ) ) ;
#26687 = CARTESIAN_POINT ( 'NONE',  ( 47.13264866673830511, -38.11667935645279925, -54.63852466879949787 ) ) ;
#26686 = CARTESIAN_POINT ( 'NONE',  ( 47.62448409337466160, 23.28090871689746422, -74.50417146696477744 ) ) ;
#26688 = CARTESIAN_POINT ( 'NONE',  ( 24.04480613576765791, -15.56695444769906977, -71.50569215503726639 ) ) ;
#26689 = CARTESIAN_POINT ( 'NONE',  ( 24.04497561966918440, -15.61618908881887080, -69.50766602643473391 ) ) ;
#26690 = PRODUCT_RELATED_PRODUCT_CATEGORY ( 'part', '', ( #23918 ) ) ;
#26691 = CARTESIAN_POINT ( 'NONE',  ( 13.04555273158369921, 34.28832529259570094, -47.48197110827519651 ) ) ;
#26692 = VERTEX_POINT ( 'NONE', #46125 ) ;
#26693 = CARTESIAN_POINT ( 'NONE',  ( 53.46953806474559201, -49.34555379450520718, -48.93764703832670193 ) ) ;
#26694 = ORIENTED_EDGE ( 'NONE', *, *, #10663, .T. ) ;
#26695 = VECTOR ( 'NONE', #3177, 1000.000000000000000 ) ;
#26696 = CARTESIAN_POINT ( 'NONE',  ( 40.57483056633861196, 8.377405199161493954, -83.15256529792165452 ) ) ;
#26697 = CARTESIAN_POINT ( 'NONE',  ( 22.90149177939719749, -15.54649009578485241, -40.84390380044833080 ) ) ;
#26698 = CARTESIAN_POINT ( 'NONE',  ( 13.99298669291740183, 19.94627925521579925, -22.74639520659370007 ) ) ;
#26699 = CARTESIAN_POINT ( 'NONE',  ( 46.98749101202549383, -39.23094825485602399, -34.79644638567071269 ) ) ;
#26700 = CARTESIAN_POINT ( 'NONE',  ( 16.58402498330990227, -8.577724633346759830, -41.97314745188879215 ) ) ;
#26702 = LINE ( 'NONE', #39741, #9859 ) ;
#26701 = TOROIDAL_SURFACE ( 'NONE', #4988, 48.00000000000000000, 2.000000000000000000 ) ;
#26703 = CARTESIAN_POINT ( 'NONE',  ( 52.63212352556610085, 18.56439172932729775, -48.50958596172849724 ) ) ;
#26704 = CARTESIAN_POINT ( 'NONE',  ( 55.05621579753230321, -46.03286285214759488, -16.12183698155410028 ) ) ;
#26705 = DIRECTION ( 'NONE',  ( 0.000000000000000000, 1.000000000000000000, 0.000000000000000000 ) ) ;
#26706 = ORIENTED_EDGE ( 'NONE', *, *, #35132, .F. ) ;
#26707 = EDGE_CURVE ( 'NONE', #15849, #3072, #35456, .T. ) ;
#26708 = AXIS2_PLACEMENT_3D ( 'NONE', #43045, #43303, #19438 ) ;
#26709 = CARTESIAN_POINT ( 'NONE',  ( 23.32935734630029856, -13.68438637900169930, -80.98384931626929983 ) ) ;
#26710 = VERTEX_POINT ( 'NONE', #25391 ) ;
#26711 = EDGE_CURVE ( 'NONE', #34663, #25686, #35725, .T. ) ;
#26712 = CARTESIAN_POINT ( 'NONE',  ( 73.01642658308999501, 0.9425424353906030062, -69.13730826794480322 ) ) ;
#26713 = CARTESIAN_POINT ( 'NONE',  ( 10.99340395496080092, 33.76106700544529815, -46.99437235894899345 ) ) ;
#26714 = CARTESIAN_POINT ( 'NONE',  ( 72.82889308507860449, 1.369976237678190101, -62.46883854029779570 ) ) ;
#26715 =( BOUNDED_CURVE ( )  B_SPLINE_CURVE ( 3, ( #22137, #38403, #1462, #10109 ),
 .UNSPECIFIED., .F., .T. ) 
 B_SPLINE_CURVE_WITH_KNOTS ( ( 4, 4 ),
 ( 2.299782947909850161, 2.699475143822985146 ),
 .UNSPECIFIED. ) 
 CURVE ( )  GEOMETRIC_REPRESENTATION_ITEM ( )  RATIONAL_B_SPLINE_CURVE ( ( 1.000000000000000000, 0.9867314279001654365, 0.9867314279001654365, 1.000000000000000000 ) ) 
 REPRESENTATION_ITEM ( '' )  );
#26716 = CARTESIAN_POINT ( 'NONE',  ( 11.49998292431379987, -65.37168222854499788, -17.88621716038850096 ) ) ;
#26717 = EDGE_CURVE ( 'NONE', #49517, #9988, #42180, .T. ) ;
#26718 = CARTESIAN_POINT ( 'NONE',  ( 16.13393739769620083, -29.47259540523039689, -35.14999999999999858 ) ) ;
#26719 = CARTESIAN_POINT ( 'NONE',  ( 22.34690280317739663, -12.84547917103817305, -62.31919153057756944 ) ) ;
#26720 = CARTESIAN_POINT ( 'NONE',  ( 24.04805248749356394, -15.76022397032248179, -45.51348880828970067 ) ) ;
#26721 = EDGE_CURVE ( 'NONE', #24734, #39182, #39077, .T. ) ;
#26722 = ORIENTED_EDGE ( 'NONE', *, *, #43202, .F. ) ;
#26723 = DIRECTION ( 'NONE',  ( 0.000000000000000000, -1.000000000000000000, 0.000000000000000000 ) ) ;
#26724 = VERTEX_POINT ( 'NONE', #2606 ) ;
#26725 = CARTESIAN_POINT ( 'NONE',  ( 10.77036614487909993, -63.18183448256370127, -45.20525045113869567 ) ) ;
#26726 = CARTESIAN_POINT ( 'NONE',  ( 23.04646929297832258, -11.63207376528382753, -47.62566650700710369 ) ) ;
#26727 = VERTEX_POINT ( 'NONE', #50308 ) ;
#26728 = CARTESIAN_POINT ( 'NONE',  ( 0.2019507440921954611, -8.287282526050189446, -34.66067286864802099 ) ) ;
#26729 = CARTESIAN_POINT ( 'NONE',  ( 57.03340744182619915, 19.08153169885300215, -52.79504028237870017 ) ) ;
#26730 = CARTESIAN_POINT ( 'NONE',  ( 53.45776890000269788, 19.34146221496600049, -76.87859199860160686 ) ) ;
#26731 = ORIENTED_EDGE ( 'NONE', *, *, #20425, .F. ) ;
#26732 = CARTESIAN_POINT ( 'NONE',  ( -12.13714804906302369, -15.61618894467930119, 9.349999999999999645 ) ) ;
#26733 = CARTESIAN_POINT ( 'NONE',  ( 44.09915591415798275, 1.883883970182539835, -54.64999999999999858 ) ) ;
#26734 = CARTESIAN_POINT ( 'NONE',  ( 16.13393739769620083, -15.61618894467929941, -32.14999999999999858 ) ) ;
#26735 = CARTESIAN_POINT ( 'NONE',  ( 12.14976682726940460, -8.703687915727341462, -69.12566588673060153 ) ) ;
#26736 = CARTESIAN_POINT ( 'NONE',  ( 21.05699174304649901, -22.23028419411919998, -68.08865744343930260 ) ) ;
#26737 = CYLINDRICAL_SURFACE ( 'NONE', #49782, 16.00000000000000000 ) ;
#26738 = CARTESIAN_POINT ( 'NONE',  ( 46.93999483510361870, -38.24462483669982049, -55.61966498947037252 ) ) ;
#26739 = ORIENTED_EDGE ( 'NONE', *, *, #7620, .F. ) ;
#26740 = EDGE_CURVE ( 'NONE', #7036, #1146, #1564, .T. ) ;
#26741 = ORIENTED_EDGE ( 'NONE', *, *, #19551, .T. ) ;
#26742 = AXIS2_PLACEMENT_3D ( 'NONE', #4145, #15953, #36115 ) ;
#26743 = CIRCLE ( 'NONE', #29245, 21.96784688337769964 ) ;
#26744 = CARTESIAN_POINT ( 'NONE',  ( -22.79130321220790378, -13.38297325766516011, -54.71749000676463481 ) ) ;
#26745 = CARTESIAN_POINT ( 'NONE',  ( 12.61621733769010056, -9.048667388979911408, -51.57613200112670171 ) ) ;
#26746 = CIRCLE ( 'NONE', #51040, 0.5000000000000004441 ) ;
#26747 = CONICAL_SURFACE ( 'NONE', #37642, 0.6299999999999991163, 0.7853981633974490562 ) ;
#26748 = CARTESIAN_POINT ( 'NONE',  ( 8.873811137001389682, -15.29904210822119914, -32.14999999999999858 ) ) ;
#26749 = DIRECTION ( 'NONE',  ( 0.8857883891771956009, -0.4640893551880597712, 2.775557561562888578E-17 ) ) ;
#26750 = AXIS2_PLACEMENT_3D ( 'NONE', #39629, #3733, #19704 ) ;
#26751 = DIRECTION ( 'NONE',  ( -0.4156269377774536311, 0.5720614028176836952, 0.7071067811865477948 ) ) ;
#26752 = FACE_OUTER_BOUND ( 'NONE', #20572, .T. ) ;
#26753 = CARTESIAN_POINT ( 'NONE',  ( 41.35843174423229840, -44.86402911857589970, -5.517451181412050154 ) ) ;
#26754 = CARTESIAN_POINT ( 'NONE',  ( 17.53709516631539955, -7.809917705144554745, -61.06435815452337579 ) ) ;
#26755 = EDGE_CURVE ( 'NONE', #48585, #20803, #46590, .T. ) ;
#26756 = CARTESIAN_POINT ( 'NONE',  ( 17.44196880168159680, -23.75693673312990128, -67.95695684075599274 ) ) ;
#26757 = CARTESIAN_POINT ( 'NONE',  ( 21.14377605645180225, -21.55665859497039705, -32.14999999999999858 ) ) ;
#26758 = CARTESIAN_POINT ( 'NONE',  ( 54.73608448560249684, -51.07312271709760410, -75.36140526845879606 ) ) ;
#26760 = CARTESIAN_POINT ( 'NONE',  ( 22.90073451867936072, -15.61618922653637931, -60.45281425156898791 ) ) ;
#26759 = CARTESIAN_POINT ( 'NONE',  ( -8.972852706257611999, 12.24880239228480150, -4.689908045945220039 ) ) ;
#26761 = CARTESIAN_POINT ( 'NONE',  ( -3.866062602303799611, -15.61618894467929763, -18.58999999999999986 ) ) ;
#26762 = DIRECTION ( 'NONE',  ( -1.000000000000000000, 0.000000000000000000, 0.000000000000000000 ) ) ;
#26763 = ORIENTED_EDGE ( 'NONE', *, *, #44610, .F. ) ;
#26764 = LINE ( 'NONE', #27286, #18949 ) ;
#26765 = CARTESIAN_POINT ( 'NONE',  ( 47.82244534609320397, 23.17065945679449968, -54.75726970773219904 ) ) ;
#26766 = CARTESIAN_POINT ( 'NONE',  ( 18.39424314599772359, -8.017305291866634320, -65.38436368376463292 ) ) ;
#26767 = CARTESIAN_POINT ( 'NONE',  ( 8.222913330528481168, -16.65156021647412388, -72.75066848630076777 ) ) ;
#26768 = CARTESIAN_POINT ( 'NONE',  ( 61.00282475136230431, 14.19724498751740072, -47.27680998975259996 ) ) ;
#26769 = CARTESIAN_POINT ( 'NONE',  ( 11.94527157685780061, 34.17980222613059738, -17.48520199522390328 ) ) ;
#26770 = CARTESIAN_POINT ( 'NONE',  ( 51.50850416226409578, 17.38380873894399770, -76.79363219169579224 ) ) ;
#26771 = CARTESIAN_POINT ( 'NONE',  ( 52.90228695499589406, 18.39054173078930177, -48.72753549895890046 ) ) ;
#26772 = PLANE ( 'NONE',  #6651 ) ;
#26773 = CARTESIAN_POINT ( 'NONE',  ( 14.04950511168915206, -17.13061764721085467, -22.64999999999999858 ) ) ;
#26774 = CARTESIAN_POINT ( 'NONE',  ( 54.23599842029290130, 17.14189944890559758, -26.83793738065240220 ) ) ;
#26775 = CARTESIAN_POINT ( 'NONE',  ( 50.90601119115756745, 4.155396614399425204, -76.35101117172904139 ) ) ;
#26776 = AXIS2_PLACEMENT_3D ( 'NONE', #8833, #24783, #40792 ) ;
#26777 = EDGE_CURVE ( 'NONE', #38024, #41237, #14650, .T. ) ;
#26778 = CARTESIAN_POINT ( 'NONE',  ( 54.44538087470321130, -48.22925714520665252, -26.80321430961254947 ) ) ;
#26779 = AXIS2_PLACEMENT_3D ( 'NONE', #20541, #19785, #48610 ) ;
#26780 = CARTESIAN_POINT ( 'NONE',  ( 40.00893739769619373, -16.26570799751769769, -35.14999999999999858 ) ) ;
#26781 = CARTESIAN_POINT ( 'NONE',  ( 20.99560662150501145, -21.94236121597040068, -75.79935198058029755 ) ) ;
#26782 = CARTESIAN_POINT ( 'NONE',  ( 71.27241355379879906, 0.9209567800143640959, -60.53623002923360730 ) ) ;
#26783 = CARTESIAN_POINT ( 'NONE',  ( 10.49286768590240015, 32.07784613589559797, -45.62589547488590114 ) ) ;
#26784 = CARTESIAN_POINT ( 'NONE',  ( 72.92115325010770732, 1.229987811083100180, -62.21316185480839778 ) ) ;
#26785 = CONICAL_SURFACE ( 'NONE', #45246, 0.3230324999999999447, 0.7853981633974469467 ) ;
#26786 = VECTOR ( 'NONE', #33571, 1000.000000000000000 ) ;
#26787 = CARTESIAN_POINT ( 'NONE',  ( 66.72606212556679850, -33.11598147586919794, -20.65075273511109799 ) ) ;
#26788 = EDGE_CURVE ( 'NONE', #30697, #5671, #17554, .T. ) ;
#26789 = B_SPLINE_CURVE_WITH_KNOTS ( 'NONE', 3,
 ( #35947, #27824, #3742, #20213, #39897, #36201, #35177, #7923, #19712, #43318, #15275, #35704, #19955, #12366, #28329, #31230, #47257, #8961 ),
 .UNSPECIFIED., .F., .F.,
 ( 4, 2, 2, 2, 1, 1, 1, 1, 2, 2, 4 ),
 ( 0.4288339318601827599, 0.5716254488951695301, 0.6430212074126628874, 0.6787190866714091220, 0.6965680263007817397, 0.7054924961154681595, 0.7099547310228111474, 0.7121858484764826969, 0.7133014072033192488, 0.7144169659301558006, 1.000000000000000000 ),
 .UNSPECIFIED. ) ;
#26790 = CARTESIAN_POINT ( 'NONE',  ( 9.366809454094768839, -15.61635577034980038, -65.45282021618999124 ) ) ;
#26791 = ORIENTED_EDGE ( 'NONE', *, *, #7799, .F. ) ;
#26792 = ORIENTED_EDGE ( 'NONE', *, *, #15909, .T. ) ;
#26793 = CARTESIAN_POINT ( 'NONE',  ( 40.36721523010790236, 13.65407319109839790, -4.296538310233780855 ) ) ;
#26794 = CARTESIAN_POINT ( 'NONE',  ( 76.49291921988624665, -3.342101280679246056, -13.19690610020979982 ) ) ;
#26795 = ORIENTED_EDGE ( 'NONE', *, *, #26021, .T. ) ;
#26796 = CARTESIAN_POINT ( 'NONE',  ( 13.00893739769619906, -65.51843714052719747, -47.75434321273180416 ) ) ;
#26797 = CARTESIAN_POINT ( 'NONE',  ( 56.99279156800540136, -45.19728653190040291, -25.51108452758600009 ) ) ;
#26798 = CARTESIAN_POINT ( 'NONE',  ( 21.51003971160372785, -21.42087352377891563, -77.76985987278362700 ) ) ;
#26799 = CARTESIAN_POINT ( 'NONE',  ( 31.13393739769620083, -36.11618894467930119, -81.65000000000000568 ) ) ;
#26800 = CARTESIAN_POINT ( 'NONE',  ( 42.76911844754650360, -36.11618894467930119, -61.17703620997009750 ) ) ;
#26801 = ORIENTED_EDGE ( 'NONE', *, *, #25134, .T. ) ;
#26802 = DIRECTION ( 'NONE',  ( -1.000000000000000000, 0.000000000000000000, 0.000000000000000000 ) ) ;
#26803 = CARTESIAN_POINT ( 'NONE',  ( 43.77342226960121252, 6.654908062603587915, -71.45256550439793841 ) ) ;
#26804 = CARTESIAN_POINT ( 'NONE',  ( 41.58742287076989896, -44.81259267420119841, -5.496112453488630756 ) ) ;
#26805 = ORIENTED_EDGE ( 'NONE', *, *, #32909, .T. ) ;
#26806 = CARTESIAN_POINT ( 'NONE',  ( 21.34594057796939737, -9.227312446831069437, -37.51015005288210347 ) ) ;
#26807 = CARTESIAN_POINT ( 'NONE',  ( 51.18332209997665672, 0.4329010285075667874, -17.12802215458399857 ) ) ;
#26808 = CARTESIAN_POINT ( 'NONE',  ( 16.05644225717160012, 19.79911103497629909, -20.34167354763550151 ) ) ;
#26809 = ADVANCED_FACE ( 'NONE', ( #2085 ), #6020, .T. ) ;
#26810 = AXIS2_PLACEMENT_3D ( 'NONE', #3374, #7562, #18823 ) ;
#26811 = CARTESIAN_POINT ( 'NONE',  ( 61.02197387602029721, -29.53831944543249932, -15.95139295748569985 ) ) ;
#26812 = DIRECTION ( 'NONE',  ( -1.000000000000000000, 0.000000000000000000, 0.000000000000000000 ) ) ;
#26813 = CARTESIAN_POINT ( 'NONE',  ( 47.37032927764639822, -54.67515752274410090, -74.14999999999999147 ) ) ;
#26814 = CARTESIAN_POINT ( 'NONE',  ( 58.22650904342010136, 12.52539876674930142, -8.667039378196390587 ) ) ;
#26815 = CARTESIAN_POINT ( 'NONE',  ( 15.05440318628110141, 21.88381105532300097, -76.14999999999999147 ) ) ;
#26816 = VECTOR ( 'NONE', #40472, 1000.000000000000114 ) ;
#26817 = AXIS2_PLACEMENT_3D ( 'NONE', #20879, #40293, #24013 ) ;
#26818 = AXIS2_PLACEMENT_3D ( 'NONE', #46026, #2769, #14561 ) ;
#26819 = DIRECTION ( 'NONE',  ( 0.000000000000000000, 0.000000000000000000, 1.000000000000000000 ) ) ;
#26820 = EDGE_CURVE ( 'NONE', #16107, #45923, #31512, .T. ) ;
#26821 = CIRCLE ( 'NONE', #3386, 3.000000000000001776 ) ;
#26822 = CLOSED_SHELL ( 'NONE', ( #50283, #35053, #32791, #7406, #32201, #35946, #1826, #31457, #17743, #21638, #37154, #39328, #27267, #38463, #8800, #21755, #20971, #32546, #26056, #30161, #40326, #32043, #11295, #17321, #32854, #1759, #35238, #35826, #49633, #50865, #19076, #23761, #19850, #31168, #8236, #7570, #25400, #6274 ) ) ;
#26823 = CARTESIAN_POINT ( 'NONE',  ( 8.624584447526789432, -17.89574294739870197, -78.19369283850269881 ) ) ;
#26824 = B_SPLINE_SURFACE_WITH_KNOTS ( 'NONE', 3, 3, ( 
 ( #46510, #2461, #50167, #21849, #1952, #38641, #6405, #18703, #10598, #33645, #14264, #42045, #26035, #34153, #49664, #49911, #29708, #26296 ),
 ( #2209, #6660, #18446, #2730, #14519, #6148, #38369, #30487, #42569, #13752, #17929, #33900, #14005, #45719, #9820, #22103, #18186, #25772 ),
 ( #10338, #38114, #50430, #30232, #41779, #5883, #45983, #42306, #10076, #46249, #22364, #34419, #8701, #12637, #24653, #45635, #45119, #13420 ),
 ( #17597, #36993, #25693, #21511, #29632, #823, #9227, #12904, #37509, #17344, #40923, #13670, #25435, #37256, #45382, #33820, #5553, #49584 ),
 ( #33310, #41437, #25180, #24910, #41696, #49323, #5296, #21247, #40664, #44596, #13172, #9733, #1608, #28595, #5803, #33568, #21764, #37775 ),
 ( #1353, #32770, #17847, #28859, #8966, #29380, #9487, #1868, #4763, #1089, #20733, #17088, #16824, #36720, #48795, #49064, #44862, #5033 ),
 ( #20996, #33040, #29121, #41186, #13925, #14692, #29880, #22794, #45900, #50349, #2126, #18619, #10772, #46685, #14177, #9987, #50857, #42748 ),
 ( #18106, #34073, #43004, #26730, #3164, #14950, #49833, #6577, #18354, #38289, #10514, #19134, #30146, #25949, #34597, #41966, #6062, #30661 ),
 ( #50602, #34332, #6845, #7103, #50082, #38815, #26998, #2906, #2379, #18875, #34858, #30914, #46944, #46167, #10254, #42487, #23052, #14434 ),
 ( #11030, #30404, #26212, #22020, #39073, #38032, #42222, #6322, #22279, #46427, #26471, #22540, #38551, #2650, #4438, #23299, #51629, #11546 ) ),
 .UNSPECIFIED., .F., .F., .F.,
 ( 4, 1, 1, 1, 1, 1, 1, 4 ),
 ( 4, 2, 2, 2, 2, 2, 2, 2, 4 ),
 ( 0.000000000000000000, 0.1428571428571430157, 0.2857142857142860315, 0.4285714285714289917, 0.5714285714285709528, 0.7142857142857139685, 0.8571428571428569843, 1.000073332888519850 ),
 ( -7.333288851099999919E-05, 0.9295627158857400207, 1.472201184288379983, 1.962934912384509900, 2.208301776432569863, 2.600888758909470244, 3.229027930872510055, 3.861273708119669745, 3.925943157657540095 ),
 .UNSPECIFIED. ) ;
#26825 = EDGE_LOOP ( 'NONE', ( #7857, #19407, #13232, #33569, #19817, #956 ) ) ;
#26827 = ADVANCED_FACE ( 'NONE', ( #18313 ), #34288, .F. ) ;
#26826 = CARTESIAN_POINT ( 'NONE',  ( 68.13393739769620083, 1.383811055320669947, -65.65000000000000568 ) ) ;
#26828 = CARTESIAN_POINT ( 'NONE',  ( -6.023628976439000304, -47.42688974637729871, -6.961268883118139961 ) ) ;
#26829 = CARTESIAN_POINT ( 'NONE',  ( 76.57120089795539286, -34.85044501265049632, -13.53274818732839968 ) ) ;
#26830 = CARTESIAN_POINT ( 'NONE',  ( 75.01492932893468435, 13.86426277530698492, -15.01926194450931362 ) ) ;
#26831 = LINE ( 'NONE', #50947, #41559 ) ;
#26832 = CARTESIAN_POINT ( 'NONE',  ( 14.19855276898620033, -55.56934008872499930, -76.14999999999999147 ) ) ;
#26833 = CARTESIAN_POINT ( 'NONE',  ( 39.13393739769620083, -15.61618894467929941, -14.65000000000000036 ) ) ;
#26834 = CARTESIAN_POINT ( 'NONE',  ( 82.13853704237929776, -45.28162313823070662, -47.17417977903829751 ) ) ;
#26835 = DIRECTION ( 'NONE',  ( 0.000000000000000000, 0.000000000000000000, 1.000000000000000000 ) ) ;
#26836 = CARTESIAN_POINT ( 'NONE',  ( 41.35854804407180296, 12.82120953887990034, -3.852418314459289839 ) ) ;
#26837 = CARTESIAN_POINT ( 'NONE',  ( 61.28398356449380202, -45.60471458446119897, -47.68178229846480320 ) ) ;
#26838 = CYLINDRICAL_SURFACE ( 'NONE', #23322, 0.4999999999999982236 ) ;
#26839 = CARTESIAN_POINT ( 'NONE',  ( 67.04038824939736685, -50.70395984888217811, -72.15645085170115181 ) ) ;
#26840 = CARTESIAN_POINT ( 'NONE',  ( 75.47966807050509885, -43.37310274687460065, -13.40512917118210012 ) ) ;
#26841 = CARTESIAN_POINT ( 'NONE',  ( 18.12479075550290020, -52.38392585211880714, -75.82251062550821530 ) ) ;
#26842 = CARTESIAN_POINT ( 'NONE',  ( 52.59140206479120394, -52.14549427466430842, -53.43195377655929690 ) ) ;
#26843 = VERTEX_POINT ( 'NONE', #43468 ) ;
#26844 = EDGE_CURVE ( 'NONE', #10891, #35613, #20628, .T. ) ;
#26845 = CARTESIAN_POINT ( 'NONE',  ( 22.99909601152119976, -12.72200658253170147, -52.94034771974799725 ) ) ;
#26846 = CARTESIAN_POINT ( 'NONE',  ( 63.66432091401989624, 1.390572245144690022, -61.96641623988760017 ) ) ;
#26847 = ORIENTED_EDGE ( 'NONE', *, *, #43444, .T. ) ;
#26848 = CARTESIAN_POINT ( 'NONE',  ( -11.32734372065470119, 10.64934054434680100, -6.430561461456250072 ) ) ;
#26849 = CARTESIAN_POINT ( 'NONE',  ( 9.367299438200719308, -15.61632798465739924, -73.84717978381010539 ) ) ;
#26850 = CARTESIAN_POINT ( 'NONE',  ( 73.15787026839889506, 0.9945465939392541532, -68.91635399151641650 ) ) ;
#26851 = CARTESIAN_POINT ( 'NONE',  ( 11.97538944125683713, -10.20477556317503876, -73.74448688630067750 ) ) ;
#26852 = CARTESIAN_POINT ( 'NONE',  ( 9.945350952399207856, -18.63771621449150118, -81.23899999999999011 ) ) ;
#26853 = CARTESIAN_POINT ( 'NONE',  ( 43.99490479527259623, -45.81249226280370124, -8.084108929775279506 ) ) ;
#26854 = EDGE_CURVE ( 'NONE', #36140, #50419, #27465, .T. ) ;
#26855 = ORIENTED_EDGE ( 'NONE', *, *, #45563, .T. ) ;
#26856 = ORIENTED_EDGE ( 'NONE', *, *, #34670, .F. ) ;
#26857 = EDGE_LOOP ( 'NONE', ( #8038, #34760, #46296, #38548, #22475, #17033 ) ) ;
#26858 = CARTESIAN_POINT ( 'NONE',  ( 57.12835595156409596, -45.11618894467940066, -16.21298877816359862 ) ) ;
#26859 = CARTESIAN_POINT ( 'NONE',  ( 23.59011241424889960, -14.63756608872980003, -81.23899999999999011 ) ) ;
#26860 = AXIS2_PLACEMENT_3D ( 'NONE', #39613, #3716, #39870 ) ;
#26861 = CARTESIAN_POINT ( 'NONE',  ( 16.13393739769620083, -15.61618894467929941, -28.45282021618999835 ) ) ;
#26862 = AXIS2_PLACEMENT_3D ( 'NONE', #29630, #9485, #17086 ) ;
#26863 = ORIENTED_EDGE ( 'NONE', *, *, #9214, .F. ) ;
#26864 = CIRCLE ( 'NONE', #32669, 6.000000000000005329 ) ;
#26865 = CARTESIAN_POINT ( 'NONE',  ( 8.428836555654854124, -13.54551232982551667, -52.59100207975336616 ) ) ;
#26866 = ORIENTED_EDGE ( 'NONE', *, *, #42442, .F. ) ;
#26867 = CARTESIAN_POINT ( 'NONE',  ( 8.222948442953439852, -14.58056061358565358, -62.83399826733404581 ) ) ;
#26868 = CARTESIAN_POINT ( 'NONE',  ( 22.90093739769620029, -15.61618894467913243, -28.45282021618999835 ) ) ;
#26869 = ORIENTED_EDGE ( 'NONE', *, *, #11186, .T. ) ;
#26870 = LINE ( 'NONE', #6973, #38398 ) ;
#26871 = CARTESIAN_POINT ( 'NONE',  ( 51.62918029574790069, -50.98197525970820010, -76.14997290400350494 ) ) ;
#26872 = CARTESIAN_POINT ( 'NONE',  ( 60.51088772352670020, 14.40667547550430072, -47.25398757032650110 ) ) ;
#26873 = B_SPLINE_CURVE_WITH_KNOTS ( 'NONE', 3,
 ( #170, #11466, #15388, #8556, #15899, #8288, #16407, #39497, #11978, #15644, #24236, #20070, #31598, #36063, #32364, #7783, #48383, #44189 ),
 .UNSPECIFIED., .F., .F.,
 ( 4, 2, 2, 2, 2, 2, 2, 2, 4 ),
 ( 0.000000000000000000, 0.1250000000000077993, 0.1875000000000098532, 0.2500000000000119349, 0.3750000000000123790, 0.4375000000000107692, 0.4687500000000119349, 0.5000000000000131006, 1.000000000000000000 ),
 .UNSPECIFIED. ) ;
#26874 = DIRECTION ( 'NONE',  ( 1.000000000000000000, 0.000000000000000000, 0.000000000000000000 ) ) ;
#26875 = CARTESIAN_POINT ( 'NONE',  ( 41.67695036363830496, -43.85159771036679643, -4.028589966754839047 ) ) ;
#26876 = CARTESIAN_POINT ( 'NONE',  ( 65.03603135454920903, 1.015437840524759938, -17.83403478221330118 ) ) ;
#26877 = CARTESIAN_POINT ( 'NONE',  ( -5.339665001452960524, 15.83869399000049860, -5.053056987543070200 ) ) ;
#26878 = CARTESIAN_POINT ( 'NONE',  ( 64.70947553222160309, 1.229745425602249975, -70.44444055526530235 ) ) ;
#26879 = CARTESIAN_POINT ( 'NONE',  ( 9.735928820737651535, -18.42464518422739772, -39.71510072233680688 ) ) ;
#26880 = CARTESIAN_POINT ( 'NONE',  ( 17.74855170510530300, -51.60941532113833574, -75.47165350121125016 ) ) ;
#26881 = CARTESIAN_POINT ( 'NONE',  ( 22.08951763117189770, -10.50563004512479992, -55.06176496792589603 ) ) ;
#26882 = ORIENTED_EDGE ( 'NONE', *, *, #46527, .T. ) ;
#26884 = EDGE_CURVE ( 'NONE', #21889, #13277, #13161, .T. ) ;
#26883 = DIRECTION ( 'NONE',  ( 1.000000000000000000, 0.000000000000000000, 0.000000000000000000 ) ) ;
#26885 = CARTESIAN_POINT ( 'NONE',  ( 43.24982176573970349, 14.76832211732570244, -7.760834293533140027 ) ) ;
#26886 = CARTESIAN_POINT ( 'NONE',  ( 71.81250362359278938, 1.245299373074770122, -70.28264056245218683 ) ) ;
#26887 = EDGE_CURVE ( 'NONE', #39996, #32099, #12271, .T. ) ;
#26888 = CARTESIAN_POINT ( 'NONE',  ( 45.81018332226489065, -40.08279255246922190, -57.88043798612723378 ) ) ;
#26889 = CARTESIAN_POINT ( 'NONE',  ( 14.18385191393459976, 19.60157099775030076, -21.44137102719379939 ) ) ;
#26890 = AXIS2_PLACEMENT_3D ( 'NONE', #45287, #9128, #48441 ) ;
#26891 = AXIS2_PLACEMENT_3D ( 'NONE', #51753, #19006, #3810 ) ;
#26892 = CARTESIAN_POINT ( 'NONE',  ( 21.77064918506680158, -11.55215727437349926, -32.14999999999999858 ) ) ;
#26893 = VECTOR ( 'NONE', #51688, 1000.000000000000114 ) ;
#26894 = CARTESIAN_POINT ( 'NONE',  ( 9.044388546175500920, -19.20379739193470670, -32.35863995352835332 ) ) ;
#26895 = CARTESIAN_POINT ( 'NONE',  ( 63.23867883281550206, 0.9065823421260970072, -69.11945805671260246 ) ) ;
#26896 = CARTESIAN_POINT ( 'NONE',  ( 48.08338613907370274, -54.27467684138100168, -54.77539264028180099 ) ) ;
#26897 = CARTESIAN_POINT ( 'NONE',  ( 53.53273701459760048, 1.883811055320649963, -56.74709961107230782 ) ) ;
#26898 = CARTESIAN_POINT ( 'NONE',  ( 9.367509928541279507, -15.61618483373539767, -35.84717978380999881 ) ) ;
#26899 = CARTESIAN_POINT ( 'NONE',  ( 47.73325073025490184, 23.25446252339419928, -54.99405306332750598 ) ) ;
#26900 = ORIENTED_EDGE ( 'NONE', *, *, #33836, .T. ) ;
#26901 = CARTESIAN_POINT ( 'NONE',  ( 21.94086349853619922, -19.61895903973029931, -69.03928461620259327 ) ) ;
#26902 = VERTEX_POINT ( 'NONE', #46902 ) ;
#26903 = CARTESIAN_POINT ( 'NONE',  ( 71.48629080024771554, 0.9281439705311279598, -70.62613840402418930 ) ) ;
#26904 = FACE_OUTER_BOUND ( 'NONE', #26650, .T. ) ;
#26905 = CARTESIAN_POINT ( 'NONE',  ( 48.51115049231166410, -54.01384098269411282, -54.58190071400569110 ) ) ;
#26906 = PLANE ( 'NONE',  #17733 ) ;
#26908 = CARTESIAN_POINT ( 'NONE',  ( 44.30395658100767520, -33.11967951199632409, -51.34838756301716955 ) ) ;
#26907 = CARTESIAN_POINT ( 'NONE',  ( 84.09627682649329472, 13.28281544432810080, -47.44643906338429673 ) ) ;
#26909 = LINE ( 'NONE', #43173, #43916 ) ;
#26910 = CARTESIAN_POINT ( 'NONE',  ( 8.222962225833626349, -14.58045970421460957, -66.83399807476841659 ) ) ;
#26911 = FACE_OUTER_BOUND ( 'NONE', #50728, .T. ) ;
#26912 = EDGE_CURVE ( 'NONE', #32793, #4963, #3898, .T. ) ;
#26913 = VERTEX_POINT ( 'NONE', #3640 ) ;
#26914 = CARTESIAN_POINT ( 'NONE',  ( -15.63324371469529694, 14.93421758625839857, 16.85000000000000142 ) ) ;
#26915 = VERTEX_POINT ( 'NONE', #19610 ) ;
#26916 = ORIENTED_EDGE ( 'NONE', *, *, #48245, .T. ) ;
#26917 = CARTESIAN_POINT ( 'NONE',  ( 12.24959214048389811, -64.71630487127059439, -15.94651421640129740 ) ) ;
#26918 = CARTESIAN_POINT ( 'NONE',  ( 23.83903321696472588, -13.54549142372404447, -39.70899962327502664 ) ) ;
#26919 = CARTESIAN_POINT ( 'NONE',  ( 9.518314214286407449, -13.60873826579939205, -61.94159309563030291 ) ) ;
#26920 = CARTESIAN_POINT ( 'NONE',  ( 9.002245833509869399, -63.28624783032829271, -46.62846273742899683 ) ) ;
#26921 = AXIS2_PLACEMENT_3D ( 'NONE', #24799, #4909, #36878 ) ;
#26922 = ORIENTED_EDGE ( 'NONE', *, *, #31513, .T. ) ;
#26923 = ORIENTED_EDGE ( 'NONE', *, *, #41538, .F. ) ;
#26924 = CARTESIAN_POINT ( 'NONE',  ( 24.03381970956576552, -16.06908057521573241, -55.52589602977201366 ) ) ;
#26925 = CARTESIAN_POINT ( 'NONE',  ( 63.93393739769609141, 10.88381105532060111, -68.84999999999999432 ) ) ;
#26926 = CARTESIAN_POINT ( 'NONE',  ( 22.46011740567508852, -20.47784660952951796, -69.71600428924691073 ) ) ;
#26927 = CARTESIAN_POINT ( 'NONE',  ( 22.88833302732390251, -15.19494145161055165, -46.43300353811684289 ) ) ;
#26928 = CARTESIAN_POINT ( 'NONE',  ( 62.29142313821609633, -0.6939978288072199408, -16.33503342585539997 ) ) ;
#26929 = CARTESIAN_POINT ( 'NONE',  ( 51.54546934694510441, -48.95615870297720562, -76.80150978122190963 ) ) ;
#26930 = CARTESIAN_POINT ( 'NONE',  ( 59.09164618180179929, -48.27810260483980187, -50.59936035653869624 ) ) ;
#26931 = VECTOR ( 'NONE', #41848, 1000.000000000000000 ) ;
#26932 = ORIENTED_EDGE ( 'NONE', *, *, #51511, .F. ) ;
#26933 = CARTESIAN_POINT ( 'NONE',  ( 12.81008685434317407, -8.402044234839515013, -33.15484140419596315 ) ) ;
#26935 = CARTESIAN_POINT ( 'NONE',  ( 47.13393739769619373, -36.11618894467930119, -54.64999999999999858 ) ) ;
#26934 = VECTOR ( 'NONE', #38987, 1000.000000000000000 ) ;
#26936 = ORIENTED_EDGE ( 'NONE', *, *, #29862, .F. ) ;
#26937 = CARTESIAN_POINT ( 'NONE',  ( 17.92370450339619836, 19.88381105532299742, -76.14999999999999147 ) ) ;
#26938 = CARTESIAN_POINT ( 'NONE',  ( 23.04647257630374213, -19.60029799513142734, -53.67433770499982870 ) ) ;
#26939 = CARTESIAN_POINT ( 'NONE',  ( 9.664531381497580398, -20.05843312855249749, -48.82096330443980037 ) ) ;
#26940 = CARTESIAN_POINT ( 'NONE',  ( 13.50717251036370037, -51.04402699075219374, -21.90150652010380128 ) ) ;
#26941 = CARTESIAN_POINT ( 'NONE',  ( 57.24929532239860208, 19.38381105532069881, -74.14879648477479179 ) ) ;
#26942 = CYLINDRICAL_SURFACE ( 'NONE', #9228, 3.000000000000000444 ) ;
#26943 = CARTESIAN_POINT ( 'NONE',  ( 55.42167411747570327, 13.97341619388889988, -14.99504123111160148 ) ) ;
#26944 = CARTESIAN_POINT ( 'NONE',  ( 61.07012975457860193, -45.36121598898729701, -47.07601971527900275 ) ) ;
#26945 = CARTESIAN_POINT ( 'NONE',  ( 56.85513653747680252, -50.50737975057980123, -53.07093444070599730 ) ) ;
#26946 = CARTESIAN_POINT ( 'NONE',  ( 13.45712100228560182, -22.14131064160670093, -41.47109660606309944 ) ) ;
#26947 = CARTESIAN_POINT ( 'NONE',  ( 47.08181966212730174, -39.34878172615530190, -53.90061828279809930 ) ) ;
#26948 = ORIENTED_EDGE ( 'NONE', *, *, #12013, .T. ) ;
#26950 = EDGE_CURVE ( 'NONE', #50433, #17972, #31208, .T. ) ;
#26949 = CARTESIAN_POINT ( 'NONE',  ( 47.15730504846059290, 22.76836487247490126, -75.65554796064559184 ) ) ;
#26951 = CARTESIAN_POINT ( 'NONE',  ( 64.79174514991440503, 0.8925687589132640376, -60.66703147076970737 ) ) ;
#26952 = CARTESIAN_POINT ( 'NONE',  ( 47.64143405402000297, 23.30250925608569901, -55.14905519569659731 ) ) ;
#26953 = CARTESIAN_POINT ( 'NONE',  ( 51.13393739769659874, -50.61618894467899565, 16.21999999999999886 ) ) ;
#26954 = CARTESIAN_POINT ( 'NONE',  ( 15.09846244433525797, -7.705180183529160232, -46.96600246067505680 ) ) ;
#26955 = CYLINDRICAL_SURFACE ( 'NONE', #30605, 1.999999999999995115 ) ;
#26956 = CARTESIAN_POINT ( 'NONE',  ( 82.36129846001850296, 13.87672100883400006, -46.45437161147240346 ) ) ;
#26957 = CARTESIAN_POINT ( 'NONE',  ( -0.2606685752331820427, 19.44500263626499859, -34.99215748765989531 ) ) ;
#26959 = CARTESIAN_POINT ( 'NONE',  ( 45.52271482667700297, -37.98968692785550161, -62.69526427244640132 ) ) ;
#26958 = CARTESIAN_POINT ( 'NONE',  ( 52.91668457653215540, 19.03365523282223748, -77.24653539121042911 ) ) ;
#26960 = DIRECTION ( 'NONE',  ( 0.000000000000000000, -1.000000000000000000, 0.000000000000000000 ) ) ;
#26961 = CARTESIAN_POINT ( 'NONE',  ( 49.43322755553389669, 22.52438033512590110, -54.94234374367420060 ) ) ;
#26962 = EDGE_CURVE ( 'NONE', #6769, #39697, #3766, .T. ) ;
#26963 = ORIENTED_EDGE ( 'NONE', *, *, #4174, .T. ) ;
#26964 = AXIS2_PLACEMENT_3D ( 'NONE', #47882, #39243, #43942 ) ;
#26965 = CARTESIAN_POINT ( 'NONE',  ( 52.70437350293030221, -49.73931392293049925, -48.55297031683699771 ) ) ;
#26966 = AXIS2_PLACEMENT_3D ( 'NONE', #37945, #2298, #10687 ) ;
#26967 = ORIENTED_EDGE ( 'NONE', *, *, #24867, .F. ) ;
#26968 = CARTESIAN_POINT ( 'NONE',  ( -18.86606260230390220, 13.88381105532060289, 14.21249999999999858 ) ) ;
#26969 = CARTESIAN_POINT ( 'NONE',  ( 20.29261355638415409, -10.20487415642876350, -42.16115314179906903 ) ) ;
#26970 = CARTESIAN_POINT ( 'NONE',  ( 13.85785670643420175, 19.97506034401209973, -22.56070333950139783 ) ) ;
#26971 = CARTESIAN_POINT ( 'NONE',  ( -18.86606260230390220, 13.88381105532060289, 11.34999999999999964 ) ) ;
#26972 = CARTESIAN_POINT ( 'NONE',  ( 18.75695854933399787, -9.069256935357190130, -56.07411718121309008 ) ) ;
#26973 = CARTESIAN_POINT ( 'NONE',  ( 52.70623495221639843, 18.51481665853420111, -48.71311406155950152 ) ) ;
#26974 = CARTESIAN_POINT ( 'NONE',  ( 56.26288285225719221, -45.53040306498559886, -17.58692621438209969 ) ) ;
#26975 = ADVANCED_FACE ( 'NONE', ( #8857 ), #44751, .T. ) ;
#26976 = DIRECTION ( 'NONE',  ( 0.000000000000000000, -1.000000000000000000, 0.000000000000000000 ) ) ;
#26977 = VERTEX_POINT ( 'NONE', #45013 ) ;
#26978 = CARTESIAN_POINT ( 'NONE',  ( 11.45601973047439870, -9.315091065588880781, -38.58422730669299483 ) ) ;
#26979 = ADVANCED_FACE ( 'NONE', ( #24808 ), #9114, .T. ) ;
#26980 = B_SPLINE_CURVE_WITH_KNOTS ( 'NONE', 3,
 ( #48323, #20777, #1137, #19311, #44389, #36767, #23217, #12949, #35292, #48069, #8490, #7266 ),
 .UNSPECIFIED., .F., .F.,
 ( 4, 1, 2, 2, 1, 2, 4 ),
 ( 0.000000000000000000, 0.2500000000000280886, 0.3750000000000361933, 0.4062500000000416334, 0.4375000000000470735, 0.5000000000000446310, 1.000000000000000000 ),
 .UNSPECIFIED. ) ;
#26981 = VERTEX_POINT ( 'NONE', #48694 ) ;
#26982 = CARTESIAN_POINT ( 'NONE',  ( 72.76128204928129151, 1.388313565858570131, -68.83005089568659685 ) ) ;
#26983 = CARTESIAN_POINT ( 'NONE',  ( 9.023714487127799444, 32.18236227648780101, -46.63240982052630557 ) ) ;
#26984 = CARTESIAN_POINT ( 'NONE',  ( 72.72056432233058842, 1.396834109478120034, -62.44999999999999574 ) ) ;
#26985 = B_SPLINE_CURVE_WITH_KNOTS ( 'NONE', 3,
 ( #13286, #29239, #3937, #40087, #27507, #47451, #7350, #11804, #19394, #23559, #20856, #35375, #51373, #7611, #39574, #43762, #7864, #23812, #39831, #19897, #958, #16955, #48932, #26338, #25813, #46029, #22409, #41563, #22145, #45767, #30274, #1994, #5678, #37630, #45510, #18229 ),
 .UNSPECIFIED., .F., .F.,
 ( 4, 2, 2, 2, 2, 2, 2, 2, 2, 2, 2, 2, 2, 2, 1, 1, 1, 1, 2, 4 ),
 ( 0.000000000000000000, 0.06250043248147645059, 0.1250008649629529012, 0.1875012974444293379, 0.2500017299259058023, 0.2812519461666440068, 0.3125021624073822668, 0.3437523786481204713, 0.3750025948888586758, 0.4062528111295969357, 0.4375030273703351402, 0.4687532436110734002, 0.4843783517314425580, 0.4921909057916271646, 0.4960971828217194401, 0.4980503213367655224, 0.4990268905942885080, 0.4995151752230500564, 0.4997593175374308583, 0.5000034598518116047 ),
 .UNSPECIFIED. ) ;
#26986 = CARTESIAN_POINT ( 'NONE',  ( 53.52964967199919499, -49.40236756415160357, -49.18086210135690095 ) ) ;
#26987 = CARTESIAN_POINT ( 'NONE',  ( 52.88388587306728539, -49.67261804826031835, -49.00306437247584768 ) ) ;
#26988 = DIRECTION ( 'NONE',  ( 0.000000000000000000, 0.000000000000000000, -1.000000000000000000 ) ) ;
#26989 = CARTESIAN_POINT ( 'NONE',  ( 50.33545347434720441, -53.26974486897529459, -54.25199063940150523 ) ) ;
#26990 = ORIENTED_EDGE ( 'NONE', *, *, #40051, .T. ) ;
#26991 = CARTESIAN_POINT ( 'NONE',  ( 61.43314648866955707, 14.21603639159006427, -47.47826202051524547 ) ) ;
#26992 = EDGE_LOOP ( 'NONE', ( #28200, #16162, #36206, #36050, #41075, #7954 ) ) ;
#26993 = CARTESIAN_POINT ( 'NONE',  ( 10.48935662701619975, -63.21776614012360085, -45.62600156124040041 ) ) ;
#26994 = CARTESIAN_POINT ( 'NONE',  ( 70.03247032090601465, 18.72622661238470343, -69.60146707679315625 ) ) ;
#26995 = VERTEX_POINT ( 'NONE', #37151 ) ;
#26996 = CARTESIAN_POINT ( 'NONE',  ( 13.36500334305701365, -23.09455901958340007, -44.40493357439147815 ) ) ;
#26997 = CARTESIAN_POINT ( 'NONE',  ( 57.34839258692319675, 19.00579764154129592, -52.73846305600119422 ) ) ;
#26998 = CARTESIAN_POINT ( 'NONE',  ( 53.19378594384949821, 19.20558095012749789, -77.11066260656291149 ) ) ;
#26999 = ORIENTED_EDGE ( 'NONE', *, *, #27532, .T. ) ;
#27000 = CARTESIAN_POINT ( 'NONE',  ( 10.23245084088046220, -64.79111536330883325, -47.03631046558128759 ) ) ;
#27001 = CARTESIAN_POINT ( 'NONE',  ( 11.67619942398430055, 33.65927571709689659, -45.08494251881550241 ) ) ;
#27002 = CARTESIAN_POINT ( 'NONE',  ( 83.62039307877681438, -44.54160141935248163, -46.55140768024734399 ) ) ;
#27003 = CARTESIAN_POINT ( 'NONE',  ( 22.46009313275346742, -10.75449796053407603, -69.58400065715915161 ) ) ;
#27004 = CARTESIAN_POINT ( 'NONE',  ( 17.24925778731569892, -7.446808277551939526, -63.33552157962218843 ) ) ;
#27005 = CARTESIAN_POINT ( 'NONE',  ( 57.55751162049570269, -50.61618894467930119, -53.92796738110899923 ) ) ;
#27006 = CARTESIAN_POINT ( 'NONE',  ( 46.24251708701347496, -38.17788423405144727, -59.10706492824460412 ) ) ;
#27007 = ORIENTED_EDGE ( 'NONE', *, *, #21797, .F. ) ;
#27008 = ORIENTED_EDGE ( 'NONE', *, *, #49823, .F. ) ;
#27009 = AXIS2_PLACEMENT_3D ( 'NONE', #20995, #24909, #36457 ) ;
#27010 = DIRECTION ( 'NONE',  ( 0.000000000000000000, 1.000000000000000000, 0.000000000000000000 ) ) ;
#27011 = CARTESIAN_POINT ( 'NONE',  ( 18.59482207321979885, -22.64831098705879953, -50.62550482836319787 ) ) ;
#27012 = AXIS2_PLACEMENT_3D ( 'NONE', #21188, #41633, #34013 ) ;
#27013 = CARTESIAN_POINT ( 'NONE',  ( 53.23850466849069818, -49.52901910977939792, -49.17578823945770239 ) ) ;
#27014 = CARTESIAN_POINT ( 'NONE',  ( 50.44542158146659716, 13.88381105532070059, -10.59990841316350085 ) ) ;
#27015 = LINE ( 'NONE', #31185, #6961 ) ;
#27017 = EDGE_CURVE ( 'NONE', #49799, #17454, #12270, .T. ) ;
#27016 = CARTESIAN_POINT ( 'NONE',  ( 16.13393739769620083, -15.61618894467929941, -18.58999999999999986 ) ) ;
#27018 = CYLINDRICAL_SURFACE ( 'NONE', #33182, 2.999999999999999112 ) ;
#27019 = CARTESIAN_POINT ( 'NONE',  ( 12.14166061495670057, 33.87333292297899590, -16.52221827437060142 ) ) ;
#27020 = CARTESIAN_POINT ( 'NONE',  ( 23.53364714576019878, -11.97929241695389990, -63.36225883906600131 ) ) ;
#27021 = CARTESIAN_POINT ( 'NONE',  ( 55.69969381902829753, -46.18869917138589898, -25.38063810554809763 ) ) ;
#27022 = CIRCLE ( 'NONE', #31192, 0.4999999999999865663 ) ;
#27023 = CARTESIAN_POINT ( 'NONE',  ( 53.82407901297139574, -51.23529577529289725, -75.59334556761540114 ) ) ;
#27025 = CARTESIAN_POINT ( 'NONE',  ( 8.223487313465298598, -15.61606829411550024, -62.50766849176299189 ) ) ;
#27024 = CARTESIAN_POINT ( 'NONE',  ( -7.134180881003870489, 15.03340159476780080, -6.707190621226460259 ) ) ;
#27026 = DIRECTION ( 'NONE',  ( 0.8732394366197160362, -0.4872913772396150756, 0.000000000000000000 ) ) ;
#27027 = DIRECTION ( 'NONE',  ( 0.000000000000000000, 0.000000000000000000, 1.000000000000000000 ) ) ;
#27028 = ORIENTED_EDGE ( 'NONE', *, *, #18404, .F. ) ;
#27029 =( BOUNDED_CURVE ( )  B_SPLINE_CURVE ( 3, ( #28732, #49710, #29251, #33179 ),
 .UNSPECIFIED., .F., .T. ) 
 B_SPLINE_CURVE_WITH_KNOTS ( ( 4, 4 ),
 ( 4.862900663153626013, 4.999863811009007009 ),
 .UNSPECIFIED. ) 
 CURVE ( )  GEOMETRIC_REPRESENTATION_ITEM ( )  RATIONAL_B_SPLINE_CURVE ( ( 1.000000000000000000, 0.9984373688466792185, 0.9984373688466792185, 1.000000000000000000 ) ) 
 REPRESENTATION_ITEM ( '' )  );
#27030 = CARTESIAN_POINT ( 'NONE',  ( -9.553724527302819070, -43.62474080911430008, -5.594726724945660479 ) ) ;
#27031 = B_SPLINE_CURVE_WITH_KNOTS ( 'NONE', 3,
 ( #24666, #48813, #582, #332, #48040, #25196, #41202, #17105, #44354, #40681, #16837, #13187, #4513, #8459, #5311, #1372, #20232, #48550 ),
 .UNSPECIFIED., .F., .F.,
 ( 4, 2, 2, 2, 2, 2, 2, 2, 4 ),
 ( -2.552633636494849867, -2.454247488323869852, -1.948999206626869984, -1.633219030566239960, -1.435856420528349942, -1.276316818247430041, -0.9572376136855691442, -0.4467108863865978385, 2.220446049250313081E-15 ),
 .UNSPECIFIED. ) ;
#27032 = CARTESIAN_POINT ( 'NONE',  ( 47.62602275188279322, 23.28642693250159823, -54.79164112689819888 ) ) ;
#27033 = EDGE_CURVE ( 'NONE', #45554, #40162, #46290, .T. ) ;
#27034 = DIRECTION ( 'NONE',  ( 0.000000000000000000, -1.000000000000000000, 0.000000000000000000 ) ) ;
#27035 = CARTESIAN_POINT ( 'NONE',  ( 84.44421850428412313, -43.32357619328593756, -47.46023813354324261 ) ) ;
#27036 = CARTESIAN_POINT ( 'NONE',  ( 60.92599952699959687, 14.37113304530450009, -47.62103037817029616 ) ) ;
#27037 = CARTESIAN_POINT ( 'NONE',  ( 11.41186166766810040, 33.90528444067879832, -17.00495033411830192 ) ) ;
#27038 = CARTESIAN_POINT ( 'NONE',  ( 51.37477221945899686, 17.86423695781330068, -76.61256277725719599 ) ) ;
#27039 = CARTESIAN_POINT ( 'NONE',  ( 52.82466266506040142, 18.43121127117079894, -48.56034107118879461 ) ) ;
#27040 = FACE_OUTER_BOUND ( 'NONE', #16445, .T. ) ;
#27041 = CARTESIAN_POINT ( 'NONE',  ( -0.2905447780693382609, -45.37728495500358861, -35.01965454424513524 ) ) ;
#27042 = CARTESIAN_POINT ( 'NONE',  ( 56.45717822463519298, 14.96703538239720110, -26.24611782501470003 ) ) ;
#27043 = CARTESIAN_POINT ( 'NONE',  ( 47.13393739769619373, -38.26167638829240047, -54.64999999999999858 ) ) ;
#27044 = EDGE_CURVE ( 'NONE', #8290, #51304, #25644, .T. ) ;
#27045 = CIRCLE ( 'NONE', #17848, 17.39999999999999503 ) ;
#27046 = CARTESIAN_POINT ( 'NONE',  ( 24.04493739429386068, -14.58063990169072177, -37.75066784073908366 ) ) ;
#27047 = CARTESIAN_POINT ( 'NONE',  ( 52.97667581671070280, 18.39974466412820320, -49.06651679849090186 ) ) ;
#27048 = CARTESIAN_POINT ( 'NONE',  ( 60.49441524024199879, -30.20409861275970087, -16.10365693432350298 ) ) ;
#27049 = CARTESIAN_POINT ( 'NONE',  ( 71.41555540048999262, 0.9948723650351710690, -60.63592931576840073 ) ) ;
#27050 = CARTESIAN_POINT ( 'NONE',  ( 11.13393739769619906, 32.06339680888989818, -43.91522882996569166 ) ) ;
#27051 = CARTESIAN_POINT ( 'NONE',  ( 72.36601468635269896, 1.348268854479560019, -61.55068500424459899 ) ) ;
#27052 = CARTESIAN_POINT ( 'NONE',  ( 50.96897961697546009, -35.27620091889338028, -76.38407851794919168 ) ) ;
#27053 = CARTESIAN_POINT ( 'NONE',  ( 16.13393739769620083, -45.61618894467940066, -62.64999999999999858 ) ) ;
#27054 = VERTEX_POINT ( 'NONE', #30755 ) ;
#27055 = ORIENTED_EDGE ( 'NONE', *, *, #49812, .T. ) ;
#27056 = CARTESIAN_POINT ( 'NONE',  ( 49.75284640906040323, 26.72485768586289723, -54.55457994667449384 ) ) ;
#27057 = CARTESIAN_POINT ( 'NONE',  ( 50.02561910228128284, -1.340710577923809987, -15.97583675998615149 ) ) ;
#27058 = ORIENTED_EDGE ( 'NONE', *, *, #41234, .F. ) ;
#27059 = CARTESIAN_POINT ( 'NONE',  ( 55.93374749697019865, -46.01427663227649845, -25.74332633017289851 ) ) ;
#27060 = FACE_OUTER_BOUND ( 'NONE', #20335, .T. ) ;
#27061 = CARTESIAN_POINT ( 'NONE',  ( 63.44650199127489998, 1.383928098097870096, -68.54761322559109260 ) ) ;
#27062 = ORIENTED_EDGE ( 'NONE', *, *, #31393, .F. ) ;
#27063 = CARTESIAN_POINT ( 'NONE',  ( -8.923813801541088608, 7.426280886100511403, -42.52630539064124093 ) ) ;
#27064 = CARTESIAN_POINT ( 'NONE',  ( 43.00594420470828538, 6.546349551758413376, -75.28996588853145511 ) ) ;
#27065 = CARTESIAN_POINT ( 'NONE',  ( 41.84490955069979634, -44.86154966424449952, -5.635703470643719903 ) ) ;
#27066 = VERTEX_POINT ( 'NONE', #14785 ) ;
#27067 = CARTESIAN_POINT ( 'NONE',  ( 20.72701976924740208, -9.175108652667299580, -31.48951129204709787 ) ) ;
#27068 = AXIS2_PLACEMENT_3D ( 'NONE', #12195, #11948, #19536 ) ;
#27069 = CARTESIAN_POINT ( 'NONE',  ( 52.10267379959660161, 1.883811054221469883, -20.65000000000000213 ) ) ;
#27070 = CARTESIAN_POINT ( 'NONE',  ( 23.36114490013733658, -18.93483993365045137, -49.92920886125001090 ) ) ;
#27071 =( NAMED_UNIT ( * ) SI_UNIT ( $, .STERADIAN. ) SOLID_ANGLE_UNIT ( ) );
#27072 = CARTESIAN_POINT ( 'NONE',  ( 59.16200396169190157, -28.35957559346910273, -15.65933892576900099 ) ) ;
#27073 = CARTESIAN_POINT ( 'NONE',  ( 63.03407832914049891, 0.8840451408750739093, -62.48896739026420022 ) ) ;
#27074 = CARTESIAN_POINT ( 'NONE',  ( 47.15818641045569848, -54.58383002653739879, -75.00633330157590706 ) ) ;
#27075 = CARTESIAN_POINT ( 'NONE',  ( 46.47536507427530239, -40.11920440292289669, -54.64999999999999858 ) ) ;
#27076 = EDGE_CURVE ( 'NONE', #4059, #46792, #36223, .T. ) ;
#27077 = DIRECTION ( 'NONE',  ( 0.000000000000000000, 0.000000000000000000, -1.000000000000000000 ) ) ;
#27078 = CIRCLE ( 'NONE', #33767, 5.499999999999998224 ) ;
#27079 = B_SPLINE_CURVE_WITH_KNOTS ( 'NONE', 3,
 ( #3741, #31734, #40142, #7922, #15780, #8695, #39896, #48789, #4757, #27564, #23872, #23617, #43572, #39636, #40658, #8179, #28328, #20726 ),
 .UNSPECIFIED., .F., .F.,
 ( 4, 2, 2, 2, 2, 2, 2, 2, 4 ),
 ( 0.5000000031318456717, 0.5625000027403649350, 0.6250000023488841983, 0.6875000019574033505, 0.7500000015659226138, 0.8125000011744419881, 0.8750000007829612514, 0.9375000003914806257, 1.000000000000000000 ),
 .UNSPECIFIED. ) ;
#27080 = ADVANCED_FACE ( 'NONE', ( #30497 ), #47457, .F. ) ;
#27081 = AXIS2_PLACEMENT_3D ( 'NONE', #41239, #5351, #21305 ) ;
#27082 = CARTESIAN_POINT ( 'NONE',  ( 84.43354761919439966, -43.30556812193899674, -47.41425570151039892 ) ) ;
#27083 = CARTESIAN_POINT ( 'NONE',  ( 61.47394622263419706, 13.88380263855350094, -27.27040111922170240 ) ) ;
#27084 = ADVANCED_FACE ( 'NONE', ( #34687 ), #33198, .T. ) ;
#27085 = CARTESIAN_POINT ( 'NONE',  ( 13.27943376031980094, -8.306020878940559626, -78.66900642488428730 ) ) ;
#27086 = ORIENTED_EDGE ( 'NONE', *, *, #36261, .F. ) ;
#27087 = DIRECTION ( 'NONE',  ( 1.000000000000000000, 0.000000000000000000, 0.000000000000000000 ) ) ;
#27088 = CARTESIAN_POINT ( 'NONE',  ( 10.81351130465269961, -63.69219886199940817, -15.12224224647750148 ) ) ;
#27089 = CARTESIAN_POINT ( 'NONE',  ( 76.55459068199429851, 0.4406365421732439946, -13.46266660724949915 ) ) ;
#27090 = CARTESIAN_POINT ( 'NONE',  ( 75.26896404091627346, 13.46709405488641309, -14.13654111410380665 ) ) ;
#27091 = DIRECTION ( 'NONE',  ( 9.341879000000000579E-17, -6.787273000000000785E-17, 1.000000000000000000 ) ) ;
#27092 = DIRECTION ( 'NONE',  ( 0.000000000000000000, 0.000000000000000000, -1.000000000000000000 ) ) ;
#27093 = CARTESIAN_POINT ( 'NONE',  ( 12.84688943576596643, 20.36144273378011249, -21.73578643762688856 ) ) ;
#27094 = CARTESIAN_POINT ( 'NONE',  ( 63.00666467042349694, 0.8838110553206759423, -62.53374032209040223 ) ) ;
#27095 = CARTESIAN_POINT ( 'NONE',  ( 13.05742136612449933, 19.08961680411999851, -21.18088012638509809 ) ) ;
#27096 = CARTESIAN_POINT ( 'NONE',  ( 57.29642382700900072, -50.59336727787100330, -53.60300200697109574 ) ) ;
#27097 = CARTESIAN_POINT ( 'NONE',  ( 41.14792778566190634, 13.00557415106479908, -3.958129196103689296 ) ) ;
#27098 = CARTESIAN_POINT ( 'NONE',  ( 18.86789271228509790, -51.78678246903520233, -74.14999999999999147 ) ) ;
#27099 = DIRECTION ( 'NONE',  ( 0.000000000000000000, 0.000000000000000000, 1.000000000000000000 ) ) ;
#27100 = LINE ( 'NONE', #7964, #20870 ) ;
#27101 = CARTESIAN_POINT ( 'NONE',  ( 65.43393739769578588, -48.11618894467640217, -73.25000000000000000 ) ) ;
#27102 = CIRCLE ( 'NONE', #27946, 1.000000000000000000 ) ;
#27103 = CARTESIAN_POINT ( 'NONE',  ( 67.94624738391060248, -1.132776823338670136, -17.85820666156480030 ) ) ;
#27104 = CARTESIAN_POINT ( 'NONE',  ( 17.77815508849479897, -51.52596624575240725, -75.36996982820370761 ) ) ;
#27106 = EDGE_CURVE ( 'NONE', #26902, #8993, #26831, .T. ) ;
#27105 = CARTESIAN_POINT ( 'NONE',  ( 63.36072709640390599, -45.11618894467940066, -12.04575099730080012 ) ) ;
#27107 = CARTESIAN_POINT ( 'NONE',  ( 19.66348914187359753, -9.055018407075850817, -66.72444172481779390 ) ) ;
#27108 = CARTESIAN_POINT ( 'NONE',  ( 63.60923929913089836, 1.000506532485009981, -61.70853630543769697 ) ) ;
#27109 = ORIENTED_EDGE ( 'NONE', *, *, #14346, .T. ) ;
#27110 = CARTESIAN_POINT ( 'NONE',  ( 8.949719927774120620, 31.88305279702909800, -46.63538165998269847 ) ) ;
#27111 = CARTESIAN_POINT ( 'NONE',  ( 64.43393739769619799, 11.38381105532070059, -62.44999999999999574 ) ) ;
#27112 = CARTESIAN_POINT ( 'NONE',  ( 73.15966969277990017, 1.196343736543249880, -68.73232403594570883 ) ) ;
#27113 = CARTESIAN_POINT ( 'NONE',  ( 45.41100509400894936, 8.825660103508100818, -59.81845664609551250 ) ) ;
#27114 = CARTESIAN_POINT ( 'NONE',  ( 10.58153729635829876, -19.54390142674099806, -81.23899999999999011 ) ) ;
#27115 = CARTESIAN_POINT ( 'NONE',  ( 40.73312973959730243, -45.28955000209560211, -5.671162506903860034 ) ) ;
#27116 = ORIENTED_EDGE ( 'NONE', *, *, #6563, .T. ) ;
#27117 = CARTESIAN_POINT ( 'NONE',  ( 17.72121729522119793, 20.57774151326000123, -75.67041253543310120 ) ) ;
#27118 = VERTEX_POINT ( 'NONE', #42054 ) ;
#27119 = ORIENTED_EDGE ( 'NONE', *, *, #26411, .T. ) ;
#27120 = ORIENTED_EDGE ( 'NONE', *, *, #9652, .F. ) ;
#27121 = DIRECTION ( 'NONE',  ( 1.000000000000000000, 0.000000000000000000, 0.000000000000000000 ) ) ;
#27122 = CARTESIAN_POINT ( 'NONE',  ( 23.08642316010210038, -12.32642676488089961, -81.23899999999999011 ) ) ;
#27123 = AXIS2_PLACEMENT_3D ( 'NONE', #42972, #27982, #35609 ) ;
#27124 = DIRECTION ( 'NONE',  ( -0.3502816565540429750, 0.000000000000000000, 0.9366444154970205993 ) ) ;
#27125 = ADVANCED_FACE ( 'NONE', ( #42839 ), #29018, .T. ) ;
#27126 = ORIENTED_EDGE ( 'NONE', *, *, #10833, .T. ) ;
#27127 = CARTESIAN_POINT ( 'NONE',  ( 19.31296351478369999, -49.88685839599860117, -82.14319696191608955 ) ) ;
#27128 = ORIENTED_EDGE ( 'NONE', *, *, #8795, .F. ) ;
#27129 = DIRECTION ( 'NONE',  ( 1.000000000000000000, 0.000000000000000000, 0.000000000000000000 ) ) ;
#27130 = DIRECTION ( 'NONE',  ( 0.7071067811865475727, 0.000000000000000000, 0.7071067811865475727 ) ) ;
#27131 = EDGE_LOOP ( 'NONE', ( #10900, #48243, #17345, #6170, #46945 ) ) ;
#27132 = CARTESIAN_POINT ( 'NONE',  ( 82.13853704237929776, 14.01986140997038888, -47.09707863094710945 ) ) ;
#27133 = CARTESIAN_POINT ( 'NONE',  ( 51.42797784481540191, -51.20406220416529663, -76.10787249881708760 ) ) ;
#27134 = CARTESIAN_POINT ( 'NONE',  ( 61.10834071495069963, 14.19179375509720131, -47.35406349611139376 ) ) ;
#27135 = CARTESIAN_POINT ( 'NONE',  ( 10.95257998347446282, -11.16488345018802875, -39.67851141808000648 ) ) ;
#27136 = AXIS2_PLACEMENT_3D ( 'NONE', #19466, #18692, #6915 ) ;
#27137 = DIRECTION ( 'NONE',  ( 0.000000000000000000, 1.000000000000000000, 0.000000000000000000 ) ) ;
#27138 = CARTESIAN_POINT ( 'NONE',  ( -9.434644029686850786, 12.51702915438919916, -5.750855165144660219 ) ) ;
#27139 = EDGE_CURVE ( 'NONE', #23799, #30077, #38765, .T. ) ;
#27140 = CARTESIAN_POINT ( 'NONE',  ( 0.6614253361915112261, -22.46035056599116686, -34.75586992539663100 ) ) ;
#27141 = FACE_OUTER_BOUND ( 'NONE', #31910, .T. ) ;
#27142 = ADVANCED_FACE ( 'NONE', ( #50176 ), #28151, .F. ) ;
#27143 = CARTESIAN_POINT ( 'NONE',  ( 12.76218697320820006, -8.529719636332050214, -56.64614358919829584 ) ) ;
#27144 = ORIENTED_EDGE ( 'NONE', *, *, #23461, .F. ) ;
#27145 = CARTESIAN_POINT ( 'NONE',  ( 58.45382029077139663, 15.48193787282010092, -47.52511337483100107 ) ) ;
#27146 = CARTESIAN_POINT ( 'NONE',  ( 57.29403763066589761, 19.36100728100389645, -53.60293029200749970 ) ) ;
#27147 = CARTESIAN_POINT ( 'NONE',  ( 72.04719216831770723, 1.025918948571509892, -70.19928925136699149 ) ) ;
#27148 = CARTESIAN_POINT ( 'NONE',  ( 45.06052948167663175, -40.03471377011139509, -61.51912326202059234 ) ) ;
#27149 = CARTESIAN_POINT ( 'NONE',  ( 15.00521638035900018, 19.40293989305209976, -20.65446309923339641 ) ) ;
#27150 = CARTESIAN_POINT ( 'NONE',  ( 16.13393739769620083, -15.61618894467929941, -18.08174999999999955 ) ) ;
#27151 = CARTESIAN_POINT ( 'NONE',  ( 48.21519585597539503, -54.28409539510870019, -55.14684628828510427 ) ) ;
#27152 = CARTESIAN_POINT ( 'NONE',  ( 22.90093739769620029, -15.61618894467913243, -28.45282021618999835 ) ) ;
#27153 = CARTESIAN_POINT ( 'NONE',  ( 63.65233837787879878, 1.010052234904250001, -69.64061050479490689 ) ) ;
#27154 = CARTESIAN_POINT ( 'NONE',  ( 9.221376762100923941, -11.63212162064420596, -70.95898967772608046 ) ) ;
#27155 = ORIENTED_EDGE ( 'NONE', *, *, #36010, .F. ) ;
#27156 = CARTESIAN_POINT ( 'NONE',  ( 17.38960780687880003, -8.272485099762899807, -36.62124792064249590 ) ) ;
#27157 = ORIENTED_EDGE ( 'NONE', *, *, #38361, .T. ) ;
#27158 = CARTESIAN_POINT ( 'NONE',  ( 71.26748243800840044, 1.369544300367010026, -70.36404682606520566 ) ) ;
#27159 = CARTESIAN_POINT ( 'NONE',  ( 60.41042530350419781, -45.68919557567430445, -47.20254626644950235 ) ) ;
#27160 = CARTESIAN_POINT ( 'NONE',  ( 54.20043578389000061, -48.94278307704069420, -48.51842787370119936 ) ) ;
#27161 = CARTESIAN_POINT ( 'NONE',  ( 16.13393739769620083, -15.61618894467929941, 4.450000000000000178 ) ) ;
#27163 = DIRECTION ( 'NONE',  ( 0.000000000000000000, 1.000000000000000000, 0.000000000000000000 ) ) ;
#27162 = DIRECTION ( 'NONE',  ( -2.066387465239710029E-12, 1.205421602240320019E-11, 1.000000000000000000 ) ) ;
#27164 = CARTESIAN_POINT ( 'NONE',  ( 68.13393739844677555, -29.16618894467940137, -42.14999999999999858 ) ) ;
#27165 = CARTESIAN_POINT ( 'NONE',  ( 22.46012542801484102, -10.75454228593980943, -67.58399627233477247 ) ) ;
#27166 = CARTESIAN_POINT ( 'NONE',  ( 11.27235466147499743, -9.289951649597259831, -66.79933434006539983 ) ) ;
#27167 = ORIENTED_EDGE ( 'NONE', *, *, #49145, .T. ) ;
#27168 = CARTESIAN_POINT ( 'NONE',  ( -0.2865249686165991516, -22.78714623532964723, -35.01561944896766931 ) ) ;
#27169 = CIRCLE ( 'NONE', #23821, 0.9999999999999974465 ) ;
#27170 = B_SPLINE_CURVE_WITH_KNOTS ( 'NONE', 3,
 ( #20757, #36744, #851, #16848, #48820, #38315, #25978, #30176 ),
 .UNSPECIFIED., .F., .F.,
 ( 4, 2, 2, 4 ),
 ( 0.000000000000000000, 0.2500000000000000000, 0.5000000000000000000, 1.000000000000000000 ),
 .UNSPECIFIED. ) ;
#27171 = ORIENTED_EDGE ( 'NONE', *, *, #34899, .T. ) ;
#27172 = VERTEX_POINT ( 'NONE', #3253 ) ;
#27173 = CARTESIAN_POINT ( 'NONE',  ( 8.222937397696199469, -15.61618894467929941, -32.14999999999999858 ) ) ;
#27174 = CARTESIAN_POINT ( 'NONE',  ( 71.33393739766809460, 1.883811055273910018, -68.84999999991929087 ) ) ;
#27175 = CARTESIAN_POINT ( 'NONE',  ( 22.90093739769620029, -15.61618894467913243, -28.45282021618999835 ) ) ;
#27176 = CARTESIAN_POINT ( 'NONE',  ( 9.374134746951858332, -64.20245714978280205, -46.81441715858309749 ) ) ;
#27177 = ORIENTED_EDGE ( 'NONE', *, *, #6654, .T. ) ;
#27178 = EDGE_CURVE ( 'NONE', #9877, #32504, #3314, .T. ) ;
#27179 = ORIENTED_EDGE ( 'NONE', *, *, #26605, .T. ) ;
#27180 = CARTESIAN_POINT ( 'NONE',  ( 56.46551611171859975, 19.54378718077660082, -53.85224439323700096 ) ) ;
#27181 = EDGE_CURVE ( 'NONE', #3105, #37975, #16453, .T. ) ;
#27182 = CARTESIAN_POINT ( 'NONE',  ( 56.43758032280119608, -50.61865618686479706, -53.06658686592589902 ) ) ;
#27183 = CARTESIAN_POINT ( 'NONE',  ( 10.72266466894950732, -11.45745788688983424, -35.66115297843326459 ) ) ;
#27184 = CARTESIAN_POINT ( 'NONE',  ( 64.74596444412888729, 0.01574119868441500175, -16.86735715512289957 ) ) ;
#27185 = CARTESIAN_POINT ( 'NONE',  ( 51.81004866964649835, -49.31229632625730375, -76.98867843529478705 ) ) ;
#27186 = EDGE_CURVE ( 'NONE', #22022, #4375, #20625, .T. ) ;
#27187 = DIRECTION ( 'NONE',  ( -1.000000000000000000, 0.000000000000000000, 0.000000000000000000 ) ) ;
#27188 = ORIENTED_EDGE ( 'NONE', *, *, #3135, .T. ) ;
#27189 = CARTESIAN_POINT ( 'NONE',  ( 13.13393739769600010, 18.38381105532060289, -34.64999999999999858 ) ) ;
#27190 = DIRECTION ( 'NONE',  ( 0.000000000000000000, -1.000000000000000000, 0.000000000000000000 ) ) ;
#27191 = CARTESIAN_POINT ( 'NONE',  ( 20.99564860854162518, -21.94232770570259206, -53.79933732301430638 ) ) ;
#27192 = CARTESIAN_POINT ( 'NONE',  ( 11.98811719313489910, -8.952937304298819399, -45.33533033764059894 ) ) ;
#27193 = CARTESIAN_POINT ( 'NONE',  ( 12.89174309999000023, -50.31665465520150349, -21.19267362013180289 ) ) ;
#27194 = DIRECTION ( 'NONE',  ( 0.000000000000000000, 0.000000000000000000, 1.000000000000000000 ) ) ;
#27195 = CARTESIAN_POINT ( 'NONE',  ( 55.89391012728359698, 14.06573721227290008, -15.81894319212849886 ) ) ;
#27196 = CARTESIAN_POINT ( 'NONE',  ( 61.08978236430399988, -45.33605757380430390, -46.92961198363219921 ) ) ;
#27197 = CARTESIAN_POINT ( 'NONE',  ( 56.52076750121499771, -50.75359106364579986, -53.72896418895009418 ) ) ;
#27198 = CARTESIAN_POINT ( 'NONE',  ( 23.18271560078089877, -15.85553183295759716, -46.85798391838910248 ) ) ;
#27199 = CARTESIAN_POINT ( 'NONE',  ( 15.24806174914439438, -8.849198298406202312, -43.91112208262838124 ) ) ;
#27200 = EDGE_CURVE ( 'NONE', #12954, #2493, #39409, .T. ) ;
#27201 = ORIENTED_EDGE ( 'NONE', *, *, #7158, .T. ) ;
#27202 = CIRCLE ( 'NONE', #30560, 17.09468304687048956 ) ;
#27203 = CARTESIAN_POINT ( 'NONE',  ( 13.39996905094259994, -51.78681982904430470, -74.14993593045390696 ) ) ;
#27204 = CARTESIAN_POINT ( 'NONE',  ( 64.90740703336619788, 0.9940423591679348192, -60.60059430635039490 ) ) ;
#27205 = CARTESIAN_POINT ( 'NONE',  ( 44.79293918095169147, -46.10604169002750297, -8.834396361043069135 ) ) ;
#27206 = CARTESIAN_POINT ( 'NONE',  ( 14.34417029198876037, -51.11618894467900986, -74.34716300801292732 ) ) ;
#27207 = CARTESIAN_POINT ( 'NONE',  ( 14.22007340590318591, -50.37075074235775674, -20.84587593357120738 ) ) ;
#27208 = CARTESIAN_POINT ( 'NONE',  ( 8.428872386935585936, -13.54538205412076657, -46.59100194065602096 ) ) ;
#27209 = CARTESIAN_POINT ( 'NONE',  ( 10.85466640530910176, -64.96697012893029921, -17.55961383758990024 ) ) ;
#27210 = CARTESIAN_POINT ( 'NONE',  ( 82.43661600080049823, 13.98517417207279934, -47.02799317055919914 ) ) ;
#27211 = CARTESIAN_POINT ( 'NONE',  ( 71.83679462228410273, 0.9486745332793850016, -70.37196876996070216 ) ) ;
#27213 = CARTESIAN_POINT ( 'NONE',  ( 11.58723606553711960, 33.56456631676410041, -23.92637893903365764 ) ) ;
#27212 = DIRECTION ( 'NONE',  ( 0.000000000000000000, 1.000000000000000000, 0.000000000000000000 ) ) ;
#27214 = CIRCLE ( 'NONE', #22157, 1.999999999999996669 ) ;
#27215 = CARTESIAN_POINT ( 'NONE',  ( 8.307302965981692822, -16.94665780510273834, -32.73880447305563735 ) ) ;
#27216 = CARTESIAN_POINT ( 'NONE',  ( 49.35532640881360322, 22.36582529078320292, -54.31909934291780218 ) ) ;
#27217 = ORIENTED_EDGE ( 'NONE', *, *, #14346, .F. ) ;
#27218 = CARTESIAN_POINT ( 'NONE',  ( 53.38243181765169965, -49.43430105679019704, -49.11031764516960152 ) ) ;
#27219 = VERTEX_POINT ( 'NONE', #15811 ) ;
#27220 = CARTESIAN_POINT ( 'NONE',  ( 46.31133434054406450, 7.971624601050109504, -59.28131743592275171 ) ) ;
#27221 = CARTESIAN_POINT ( 'NONE',  ( 55.91595717589669334, -45.90465048314089103, -17.93019253464870033 ) ) ;
#27222 = CARTESIAN_POINT ( 'NONE',  ( 13.59495223564569955, 20.17160945779230019, -22.70120839867610130 ) ) ;
#27223 = CARTESIAN_POINT ( 'NONE',  ( 12.89240665056879287, 24.25254711536716101, -75.71737149047099535 ) ) ;
#27224 = CARTESIAN_POINT ( 'NONE',  ( 23.13939390996569756, -16.43236156816429983, -54.48973855994069737 ) ) ;
#27225 = CARTESIAN_POINT ( 'NONE',  ( 52.62812434242830051, 18.56774166479950239, -48.49159175247050513 ) ) ;
#27226 = CARTESIAN_POINT ( 'NONE',  ( 55.98987895930139302, -45.71865684571069721, -17.27603967193159917 ) ) ;
#27227 = CARTESIAN_POINT ( 'NONE',  ( 55.44576274181299880, 15.28165783319319893, -25.46131564888750276 ) ) ;
#27228 = VERTEX_POINT ( 'NONE', #23902 ) ;
#27229 = CARTESIAN_POINT ( 'NONE',  ( 8.726417494668801567, -16.41327870859180038, -80.03322214350579600 ) ) ;
#27230 = ORIENTED_EDGE ( 'NONE', *, *, #34515, .T. ) ;
#27231 = CARTESIAN_POINT ( 'NONE',  ( 10.99341273097670069, -65.07165995155320104, -17.55111636776990025 ) ) ;
#27232 = CARTESIAN_POINT ( 'NONE',  ( 12.50062754218100025, 34.23954769984390367, -47.60354279947580380 ) ) ;
#27233 = CARTESIAN_POINT ( 'NONE',  ( 72.99348972288790094, 1.187296498006439993, -62.27829692513819992 ) ) ;
#27234 = CARTESIAN_POINT ( 'NONE',  ( 8.222937397696199469, -15.61618894467929941, -32.14999999999999858 ) ) ;
#27235 = CARTESIAN_POINT ( 'NONE',  ( -0.007164427059776000244, -4.186223695871990280, -34.77269723891829756 ) ) ;
#27236 = DIRECTION ( 'NONE',  ( -1.000000000000000000, 0.000000000000000000, 0.000000000000000000 ) ) ;
#27237 = CARTESIAN_POINT ( 'NONE',  ( 50.49348186761249480, -53.32002352356300179, -54.80181514761489581 ) ) ;
#27238 = EDGE_LOOP ( 'NONE', ( #12975, #22016, #25579, #22454, #44666, #176 ) ) ;
#27239 = CARTESIAN_POINT ( 'NONE',  ( 64.85866674173250601, 1.325841671674429900, -70.40030171741140919 ) ) ;
#27240 = CARTESIAN_POINT ( 'NONE',  ( 10.49445490244490031, -63.35389096203630999, -45.62690019722019485 ) ) ;
#27241 = EDGE_CURVE ( 'NONE', #18727, #50035, #11384, .T. ) ;
#27242 = FACE_OUTER_BOUND ( 'NONE', #45120, .T. ) ;
#27243 = B_SPLINE_CURVE_WITH_KNOTS ( 'NONE', 3,
 ( #45261, #25049, #33183, #21636, #9368, #37391, #17476, #37135 ),
 .UNSPECIFIED., .F., .F.,
 ( 4, 2, 2, 4 ),
 ( 0.05031563485850510525, 0.06814349192389300425, 0.08666255477376220984, 0.09307761161249389348 ),
 .UNSPECIFIED. ) ;
#27244 = ORIENTED_EDGE ( 'NONE', *, *, #8220, .T. ) ;
#27245 = CARTESIAN_POINT ( 'NONE',  ( 11.63780894515396902, -64.84990601410612499, -45.00312526891814002 ) ) ;
#27246 = CARTESIAN_POINT ( 'NONE',  ( 57.18740753958720546, 19.19824428508539782, -53.01833411987959721 ) ) ;
#27247 = EDGE_CURVE ( 'NONE', #40660, #32504, #32494, .T. ) ;
#27248 = CARTESIAN_POINT ( 'NONE',  ( 0.6045892726184427524, -8.790618991491967904, -34.79644291222913921 ) ) ;
#27249 = VERTEX_POINT ( 'NONE', #15567 ) ;
#27250 = CARTESIAN_POINT ( 'NONE',  ( 23.04645488412634080, -19.60033111914527382, -61.95899558997343348 ) ) ;
#27251 = CARTESIAN_POINT ( 'NONE',  ( 52.03944399862464110, 20.14552308598237573, -75.97489327919006996 ) ) ;
#27252 = CARTESIAN_POINT ( 'NONE',  ( 17.52689767915063968, -22.28079415070259017, -32.88709510709496442 ) ) ;
#27253 = DIRECTION ( 'NONE',  ( 0.000000000000000000, 0.000000000000000000, -1.000000000000000000 ) ) ;
#27254 = B_SPLINE_SURFACE_WITH_KNOTS ( 'NONE', 3, 3, ( 
 ( #39934, #51724, #11642, #19748, #3780, #4031, #7715, #35741, #23660, #15818, #51473, #51219 ),
 ( #16076, #19991, #104, #50951, #18971, #39422, #35988, #31783, #8218, #32034, #47800, #48057 ),
 ( #47041, #27607, #7192, #44119, #39164, #35216, #11906, #43356, #15313, #43100, #43862, #7960 ),
 ( #27862, #12157, #28112, #7449, #39674, #34951, #23909, #15049, #27096, #47298, #11128, #19492 ),
 ( #31016, #38910, #3000, #3522, #23399, #35482, #23147, #3257, #19234, #31265, #11388, #27350 ),
 ( #15572, #31528, #47546, #43612, #29413, #41217, #24164, #32806, #44629, #12674, #36753, #45417 ) ),
 .UNSPECIFIED., .F., .F., .F.,
 ( 4, 2, 4 ),
 ( 4, 1, 1, 1, 1, 1, 1, 1, 1, 4 ),
 ( -1.569668176790179892, -1.294976245851900076, -1.261864097015199970 ),
 ( 0.000000000000000000, 0.1111111111111110078, 0.2222222222222219878, 0.3333333333333329818, 0.4444444444444439757, 0.5555555555555560243, 0.6666666666666670737, 0.7777777777777779011, 0.8888888888888889506, 1.000000000000000000 ),
 .UNSPECIFIED. ) ;
#27255 = CARTESIAN_POINT ( 'NONE',  ( 13.21347626774960027, -7.905571145539870059, -63.17708371749469620 ) ) ;
#27256 = CYLINDRICAL_SURFACE ( 'NONE', #35562, 7.910999999999997812 ) ;
#27257 = CYLINDRICAL_SURFACE ( 'NONE', #43135, 6.766999999999998572 ) ;
#27258 = CARTESIAN_POINT ( 'NONE',  ( 0.000000000000000000, 0.000000000000000000, 0.000000000000000000 ) ) ;
#27259 = EDGE_LOOP ( 'NONE', ( #15280, #37936, #36145, #10765, #42140 ) ) ;
#27260 = ORIENTED_EDGE ( 'NONE', *, *, #16385, .F. ) ;
#27261 = CARTESIAN_POINT ( 'NONE',  ( 42.80890084010550112, -44.10023144781310123, -5.063862467037759885 ) ) ;
#27262 = CARTESIAN_POINT ( 'NONE',  ( 13.04913953162400020, -8.834543426766860108, -57.59677076196169310 ) ) ;
#27263 = CARTESIAN_POINT ( 'NONE',  ( 52.63891792457810226, -49.80233798285760116, -48.69614933315279615 ) ) ;
#27264 = AXIS2_PLACEMENT_3D ( 'NONE', #32425, #44775, #48448 ) ;
#27265 = CARTESIAN_POINT ( 'NONE',  ( 53.41693480164780539, 18.12090330447910347, -48.75416851879779756 ) ) ;
#27266 = CARTESIAN_POINT ( 'NONE',  ( 10.29526228329839910, -20.60856492654189864, -32.14999999999999858 ) ) ;
#27267 = ADVANCED_FACE ( 'NONE', ( #35978 ), #24809, .F. ) ;
#27268 = CIRCLE ( 'NONE', #50698, 33.97624844042369574 ) ;
#27269 = CARTESIAN_POINT ( 'NONE',  ( 47.24090259303480366, 23.52242523391999640, -74.36162934055690243 ) ) ;
#27270 = ADVANCED_FACE ( 'NONE', ( #23651 ), #48301, .T. ) ;
#27271 = SPHERICAL_SURFACE ( 'NONE', #11686, 1.999999999999879874 ) ;
#27272 = CARTESIAN_POINT ( 'NONE',  ( 41.64265090550289727, -46.42699119286240261, -4.296538310234230273 ) ) ;
#27273 = B_SPLINE_CURVE_WITH_KNOTS ( 'NONE', 3,
 ( #23476, #47876, #51798, #10947, #4095, #27166, #11720, #11979, #23734, #23220, #15645, #39750, #15900, #19826, #47368, #27421, #19050, #42918 ),
 .UNSPECIFIED., .F., .F.,
 ( 4, 2, 2, 2, 2, 2, 2, 2, 4 ),
 ( 0.000000000000000000, 0.06249982463622441586, 0.1249996492724488317, 0.1874994739086732476, 0.2499992985448976635, 0.3124991231811220516, 0.3749989478173464952, 0.4374987724535709388, 0.4999985970897953269 ),
 .UNSPECIFIED. ) ;
#27274 = CARTESIAN_POINT ( 'NONE',  ( 11.92574115022319958, 33.61414101779169528, -16.17905523990620154 ) ) ;
#27275 = VECTOR ( 'NONE', #32349, 1000.000000000000000 ) ;
#27276 = CARTESIAN_POINT ( 'NONE',  ( 8.119001781468568879, -17.55100877523230096, -68.43227042713769492 ) ) ;
#27277 = CARTESIAN_POINT ( 'NONE',  ( 20.97675674825520176, -21.71492495383600385, -32.14999999999999858 ) ) ;
#27278 = AXIS2_PLACEMENT_3D ( 'NONE', #35291, #19567, #38984 ) ;
#27279 = CARTESIAN_POINT ( 'NONE',  ( 54.08208344327369588, -50.62656384555610600, -76.77976102529341063 ) ) ;
#27281 = CARTESIAN_POINT ( 'NONE',  ( 31.79224979287389985, -36.11618894467930119, -84.65000000000000568 ) ) ;
#27280 = CARTESIAN_POINT ( 'NONE',  ( -5.732068215684789969, 16.49934381252809956, -7.265698657585460296 ) ) ;
#27282 = CARTESIAN_POINT ( 'NONE',  ( 16.13393739769620083, -45.61618894467940066, -35.14999999999999858 ) ) ;
#27283 = CARTESIAN_POINT ( 'NONE',  ( 9.221458473665698818, -11.63198193419115789, -78.67433547361216029 ) ) ;
#27284 = DIRECTION ( 'NONE',  ( 1.000000000000000000, 0.000000000000000000, 0.000000000000000000 ) ) ;
#27285 = EDGE_LOOP ( 'NONE', ( #42138, #8454 ) ) ;
#27286 = CARTESIAN_POINT ( 'NONE',  ( 50.95182575631829991, 19.71852405838109945, -76.14999999999999147 ) ) ;
#27287 = CARTESIAN_POINT ( 'NONE',  ( 47.61319252893540011, 23.29799037178950272, -54.82509320845959877 ) ) ;
#27288 = CARTESIAN_POINT ( 'NONE',  ( 61.26731136653179988, -45.17707473731150003, -27.55258710780080378 ) ) ;
#27289 = CARTESIAN_POINT ( 'NONE',  ( 63.29941945011370308, 1.188860127980290171, -62.23803121388370130 ) ) ;
#27290 = CARTESIAN_POINT ( 'NONE',  ( 61.44133208345009933, 14.11479117031280062, -47.30158650751790361 ) ) ;
#27291 = CARTESIAN_POINT ( 'NONE',  ( 17.61382546585139863, -22.91801235355460165, -78.66900642488448625 ) ) ;
#27292 = CARTESIAN_POINT ( 'NONE',  ( 51.31527825151569999, 17.56656504245249906, -76.60412086039399071 ) ) ;
#27293 = CARTESIAN_POINT ( 'NONE',  ( 53.21186570040269714, 18.22927129311189987, -48.84882494703119704 ) ) ;
#27294 = CARTESIAN_POINT ( 'NONE',  ( 16.13393739769620083, -38.61618894467930119, 4.943674098299959851 ) ) ;
#27295 = CARTESIAN_POINT ( 'NONE',  ( 13.13393739769596102, 18.38381105532059934, -35.01561944896766221 ) ) ;
#27296 = COLOUR_RGB ( '', 0.31764706, 0.68627451, 0.89019608) ;
#27297 = CARTESIAN_POINT ( 'NONE',  ( 50.52370621751256152, 4.812620015576031918, -76.21186558187457649 ) ) ;
#27298 = CARTESIAN_POINT ( 'NONE',  ( 16.14193623000787881, -23.52718903762350422, -62.00734913397092640 ) ) ;
#27299 = CARTESIAN_POINT ( 'NONE',  ( 65.03603135455020379, -32.24781572988710110, -17.83403478221860183 ) ) ;
#27300 = CARTESIAN_POINT ( 'NONE',  ( 15.24817897964529223, -22.38319375460040916, -70.99448831995151465 ) ) ;
#27301 = CARTESIAN_POINT ( 'NONE',  ( 63.83689218472199656, -31.35186283222479631, -16.87006829021100174 ) ) ;
#27302 = CARTESIAN_POINT ( 'NONE',  ( 71.09849264842429761, 1.384887413063060180, -60.98363600610959878 ) ) ;
#27303 = CARTESIAN_POINT ( 'NONE',  ( 12.06284766121009966, 32.21085600226960111, -46.39999999999999858 ) ) ;
#27304 = CARTESIAN_POINT ( 'NONE',  ( 72.32557311402300115, 1.409766894666529824, -61.59342351728570009 ) ) ;
#27305 = VECTOR ( 'NONE', #10167, 1000.000000000000114 ) ;
#27306 = CARTESIAN_POINT ( 'NONE',  ( 16.13393739769609780, -15.61618894467929941, 7.919999999999999929 ) ) ;
#27307 = CIRCLE ( 'NONE', #4713, 1.999999999999998224 ) ;
#27308 = CARTESIAN_POINT ( 'NONE',  ( 14.73211787852873655, -8.975754037563948629, -65.88667435850260290 ) ) ;
#27309 = ORIENTED_EDGE ( 'NONE', *, *, #44753, .F. ) ;
#27310 = ORIENTED_EDGE ( 'NONE', *, *, #40507, .T. ) ;
#27311 = CARTESIAN_POINT ( 'NONE',  ( 16.03351556195739747, -22.66831448449761055, -37.35171219075489546 ) ) ;
#27312 = EDGE_CURVE ( 'NONE', #23745, #44974, #23391, .T. ) ;
#27313 = EDGE_LOOP ( 'NONE', ( #46936, #11951, #16380, #5919, #43385 ) ) ;
#27314 = CARTESIAN_POINT ( 'NONE',  ( 56.76430699766049770, -45.27286064042839797, -25.50473296857350292 ) ) ;
#27315 = CARTESIAN_POINT ( 'NONE',  ( 22.09260590323088636, -20.84538979432554484, -77.73690341447758101 ) ) ;
#27316 = ORIENTED_EDGE ( 'NONE', *, *, #43651, .T. ) ;
#27317 = CARTESIAN_POINT ( 'NONE',  ( 68.13393739769620083, -43.11618894467930119, -73.25000000000000000 ) ) ;
#27318 = CARTESIAN_POINT ( 'NONE',  ( 42.74343314659522264, 6.507180287579836353, -76.60246204020066330 ) ) ;
#27319 = CONICAL_SURFACE ( 'NONE', #28128, 0.6405000000000011795, 1.029744258676660307 ) ;
#27320 = CARTESIAN_POINT ( 'NONE',  ( 10.64252135837869950, 32.35448059989499825, -23.65858396068249903 ) ) ;
#27321 = VERTEX_POINT ( 'NONE', #39927 ) ;
#27322 = CARTESIAN_POINT ( 'NONE',  ( 7.939473004570360537, -16.52913894747350199, -32.75701418906499640 ) ) ;
#27323 = AXIS2_PLACEMENT_3D ( 'NONE', #9846, #29137, #8982 ) ;
#27324 = CARTESIAN_POINT ( 'NONE',  ( 29.63393739769620083, -15.61618894467929941, -6.189999999999999503 ) ) ;
#27325 = CARTESIAN_POINT ( 'NONE',  ( 14.34417029198830029, 20.88381105532299742, -74.14999999999999147 ) ) ;
#27326 = CARTESIAN_POINT ( 'NONE',  ( 19.93518543153535916, -21.27024298737090646, -50.76453705344157186 ) ) ;
#27327 = CARTESIAN_POINT ( 'NONE',  ( 61.13643316145629569, -29.09601468760619980, -15.93607196403809922 ) ) ;
#27328 = CARTESIAN_POINT ( 'NONE',  ( 63.15932386229340523, 0.8936201581567960739, -62.29538467389520662 ) ) ;
#27329 = CARTESIAN_POINT ( 'NONE',  ( 46.46443538989580446, -53.12220744445389897, -76.13964794981698958 ) ) ;
#27330 = CARTESIAN_POINT ( 'NONE',  ( 10.22350615826409914, -10.45348132381399964, -79.24103283286969202 ) ) ;
#27331 = CARTESIAN_POINT ( 'NONE',  ( -0.3016046179078940015, -20.31737465961040101, -35.02873218748179340 ) ) ;
#27332 = CARTESIAN_POINT ( 'NONE',  ( 40.80913032419420716, 13.98564897013269892, -5.659189743293089769 ) ) ;
#27333 = CIRCLE ( 'NONE', #3063, 2.000000000000001332 ) ;
#27334 = EDGE_CURVE ( 'NONE', #23591, #25918, #19226, .T. ) ;
#27335 = CARTESIAN_POINT ( 'NONE',  ( 10.47385200046668707, 23.98129158042145548, -45.62050397739949403 ) ) ;
#27336 =( BOUNDED_CURVE ( )  B_SPLINE_CURVE ( 3, ( #25695, #6580, #34077, #10258 ),
 .UNSPECIFIED., .F., .T. ) 
 B_SPLINE_CURVE_WITH_KNOTS ( ( 4, 4 ),
 ( 2.239730981376319097, 2.341125871569534223 ),
 .UNSPECIFIED. ) 
 CURVE ( )  GEOMETRIC_REPRESENTATION_ITEM ( )  RATIONAL_B_SPLINE_CURVE ( ( 1.000000000000000000, 0.9991434398402569972, 0.9991434398402569972, 1.000000000000000000 ) ) 
 REPRESENTATION_ITEM ( '' )  );
#27337 = CARTESIAN_POINT ( 'NONE',  ( 82.68714621053820224, -45.11135183450330288, -46.76937705306080062 ) ) ;
#27338 = CIRCLE ( 'NONE', #4752, 0.9999999999999992228 ) ;
#27339 = CARTESIAN_POINT ( 'NONE',  ( 15.67962062493570130, 19.63028992856250099, -20.15000000000000213 ) ) ;
#27340 = CARTESIAN_POINT ( 'NONE',  ( 7.956346363297368995, -16.66974440877379848, -32.46687572425439328 ) ) ;
#27341 = ORIENTED_EDGE ( 'NONE', *, *, #35012, .T. ) ;
#27342 = DIRECTION ( 'NONE',  ( 0.000000000000000000, -1.000000000000000000, 0.000000000000000000 ) ) ;
#27343 = CARTESIAN_POINT ( 'NONE',  ( 2.905851976713329954, -55.66614162501279850, -9.124290884277760583 ) ) ;
#27344 = CARTESIAN_POINT ( 'NONE',  ( 76.46067994297268910, -29.90098307356280216, -13.05651891160819922 ) ) ;
#27345 = CARTESIAN_POINT ( 'NONE',  ( 75.27756523070299011, 13.44262948222908527, -14.10653473551886883 ) ) ;
#27346 = DIRECTION ( 'NONE',  ( 0.5516667872527503125, 0.8340645993220362486, 0.000000000000000000 ) ) ;
#27347 = CARTESIAN_POINT ( 'NONE',  ( 12.95505628089291328, -55.48922089072598851, -75.75074683306100098 ) ) ;
#27348 = AXIS2_PLACEMENT_3D ( 'NONE', #21678, #10435, #6242 ) ;
#27349 = CARTESIAN_POINT ( 'NONE',  ( 82.13853704237929776, -45.22180057317820001, -47.02038781679129897 ) ) ;
#27350 = CARTESIAN_POINT ( 'NONE',  ( 57.26033578974089977, -50.61618894467930119, -53.91588143635480179 ) ) ;
#27351 = CARTESIAN_POINT ( 'NONE',  ( 42.08165257923059954, 13.00661616386149966, -4.969335771722079187 ) ) ;
#27352 = DIRECTION ( 'NONE',  ( 0.000000000000000000, 0.000000000000000000, 1.000000000000000000 ) ) ;
#27353 = CARTESIAN_POINT ( 'NONE',  ( 64.43108017310198932, 0.9486745332807529074, -60.92803123004440380 ) ) ;
#27354 = CARTESIAN_POINT ( 'NONE',  ( 56.99484845788649778, -47.50308119450649968, -48.07762127917849426 ) ) ;
#27355 = CARTESIAN_POINT ( 'NONE',  ( 65.43393739769584272, -48.11618894467441976, -75.95000000000109708 ) ) ;
#27356 = CARTESIAN_POINT ( 'NONE',  ( 44.11147024075970080, -33.11640768660669920, -54.64999999999999858 ) ) ;
#27357 = CARTESIAN_POINT ( 'NONE',  ( 17.93795525508479827, -51.86173801737519540, -75.67066142420200947 ) ) ;
#27358 = CARTESIAN_POINT ( 'NONE',  ( 45.01728387151260335, -44.97693402557090536, -6.411623703542949748 ) ) ;
#27359 = CARTESIAN_POINT ( 'NONE',  ( 18.66652200592500321, -22.62280792536489926, -65.45693882779990247 ) ) ;
#27360 = CARTESIAN_POINT ( 'NONE',  ( 8.428889295206310805, -13.54532057320010452, -40.59100171928430711 ) ) ;
#27361 = CARTESIAN_POINT ( 'NONE',  ( 63.54193824524709555, 1.394012070864489861, -62.35876656057820355 ) ) ;
#27362 = ORIENTED_EDGE ( 'NONE', *, *, #8933, .T. ) ;
#27363 = CARTESIAN_POINT ( 'NONE',  ( 46.03122142033570441, 13.88381105532070059, -7.582879021622040305 ) ) ;
#27364 = DIRECTION ( 'NONE',  ( 0.000000000000000000, 0.000000000000000000, -1.000000000000000000 ) ) ;
#27365 = CARTESIAN_POINT ( 'NONE',  ( 73.02275056366489991, 1.266538207494809942, -68.83138049123679991 ) ) ;
#27366 = CARTESIAN_POINT ( 'NONE',  ( 46.11276164393227361, 8.867600659815479958, -56.41146322270898139 ) ) ;
#27367 = CARTESIAN_POINT ( 'NONE',  ( 10.08830361353289895, -11.20408907387949782, -81.23899999999999011 ) ) ;
#27368 = EDGE_LOOP ( 'NONE', ( #18071, #12612, #29112, #45051, #34053 ) ) ;
#27369 = CIRCLE ( 'NONE', #15671, 38.00000000000000000 ) ;
#27370 = CARTESIAN_POINT ( 'NONE',  ( 17.68156872138649760, 20.67960354982550086, -75.75221093576890041 ) ) ;
#27371 = ORIENTED_EDGE ( 'NONE', *, *, #6462, .F. ) ;
#27372 = VECTOR ( 'NONE', #13299, 1000.000000000000000 ) ;
#27373 = EDGE_CURVE ( 'NONE', #47321, #37740, #6448, .T. ) ;
#27374 = ORIENTED_EDGE ( 'NONE', *, *, #50099, .F. ) ;
#27375 = CARTESIAN_POINT ( 'NONE',  ( 56.87513795754310308, -45.11618894467940066, -15.74603272341079929 ) ) ;
#27376 = CARTESIAN_POINT ( 'NONE',  ( 23.44306558266119822, -13.53261324785490061, -81.23899999999999011 ) ) ;
#27377 = DIRECTION ( 'NONE',  ( -1.000000000000000000, 0.000000000000000000, 0.000000000000000000 ) ) ;
#27378 = ADVANCED_FACE ( 'NONE', ( #11636 ), #39417, .F. ) ;
#27379 = CARTESIAN_POINT ( 'NONE',  ( 61.69283295620359553, 13.94392212662380182, -46.85915540805209645 ) ) ;
#27380 = ADVANCED_FACE ( 'NONE', ( #31773 ), #3517, .T. ) ;
#27381 = EDGE_LOOP ( 'NONE', ( #8439, #48703, #18932, #30840 ) ) ;
#27382 = EDGE_CURVE ( 'NONE', #4500, #39126, #51468, .T. ) ;
#27383 = CARTESIAN_POINT ( 'NONE',  ( 18.13393739769620083, -41.61618894467930119, -35.14999999999999858 ) ) ;
#27384 = ORIENTED_EDGE ( 'NONE', *, *, #48099, .T. ) ;
#27385 = PLANE ( 'NONE',  #26891 ) ;
#27386 = DIRECTION ( 'NONE',  ( 1.000000000000000000, 0.000000000000000000, 0.000000000000000000 ) ) ;
#27387 = ORIENTED_EDGE ( 'NONE', *, *, #27774, .T. ) ;
#27388 = CARTESIAN_POINT ( 'NONE',  ( 72.82137280411760116, 1.383928098097870096, -62.75238677440889035 ) ) ;
#27389 = CARTESIAN_POINT ( 'NONE',  ( 51.03828674417159306, -50.88950370325699879, -76.15016575943649002 ) ) ;
#27390 = CARTESIAN_POINT ( 'NONE',  ( 60.82036937039629976, 14.47434740296430178, -47.72837797750310074 ) ) ;
#27391 = CARTESIAN_POINT ( 'NONE',  ( 15.80267776464130947, -8.799503143537849681, -39.93719130176964427 ) ) ;
#27392 = EDGE_CURVE ( 'NONE', #42919, #38484, #8211, .T. ) ;
#27393 = CARTESIAN_POINT ( 'NONE',  ( 41.57697697597580344, -43.84131550590989690, -3.558127429192100344 ) ) ;
#27394 = CARTESIAN_POINT ( 'NONE',  ( -11.32734370190460105, 10.64934056395049922, -6.430192534648650593 ) ) ;
#27395 = CARTESIAN_POINT ( 'NONE',  ( 46.84224739830732176, 22.80152007029589001, -75.76637087393561387 ) ) ;
#27396 = CARTESIAN_POINT ( 'NONE',  ( 19.00123712817629951, -22.05987976827099928, -43.21391308946270016 ) ) ;
#27397 = CARTESIAN_POINT ( 'NONE',  ( 16.04609829188889947, -7.768958065275190172, -50.78394269049039877 ) ) ;
#27398 = ORIENTED_EDGE ( 'NONE', *, *, #28958, .F. ) ;
#27399 = CARTESIAN_POINT ( 'NONE',  ( 56.84932596551109185, -50.65659107673559447, -53.85230338955700091 ) ) ;
#27400 = CARTESIAN_POINT ( 'NONE',  ( 44.79311949664099757, 14.87366903724590017, -8.834518368838249813 ) ) ;
#27401 = CARTESIAN_POINT ( 'NONE',  ( 71.65899916879679665, 1.412342135319139880, -70.14294384383438796 ) ) ;
#27402 = CARTESIAN_POINT ( 'NONE',  ( 45.77359740143206324, -40.08047819383660482, -58.05860318629369488 ) ) ;
#27403 = CARTESIAN_POINT ( 'NONE',  ( 15.65801254756719807, 19.62299100880909819, -20.25518593351949903 ) ) ;
#27404 = EDGE_CURVE ( 'NONE', #46283, #20497, #45764, .T. ) ;
#27405 = DIRECTION ( 'NONE',  ( 1.000000000000000000, 2.460964292799963328E-14, 0.000000000000000000 ) ) ;
#27406 = LINE ( 'NONE', #34748, #4581 ) ;
#27407 = CARTESIAN_POINT ( 'NONE',  ( 48.85881101229590229, -54.00570711265250168, -55.08347352314449807 ) ) ;
#27408 = CARTESIAN_POINT ( 'NONE',  ( -12.74484839418222748, -57.05697611480018594, -53.24848714985477471 ) ) ;
#27409 = DIRECTION ( 'NONE',  ( -0.7286256507163790808, -0.6849121557675359462, 0.000000000000000000 ) ) ;
#27410 = CARTESIAN_POINT ( 'NONE',  ( 18.20468663224212946, -23.32126934762677095, -37.92433689214998793 ) ) ;
#27411 = CARTESIAN_POINT ( 'NONE',  ( 47.73402016065340092, 23.24730430298579975, -54.93079182720639864 ) ) ;
#27412 = ORIENTED_EDGE ( 'NONE', *, *, #32094, .T. ) ;
#27413 = CARTESIAN_POINT ( 'NONE',  ( 12.48397201735700079, -22.11114445343120138, -37.73031295553310116 ) ) ;
#27414 = VERTEX_POINT ( 'NONE', #9514 ) ;
#27415 = CARTESIAN_POINT ( 'NONE',  ( 18.38332385620206111, 20.94377882893676102, -75.56421372420827254 ) ) ;
#27416 = CARTESIAN_POINT ( 'NONE',  ( 60.30125063334870106, -45.75567911012539923, -47.36809293580299851 ) ) ;
#27417 = DIRECTION ( 'NONE',  ( -1.000000000000000000, 0.000000000000000000, 0.000000000000000000 ) ) ;
#27418 = CARTESIAN_POINT ( 'NONE',  ( -18.86606260230390220, 19.38381105532060289, 11.97999999999999865 ) ) ;
#27419 = DIRECTION ( 'NONE',  ( 0.000000000000000000, 1.000000000000000000, 0.000000000000000000 ) ) ;
#27420 = CARTESIAN_POINT ( 'NONE',  ( 51.13393739769620083, 19.38381105532069881, 11.34999999999999964 ) ) ;
#27421 = CARTESIAN_POINT ( 'NONE',  ( 23.83903810970707227, -13.54551561636778878, -67.42433258642762439 ) ) ;
#27422 = ORIENTED_EDGE ( 'NONE', *, *, #4649, .F. ) ;
#27423 = DIRECTION ( 'NONE',  ( -0.8224686640529090820, -0.3976080002595601126, -0.4067593573362717763 ) ) ;
#27424 = B_SPLINE_CURVE_WITH_KNOTS ( 'NONE', 3,
 ( #35171, #63, #24118, #43313, #3478, #23867, #35433, #40138, #39891, #31991 ),
 .UNSPECIFIED., .F., .F.,
 ( 4, 1, 1, 1, 1, 1, 1, 4 ),
 ( 0.5000016690426868360, 0.5743016179356827955, 0.6535205489993028971, 0.7327394800629218885, 0.8119584111265421011, 0.8911773421901610925, 0.9703962732537800839, 1.000000000000000000 ),
 .UNSPECIFIED. ) ;
#27425 = ORIENTED_EDGE ( 'NONE', *, *, #13626, .T. ) ;
#27426 = AXIS2_PLACEMENT_3D ( 'NONE', #17893, #42270, #45946 ) ;
#27427 =( REPRESENTATION_RELATIONSHIP ('NONE','NONE', #29764, #50919 ) REPRESENTATION_RELATIONSHIP_WITH_TRANSFORMATION ( #19661 )SHAPE_REPRESENTATION_RELATIONSHIP( ) );
#27428 = EDGE_LOOP ( 'NONE', ( #737, #9905, #35029, #25944, #44337 ) ) ;
#27429 = CARTESIAN_POINT ( 'NONE',  ( 18.95614455194280268, -22.07975653177619790, -59.21613716431369312 ) ) ;
#27430 = CARTESIAN_POINT ( 'NONE',  ( 22.90083016047308462, -15.61618874168370752, -60.84718745454353694 ) ) ;
#27431 = CARTESIAN_POINT ( 'NONE',  ( 76.87859684847769870, -43.11619168008749625, -14.85884840380859906 ) ) ;
#27432 = CARTESIAN_POINT ( 'NONE',  ( 12.77819848573380135, -65.50111593353840078, -47.68593301887450053 ) ) ;
#27433 = VERTEX_POINT ( 'NONE', #33066 ) ;
#27434 = ORIENTED_EDGE ( 'NONE', *, *, #16648, .F. ) ;
#27435 = EDGE_CURVE ( 'NONE', #14727, #42029, #23135, .T. ) ;
#27436 = CARTESIAN_POINT ( 'NONE',  ( 23.98146843348427737, -16.64924324331575889, -55.54932755510194653 ) ) ;
#27437 = CARTESIAN_POINT ( 'NONE',  ( -22.60067283610179700, -11.07416626356550005, -54.64998264227110525 ) ) ;
#27438 = CARTESIAN_POINT ( 'NONE',  ( 56.39270784037439199, -50.52750194525579985, -52.86271187285759510 ) ) ;
#27439 = DIRECTION ( 'NONE',  ( 0.9313175168446001795, -0.3616257875446830528, 0.04329517988293300756 ) ) ;
#27440 = CARTESIAN_POINT ( 'NONE',  ( 62.98651954880020298, -0.7832202496777560530, -16.35632123205009947 ) ) ;
#27441 = B_SPLINE_CURVE_WITH_KNOTS ( 'NONE', 3,
 ( #46840, #3316, #51779, #35276, #3059, #15883, #19031, #15371, #35540, #35007 ),
 .UNSPECIFIED., .F., .F.,
 ( 4, 1, 1, 1, 1, 1, 1, 4 ),
 ( 0.5000037312039752324, 0.5547748945261627984, 0.6339938255897815678, 0.7132127566533992269, 0.7924316877170179962, 0.8716506187806356554, 0.9508695498442544247, 1.000000000000000000 ),
 .UNSPECIFIED. ) ;
#27442 = CARTESIAN_POINT ( 'NONE',  ( 51.31527825141329657, -48.79894293239630088, -76.60412086037939616 ) ) ;
#27443 = CARTESIAN_POINT ( 'NONE',  ( 60.48885993748309886, -46.71224472025600249, -48.89115175517449785 ) ) ;
#27444 = ORIENTED_EDGE ( 'NONE', *, *, #21371, .F. ) ;
#27445 = LINE ( 'NONE', #39009, #15758 ) ;
#27446 = CARTESIAN_POINT ( 'NONE',  ( 24.04518460902906085, -15.61618869790763675, -47.79232989768991757 ) ) ;
#27447 = DIRECTION ( 'NONE',  ( 0.000000000000000000, 0.000000000000000000, -1.000000000000000000 ) ) ;
#27448 = CARTESIAN_POINT ( 'NONE',  ( 83.36355414456373580, -45.34681625531927551, -47.55048134727741171 ) ) ;
#27449 = CARTESIAN_POINT ( 'NONE',  ( 17.64329854752050153, -7.914982772203240202, -53.57409916825699270 ) ) ;
#27450 = CARTESIAN_POINT ( 'NONE',  ( 12.89658886673069915, -50.00140124964299559, -21.06837794024639976 ) ) ;
#27451 = CARTESIAN_POINT ( 'NONE',  ( 56.53391597728690243, 19.38755390252309851, -75.43697629958880668 ) ) ;
#27452 = EDGE_CURVE ( 'NONE', #29653, #37505, #27338, .T. ) ;
#27453 = DIRECTION ( 'NONE',  ( -0.8320502943378438321, 0.000000000000000000, 0.5547001962252288143 ) ) ;
#27454 = CARTESIAN_POINT ( 'NONE',  ( 56.00506715693309445, 13.88381105532070059, -14.82112848627589941 ) ) ;
#27455 = CARTESIAN_POINT ( 'NONE',  ( 60.70258586536569823, -45.54124907573869763, -47.21990429565040159 ) ) ;
#27456 = CARTESIAN_POINT ( 'NONE',  ( 71.33393739769650210, 1.396834109478129804, -70.23662692463440749 ) ) ;
#27457 = CARTESIAN_POINT ( 'NONE',  ( 17.37116791007819927, -8.672715762353169211, -52.40330909284259775 ) ) ;
#27458 = CARTESIAN_POINT ( 'NONE',  ( 22.04683866091923150, -12.20817827527022637, -44.28613215260582336 ) ) ;
#27459 = VERTEX_POINT ( 'NONE', #16850 ) ;
#27460 = CARTESIAN_POINT ( 'NONE',  ( 46.90960455200850276, 22.37535576487919897, -75.96332490897151501 ) ) ;
#27461 = CARTESIAN_POINT ( 'NONE',  ( 65.01767019485720311, 1.328674444234379859, -60.82574149480920056 ) ) ;
#27462 = LINE ( 'NONE', #26952, #22220 ) ;
#27463 = LINE ( 'NONE', #43466, #13705 ) ;
#27464 = CARTESIAN_POINT ( 'NONE',  ( 14.16187783161290170, -50.35113599914600258, -20.85710678118659800 ) ) ;
#27465 = LINE ( 'NONE', #39538, #32328 ) ;
#27466 = EDGE_CURVE ( 'NONE', #24630, #8804, #10640, .T. ) ;
#27467 = CARTESIAN_POINT ( 'NONE',  ( 10.64977475910500004, -64.85626261263139725, -18.05902683592860214 ) ) ;
#27469 = EDGE_CURVE ( 'NONE', #26913, #8932, #34058, .T. ) ;
#27468 = CARTESIAN_POINT ( 'NONE',  ( 10.80633501409609920, 33.76396855927119844, -17.92671787883650225 ) ) ;
#27470 = CARTESIAN_POINT ( 'NONE',  ( 56.46551567295650642, -50.77616483221130750, -74.14999999999999147 ) ) ;
#27472 = CARTESIAN_POINT ( 'NONE',  ( 43.68604305009880306, -37.81292632501880036, -71.88615322025499665 ) ) ;
#27471 = CARTESIAN_POINT ( 'NONE',  ( 62.63393739769619373, 21.88381105532059934, 11.84999999999999964 ) ) ;
#27473 = CARTESIAN_POINT ( 'NONE',  ( -0.2744272739026379915, -53.43782452381620374, -9.661128459681899372 ) ) ;
#27474 = CARTESIAN_POINT ( 'NONE',  ( 49.06940219517189661, 22.69206583466019822, -55.15293681905570367 ) ) ;
#27475 = EDGE_CURVE ( 'NONE', #20296, #45486, #14821, .T. ) ;
#27476 = ORIENTED_EDGE ( 'NONE', *, *, #17913, .T. ) ;
#27477 = CARTESIAN_POINT ( 'NONE',  ( 53.15063603407050152, -49.53259255823910223, -49.06766781164589730 ) ) ;
#27478 = B_SPLINE_CURVE_WITH_KNOTS ( 'NONE', 3,
 ( #51264, #14578, #6726, #42890, #27396, #3822, #43655, #7757, #43397, #47086 ),
 .UNSPECIFIED., .F., .F.,
 ( 4, 1, 1, 1, 1, 1, 1, 4 ),
 ( 0.4999963331327971772, 0.5249287906993036490, 0.6041477217628976604, 0.6833666528264928930, 0.7625855838900870154, 0.8418045149536969030, 0.9210234460172921356, 1.000000000000000000 ),
 .UNSPECIFIED. ) ;
#27479 = ORIENTED_EDGE ( 'NONE', *, *, #50840, .T. ) ;
#27480 = CARTESIAN_POINT ( 'NONE',  ( 43.75706346978401484, 7.740046907999022174, -71.93205349775588786 ) ) ;
#27481 = CARTESIAN_POINT ( 'NONE',  ( 17.90524903744462293, -22.20704404317461567, -74.86948688974470656 ) ) ;
#27482 = FACE_OUTER_BOUND ( 'NONE', #26532, .T. ) ;
#27483 = CARTESIAN_POINT ( 'NONE',  ( 13.87880486592528406, 24.32147317887789839, -76.14999999999997726 ) ) ;
#27484 = CARTESIAN_POINT ( 'NONE',  ( 22.30826260938979999, -12.20733768994999835, -58.29224725099429349 ) ) ;
#27485 = CARTESIAN_POINT ( 'NONE',  ( 55.87801225299120489, -45.85446601339950234, -17.30532844135920101 ) ) ;
#27486 = FACE_OUTER_BOUND ( 'NONE', #17405, .T. ) ;
#27487 = ORIENTED_EDGE ( 'NONE', *, *, #25115, .F. ) ;
#27488 = CARTESIAN_POINT ( 'NONE',  ( 23.88928256296529895, -14.41561843416390154, -45.23861751603709536 ) ) ;
#27489 = VERTEX_POINT ( 'NONE', #25461 ) ;
#27490 = CARTESIAN_POINT ( 'NONE',  ( 11.98643060099639968, -65.41791523794120167, -17.50083490704260214 ) ) ;
#27491 = CARTESIAN_POINT ( 'NONE',  ( 10.13410506179149984, 33.50987130412710258, -47.01082059592499718 ) ) ;
#27492 = CARTESIAN_POINT ( 'NONE',  ( 73.07318775143950518, 0.8986939045430379913, -62.24348040161360274 ) ) ;
#27493 = EDGE_CURVE ( 'NONE', #45223, #7747, #41591, .T. ) ;
#27494 = DIRECTION ( 'NONE',  ( -0.7071067811865475727, 0.000000000000000000, -0.7071067811865475727 ) ) ;
#27495 = FACE_OUTER_BOUND ( 'NONE', #40401, .T. ) ;
#27496 = DIRECTION ( 'NONE',  ( 0.000000000000000000, -1.000000000000000000, 0.000000000000000000 ) ) ;
#27497 = VECTOR ( 'NONE', #3501, 1000.000000000000000 ) ;
#27498 = VECTOR ( 'NONE', #37244, 1000.000000000000000 ) ;
#27499 = ORIENTED_EDGE ( 'NONE', *, *, #43713, .T. ) ;
#27500 = EDGE_CURVE ( 'NONE', #29825, #44194, #31857, .T. ) ;
#27501 = CARTESIAN_POINT ( 'NONE',  ( 8.223360643215830379, -15.61635149015999957, -74.50766849176298479 ) ) ;
#27502 = CARTESIAN_POINT ( 'NONE',  ( 11.13393739769619906, -63.50859000450320480, -43.92731420739779225 ) ) ;
#27503 = VECTOR ( 'NONE', #10029, 1000.000000000000000 ) ;
#27504 = CARTESIAN_POINT ( 'NONE',  ( 68.13393739769810509, 19.38381105532030091, -71.50000000000198952 ) ) ;
#27505 = ORIENTED_EDGE ( 'NONE', *, *, #12009, .T. ) ;
#27506 = CARTESIAN_POINT ( 'NONE',  ( 24.01324593353028547, -16.33809533768586419, -43.82140147199449842 ) ) ;
#27507 = CARTESIAN_POINT ( 'NONE',  ( 8.820368351115295269, -12.49945830288972282, -76.63581724531364614 ) ) ;
#27508 = CARTESIAN_POINT ( 'NONE',  ( 8.222988179026620159, -15.61639226004780134, -48.50766849176299189 ) ) ;
#27509 = ORIENTED_EDGE ( 'NONE', *, *, #45929, .T. ) ;
#27510 = CARTESIAN_POINT ( 'NONE',  ( 12.14975833386557724, -22.52868516919143715, -62.45899714093157939 ) ) ;
#27511 = CARTESIAN_POINT ( 'NONE',  ( 19.31296351478369999, -49.88685839599860117, -82.14319696191608955 ) ) ;
#27512 = CARTESIAN_POINT ( 'NONE',  ( 20.26128133979632651, -21.03119890602486208, -32.74566382982119706 ) ) ;
#27513 = CARTESIAN_POINT ( 'NONE',  ( 11.27221847759618534, -9.290054678679373623, -69.08399908941892420 ) ) ;
#27514 = CARTESIAN_POINT ( 'NONE',  ( 24.31740379465060187, -14.60941300932350018, -77.75336703320090237 ) ) ;
#27515 = DIRECTION ( 'NONE',  ( -0.5720614028176880250, 0.7071067811865480168, 0.4156269377774474139 ) ) ;
#27516 = DIRECTION ( 'NONE',  ( 0.000000000000000000, 1.000000000000000000, 0.000000000000000000 ) ) ;
#27517 = PRODUCT_CONTEXT ( 'NONE', #22066, 'mechanical' ) ;
#27518 = VERTEX_POINT ( 'NONE', #20496 ) ;
#27519 = ORIENTED_EDGE ( 'NONE', *, *, #36141, .T. ) ;
#27520 = CARTESIAN_POINT ( 'NONE',  ( 22.40917576918729992, -11.60021120742629996, -52.05144558750829731 ) ) ;
#27521 = CARTESIAN_POINT ( 'NONE',  ( 52.90434498377169348, -49.66345680823589959, -49.01850774012499556 ) ) ;
#27522 = CARTESIAN_POINT ( 'NONE',  ( 10.33790303897889906, -20.66510390621489890, -32.14999999999999858 ) ) ;
#27523 = CARTESIAN_POINT ( 'NONE',  ( 47.07006461603479863, 23.03759314561689919, -75.46887108633461594 ) ) ;
#27524 = DIRECTION ( 'NONE',  ( -0.2717754459342062168, -0.4033282527652566896, 0.8737645149058118621 ) ) ;
#27525 = B_SPLINE_CURVE_WITH_KNOTS ( 'NONE', 3,
 ( #12871, #9456, #13139, #49292, #13389, #40633, #20962, #36689, #4732, #28827, #1840, #1325, #41407, #17818, #1060, #33537, #29348, #41667, #25405, #17055 ),
 .UNSPECIFIED., .F., .F.,
 ( 4, 2, 2, 2, 2, 2, 2, 2, 2, 4 ),
 ( 0.000000000000000000, 0.05535613038339300823, 0.2869944836127450438, 0.5186328368420959345, 0.8630971313986249838, 1.150796175198169902, 1.294645697097940085, 1.524804932137569846, 1.893059708200979907, 2.301592350396330033 ),
 .UNSPECIFIED. ) ;
#27526 = DIRECTION ( 'NONE',  ( 0.000000000000000000, 1.000000000000000000, 0.000000000000000000 ) ) ;
#27527 = CARTESIAN_POINT ( 'NONE',  ( 11.86574223145029983, 33.83900248408709643, -16.54426240393689795 ) ) ;
#27528 = TOROIDAL_SURFACE ( 'NONE', #19199, 5.500000000000000000, 0.5000000000000000000 ) ;
#27530 = VECTOR ( 'NONE', #14690, 1000.000000000000000 ) ;
#27529 = CARTESIAN_POINT ( 'NONE',  ( 11.31210022934189929, -8.927945002443658851, -70.80883835904629109 ) ) ;
#27531 = CARTESIAN_POINT ( 'NONE',  ( 20.45445179548310222, -22.15697897774440150, -32.14999999999999858 ) ) ;
#27532 = EDGE_CURVE ( 'NONE', #35884, #22335, #3944, .T. ) ;
#27533 = CARTESIAN_POINT ( 'NONE',  ( 54.33632571825120294, -50.61618477685789941, -76.86293993265819324 ) ) ;
#27535 = CARTESIAN_POINT ( 'NONE',  ( 47.18325654339099628, 23.57487866773040253, -54.61058579560449289 ) ) ;
#27534 = CARTESIAN_POINT ( 'NONE',  ( -2.912062977092380045, 18.91103907894019898, -6.721088743486959949 ) ) ;
#27536 = CARTESIAN_POINT ( 'NONE',  ( 63.42952807919409253, 1.382830464309369844, -68.61079447352989291 ) ) ;
#27537 = CARTESIAN_POINT ( 'NONE',  ( 61.38942555204300078, 13.99165690388499961, -46.90185059412529966 ) ) ;
#27538 = CARTESIAN_POINT ( 'NONE',  ( 22.37318698975099807, -53.60726374558549878, -34.64999999999999858 ) ) ;
#27539 = EDGE_CURVE ( 'NONE', #10341, #49525, #20759, .T. ) ;
#27540 = ORIENTED_EDGE ( 'NONE', *, *, #3093, .T. ) ;
#27541 = CARTESIAN_POINT ( 'NONE',  ( 53.39564317062880150, -49.36443647587950068, -48.78219654307289943 ) ) ;
#27542 = CARTESIAN_POINT ( 'NONE',  ( 47.83453594094610395, 23.15510728029320120, -54.72216408865189408 ) ) ;
#27543 = CARTESIAN_POINT ( 'NONE',  ( 57.83204157793740308, -45.68025036402679717, -26.31202219667439834 ) ) ;
#27544 = CARTESIAN_POINT ( 'NONE',  ( 17.16940068822441390, -23.52720096816359074, -72.25068831949764103 ) ) ;
#27545 = CARTESIAN_POINT ( 'NONE',  ( 61.24439460628430254, 14.13692964258179963, -47.29149699898169956 ) ) ;
#27546 = CARTESIAN_POINT ( 'NONE',  ( 11.87813115486479987, -21.73131829969980089, -76.92618994148479317 ) ) ;
#27547 = CARTESIAN_POINT ( 'NONE',  ( 51.34762213738049752, 17.76135683261760079, -76.60870781513519034 ) ) ;
#27548 = CARTESIAN_POINT ( 'NONE',  ( 52.77257271998939814, 18.46126773324610326, -48.57104616786630658 ) ) ;
#27549 = DIRECTION ( 'NONE',  ( 0.6339889056055360017, 0.000000000000000000, -0.7733421413379041320 ) ) ;
#27550 = CARTESIAN_POINT ( 'NONE',  ( 52.86024057890899996, -49.64494889463909999, -48.64479820451980174 ) ) ;
#27551 = FACE_OUTER_BOUND ( 'NONE', #45746, .T. ) ;
#27552 = CARTESIAN_POINT ( 'NONE',  ( 47.57920160075400418, -54.54378672726409860, -54.77372601769780402 ) ) ;
#27553 = CARTESIAN_POINT ( 'NONE',  ( 63.63877703368444116, -31.87229146824659765, -17.33502983657059460 ) ) ;
#27554 = CARTESIAN_POINT ( 'NONE',  ( 45.34397758664299971, 2.696163290909390220, -34.64999999999999858 ) ) ;
#27555 = CARTESIAN_POINT ( 'NONE',  ( 59.97735437335310138, -29.43971439818610136, -15.84040877096640187 ) ) ;
#27556 = CARTESIAN_POINT ( 'NONE',  ( 71.15687762518609816, 1.370937308141420230, -60.89332811547459556 ) ) ;
#27557 = CARTESIAN_POINT ( 'NONE',  ( 11.13393739769619906, 32.10364385886999372, -43.74837338606149473 ) ) ;
#27558 = CARTESIAN_POINT ( 'NONE',  ( 72.22406619500640090, 1.409763019284739904, -61.49193411207189541 ) ) ;
#27559 = CARTESIAN_POINT ( 'NONE',  ( 51.37212073277904523, -34.54336882558848743, -76.66706012796622360 ) ) ;
#27560 = ADVANCED_FACE ( 'NONE', ( #8728 ), #44887, .T. ) ;
#27561 = CARTESIAN_POINT ( 'NONE',  ( 11.85320398676953246, -10.34456170899610861, -65.73580935773964029 ) ) ;
#27562 = ORIENTED_EDGE ( 'NONE', *, *, #33968, .T. ) ;
#27563 = EDGE_LOOP ( 'NONE', ( #32658, #15532, #18824, #38240 ) ) ;
#27564 = CARTESIAN_POINT ( 'NONE',  ( 15.09833416417832375, -7.705195683357469960, -55.25065450683342760 ) ) ;
#27565 = EDGE_CURVE ( 'NONE', #29281, #46345, #19002, .T. ) ;
#27566 = CARTESIAN_POINT ( 'NONE',  ( 0.1416488651360897633, -45.95570562466429010, -34.68322412398369892 ) ) ;
#27567 = EDGE_LOOP ( 'NONE', ( #9217, #42467, #8177, #25108 ) ) ;
#27568 = DIRECTION ( 'NONE',  ( 0.000000000000000000, 0.000000000000000000, 1.000000000000000000 ) ) ;
#27569 = CARTESIAN_POINT ( 'NONE',  ( 16.07729529398784862, -23.52701512416443563, -78.00994996383560931 ) ) ;
#27570 = TOROIDAL_SURFACE ( 'NONE', #44335, 34.99999963932619806, 4.999999999166930387 ) ;
#27571 = AXIS2_PLACEMENT_3D ( 'NONE', #13353, #4962, #8900 ) ;
#27572 = EDGE_LOOP ( 'NONE', ( #10603, #49797, #48127, #40979 ) ) ;
#27573 = DIRECTION ( 'NONE',  ( 0.000000000000000000, 0.000000000000000000, 1.000000000000000000 ) ) ;
#27574 = CONICAL_SURFACE ( 'NONE', #48534, 0.6299999999999866818, 0.7853981633974476129 ) ;
#27575 = CARTESIAN_POINT ( 'NONE',  ( 43.51419838157591613, 6.618822493252672245, -72.74866027328177154 ) ) ;
#27576 = CARTESIAN_POINT ( 'NONE',  ( 41.47581685013189912, -44.78873423027059886, -5.433834233955179727 ) ) ;
#27577 = CIRCLE ( 'NONE', #42671, 1.000000000000000444 ) ;
#27578 = AXIS2_PLACEMENT_3D ( 'NONE', #18463, #26570, #6680 ) ;
#27579 = CARTESIAN_POINT ( 'NONE',  ( 24.35368793360969875, -14.96933410525219976, -35.76733356948250275 ) ) ;
#27580 = CARTESIAN_POINT ( 'NONE',  ( 45.25840371050470168, 2.392299703521869603, -34.70497375832189846 ) ) ;
#27581 = CARTESIAN_POINT ( 'NONE',  ( 24.04402149975506831, -15.74633035369765466, -49.79756549422418033 ) ) ;
#27582 = CARTESIAN_POINT ( 'NONE',  ( 62.94494383321469400, -29.78410970874689667, -16.20581832066559969 ) ) ;
#27583 = CARTESIAN_POINT ( 'NONE',  ( 14.38797371179902385, 20.00716050925374390, -74.86151687917137565 ) ) ;
#27584 = CARTESIAN_POINT ( 'NONE',  ( 47.29839800642639602, -54.29825318176240501, -75.29258675765889564 ) ) ;
#27585 = CARTESIAN_POINT ( 'NONE',  ( 13.83560527192710232, -8.112562019569040217, -69.41788538098089134 ) ) ;
#27586 = CARTESIAN_POINT ( 'NONE',  ( 54.47257875656340076, 15.01998573668699954, -15.76423485725169904 ) ) ;
#27587 = CARTESIAN_POINT ( 'NONE',  ( 42.77859928634750020, 14.48502410817190089, -7.241844954409731194 ) ) ;
#27588 = CARTESIAN_POINT ( 'NONE',  ( 15.05440318628110141, 21.88381105532300097, -76.14999999999999147 ) ) ;
#27589 = CARTESIAN_POINT ( 'NONE',  ( 84.44784216359251161, -43.11618894467930119, -47.47585302082339354 ) ) ;
#27590 = DIRECTION ( 'NONE',  ( -1.000000000000000000, 0.000000000000000000, 0.000000000000000000 ) ) ;
#27591 = CARTESIAN_POINT ( 'NONE',  ( 20.83159658330290043, -22.39222900395139959, -41.81470958976159835 ) ) ;
#27592 = EDGE_LOOP ( 'NONE', ( #46552, #49638, #21694, #22599 ) ) ;
#27593 = CARTESIAN_POINT ( 'NONE',  ( 56.48923526673240048, -46.16653024775970238, -26.24159571999479823 ) ) ;
#27594 = EDGE_CURVE ( 'NONE', #46163, #51177, #44102, .T. ) ;
#27595 = CARTESIAN_POINT ( 'NONE',  ( 15.03857555097549970, -50.67925693779799445, -20.69450120486489908 ) ) ;
#27596 = CARTESIAN_POINT ( 'NONE',  ( 76.82820088796398750, 11.97361217437780034, -14.64015420985709959 ) ) ;
#27597 = CARTESIAN_POINT ( 'NONE',  ( 16.13393739769620083, -15.61618894467929941, -6.189999999999999503 ) ) ;
#27598 = CARTESIAN_POINT ( 'NONE',  ( 20.78393739769619941, -15.61618894467929941, -14.03562394879499919 ) ) ;
#27599 = AXIS2_PLACEMENT_3D ( 'NONE', #6727, #50741, #14839 ) ;
#27600 = VERTEX_POINT ( 'NONE', #45408 ) ;
#27601 = AXIS2_PLACEMENT_3D ( 'NONE', #3626, #36873, #20353 ) ;
#27602 = CARTESIAN_POINT ( 'NONE',  ( -10.87300634462279980, -42.35673974988220181, -6.273959123267670357 ) ) ;
#27603 = TOROIDAL_SURFACE ( 'NONE', #10909, 9.000000000000000000, 1.000000000000000000 ) ;
#27604 = CARTESIAN_POINT ( 'NONE',  ( 9.127429636406475311, -55.01082058323148516, -22.14349223871027306 ) ) ;
#27605 = LINE ( 'NONE', #102, #16157 ) ;
#27606 = CARTESIAN_POINT ( 'NONE',  ( 63.18512348867459849, 1.274277262446050107, -62.58867475943009850 ) ) ;
#27607 = CARTESIAN_POINT ( 'NONE',  ( 57.43802301110889630, -50.15325042756680318, -52.64491009731540316 ) ) ;
#27608 = CARTESIAN_POINT ( 'NONE',  ( 42.52205268124630066, 12.26030094018719829, -4.456987777771080239 ) ) ;
#27609 = LINE ( 'NONE', #3259, #33400 ) ;
#27610 = CARTESIAN_POINT ( 'NONE',  ( 73.34727812780759848, -45.11618894467940066, -14.85468426629290128 ) ) ;
#27611 = DIRECTION ( 'NONE',  ( -1.000000000000000000, 0.000000000000000000, 0.000000000000000000 ) ) ;
#27612 = CARTESIAN_POINT ( 'NONE',  ( 68.13393739769840352, -50.61618894467879670, -73.25000000000220268 ) ) ;
#27613 = CARTESIAN_POINT ( 'NONE',  ( 68.13393739769625768, -15.41618894467990764, -28.20067248431510976 ) ) ;
#27614 = CARTESIAN_POINT ( 'NONE',  ( 17.72038853882659737, -51.81226317974009987, -75.66803551354809088 ) ) ;
#27615 = CARTESIAN_POINT ( 'NONE',  ( 16.13393739769620083, -15.61618894467929941, -6.928362978644219794 ) ) ;
#27616 = CARTESIAN_POINT ( 'NONE',  ( 21.70451063365279865, -20.56345163845099933, -65.29850096567270157 ) ) ;
#27617 = CARTESIAN_POINT ( 'NONE',  ( 47.07753517504149698, 8.029056321811339103, -34.91082242604309727 ) ) ;
#27618 = CARTESIAN_POINT ( 'NONE',  ( 63.38217364139809007, 0.9405967369938039724, -61.98545004926849344 ) ) ;
#27619 = EDGE_LOOP ( 'NONE', ( #38394, #4593, #1927, #19520 ) ) ;
#27620 = DIRECTION ( 'NONE',  ( -0.5516667872527302174, -0.8340645993220495713, 0.000000000000000000 ) ) ;
#27621 = CARTESIAN_POINT ( 'NONE',  ( 68.13393739769620083, -42.11618894467930119, -71.65000000000000568 ) ) ;
#27622 = CARTESIAN_POINT ( 'NONE',  ( 73.24758132965840218, 0.8838110553206759423, -68.78868353141480441 ) ) ;
#27623 = DIRECTION ( 'NONE',  ( 0.000000000000000000, 0.000000000000000000, -1.000000000000000000 ) ) ;
#27624 = CARTESIAN_POINT ( 'NONE',  ( 9.045058299293090798, -14.07202885548180049, -81.23899999999999011 ) ) ;
#27625 = ORIENTED_EDGE ( 'NONE', *, *, #29926, .F. ) ;
#27626 = EDGE_CURVE ( 'NONE', #26340, #13860, #37405, .T. ) ;
#27627 = CARTESIAN_POINT ( 'NONE',  ( 18.22266512930399784, 21.07290090200189780, -75.74020909530109691 ) ) ;
#27628 = EDGE_LOOP ( 'NONE', ( #16932, #48816, #29912, #17963, #51507, #18166 ) ) ;
#27629 = ADVANCED_FACE ( 'NONE', ( #18904 ), #10546, .T. ) ;
#27630 = ORIENTED_EDGE ( 'NONE', *, *, #45187, .F. ) ;
#27631 = DIRECTION ( 'NONE',  ( -1.000000000000000000, 0.000000000000000000, 0.000000000000000000 ) ) ;
#27632 = B_SPLINE_CURVE_WITH_KNOTS ( 'NONE', 3,
 ( #16598, #32551, #48586, #12687, #44642, #45948, #49879, #21296, #42271, #18409, #13974, #29931, #26003, #21556, #17895, #45686, #38336, #26265, #29676, #10039, #10303, #22070, #38079, #49371, #17387 ),
 .UNSPECIFIED., .F., .F.,
 ( 4, 1, 1, 1, 2, 2, 1, 2, 2, 1, 2, 2, 2, 2, 4 ),
 ( 0.000000000000000000, 0.1250000000000037748, 0.1875000000000047184, 0.2187500000000053846, 0.2343750000000057176, 0.2500000000000060507, 0.3125000000000070499, 0.3437500000000067168, 0.3750000000000063838, 0.4375000000000049960, 0.4687500000000051070, 0.5000000000000052180, 0.6250000000000039968, 0.7500000000000027756, 1.000000000000000000 ),
 .UNSPECIFIED. ) ;
#27633 = CARTESIAN_POINT ( 'NONE',  ( 22.43307764042800301, -11.02875726361830111, -81.23899999999999011 ) ) ;
#27634 = CARTESIAN_POINT ( 'NONE',  ( 61.61165453121049751, 14.00280548404949954, -47.05504859273239759 ) ) ;
#27635 = VERTEX_POINT ( 'NONE', #46199 ) ;
#27636 = CARTESIAN_POINT ( 'NONE',  ( 68.13393739769620083, -48.61618894467930119, -65.65000000000000568 ) ) ;
#27637 = VERTEX_POINT ( 'NONE', #38845 ) ;
#27638 = CARTESIAN_POINT ( 'NONE',  ( 20.99563574407254407, -9.290039920899717529, -63.50066641288683655 ) ) ;
#27639 = CARTESIAN_POINT ( 'NONE',  ( 57.24929578595760660, 19.38381105532069881, -74.14999999999999147 ) ) ;
#27640 = VECTOR ( 'NONE', #9031, 1000.000000000000000 ) ;
#27641 = AXIS2_PLACEMENT_3D ( 'NONE', #20922, #28263, #16228 ) ;
#27643 = ORIENTED_EDGE ( 'NONE', *, *, #110, .T. ) ;
#27642 =( BOUNDED_CURVE ( )  B_SPLINE_CURVE ( 3, ( #39804, #32165, #15960, #48181 ),
 .UNSPECIFIED., .F., .T. ) 
 B_SPLINE_CURVE_WITH_KNOTS ( ( 4, 4 ),
 ( 5.497787143782128183, 6.283185307179577350 ),
 .UNSPECIFIED. ) 
 CURVE ( )  GEOMETRIC_REPRESENTATION_ITEM ( )  RATIONAL_B_SPLINE_CURVE ( ( 1.000000000000000000, 0.9492530216741897897, 0.9492530216741897897, 1.000000000000000000 ) ) 
 REPRESENTATION_ITEM ( '' )  );
#27644 = DIRECTION ( 'NONE',  ( 0.000000000000000000, 5.418249000000000090E-13, 1.000000000000000000 ) ) ;
#27645 = CARTESIAN_POINT ( 'NONE',  ( 51.49462705094970261, -51.12905048845459532, -76.11693519191881308 ) ) ;
#27646 = CIRCLE ( 'NONE', #906, 0.5000000000000028866 ) ;
#27647 = CARTESIAN_POINT ( 'NONE',  ( 61.29825847224779523, 14.29443508044710143, -47.59225652243549831 ) ) ;
#27648 = DIRECTION ( 'NONE',  ( -0.5516667872527557526, 0.8340645993220324739, 0.000000000000000000 ) ) ;
#27649 = DIRECTION ( 'NONE',  ( 0.000000000000000000, 0.000000000000000000, 1.000000000000000000 ) ) ;
#27650 = CARTESIAN_POINT ( 'NONE',  ( -3.908839563797870120, 17.07291065422449705, -5.445805040184419354 ) ) ;
#27651 = CYLINDRICAL_SURFACE ( 'NONE', #31241, 0.4999999999999967248 ) ;
#27652 = CARTESIAN_POINT ( 'NONE',  ( 22.90018981389043873, -16.24635821130550539, -38.87681876136569770 ) ) ;
#27653 = CARTESIAN_POINT ( 'NONE',  ( 8.856465214167128508, -12.67932892058150074, -64.40959883343289505 ) ) ;
#27654 = ORIENTED_EDGE ( 'NONE', *, *, #13957, .F. ) ;
#27655 = CARTESIAN_POINT ( 'NONE',  ( 56.83722671258179560, -50.65906061578299813, -53.85090158306050512 ) ) ;
#27656 = ADVANCED_FACE ( 'NONE', ( #18137 ), #2406, .T. ) ;
#27657 = CARTESIAN_POINT ( 'NONE',  ( 41.43966039318529937, 14.40677330313000049, -6.362507098331501076 ) ) ;
#27658 = CARTESIAN_POINT ( 'NONE',  ( 71.70128097442669457, 1.382578538659040124, -70.18625692817499839 ) ) ;
#27659 = CARTESIAN_POINT ( 'NONE',  ( 43.66028230008726041, -39.92605316001158400, -68.30461377173425319 ) ) ;
#27660 = ADVANCED_FACE ( 'NONE', ( #50114 ), #50629, .T. ) ;
#27661 = CARTESIAN_POINT ( 'NONE',  ( 14.22165922051550169, 19.31192048736480160, -21.01402899345969999 ) ) ;
#27662 = ADVANCED_FACE ( 'NONE', ( #10019 ), #25981, .T. ) ;
#27663 = CARTESIAN_POINT ( 'NONE',  ( 12.53549334626059952, 18.74519656086519959, -21.12176656462050062 ) ) ;
#27664 = CARTESIAN_POINT ( 'NONE',  ( 63.22228946811700467, 1.003508719580009867, -69.08444824154609876 ) ) ;
#27665 = CARTESIAN_POINT ( 'NONE',  ( 48.74537093715300529, -53.89676824263879951, -54.52146652541890148 ) ) ;
#27666 = DIRECTION ( 'NONE',  ( 1.000000000000000000, 0.000000000000000000, 0.000000000000000000 ) ) ;
#27667 = CARTESIAN_POINT ( 'NONE',  ( 63.95040967837099544, 1.031857118852239852, -69.95114096137160686 ) ) ;
#27668 = CARTESIAN_POINT ( 'NONE',  ( 22.46012080236426911, -20.47784194944630443, -37.71600417800252103 ) ) ;
#27669 = CARTESIAN_POINT ( 'NONE',  ( 24.04468322966528859, -15.61618861995729013, -71.79233702014498419 ) ) ;
#27670 = ORIENTED_EDGE ( 'NONE', *, *, #33653, .F. ) ;
#27671 = CARTESIAN_POINT ( 'NONE',  ( 18.73669033277520057, -8.635331440240550549, -38.68094012829649841 ) ) ;
#27672 = CARTESIAN_POINT ( 'NONE',  ( 9.366428224829499882, -15.61611423639980067, -77.45282021618989177 ) ) ;
#27673 = VERTEX_POINT ( 'NONE', #14464 ) ;
#27674 = CARTESIAN_POINT ( 'NONE',  ( 68.13393739769618662, -0.5161889446793590519, -65.65000000000000568 ) ) ;
#27675 = CIRCLE ( 'NONE', #47782, 2.000000000000001332 ) ;
#27676 = CARTESIAN_POINT ( 'NONE',  ( 60.70114797779579874, -45.57531533405330748, -47.37795440859400031 ) ) ;
#27677 = LINE ( 'NONE', #39745, #43810 ) ;
#27678 = CARTESIAN_POINT ( 'NONE',  ( 27.50893739769620083, -36.61730498645199816, -35.14999999999999858 ) ) ;
#27679 = EDGE_CURVE ( 'NONE', #13493, #45801, #6352, .T. ) ;
#27681 = LINE ( 'NONE', #51289, #33959 ) ;
#27680 = CARTESIAN_POINT ( 'NONE',  ( 41.77940164082745156, 8.508192307914475450, -77.39573496664088736 ) ) ;
#27682 = VECTOR ( 'NONE', #33504, 1000.000000000000000 ) ;
#27683 = DIRECTION ( 'NONE',  ( 0.000000000000000000, 0.000000000000000000, 1.000000000000000000 ) ) ;
#27684 = CARTESIAN_POINT ( 'NONE',  ( 16.13393739769620083, -15.61618894467929941, -41.69811738492444420 ) ) ;
#27685 = ORIENTED_EDGE ( 'NONE', *, *, #6922, .F. ) ;
#27686 = CARTESIAN_POINT ( 'NONE',  ( 0.06064750360406240270, 19.78548888128160144, -34.82147232542479998 ) ) ;
#27687 = ORIENTED_EDGE ( 'NONE', *, *, #18442, .T. ) ;
#27688 = EDGE_CURVE ( 'NONE', #13415, #4297, #29758, .T. ) ;
#27689 = EDGE_LOOP ( 'NONE', ( #27736, #33707, #34186, #42233, #30329 ) ) ;
#27690 = CYLINDRICAL_SURFACE ( 'NONE', #6029, 7.910999999999997812 ) ;
#27691 = CARTESIAN_POINT ( 'NONE',  ( 8.222921866017912862, -14.58075518776391810, -38.83399696775236976 ) ) ;
#27692 = CARTESIAN_POINT ( 'NONE',  ( 12.75847677693120197, 34.25788405235230272, -47.26854789455460093 ) ) ;
#27693 = CARTESIAN_POINT ( 'NONE',  ( 12.19850843269619922, -65.41247318024639412, -47.44469434798769925 ) ) ;
#27694 = ORIENTED_EDGE ( 'NONE', *, *, #11492, .F. ) ;
#27695 = CARTESIAN_POINT ( 'NONE',  ( 16.13393739769620083, -15.61618894467929941, 14.34999999999999964 ) ) ;
#27696 = CARTESIAN_POINT ( 'NONE',  ( 56.80588353391389944, -45.24242660625780132, -25.29585452565680015 ) ) ;
#27697 = CARTESIAN_POINT ( 'NONE',  ( 56.46328325841249551, -50.76386906370840535, -53.62058756809589255 ) ) ;
#27698 = CARTESIAN_POINT ( 'NONE',  ( 22.77734342274874280, -14.28677838390695776, -46.38995319782638660 ) ) ;
#27699 = CARTESIAN_POINT ( 'NONE',  ( 59.04067005502180621, -2.813652991295200412, -15.65184294716019942 ) ) ;
#27700 = CARTESIAN_POINT ( 'NONE',  ( 51.85163801358509517, -49.58237482539740171, -76.86771389695809376 ) ) ;
#27701 = FACE_OUTER_BOUND ( 'NONE', #9726, .T. ) ;
#27702 = ORIENTED_EDGE ( 'NONE', *, *, #12380, .T. ) ;
#27703 = CARTESIAN_POINT ( 'NONE',  ( 63.93393739769594930, 10.88381105532010551, -61.44999999999983231 ) ) ;
#27704 = LINE ( 'NONE', #51316, #37636 ) ;
#27705 = CARTESIAN_POINT ( 'NONE',  ( 9.984421472749652082, -12.69805524141423270, -33.59399944151634543 ) ) ;
#27706 = DIRECTION ( 'NONE',  ( 1.000000000000000000, 0.000000000000000000, 0.000000000000000000 ) ) ;
#27707 = CARTESIAN_POINT ( 'NONE',  ( 22.54949557071089927, -20.13585275078779802, -54.20785061676599526 ) ) ;
#27708 = CARTESIAN_POINT ( 'NONE',  ( 17.76831794872855141, -41.98180839364705008, -34.64999999999999858 ) ) ;
#27709 = CARTESIAN_POINT ( 'NONE',  ( 55.87921360396619974, 19.38381105532069881, -76.16089020870099091 ) ) ;
#27710 = DIRECTION ( 'NONE',  ( 1.000000000000000000, 0.000000000000000000, 0.000000000000000000 ) ) ;
#27711 = CARTESIAN_POINT ( 'NONE',  ( 55.82174411980109596, 13.88381105532070059, -14.52096170695349997 ) ) ;
#27712 = CARTESIAN_POINT ( 'NONE',  ( 60.67373791137799799, -45.55123872289310327, -47.14825100140640757 ) ) ;
#27713 = VECTOR ( 'NONE', #14602, 1000.000000000000000 ) ;
#27714 = CARTESIAN_POINT ( 'NONE',  ( 19.54195640215267460, -21.52908387663484291, -38.78615563590209803 ) ) ;
#27715 = CARTESIAN_POINT ( 'NONE',  ( 9.436316225021858628, -13.40611433014809961, -57.94863426729589406 ) ) ;
#27716 = CARTESIAN_POINT ( 'NONE',  ( 16.13393739769620083, -15.61618894467929941, -28.45282021618999835 ) ) ;
#27717 = AXIS2_PLACEMENT_3D ( 'NONE', #32765, #9482, #48790 ) ;
#27718 = EDGE_LOOP ( 'NONE', ( #7736, #48922, #46719, #931, #45637 ) ) ;
#27719 = DIRECTION ( 'NONE',  ( 1.000000000000000000, 0.000000000000000000, -1.224646799147353207E-16 ) ) ;
#27720 = ADVANCED_FACE ( 'NONE', ( #14726 ), #30179, .T. ) ;
#27721 = DIRECTION ( 'NONE',  ( 0.000000000000000000, 0.000000000000000000, 1.000000000000000000 ) ) ;
#27722 = CARTESIAN_POINT ( 'NONE',  ( 0.1457841021255935343, -4.451138319363987073, -34.68167779225149161 ) ) ;
#27723 = EDGE_CURVE ( 'NONE', #17152, #28405, #48188, .T. ) ;
#27724 = CARTESIAN_POINT ( 'NONE',  ( 14.39524263072926047, -51.26000751222474605, -74.91995119710422557 ) ) ;
#27725 = EDGE_CURVE ( 'NONE', #37443, #51612, #30946, .T. ) ;
#27726 = CARTESIAN_POINT ( 'NONE',  ( 8.737696419500725398, -48.93815596428014203, -34.78557451168259007 ) ) ;
#27727 = CARTESIAN_POINT ( 'NONE',  ( 0.02075511821175915136, 19.53788625088298048, -34.74841884006161052 ) ) ;
#27728 = ADVANCED_FACE ( 'NONE', ( #42253 ), #19754, .F. ) ;
#27729 = CARTESIAN_POINT ( 'NONE',  ( 11.43830175784020042, 34.12894736269659290, -18.07704217307109928 ) ) ;
#27730 = CARTESIAN_POINT ( 'NONE',  ( 72.88570115400600002, 0.9405967369906039766, -69.31454995071669600 ) ) ;
#27732 = LINE ( 'NONE', #19099, #15591 ) ;
#27731 = DIRECTION ( 'NONE',  ( 1.000000000000000000, 0.000000000000000000, 0.000000000000000000 ) ) ;
#27733 = CARTESIAN_POINT ( 'NONE',  ( 82.13853704237929776, -45.11618894467940066, -46.37203261889099792 ) ) ;
#27734 = CYLINDRICAL_SURFACE ( 'NONE', #38846, 0.4999999999999982236 ) ;
#27735 = CARTESIAN_POINT ( 'NONE',  ( 49.05097002867299949, 22.69010155233289794, -55.04456405487339765 ) ) ;
#27736 = ORIENTED_EDGE ( 'NONE', *, *, #14477, .F. ) ;
#27737 = CARTESIAN_POINT ( 'NONE',  ( 53.48011204154060039, -49.37340621726109902, -49.05829711586440567 ) ) ;
#27738 = ORIENTED_EDGE ( 'NONE', *, *, #46272, .T. ) ;
#27739 = CARTESIAN_POINT ( 'NONE',  ( 44.14073854797647556, 6.492434696291280893, -69.57759189706122527 ) ) ;
#27740 = CARTESIAN_POINT ( 'NONE',  ( 10.22109192583901560, -19.02429315089245776, -75.28615355149135269 ) ) ;
#27742 = EDGE_CURVE ( 'NONE', #12820, #26692, #36464, .T. ) ;
#27741 = DIRECTION ( 'NONE',  ( 0.000000000000000000, 1.000000000000000000, 0.000000000000000000 ) ) ;
#27743 = CARTESIAN_POINT ( 'NONE',  ( 51.70989020309399109, -48.92491896723970513, -77.02393701242800716 ) ) ;
#27744 = CARTESIAN_POINT ( 'NONE',  ( 16.63319231246079966, -8.581041239996130443, -57.97537152673989880 ) ) ;
#27745 = DIRECTION ( 'NONE',  ( 1.000000000000000000, 0.000000000000000000, 0.000000000000000000 ) ) ;
#27746 = CARTESIAN_POINT ( 'NONE',  ( 56.55503449515249770, -45.27146332001730400, -16.89072690454599979 ) ) ;
#27747 = CARTESIAN_POINT ( 'NONE',  ( 53.72005416868749705, 17.35859260027000062, -26.34191669766330079 ) ) ;
#27748 = VERTEX_POINT ( 'NONE', #34625 ) ;
#27749 = CARTESIAN_POINT ( 'NONE',  ( 15.53783599433159957, -7.791138702023379992, -44.76330392965529370 ) ) ;
#27750 = EDGE_CURVE ( 'NONE', #14841, #33088, #40601, .T. ) ;
#27751 = ORIENTED_EDGE ( 'NONE', *, *, #39030, .F. ) ;
#27752 = CARTESIAN_POINT ( 'NONE',  ( 11.19833792948340090, -65.16806354647678745, -17.40716438213639705 ) ) ;
#27753 = CARTESIAN_POINT ( 'NONE',  ( 12.52666257856989951, 34.23916454258710473, -47.57015704360200203 ) ) ;
#27754 = CARTESIAN_POINT ( 'NONE',  ( 73.05322604375929529, 1.097545367735389910, -62.28124518314879765 ) ) ;
#27755 = CIRCLE ( 'NONE', #47051, 4.296700167715679086 ) ;
#27756 = CARTESIAN_POINT ( 'NONE',  ( 52.09592895031209991, -50.80234781981220493, -50.78436303379759664 ) ) ;
#27757 = CARTESIAN_POINT ( 'NONE',  ( 8.803701492139829554, 31.98286322187070141, -46.67019247816079286 ) ) ;
#27758 = DIRECTION ( 'NONE',  ( 0.000000000000000000, -1.000000000000000000, 0.000000000000000000 ) ) ;
#27759 = CIRCLE ( 'NONE', #19386, 31.45861873485090143 ) ;
#27760 = VECTOR ( 'NONE', #1127, 1000.000000000000114 ) ;
#27761 = ORIENTED_EDGE ( 'NONE', *, *, #32152, .F. ) ;
#27762 = CARTESIAN_POINT ( 'NONE',  ( 64.97340239734430156, 1.393731187554809958, -70.25064478522961053 ) ) ;
#27763 = CARTESIAN_POINT ( 'NONE',  ( 11.13393739769619906, -63.42417329230280387, -43.75301033632869263 ) ) ;
#27764 = CARTESIAN_POINT ( 'NONE',  ( 67.04038824939814845, 19.47158195952278703, -71.50000000000200373 ) ) ;
#27765 = VERTEX_POINT ( 'NONE', #38318 ) ;
#27766 = CARTESIAN_POINT ( 'NONE',  ( 8.222290034161709116, -15.61613760572089937, -44.79233150823699816 ) ) ;
#27767 = CARTESIAN_POINT ( 'NONE',  ( 56.85513652204900126, 19.27500186593999842, -53.07093444364119961 ) ) ;
#27768 = CARTESIAN_POINT ( 'NONE',  ( 20.53874876090047863, -9.019602519203475666, -49.19511954482316440 ) ) ;
#27769 = EDGE_LOOP ( 'NONE', ( #14491, #37619, #35568, #2095 ) ) ;
#27770 = CARTESIAN_POINT ( 'NONE',  ( 8.428838373751766255, -17.68687216982602095, -36.42433490654720174 ) ) ;
#27771 = CARTESIAN_POINT ( 'NONE',  ( 19.28172483834616457, -49.83962866466755059, -82.44267625234891739 ) ) ;
#27772 = CARTESIAN_POINT ( 'NONE',  ( 8.222963747489538733, -14.58044856772349895, -56.54933511702171245 ) ) ;
#27773 = CARTESIAN_POINT ( 'NONE',  ( 56.44284150913800602, 14.76297046884359965, -45.11789043107459918 ) ) ;
#27774 = EDGE_CURVE ( 'NONE', #29389, #15078, #22240, .T. ) ;
#27775 = CARTESIAN_POINT ( 'NONE',  ( 9.921146318005629183, -21.03688512285170376, -68.56397102982089109 ) ) ;
#27776 = EDGE_CURVE ( 'NONE', #1527, #13981, #51557, .T. ) ;
#27777 = CARTESIAN_POINT ( 'NONE',  ( 12.37200837385271868, -18.34939036783928046, -9.721247897589949005 ) ) ;
#27778 = CARTESIAN_POINT ( 'NONE',  ( 46.69599177284572988, -38.22215067635794128, -56.83968353337930068 ) ) ;
#27779 = PRODUCT_CONTEXT ( 'NONE', #19408, 'mechanical' ) ;
#27780 = ORIENTED_EDGE ( 'NONE', *, *, #8252, .T. ) ;
#27781 = CARTESIAN_POINT ( 'NONE',  ( 9.292831712696338897, -18.56677648139270076, -67.10304248959609197 ) ) ;
#27782 = CARTESIAN_POINT ( 'NONE',  ( 10.25343679584480050, -20.55147180341439750, -32.14999999999999858 ) ) ;
#27783 = CARTESIAN_POINT ( 'NONE',  ( 47.22841302400619412, 23.19665601663579935, -75.17093853428211503 ) ) ;
#27784 = CARTESIAN_POINT ( 'NONE',  ( -20.36606260510179567, -15.61618894418049308, 9.349999998653533595 ) ) ;
#27785 = DIRECTION ( 'NONE',  ( -0.6023772969742121619, -0.4987169684303940920, -0.6232358923310170606 ) ) ;
#27786 = EDGE_CURVE ( 'NONE', #8412, #40071, #45691, .T. ) ;
#27787 = CIRCLE ( 'NONE', #30327, 6.000000000000005329 ) ;
#27788 = CARTESIAN_POINT ( 'NONE',  ( 11.60439326025529994, 33.70240003096060377, -16.46429631544720351 ) ) ;
#27789 = AXIS2_PLACEMENT_3D ( 'NONE', #24668, #584, #35971 ) ;
#27790 = CARTESIAN_POINT ( 'NONE',  ( 23.44421149204620036, -19.42966680280959935, -73.66071987733648996 ) ) ;
#27791 = ADVANCED_FACE ( 'NONE', ( #31970 ), #39355, .F. ) ;
#27792 = CARTESIAN_POINT ( 'NONE',  ( 22.72757484624980151, -19.35329995587120067, -32.14999999999999858 ) ) ;
#27793 = CARTESIAN_POINT ( 'NONE',  ( 55.24960754175609878, -50.62333154088300091, -76.30022807136839447 ) ) ;
#27795 = CYLINDRICAL_SURFACE ( 'NONE', #36428, 0.4999999999999982236 ) ;
#27794 = CARTESIAN_POINT ( 'NONE',  ( -6.938047273389929437, 15.02604475192799960, -5.910678614907980410 ) ) ;
#27796 = CARTESIAN_POINT ( 'NONE',  ( 63.15706468848460275, 1.190292248953970011, -68.82164347790129000 ) ) ;
#27797 = CARTESIAN_POINT ( 'NONE',  ( 61.22003255449720172, 14.03468818129520024, -46.76603150336679704 ) ) ;
#27798 = CARTESIAN_POINT ( 'NONE',  ( 8.428865626044137471, -13.54540663567643399, -78.59100198268760096 ) ) ;
#27799 = CARTESIAN_POINT ( 'NONE',  ( 66.70013194292150160, -1.463538230407920082, -17.02746303015019791 ) ) ;
#27800 = VERTEX_POINT ( 'NONE', #28043 ) ;
#27801 = CARTESIAN_POINT ( 'NONE',  ( 53.39109823518269593, -49.36681769490010652, -48.76214596301609561 ) ) ;
#27802 = CARTESIAN_POINT ( 'NONE',  ( 58.98985417505780049, -45.56972936611299474, -26.56632039979439952 ) ) ;
#27803 = CARTESIAN_POINT ( 'NONE',  ( 14.59138716251818479, -23.39588144484022436, -66.35464036535437060 ) ) ;
#27804 = CARTESIAN_POINT ( 'NONE',  ( 75.41048247916201319, -50.61618894467930119, -82.11365365517009707 ) ) ;
#27805 = CARTESIAN_POINT ( 'NONE',  ( 9.116028935892819263, -18.11731961437540050, -73.12368125043110467 ) ) ;
#27806 = CARTESIAN_POINT ( 'NONE',  ( 51.63757600187660302, 18.40000253807760089, -76.65049568453349593 ) ) ;
#27807 = CARTESIAN_POINT ( 'NONE',  ( 52.90334277911429695, 18.39508939093590101, -48.83356293938759762 ) ) ;
#27808 = CARTESIAN_POINT ( 'NONE',  ( 52.83011299386760129, -49.66073358055960085, -48.49877547121819532 ) ) ;
#27809 = ORIENTED_EDGE ( 'NONE', *, *, #37329, .F. ) ;
#27810 = CARTESIAN_POINT ( 'NONE',  ( 23.32430482491550094, 18.10127401595489971, -34.64999999999999858 ) ) ;
#27811 = CARTESIAN_POINT ( 'NONE',  ( 47.77031587149589598, -54.42339131114619732, -54.72319043475250311 ) ) ;
#27812 = DIRECTION ( 'NONE',  ( 0.000000000000000000, -1.000000000000000000, 0.000000000000000000 ) ) ;
#27813 = CARTESIAN_POINT ( 'NONE',  ( -1.866062602303798723, -15.61618894467929763, -20.58999999999999986 ) ) ;
#27814 = CARTESIAN_POINT ( 'NONE',  ( 60.73270329006090407, -30.50852859027810027, -16.25406692276280296 ) ) ;
#27815 = CARTESIAN_POINT ( 'NONE',  ( 71.25658036288379549, 1.391252479931859964, -61.03617692120100457 ) ) ;
#27816 = CARTESIAN_POINT ( 'NONE',  ( 16.13393739769620083, -1.759782484128330049, -35.14999999999999858 ) ) ;
#27817 = CARTESIAN_POINT ( 'NONE',  ( 72.49434596780521645, 1.056850087111250058, -61.52764073002409617 ) ) ;
#27818 = CARTESIAN_POINT ( 'NONE',  ( 51.67587649748470113, -33.96749857170579645, -77.01363636363508647 ) ) ;
#27819 = CARTESIAN_POINT ( 'NONE',  ( 17.63393739769629676, 0.9255523191756780399, -34.64999999999999858 ) ) ;
#27820 = ORIENTED_EDGE ( 'NONE', *, *, #5685, .T. ) ;
#27821 = ORIENTED_EDGE ( 'NONE', *, *, #22096, .F. ) ;
#27822 = B_SPLINE_CURVE_WITH_KNOTS ( 'NONE', 3,
 ( #21407, #2477, #48965, #30501, #29022, #41086, #9388, #9118, #33461, #16990, #32938, #26568, #13069, #1510, #37409, #17494 ),
 .UNSPECIFIED., .F., .F.,
 ( 4, 2, 2, 2, 2, 2, 2, 4 ),
 ( -1.896558999999999901E-14, 0.4421500870759600410, 0.9474644723056518947, 1.263285963074209928, 1.421196708458489999, 1.673853901073330208, 2.078105409257089864, 2.526571926148439839 ),
 .UNSPECIFIED. ) ;
#27823 = DIRECTION ( 'NONE',  ( -1.000000000000000000, 0.000000000000000000, 0.000000000000000000 ) ) ;
#27824 = CARTESIAN_POINT ( 'NONE',  ( 51.01176328416968886, -31.39810158946774266, -16.86084553931457464 ) ) ;
#27825 = VERTEX_POINT ( 'NONE', #16011 ) ;
#27826 = CARTESIAN_POINT ( 'NONE',  ( 57.15402662460559924, -45.14613312479689711, -25.30846757484389897 ) ) ;
#27827 = CARTESIAN_POINT ( 'NONE',  ( 16.12583665212202533, -23.52718583135971997, -78.00799738171198783 ) ) ;
#27828 = B_SPLINE_CURVE_WITH_KNOTS ( 'NONE', 3,
 ( #34863, #42754, #19139, #7108, #30410, #30667, #38558, #50864, #46951, #50354 ),
 .UNSPECIFIED., .F., .F.,
 ( 4, 2, 2, 2, 4 ),
 ( -0.1857717838173399971, -0.1853436703578560107, -0.1652145016253949994, -0.1459149143061169995, -0.1350635247397783956 ),
 .UNSPECIFIED. ) ;
#27829 = ORIENTED_EDGE ( 'NONE', *, *, #41647, .F. ) ;
#27830 = AXIS2_PLACEMENT_3D ( 'NONE', #11552, #23304, #14697 ) ;
#27831 = CARTESIAN_POINT ( 'NONE',  ( 21.75737274077464178, -19.46263012217717403, -80.64360312776651085 ) ) ;
#27832 = CARTESIAN_POINT ( 'NONE',  ( 43.95317894857520002, 6.678920976524271857, -70.55372978514877502 ) ) ;
#27833 = CARTESIAN_POINT ( 'NONE',  ( 63.88393739769619373, 11.88381105532070059, -61.34712802272770915 ) ) ;
#27834 = EDGE_CURVE ( 'NONE', #37056, #14308, #23842, .T. ) ;
#27835 = CARTESIAN_POINT ( 'NONE',  ( 9.078410285617929176, -19.88259928906289886, -38.61921508777280110 ) ) ;
#27836 = EDGE_CURVE ( 'NONE', #51003, #34442, #47990, .T. ) ;
#27837 = CARTESIAN_POINT ( 'NONE',  ( 24.04493737978153689, -16.65173533839766051, -67.54933246951844694 ) ) ;
#27838 = CARTESIAN_POINT ( 'NONE',  ( 59.49262858449159808, 17.38381105532069881, -53.92796738110899923 ) ) ;
#27839 = ADVANCED_FACE ( 'NONE', ( #11839 ), #11577, .F. ) ;
#27840 = CARTESIAN_POINT ( 'NONE',  ( 61.62576467234210043, -29.29680953590479930, -16.00589161936969873 ) ) ;
#27841 = CARTESIAN_POINT ( 'NONE',  ( 63.06393505168800573, 0.8850831926798620186, -62.44126551166660022 ) ) ;
#27842 = CARTESIAN_POINT ( 'NONE',  ( 12.79739587422460012, -22.27759566055959795, -32.88046427011249051 ) ) ;
#27843 = CARTESIAN_POINT ( 'NONE',  ( 19.54193610434072781, -21.52909601099131365, -36.78615172203510753 ) ) ;
#27844 = CARTESIAN_POINT ( 'NONE',  ( 40.74407095721729632, 14.06303216148480040, -5.682177862911860444 ) ) ;
#27845 = CARTESIAN_POINT ( 'NONE',  ( 10.37023549284480595, 23.96649136636277078, -45.75009989963381685 ) ) ;
#27846 = CARTESIAN_POINT ( 'NONE',  ( 82.61657258396949999, -45.26156352634939850, -47.17378930654930258 ) ) ;
#27847 = CARTESIAN_POINT ( 'NONE',  ( 63.75227860486319997, 1.439518482450359960, -69.32544932539248350 ) ) ;
#27848 = CARTESIAN_POINT ( 'NONE',  ( 23.24087076968150001, -19.79640649346030301, -47.67691048846949542 ) ) ;
#27849 = EDGE_CURVE ( 'NONE', #35594, #43797, #27268, .T. ) ;
#27850 = ORIENTED_EDGE ( 'NONE', *, *, #29771, .F. ) ;
#27851 = CARTESIAN_POINT ( 'NONE',  ( 53.17105182305469668, -49.36586906142859732, -27.51403560245880087 ) ) ;
#27852 = CARTESIAN_POINT ( 'NONE',  ( 16.08018489229460002, -51.03388179655710388, -20.24577016824899900 ) ) ;
#27853 = CARTESIAN_POINT ( 'NONE',  ( 24.04462281140675728, -15.61619016268715399, -39.50767146438039390 ) ) ;
#27854 = CARTESIAN_POINT ( 'NONE',  ( 22.55531606818893664, -17.79663561174430697, -56.55696934072006599 ) ) ;
#27855 = CARTESIAN_POINT ( 'NONE',  ( 12.16981617636240109, -50.04926268091029584, -21.14999999999999858 ) ) ;
#27856 = VECTOR ( 'NONE', #40890, 1000.000000000000114 ) ;
#27857 = ORIENTED_EDGE ( 'NONE', *, *, #16854, .F. ) ;
#27858 = DIRECTION ( 'NONE',  ( 0.000000000000000000, 0.000000000000000000, -1.000000000000000000 ) ) ;
#27859 = CARTESIAN_POINT ( 'NONE',  ( 9.807831198552406704, -20.47794271258318943, -38.58399882689687388 ) ) ;
#27860 = CARTESIAN_POINT ( 'NONE',  ( 28.13393739769619728, -8.687985714403851034, -47.64999999999999858 ) ) ;
#27861 = CARTESIAN_POINT ( 'NONE',  ( 63.15863832053869942, 1.096036836948800053, -62.36911566638589477 ) ) ;
#27862 = CARTESIAN_POINT ( 'NONE',  ( 57.37515489807060476, -50.13231850399230183, -52.61654809435920299 ) ) ;
#27863 = CARTESIAN_POINT ( 'NONE',  ( 41.99652641013659604, 13.19240707592760131, -5.118462553216080124 ) ) ;
#27864 = CARTESIAN_POINT ( 'NONE',  ( 24.04493738991158480, -14.58064431297338537, -61.75066186890055064 ) ) ;
#27865 = CARTESIAN_POINT ( 'NONE',  ( 63.71314823352740575, 1.019773975906300034, -61.59278770926519542 ) ) ;
#27866 = DIRECTION ( 'NONE',  ( 0.000000000000000000, 0.000000000000000000, -1.000000000000000000 ) ) ;
#27867 = CARTESIAN_POINT ( 'NONE',  ( 23.64088593898193480, -13.06712279613562266, -75.68818038166295992 ) ) ;
#27868 = CARTESIAN_POINT ( 'NONE',  ( 104.6856170952499951, -2.032350560838469100, -102.2016796975540274 ) ) ;
#27869 = CARTESIAN_POINT ( 'NONE',  ( 17.46613192265609982, -52.40466508994180117, -76.02664804518839503 ) ) ;
#27870 = CARTESIAN_POINT ( 'NONE',  ( 23.31571238671009993, -13.63406827592180015, -64.98162524141820029 ) ) ;
#27871 = DIRECTION ( 'NONE',  ( 0.000000000000000000, -1.000000000000000000, 0.000000000000000000 ) ) ;
#27872 = CARTESIAN_POINT ( 'NONE',  ( 63.39226695650439325, 1.145379646619560043, -62.03974443815909723 ) ) ;
#27873 = ORIENTED_EDGE ( 'NONE', *, *, #36610, .F. ) ;
#27874 = CARTESIAN_POINT ( 'NONE',  ( 8.798174420955659158, 31.95288804203559607, -46.67020513285999783 ) ) ;
#27875 = DIRECTION ( 'NONE',  ( 0.000000000000000000, 1.000000000000000000, 0.000000000000000000 ) ) ;
#27876 = CARTESIAN_POINT ( 'NONE',  ( 9.082179215743179768, -13.83380170031609957, -81.23899999999999011 ) ) ;
#27877 = ORIENTED_EDGE ( 'NONE', *, *, #39185, .F. ) ;
#27878 = CARTESIAN_POINT ( 'NONE',  ( 17.71569765418569986, 21.30155813473500004, -76.03742712147929694 ) ) ;
#27879 = ORIENTED_EDGE ( 'NONE', *, *, #29900, .T. ) ;
#27880 = AXIS2_PLACEMENT_3D ( 'NONE', #12586, #37205, #13120 ) ;
#27881 = B_SPLINE_CURVE_WITH_KNOTS ( 'NONE', 3,
 ( #36018, #636, #8511, #4565 ),
 .UNSPECIFIED., .F., .F.,
 ( 4, 4 ),
 ( 1.172395546643479891, 1.281168487042899873 ),
 .UNSPECIFIED. ) ;
#27882 = ORIENTED_EDGE ( 'NONE', *, *, #6084, .T. ) ;
#27883 = FACE_OUTER_BOUND ( 'NONE', #33678, .T. ) ;
#27884 = CARTESIAN_POINT ( 'NONE',  ( -14.41646913324139589, -53.84900783228822263, 11.34999999999999964 ) ) ;
#27885 = CARTESIAN_POINT ( 'NONE',  ( 15.09848951713014387, -7.705176910871855966, -73.25066484698234603 ) ) ;
#27886 = ORIENTED_EDGE ( 'NONE', *, *, #26887, .F. ) ;
#27887 = CARTESIAN_POINT ( 'NONE',  ( 12.17742756452222963, 33.84218637042627620, -16.46016917631845544 ) ) ;
#27888 = ORIENTED_EDGE ( 'NONE', *, *, #22383, .F. ) ;
#27889 = CARTESIAN_POINT ( 'NONE',  ( 72.38393739883420608, 20.38443354211860026, -61.44999999999999574 ) ) ;
#27890 = EDGE_CURVE ( 'NONE', #40855, #10739, #3455, .T. ) ;
#27891 = CARTESIAN_POINT ( 'NONE',  ( -0.007164427059776000244, -10.48291004383190028, -34.77269723891829756 ) ) ;
#27892 = ORIENTED_EDGE ( 'NONE', *, *, #37070, .F. ) ;
#27893 = AXIS2_PLACEMENT_3D ( 'NONE', #29484, #21608, #10104 ) ;
#27894 = EDGE_LOOP ( 'NONE', ( #51807, #32172, #19713, #11255, #1784 ) ) ;
#27895 = CARTESIAN_POINT ( 'NONE',  ( 12.45398646450647995, -22.71722742353124858, -50.15946686457399295 ) ) ;
#27897 = CARTESIAN_POINT ( 'NONE',  ( 46.44868656089280279, -53.13167745678150311, -76.13981661584659832 ) ) ;
#27896 = AXIS2_PLACEMENT_3D ( 'NONE', #17273, #41113, #49507 ) ;
#27898 = CARTESIAN_POINT ( 'NONE',  ( 61.07726573414930016, 14.36074923854380003, -47.64481375401349794 ) ) ;
#27899 = CARTESIAN_POINT ( 'NONE',  ( 9.366922731475222363, -14.63844643040854976, -39.49882628218075098 ) ) ;
#27900 = CARTESIAN_POINT ( 'NONE',  ( 41.73867462556020058, -43.69499173931319547, -3.496169911638010053 ) ) ;
#27901 = CARTESIAN_POINT ( 'NONE',  ( -9.415595612123681235, 12.56745110274309951, -5.921523228984558962 ) ) ;
#27902 = EDGE_CURVE ( 'NONE', #10739, #46034, #26400, .T. ) ;
#27903 = LINE ( 'NONE', #47085, #20388 ) ;
#27904 = CARTESIAN_POINT ( 'NONE',  ( 57.84059259261429986, 14.33091246258259943, -26.25095046041350244 ) ) ;
#27905 = CARTESIAN_POINT ( 'NONE',  ( 8.436531076600029877, -14.08756730701639803, -62.34990662577889964 ) ) ;
#27906 = EDGE_CURVE ( 'NONE', #19736, #19697, #23331, .T. ) ;
#27907 = ORIENTED_EDGE ( 'NONE', *, *, #31393, .T. ) ;
#27908 = DIRECTION ( 'NONE',  ( 0.000000000000000000, -1.000000000000000000, 0.000000000000000000 ) ) ;
#27909 = CONICAL_SURFACE ( 'NONE', #37136, 19.50000000000000000, 0.2449786631268651149 ) ;
#27910 = CARTESIAN_POINT ( 'NONE',  ( 9.366376358913971245, -15.61615244833809868, -75.84717978381000592 ) ) ;
#27911 = CARTESIAN_POINT ( 'NONE',  ( 11.96660005458890019, -42.11618894467939356, -34.64999999999999858 ) ) ;
#27912 = ADVANCED_FACE ( 'NONE', ( #51662 ), #41491, .F. ) ;
#27913 = CARTESIAN_POINT ( 'NONE',  ( 72.51712974994539707, 1.428542319231139945, -69.37578972296869040 ) ) ;
#27914 = CARTESIAN_POINT ( 'NONE',  ( 42.23111299307110045, -39.78919581839614494, -75.21549960612240682 ) ) ;
#27915 = FILL_AREA_STYLE_COLOUR ( '', #18884 ) ;
#27916 = FACE_OUTER_BOUND ( 'NONE', #26247, .T. ) ;
#27917 = CARTESIAN_POINT ( 'NONE',  ( 47.18305960804269716, 23.57448916799839722, -74.19778952092750046 ) ) ;
#27918 = CARTESIAN_POINT ( 'NONE',  ( 48.76647860316090544, -54.05566106471979992, -55.26728053078139880 ) ) ;
#27919 = CARTESIAN_POINT ( 'NONE',  ( -11.32734372065470119, 10.64934054434680100, -6.430561461456250072 ) ) ;
#27920 = DIRECTION ( 'NONE',  ( -0.7956403955640117820, 0.6057692307692287281, 0.000000000000000000 ) ) ;
#27921 = DIRECTION ( 'NONE',  ( -0.8224686640529098591, 0.3976080002595605012, -0.4067593573362696113 ) ) ;
#27922 = CARTESIAN_POINT ( 'NONE',  ( 24.04493739712419043, -16.65173214393696810, -53.83400119000078377 ) ) ;
#27923 = EDGE_LOOP ( 'NONE', ( #14322, #5917, #29442, #15889 ) ) ;
#27924 = CARTESIAN_POINT ( 'NONE',  ( 21.24586391840339772, -10.75704091599320122, -80.60524855149108703 ) ) ;
#27925 = CARTESIAN_POINT ( 'NONE',  ( 9.543045992446268500, -17.38737032729065390, -77.36949155694581748 ) ) ;
#27926 = EDGE_LOOP ( 'NONE', ( #27687, #44983, #26320, #41554 ) ) ;
#27927 = CARTESIAN_POINT ( 'NONE',  ( 71.46077416446640029, 1.263823323415670163, -70.46116989902598959 ) ) ;
#27928 = CARTESIAN_POINT ( 'NONE',  ( 60.88268456428720299, -45.52259370110750325, -47.42394128263550357 ) ) ;
#27929 = CARTESIAN_POINT ( 'NONE',  ( 47.82353814990211305, -54.39218320395424655, -54.71742302521133894 ) ) ;
#27930 = FACE_OUTER_BOUND ( 'NONE', #50252, .T. ) ;
#27932 = CARTESIAN_POINT ( 'NONE',  ( 23.04647526746508390, -11.63208492753508416, -35.62566255721337427 ) ) ;
#27931 = CARTESIAN_POINT ( 'NONE',  ( 42.01616251554107606, 8.533769718121346770, -76.25424629209925342 ) ) ;
#27933 = DIRECTION ( 'NONE',  ( 1.000000000000000000, 0.000000000000000000, 0.000000000000000000 ) ) ;
#27934 = CARTESIAN_POINT ( 'NONE',  ( 56.76664444810730714, 19.44233945464240065, -53.84360320705440017 ) ) ;
#27935 = VERTEX_POINT ( 'NONE', #20183 ) ;
#27936 = LINE ( 'NONE', #43938, #32284 ) ;
#27937 = VERTEX_POINT ( 'NONE', #282 ) ;
#27938 = CARTESIAN_POINT ( 'NONE',  ( 22.78093346138021502, -17.47720641827233834, -58.93471117284045135 ) ) ;
#27939 = CARTESIAN_POINT ( 'NONE',  ( 53.57529274648619122, -50.54592000773362059, -77.11805841020525065 ) ) ;
#27940 = CARTESIAN_POINT ( 'NONE',  ( 76.39109092966590708, -16.43866963256245484, -12.75812042950594538 ) ) ;
#27941 = ORIENTED_EDGE ( 'NONE', *, *, #3736, .T. ) ;
#27942 = VERTEX_POINT ( 'NONE', #27538 ) ;
#27943 = CARTESIAN_POINT ( 'NONE',  ( 20.99557505903451471, -21.94238661114907529, -55.79928181614338456 ) ) ;
#27944 = LINE ( 'NONE', #35307, #5327 ) ;
#27945 = DIRECTION ( 'NONE',  ( 0.05355673487304404151, 0.9985648081870993620, 0.000000000000000000 ) ) ;
#27946 = AXIS2_PLACEMENT_3D ( 'NONE', #13603, #25623, #28791 ) ;
#27947 = ADVANCED_FACE ( 'NONE', ( #16266 ), #32219, .T. ) ;
#27948 = CARTESIAN_POINT ( 'NONE',  ( 20.63541822830159589, 20.65389878999348738, -69.46507341768980837 ) ) ;
#27949 = CARTESIAN_POINT ( 'NONE',  ( 59.52540514537479766, -1.602101419350890010, -15.86601446510490021 ) ) ;
#27950 = CARTESIAN_POINT ( 'NONE',  ( 51.96022949536530433, -49.99701410684310332, -76.69846579631709460 ) ) ;
#27951 = ORIENTED_EDGE ( 'NONE', *, *, #41129, .F. ) ;
#27952 = CARTESIAN_POINT ( 'NONE',  ( 63.10653712364229762, 0.8879664753683499390, -68.92499589875220067 ) ) ;
#27953 = CARTESIAN_POINT ( 'NONE',  ( 52.24694037885000597, -49.83134711013449447, -77.11046193146449923 ) ) ;
#27954 = CARTESIAN_POINT ( 'NONE',  ( 64.99525386628130263, 0.8838110553206740549, -70.76364393196210756 ) ) ;
#27955 = CARTESIAN_POINT ( 'NONE',  ( 47.13393739769619373, 8.048130187719129580, -35.14999999999999858 ) ) ;
#27956 = CARTESIAN_POINT ( 'NONE',  ( 22.74393318103090067, -11.38597578978039948, -51.83128268485739909 ) ) ;
#27957 = CARTESIAN_POINT ( 'NONE',  ( 13.22847210400979812, -50.60300887283339932, -21.36464641127450292 ) ) ;
#27958 = DIRECTION ( 'NONE',  ( 0.000000000000000000, -1.000000000000000000, 0.000000000000000000 ) ) ;
#27959 = AXIS2_PLACEMENT_3D ( 'NONE', #39311, #34321, #42735 ) ;
#27960 = CARTESIAN_POINT ( 'NONE',  ( 22.90065884458136480, -15.61618680935524317, -64.84717769963093303 ) ) ;
#27961 = CARTESIAN_POINT ( 'NONE',  ( 65.43042069957888884, -49.21324915460513694, -73.25000000000119371 ) ) ;
#27962 = DIRECTION ( 'NONE',  ( 0.000000000000000000, 0.000000000000000000, -1.000000000000000000 ) ) ;
#27963 = DIRECTION ( 'NONE',  ( 1.000000000000000000, 0.000000000000000000, 0.000000000000000000 ) ) ;
#27964 = CARTESIAN_POINT ( 'NONE',  ( 9.549614380104699762, -18.14388544039750073, -55.73050419751459827 ) ) ;
#27965 = CARTESIAN_POINT ( 'NONE',  ( 10.72252174668208546, -11.45764127470922489, -43.66113319608867016 ) ) ;
#27966 = ORIENTED_EDGE ( 'NONE', *, *, #51758, .F. ) ;
#27967 = B_SPLINE_CURVE_WITH_KNOTS ( 'NONE', 3,
 ( #30879, #23266, #27215, #47164, #22760, #14657, #42971, #38252, #10480, #46651, #43227, #38781, #18319, #22503, #39285, #7066, #3393, #6287 ),
 .UNSPECIFIED., .F., .F.,
 ( 4, 2, 2, 2, 2, 2, 2, 2, 4 ),
 ( 0.000000000000000000, 0.1250000000000000000, 0.2500000000000000000, 0.3750000000000000000, 0.5000000000000000000, 0.6250000000000000000, 0.7500000000000000000, 0.8750000000000000000, 1.000000000000000000 ),
 .UNSPECIFIED. ) ;
#27968 = CARTESIAN_POINT ( 'NONE',  ( 13.76101294176279843, -51.29510989453670078, -74.37030622952929093 ) ) ;
#27969 = CARTESIAN_POINT ( 'NONE',  ( 47.21794645697320192, -54.77977332054720705, -54.61771020034730384 ) ) ;
#27970 =( NAMED_UNIT ( * ) SI_UNIT ( $, .STERADIAN. ) SOLID_ANGLE_UNIT ( ) );
#27971 = EDGE_CURVE ( 'NONE', #18473, #10844, #4676, .T. ) ;
#27972 = CARTESIAN_POINT ( 'NONE',  ( 12.91569276136874578, 34.28022004554033941, -47.73039263111912334 ) ) ;
#27973 = CARTESIAN_POINT ( 'NONE',  ( 14.55219295556159409, -51.70197612871098869, -75.56421430877743717 ) ) ;
#27974 = CARTESIAN_POINT ( 'NONE',  ( 60.87387793921017476, -45.45198959003565875, -47.10856926084817786 ) ) ;
#27975 = CARTESIAN_POINT ( 'NONE',  ( 10.69832412670059973, -64.89277703499729455, -17.91220997211459931 ) ) ;
#27976 = CARTESIAN_POINT ( 'NONE',  ( 11.00562562894740104, 33.92899319167229777, -18.07900588225090033 ) ) ;
#27977 = CARTESIAN_POINT ( 'NONE',  ( 20.37502878971641351, -8.918043044671964736, -65.18732621157280960 ) ) ;
#27979 = CARTESIAN_POINT ( 'NONE',  ( 62.09157612670949788, 1.883811055320649963, -65.34607522167520699 ) ) ;
#27978 = CARTESIAN_POINT ( 'NONE',  ( 2.277530937145189949, -15.61618894467929941, -32.14999999999999858 ) ) ;
#27980 = CARTESIAN_POINT ( 'NONE',  ( 14.63258269449462823, -51.92835184173312513, -75.76245441609269449 ) ) ;
#27982 = DIRECTION ( 'NONE',  ( 0.000000000000000000, -1.000000000000000000, 0.000000000000000000 ) ) ;
#27981 = B_SPLINE_CURVE_WITH_KNOTS ( 'NONE', 3,
 ( #28637, #1134, #17129, #21035, #40448, #49111, #875, #13210, #12945, #12415, #20774, #28901, #5081, #9009, #28122, #40196, #16595, #45159 ),
 .UNSPECIFIED., .F., .F.,
 ( 4, 2, 2, 2, 2, 2, 2, 2, 4 ),
 ( 0.5000000033146290157, 0.5625000029003004443, 0.6250000024859717618, 0.6875000020716430793, 0.7500000016573145079, 0.8125000012429859364, 0.8750000008286572539, 0.9375000004143285715, 1.000000000000000000 ),
 .UNSPECIFIED. ) ;
#27983 = CARTESIAN_POINT ( 'NONE',  ( 49.60654698967459808, 22.46544607396180027, -55.15184126837920076 ) ) ;
#27984 = ORIENTED_EDGE ( 'NONE', *, *, #13717, .T. ) ;
#27985 = CARTESIAN_POINT ( 'NONE',  ( 53.33273182090660214, -49.45495365240509500, -49.10545207584610239 ) ) ;
#27986 = ORIENTED_EDGE ( 'NONE', *, *, #51184, .F. ) ;
#27987 = CARTESIAN_POINT ( 'NONE',  ( 43.45629245243522121, 6.417003004502526586, -73.00576010489325540 ) ) ;
#27988 = CARTESIAN_POINT ( 'NONE',  ( 9.543102950792974326, -17.38757742493531566, -75.36948688384066486 ) ) ;
#27989 = DIRECTION ( 'NONE',  ( 1.000000000000000000, 0.000000000000000000, 0.000000000000000000 ) ) ;
#27991 = CARTESIAN_POINT ( 'NONE',  ( 53.68517931677009614, 17.65142714004119995, -27.10739793169170042 ) ) ;
#27990 = CARTESIAN_POINT ( 'NONE',  ( 82.84359872746441056, 13.83656922206100148, -46.75796921614900015 ) ) ;
#27992 = CARTESIAN_POINT ( 'NONE',  ( 15.86297936323760283, -22.66382262132480108, -54.96505214632229297 ) ) ;
#27993 = CARTESIAN_POINT ( 'NONE',  ( 52.71325193919590646, 18.52215315012190189, -48.80820480602550049 ) ) ;
#27994 = CARTESIAN_POINT ( 'NONE',  ( 56.98602282141720110, -45.17932660430339808, -17.93020264185449975 ) ) ;
#27995 = CARTESIAN_POINT ( 'NONE',  ( 0.1457841021255935343, -15.61618894467929941, -34.68167779225149161 ) ) ;
#27996 = EDGE_LOOP ( 'NONE', ( #25811, #30437, #44826, #37046, #11559 ) ) ;
#27997 = CARTESIAN_POINT ( 'NONE',  ( 20.19834834365759590, -8.902969758213549412, -40.96079523860159810 ) ) ;
#27998 = ORIENTED_EDGE ( 'NONE', *, *, #35846, .T. ) ;
#27999 = CARTESIAN_POINT ( 'NONE',  ( 11.69717491040810131, -65.38668361297489184, -17.57872635863940403 ) ) ;
#28000 = CARTESIAN_POINT ( 'NONE',  ( 10.66723504149939927, 32.23676291041770270, -45.40177853144560061 ) ) ;
#28001 = CARTESIAN_POINT ( 'NONE',  ( -2.765096767708109748, -50.45527968746931435, -9.880994752627875855 ) ) ;
#28002 = CARTESIAN_POINT ( 'NONE',  ( 64.93393739769619799, 10.88381105532070059, -68.84999999999999432 ) ) ;
#28003 = CARTESIAN_POINT ( 'NONE',  ( 11.22148308022864072, -65.11920307228105287, -22.94887291969233090 ) ) ;
#28004 = CARTESIAN_POINT ( 'NONE',  ( 51.34655038886756273, 3.358464191959859679, -76.64437763193187436 ) ) ;
#28005 = VERTEX_POINT ( 'NONE', #51149 ) ;
#28006 = CARTESIAN_POINT ( 'NONE',  ( 13.58165716955151403, 20.15897125721314254, -22.62650420658231099 ) ) ;
#28007 = CARTESIAN_POINT ( 'NONE',  ( 11.10564815319149901, -63.39283105347629999, -44.25602923368459329 ) ) ;
#28008 = ADVANCED_FACE ( 'NONE', ( #15504 ), #19680, .T. ) ;
#28009 = CARTESIAN_POINT ( 'NONE',  ( 68.13393739769810509, 19.38381105532030091, -71.50000000000198952 ) ) ;
#28010 = ORIENTED_EDGE ( 'NONE', *, *, #8160, .T. ) ;
#28011 = CARTESIAN_POINT ( 'NONE',  ( 11.55362728243429160, -64.75226678741590547, -44.82234525104323097 ) ) ;
#28012 = CARTESIAN_POINT ( 'NONE',  ( 56.52076750121499771, 19.52121317428709801, -53.72896418895009418 ) ) ;
#28013 = CARTESIAN_POINT ( 'NONE',  ( 13.80798414608321067, -52.11463163829730405, -75.47165350121231597 ) ) ;
#28014 = CARTESIAN_POINT ( 'NONE',  ( 11.36138452961498935, -9.254399639206521755, -48.80268936686415771 ) ) ;
#28015 = VERTEX_POINT ( 'NONE', #15755 ) ;
#28016 = ADVANCED_FACE ( 'NONE', ( #7645 ), #33124, .F. ) ;
#28017 = CARTESIAN_POINT ( 'NONE',  ( 44.13393739769620083, -33.11618894467940066, -54.35294145922159714 ) ) ;
#28018 = CARTESIAN_POINT ( 'NONE',  ( 68.13393739769620083, -50.61618894467930119, -65.65000000000000568 ) ) ;
#28019 = DIRECTION ( 'NONE',  ( 1.000000000000000000, 0.000000000000000000, 0.000000000000000000 ) ) ;
#28020 = FACE_OUTER_BOUND ( 'NONE', #15361, .T. ) ;
#28021 = ADVANCED_FACE ( 'NONE', ( #31458 ), #31709, .F. ) ;
#28022 = CARTESIAN_POINT ( 'NONE',  ( 19.24953057887579888, -23.25004767963920216, -76.16898841192839598 ) ) ;
#28023 = AXIS2_PLACEMENT_3D ( 'NONE', #21132, #25315, #1492 ) ;
#28024 = CARTESIAN_POINT ( 'NONE',  ( 16.13393739769620083, -15.61618894467929941, 17.35000000000000142 ) ) ;
#28025 = CARTESIAN_POINT ( 'NONE',  ( 56.43686078178020438, 19.54004972588730027, -74.42959766581059000 ) ) ;
#28026 = DIRECTION ( 'NONE',  ( 0.000000000000000000, 0.000000000000000000, 1.000000000000000000 ) ) ;
#28027 = EDGE_LOOP ( 'NONE', ( #33017, #20392, #27244, #42543, #26438 ) ) ;
#28028 = CARTESIAN_POINT ( 'NONE',  ( 20.58238051217970366, -21.59264673022000025, -68.52898324874119851 ) ) ;
#28029 = ADVANCED_FACE ( 'NONE', ( #33005 ), #21332, .T. ) ;
#28030 = DIRECTION ( 'NONE',  ( 0.7071067811865473507, 0.7071067811865476838, 0.000000000000000000 ) ) ;
#28031 = CARTESIAN_POINT ( 'NONE',  ( 10.71761651803740101, -21.13360478435039624, -32.14999999999999858 ) ) ;
#28032 = CARTESIAN_POINT ( 'NONE',  ( 47.00520813701670164, 22.91485595127299746, -75.60950524211389734 ) ) ;
#28033 = CARTESIAN_POINT ( 'NONE',  ( 47.13393739769619373, -38.60474673416580060, -54.64997574802373492 ) ) ;
#28034 = EDGE_CURVE ( 'NONE', #5352, #28199, #39799, .T. ) ;
#28035 = CARTESIAN_POINT ( 'NONE',  ( 57.26570439199549867, 16.10442508092609870, -47.75313496841199878 ) ) ;
#28036 = CARTESIAN_POINT ( 'NONE',  ( 12.07459604305180001, 33.59801851824129670, -16.11467485432109825 ) ) ;
#28037 = CARTESIAN_POINT ( 'NONE',  ( 20.50233011740730049, -8.623345048570200788, -73.18540629095480199 ) ) ;
#28038 = CARTESIAN_POINT ( 'NONE',  ( 56.07071590434600239, -50.62114172542430168, -75.80509802105420647 ) ) ;
#28040 = CARTESIAN_POINT ( 'NONE',  ( 41.70634816843200809, -39.79356890906309729, -77.49277520938784392 ) ) ;
#28039 = CARTESIAN_POINT ( 'NONE',  ( -11.08670663458990013, 10.41904260857310049, -5.029111395560210696 ) ) ;
#28041 = CARTESIAN_POINT ( 'NONE',  ( 63.11000452699359897, 0.9945465939392450494, -68.91635399151641650 ) ) ;
#28042 = CARTESIAN_POINT ( 'NONE',  ( 61.25723346457989749, 14.07825924033359932, -47.12448165822169699 ) ) ;
#28043 = CARTESIAN_POINT ( 'NONE',  ( 8.223516320988901285, -15.61608250808600040, -78.50766849176299900 ) ) ;
#28044 = EDGE_LOOP ( 'NONE', ( #17394, #42546, #31125, #5315 ) ) ;
#28045 = CARTESIAN_POINT ( 'NONE',  ( 52.89416330280510437, -49.62717582914000047, -48.70339649242369973 ) ) ;
#28046 = ADVANCED_FACE ( 'NONE', ( #11254 ), #23528, .T. ) ;
#28047 = CARTESIAN_POINT ( 'NONE',  ( 60.27964521196050640, -45.35349871132130062, -26.98636702841220014 ) ) ;
#28048 = AXIS2_PLACEMENT_3D ( 'NONE', #45010, #6214, #13565 ) ;
#28049 = CARTESIAN_POINT ( 'NONE',  ( 23.83903219839593390, -17.68689162105726709, -71.87567630288067733 ) ) ;
#28050 = CARTESIAN_POINT ( 'NONE',  ( 56.48064340649460746, 14.96064364930199986, -26.24823062834149923 ) ) ;
#28051 = CARTESIAN_POINT ( 'NONE',  ( 16.70908614872999820, -23.04423698702060008, -74.70805987170351159 ) ) ;
#28052 = B_SPLINE_CURVE_WITH_KNOTS ( 'NONE', 3,
 ( #20058, #24488, #20568, #36049, #12213, #28174, #24752, #40762, #44177, #16928, #48904, #33916, #49933, #22385, #17437, #21867 ),
 .UNSPECIFIED., .F., .F.,
 ( 4, 2, 2, 2, 2, 2, 2, 4 ),
 ( -4.238728275518850452, -3.233993249338640297, -2.649205172199279978, -2.119364137759419897, -1.854443620539500071, -1.430570792987610140, -0.7523742689045951337, 0.000000000000000000 ),
 .UNSPECIFIED. ) ;
#28053 = CARTESIAN_POINT ( 'NONE',  ( 50.58622399142209503, 17.63286775605750023, -76.21981748726690853 ) ) ;
#28054 = CARTESIAN_POINT ( 'NONE',  ( 52.76678674812239933, 18.46451123677829997, -48.54390573034589806 ) ) ;
#28055 = CARTESIAN_POINT ( 'NONE',  ( 71.09849264842429761, 1.384887413063060180, -70.31636399389039127 ) ) ;
#28056 = CARTESIAN_POINT ( 'NONE',  ( 16.13393739769620083, -15.61618894467929941, -18.08174999999999955 ) ) ;
#28057 = AXIS2_PLACEMENT_3D ( 'NONE', #20171, #4711, #35905 ) ;
#28058 = EDGE_LOOP ( 'NONE', ( #1439, #14488, #21972, #49394, #1419 ) ) ;
#28059 = DIRECTION ( 'NONE',  ( 1.000000000000000000, 0.000000000000000000, 0.000000000000000000 ) ) ;
#28060 = CARTESIAN_POINT ( 'NONE',  ( 47.61809482659410264, -54.54244161261100032, -55.01024658974859705 ) ) ;
#28061 = CARTESIAN_POINT ( 'NONE',  ( 11.89321781986642002, -65.43603095096219135, -18.08603052201254968 ) ) ;
#28062 = CARTESIAN_POINT ( 'NONE',  ( 61.50409964634459925, -45.37406455498979341, -47.35437808299670337 ) ) ;
#28063 = CARTESIAN_POINT ( 'NONE',  ( 61.49111717500029783, -30.75662150461740296, -16.40374446335560066 ) ) ;
#28064 = CARTESIAN_POINT ( 'NONE',  ( 71.57861930639089110, 0.9369374701296400154, -60.73727483855509490 ) ) ;
#28065 = CARTESIAN_POINT ( 'NONE',  ( 2.558062577110330249, -25.18749138766609974, -34.64999999999999858 ) ) ;
#28066 = CARTESIAN_POINT ( 'NONE',  ( 72.35687375404550892, 1.441354674475110009, -61.69957420032910278 ) ) ;
#28067 = LINE ( 'NONE', #20208, #2517 ) ;
#28068 = CARTESIAN_POINT ( 'NONE',  ( 65.02843368015321346, 1.270877794983130027, -70.57718306158270138 ) ) ;
#28069 = B_SPLINE_CURVE_WITH_KNOTS ( 'NONE', 3,
 ( #11048, #10790, #35135, #18639, #23072, #15235 ),
 .UNSPECIFIED., .F., .F.,
 ( 4, 1, 1, 4 ),
 ( 0.000000000000000000, 0.3333333141630762109, 0.6666666280596336147, 1.000000000000000000 ),
 .UNSPECIFIED. ) ;
#28070 = EDGE_LOOP ( 'NONE', ( #29871, #6449, #18416, #43600, #22805, #24328, #9334, #35295, #45614, #49649, #2600, #11270, #34980 ) ) ;
#28071 = ORIENTED_EDGE ( 'NONE', *, *, #42131, .F. ) ;
#28072 = CARTESIAN_POINT ( 'NONE',  ( 72.33393739769906006, 10.88381105532050164, -61.44999999999760831 ) ) ;
#28073 = LINE ( 'NONE', #43825, #26893 ) ;
#28074 = ORIENTED_EDGE ( 'NONE', *, *, #47573, .F. ) ;
#28075 = CARTESIAN_POINT ( 'NONE',  ( 57.00424200505899819, -45.17895554415359527, -25.30170080014089962 ) ) ;
#28076 = CARTESIAN_POINT ( 'NONE',  ( 87.61621807841599718, -33.11618894467940066, -61.12885639714370001 ) ) ;
#28077 = EDGE_LOOP ( 'NONE', ( #40465, #10020 ) ) ;
#28078 = CARTESIAN_POINT ( 'NONE',  ( 51.67587649748470113, 2.735120682347050192, -77.01363636363508647 ) ) ;
#28080 = CARTESIAN_POINT ( 'NONE',  ( 17.94297559678599185, 1.205480371600828438, -34.75586992539665943 ) ) ;
#28079 = AXIS2_PLACEMENT_3D ( 'NONE', #6496, #26383, #9902 ) ;
#28081 = CARTESIAN_POINT ( 'NONE',  ( 24.04462728581425068, -15.69187742550130693, -65.51071106015494649 ) ) ;
#28082 = ADVANCED_FACE ( 'NONE', ( #30881 ), #49409, .T. ) ;
#28083 = CARTESIAN_POINT ( 'NONE',  ( 24.30253626735589734, -14.49515702607499890, -45.74891888349849722 ) ) ;
#28084 = AXIS2_PLACEMENT_3D ( 'NONE', #43796, #8662, #21475 ) ;
#28085 = CARTESIAN_POINT ( 'NONE',  ( 45.20441673098799384, 2.222700185736389944, -34.80570975016329527 ) ) ;
#28086 = CARTESIAN_POINT ( 'NONE',  ( 9.700071671388441175, -20.26994223601302636, -50.59290778570318992 ) ) ;
#28087 = ORIENTED_EDGE ( 'NONE', *, *, #47600, .T. ) ;
#28088 = SHAPE_REPRESENTATION ( 'Foot Base', ( #20940 ), #50248 ) ;
#28089 = LINE ( 'NONE', #40674, #29204 ) ;
#28090 = CARTESIAN_POINT ( 'NONE',  ( 19.90766354386979842, -22.04007435515010016, -32.56358854585799634 ) ) ;
#28091 = CARTESIAN_POINT ( 'NONE',  ( 41.00662729433690146, 13.77143252834769882, -5.555595257260869779 ) ) ;
#28092 = CIRCLE ( 'NONE', #3836, 2.000000000000000000 ) ;
#28093 = CARTESIAN_POINT ( 'NONE',  ( 14.75122413114260134, 21.64019965034979975, -76.12465403027070465 ) ) ;
#28094 = CARTESIAN_POINT ( 'NONE',  ( 11.02646362629858245, -21.74036658064323646, -60.51332976940924624 ) ) ;
#28095 = CARTESIAN_POINT ( 'NONE',  ( 84.44784216359251161, -43.11618894467930119, -47.47585302082339354 ) ) ;
#28096 = DIRECTION ( 'NONE',  ( 0.000000000000000000, 0.000000000000000000, 1.000000000000000000 ) ) ;
#28097 = CARTESIAN_POINT ( 'NONE',  ( 19.50889905593779972, -8.093399932991250267, -45.14190469443359888 ) ) ;
#28098 = ORIENTED_EDGE ( 'NONE', *, *, #23885, .T. ) ;
#28099 = CARTESIAN_POINT ( 'NONE',  ( 54.98660006789570076, -47.35355536850440217, -26.27416394216670170 ) ) ;
#28100 = CARTESIAN_POINT ( 'NONE',  ( 15.80830505657519680, -50.93044242254529763, -20.14990715359089890 ) ) ;
#28101 = CARTESIAN_POINT ( 'NONE',  ( 50.89766658690811596, -35.40215446828276669, -76.34789914821418222 ) ) ;
#28102 = CARTESIAN_POINT ( 'NONE',  ( 24.04516176800591865, -15.61618872104648226, -63.79232972929064971 ) ) ;
#28103 = CARTESIAN_POINT ( 'NONE',  ( 22.84664618675378378, -16.49985765395500437, -56.49448217489652535 ) ) ;
#28104 = CARTESIAN_POINT ( 'NONE',  ( 12.69633964705789886, -49.98156587680259832, -21.09933892968020075 ) ) ;
#28105 = ORIENTED_EDGE ( 'NONE', *, *, #17837, .T. ) ;
#28106 = DIRECTION ( 'NONE',  ( 0.5897727341282554825, -0.3900873262218120252, 0.7071067811865473507 ) ) ;
#28107 = CARTESIAN_POINT ( 'NONE',  ( 47.23649938924289415, 23.53374381085950162, -54.66384524898040098 ) ) ;
#28108 = VECTOR ( 'NONE', #24928, 1000.000000000000000 ) ;
#28109 = EDGE_CURVE ( 'NONE', #42834, #10465, #2810, .T. ) ;
#28110 = DIRECTION ( 'NONE',  ( -1.000000000000000000, 0.000000000000000000, 0.000000000000000000 ) ) ;
#28111 = CARTESIAN_POINT ( 'NONE',  ( 63.11986671346460298, 0.9948723650351710690, -62.36838199720629916 ) ) ;
#28112 = CARTESIAN_POINT ( 'NONE',  ( 57.36541752560179930, -50.23213309141979721, -52.73855437091509657 ) ) ;
#28113 = CARTESIAN_POINT ( 'NONE',  ( 43.19833518328499622, 12.57157279091759960, -5.006617643082219793 ) ) ;
#28114 = CARTESIAN_POINT ( 'NONE',  ( 68.13393739769630031, 16.88381105532302939, -68.79999999999976978 ) ) ;
#28115 = CARTESIAN_POINT ( 'NONE',  ( 70.17820777451849779, -45.11618894467940066, -13.95197280571250076 ) ) ;
#28116 = DIRECTION ( 'NONE',  ( -1.000000000000000000, 0.000000000000000000, 0.000000000000000000 ) ) ;
#28117 = CARTESIAN_POINT ( 'NONE',  ( 23.98146751630273243, -14.58312774351319341, -75.75066832808212780 ) ) ;
#28118 = EDGE_CURVE ( 'NONE', #19396, #49606, #11191, .T. ) ;
#28119 = CARTESIAN_POINT ( 'NONE',  ( 31.58225770014180256, -2.032350560841368114, -29.09832030244561807 ) ) ;
#28120 = CARTESIAN_POINT ( 'NONE',  ( 20.39068152308574966, -41.98180839364705008, -34.64999999999999147 ) ) ;
#28121 = EDGE_CURVE ( 'NONE', #4148, #20658, #6177, .T. ) ;
#28122 = CARTESIAN_POINT ( 'NONE',  ( 10.22099957837624018, -19.02413528178931656, -61.28616401637014377 ) ) ;
#28123 = CARTESIAN_POINT ( 'NONE',  ( 9.109677719005789598, -16.24994667744640253, -81.42417512157139470 ) ) ;
#28124 = DIRECTION ( 'NONE',  ( -1.000000000000000000, 0.000000000000000000, 0.000000000000000000 ) ) ;
#28125 = VERTEX_POINT ( 'NONE', #19298 ) ;
#28126 = CARTESIAN_POINT ( 'NONE',  ( 5.633937397983799222, -15.61618894439989802, -19.08999999986939855 ) ) ;
#28127 = CARTESIAN_POINT ( 'NONE',  ( 16.24075058801180660, -22.45095174809149796, -34.94749056287888322 ) ) ;
#28128 = AXIS2_PLACEMENT_3D ( 'NONE', #2164, #26253, #29918 ) ;
#28129 = CARTESIAN_POINT ( 'NONE',  ( 12.28182699806689904, -8.928754245619188623, -81.23899999999999011 ) ) ;
#28130 = VERTEX_POINT ( 'NONE', #47357 ) ;
#28131 = CARTESIAN_POINT ( 'NONE',  ( 17.81078732947910126, 21.37421319461290281, -76.02269426304029309 ) ) ;
#28132 = VECTOR ( 'NONE', #15536, 1000.000000000000000 ) ;
#28133 = ORIENTED_EDGE ( 'NONE', *, *, #12114, .T. ) ;
#28134 = VERTEX_POINT ( 'NONE', #36561 ) ;
#28135 = CARTESIAN_POINT ( 'NONE',  ( 56.52347729570519874, -46.24434533601050390, -26.27197595876690173 ) ) ;
#28136 = CARTESIAN_POINT ( 'NONE',  ( 20.94776370346930250, -20.69586690337569834, -81.23899999999999011 ) ) ;
#28137 = CARTESIAN_POINT ( 'NONE',  ( 18.47369125467839979, -4.651823196201450017, -35.14999999999999858 ) ) ;
#28138 = CARTESIAN_POINT ( 'NONE',  ( 0.4047412638266219553, -8.844334399411719616, -35.14999999999999858 ) ) ;
#28139 = DIRECTION ( 'NONE',  ( -0.1643989873053569861, -8.962268658296950507E-16, 0.9863939238321438596 ) ) ;
#28140 = EDGE_CURVE ( 'NONE', #2233, #6987, #46191, .T. ) ;
#28141 = FACE_OUTER_BOUND ( 'NONE', #38751, .T. ) ;
#28142 = VERTEX_POINT ( 'NONE', #28956 ) ;
#28143 = CARTESIAN_POINT ( 'NONE',  ( 22.57761993255723709, -12.95386672222832480, -42.72197786470339764 ) ) ;
#28144 = AXIS2_PLACEMENT_3D ( 'NONE', #41529, #17686, #29975 ) ;
#28145 = DIRECTION ( 'NONE',  ( -1.000000000000000000, 6.785502314117012559E-28, 1.822422554782380175E-11 ) ) ;
#28146 = ORIENTED_EDGE ( 'NONE', *, *, #39645, .F. ) ;
#28147 = ORIENTED_EDGE ( 'NONE', *, *, #10118, .T. ) ;
#28148 = CARTESIAN_POINT ( 'NONE',  ( 7.349327706869664745, -24.40079863550579375, -22.14999999999998792 ) ) ;
#28149 = CYLINDRICAL_SURFACE ( 'NONE', #21716, 1.999999999999998224 ) ;
#28150 = CARTESIAN_POINT ( 'NONE',  ( 61.01489880521270237, 14.38000684155560016, -47.65651487079679782 ) ) ;
#28151 = CONICAL_SURFACE ( 'NONE', #44071, 3.118521338338071214, 0.6364736820000767015 ) ;
#28152 = CARTESIAN_POINT ( 'NONE',  ( 30.13393739769619728, 7.383811055320659733, -59.64999999999999147 ) ) ;
#28153 = DIRECTION ( 'NONE',  ( 0.000000000000000000, 0.000000000000000000, -1.000000000000000000 ) ) ;
#28154 = CARTESIAN_POINT ( 'NONE',  ( -6.434752379702439740, 14.95818219322160125, -4.725866882124770463 ) ) ;
#28155 = CARTESIAN_POINT ( 'NONE',  ( 47.14848705314030042, 23.49639263515488707, -74.72737448321004194 ) ) ;
#28156 = AXIS2_PLACEMENT_3D ( 'NONE', #44375, #49356, #40954 ) ;
#28157 = CARTESIAN_POINT ( 'NONE',  ( 58.30601965111470264, 14.38410068486810012, -26.39168729330650010 ) ) ;
#28158 = CARTESIAN_POINT ( 'NONE',  ( 23.17695949768430097, -12.15460146459719937, -63.14209593641499652 ) ) ;
#28159 = EDGE_LOOP ( 'NONE', ( #7541, #1604, #42974, #47015 ) ) ;
#28160 = CIRCLE ( 'NONE', #5606, 3.000000000000001332 ) ;
#28161 = FACE_OUTER_BOUND ( 'NONE', #16737, .T. ) ;
#28162 = CARTESIAN_POINT ( 'NONE',  ( 28.37540540599746919, -8.548574094810419410, -34.70142521051217699 ) ) ;
#28163 = CARTESIAN_POINT ( 'NONE',  ( 12.04090198330849937, 33.96751094239839830, -45.84253678965290391 ) ) ;
#28164 = CARTESIAN_POINT ( 'NONE',  ( 72.29500244193140190, 1.200163167270710041, -69.93714187953969486 ) ) ;
#28165 = CARTESIAN_POINT ( 'NONE',  ( 44.09118259309181553, -39.96203129707259905, -66.21835677545064414 ) ) ;
#28166 = DIRECTION ( 'NONE',  ( -1.000000000000000000, 0.000000000000000000, 0.000000000000000000 ) ) ;
#28167 = CARTESIAN_POINT ( 'NONE',  ( 47.18323849499689970, 23.57489303030209982, -74.17387246174169491 ) ) ;
#28168 = CARTESIAN_POINT ( 'NONE',  ( 48.59292341170780105, -54.12958895873340026, -55.31326040662610666 ) ) ;
#28169 = DIRECTION ( 'NONE',  ( -1.000000000000000000, 0.000000000000000000, 0.000000000000000000 ) ) ;
#28170 = EDGE_CURVE ( 'NONE', #17698, #1081, #4342, .T. ) ;
#28171 = AXIS2_PLACEMENT_3D ( 'NONE', #14968, #41260, #35133 ) ;
#28172 = FACE_OUTER_BOUND ( 'NONE', #26127, .T. ) ;
#28173 = CARTESIAN_POINT ( 'NONE',  ( 8.222524523195870572, -15.61634168869099959, -38.50766849176289952 ) ) ;
#28174 = CARTESIAN_POINT ( 'NONE',  ( 56.78179639309170312, 13.88381105532070059, -15.59568127148800087 ) ) ;
#28175 = ADVANCED_FACE ( 'NONE', ( #32352 ), #930, .T. ) ;
#28176 = ORIENTED_EDGE ( 'NONE', *, *, #12656, .F. ) ;
#28177 = CARTESIAN_POINT ( 'NONE',  ( 15.99849640639799908, -8.167138661756609963, -34.56155571298840101 ) ) ;
#28178 = CARTESIAN_POINT ( 'NONE',  ( 64.64302830678670375, 0.9098571636355720083, -60.77008670988870165 ) ) ;
#28179 = ORIENTED_EDGE ( 'NONE', *, *, #42299, .T. ) ;
#28180 = CARTESIAN_POINT ( 'NONE',  ( 71.40920805366010882, 1.325841671674429900, -70.40030171741129550 ) ) ;
#28181 = CARTESIAN_POINT ( 'NONE',  ( 60.92563286722050009, -45.50374237643139708, -47.41214175719230184 ) ) ;
#28182 = AXIS2_PLACEMENT_3D ( 'NONE', #34101, #34888, #42518 ) ;
#28183 = CARTESIAN_POINT ( 'NONE',  ( 57.24929578234380045, 19.38381105828390361, -53.91492796160409284 ) ) ;
#28184 = FACE_OUTER_BOUND ( 'NONE', #30341, .T. ) ;
#28186 = CARTESIAN_POINT ( 'NONE',  ( 19.33046814882933973, 18.01819160635306716, -34.64999999999999858 ) ) ;
#28185 = CARTESIAN_POINT ( 'NONE',  ( 41.05890600732872286, 8.424924847782378379, -80.87056964938905423 ) ) ;
#28187 = CARTESIAN_POINT ( 'NONE',  ( 71.25019707560589666, 0.8838110553206759423, -70.77727272727270247 ) ) ;
#28188 = CARTESIAN_POINT ( 'NONE',  ( 14.06325681293461116, -23.32128858265275539, -52.09100060540798438 ) ) ;
#28189 = ORIENTED_EDGE ( 'NONE', *, *, #12918, .T. ) ;
#28190 = CARTESIAN_POINT ( 'NONE',  ( 82.75388200178990417, -45.59495393102269389, -47.67228907607359645 ) ) ;
#28191 = ORIENTED_EDGE ( 'NONE', *, *, #554, .F. ) ;
#28192 = ORIENTED_EDGE ( 'NONE', *, *, #42299, .F. ) ;
#28193 = ORIENTED_EDGE ( 'NONE', *, *, #25246, .T. ) ;
#28194 = DIRECTION ( 'NONE',  ( 0.7071067811865475727, -0.7071067811865475727, 0.000000000000000000 ) ) ;
#28195 = CARTESIAN_POINT ( 'NONE',  ( 9.807806602964351583, -10.75446673786055385, -79.00066532657710638 ) ) ;
#28196 = CARTESIAN_POINT ( 'NONE',  ( 76.40923666012143656, -10.47647217757513793, -12.83630549532472820 ) ) ;
#28197 = CARTESIAN_POINT ( 'NONE',  ( 53.59017120079079888, -51.78138378941920195, -53.35603438827740064 ) ) ;
#28198 = AXIS2_PLACEMENT_3D ( 'NONE', #18532, #34506, #50513 ) ;
#28199 = VERTEX_POINT ( 'NONE', #17184 ) ;
#28200 = ORIENTED_EDGE ( 'NONE', *, *, #19116, .F. ) ;
#28201 = EDGE_CURVE ( 'NONE', #23386, #20265, #9059, .T. ) ;
#28202 = CARTESIAN_POINT ( 'NONE',  ( 71.25019707560579718, 0.8838110553206759423, -60.52272727272730179 ) ) ;
#28203 = CARTESIAN_POINT ( 'NONE',  ( 56.92280486547669938, -45.20348458963250238, -25.29907664449969928 ) ) ;
#28204 = CARTESIAN_POINT ( 'NONE',  ( 56.28151583052680706, -50.59316951485450176, -52.90568346777400421 ) ) ;
#28205 = CARTESIAN_POINT ( 'NONE',  ( 8.784728771177240603, -63.11543068614769680, -46.67204636144870022 ) ) ;
#28206 = EDGE_CURVE ( 'NONE', #40830, #33379, #36298, .T. ) ;
#28207 = CARTESIAN_POINT ( 'NONE',  ( 24.04470022272198193, -15.61619473591594698, -59.79232576333501470 ) ) ;
#28208 = FACE_OUTER_BOUND ( 'NONE', #22531, .T. ) ;
#28209 = ORIENTED_EDGE ( 'NONE', *, *, #12829, .F. ) ;
#28210 = FACE_OUTER_BOUND ( 'NONE', #17188, .T. ) ;
#28211 = CARTESIAN_POINT ( 'NONE',  ( 53.19378597440579881, -50.43795885268350787, -77.11066259967179803 ) ) ;
#28212 = CARTESIAN_POINT ( 'NONE',  ( 60.27360767123090568, 14.56433066022204770, -47.49318409392830631 ) ) ;
#28213 = DIRECTION ( 'NONE',  ( -0.4999999999999985012, 0.8660254037844394848, 0.000000000000000000 ) ) ;
#28214 = CARTESIAN_POINT ( 'NONE',  ( 8.388736160725070334, -16.88054862072210227, -58.96098648058310232 ) ) ;
#28215 = CARTESIAN_POINT ( 'NONE',  ( 12.61047097489570135, -50.09335168391980631, -21.13759556400450279 ) ) ;
#28216 = DIRECTION ( 'NONE',  ( -1.000000000000000000, 0.000000000000000000, 0.000000000000000000 ) ) ;
#28217 = CARTESIAN_POINT ( 'NONE',  ( -22.66047177492978548, -11.61221224052196455, -54.65944424064918650 ) ) ;
#28218 = FACE_OUTER_BOUND ( 'NONE', #48015, .T. ) ;
#28219 = CARTESIAN_POINT ( 'NONE',  ( 57.39341912848639993, 13.88381105532070059, -16.95659913784360029 ) ) ;
#28220 = CARTESIAN_POINT ( 'NONE',  ( 14.63393739769640156, 10.88381105532070059, -34.64999999999999858 ) ) ;
#28221 = B_SPLINE_CURVE_WITH_KNOTS ( 'NONE', 3,
 ( #27535, #16008, #51147, #23081 ),
 .UNSPECIFIED., .F., .F.,
 ( 4, 4 ),
 ( 0.000000000000000000, 1.000000000000000000 ),
 .UNSPECIFIED. ) ;
#28222 = DIRECTION ( 'NONE',  ( 0.000000000000000000, 0.000000000000000000, -1.000000000000000000 ) ) ;
#28223 = CARTESIAN_POINT ( 'NONE',  ( 13.10370563145900036, -9.247495623648822161, -56.20581778389630045 ) ) ;
#28224 = DIRECTION ( 'NONE',  ( 1.000000000000000000, 0.000000000000000000, 0.000000000000000000 ) ) ;
#28225 = ORIENTED_EDGE ( 'NONE', *, *, #47034, .T. ) ;
#28226 = CARTESIAN_POINT ( 'NONE',  ( 47.23343139436899918, 22.78429295813339905, -75.61476957854540615 ) ) ;
#28227 = CARTESIAN_POINT ( 'NONE',  ( 47.40958959913769633, -54.64515405761270017, -54.70637844396050298 ) ) ;
#28228 = DIRECTION ( 'NONE',  ( 0.000000000000000000, 0.000000000000000000, -1.000000000000000000 ) ) ;
#28229 = CARTESIAN_POINT ( 'NONE',  ( 9.543056551245093999, -13.84496916688426182, -37.53615381032067688 ) ) ;
#28230 = CARTESIAN_POINT ( 'NONE',  ( 22.55396266313498188, -18.35526875653752299, -76.97599367191068609 ) ) ;
#28231 = CARTESIAN_POINT ( 'NONE',  ( 24.04493539499120658, -15.60966883180437570, -55.50740977386095665 ) ) ;
#28232 = AXIS2_PLACEMENT_3D ( 'NONE', #19831, #11985, #16672 ) ;
#28233 = CARTESIAN_POINT ( 'NONE',  ( 21.78494278233659998, -33.82423023735729828, -74.14999999999999147 ) ) ;
#28234 = DIRECTION ( 'NONE',  ( -1.878694634646244452E-12, -5.875576256101890322E-05, 0.9999999982738801974 ) ) ;
#28236 = CARTESIAN_POINT ( 'NONE',  ( 12.14983891641476177, -22.52873075169600625, -52.45899731366314001 ) ) ;
#28235 = FACE_OUTER_BOUND ( 'NONE', #36915, .T. ) ;
#28237 = EDGE_CURVE ( 'NONE', #9060, #6692, #48637, .T. ) ;
#28238 = CIRCLE ( 'NONE', #47538, 3.000000000000003109 ) ;
#28239 = CARTESIAN_POINT ( 'NONE',  ( -4.193170025096960352, -49.34067901558599800, -7.780630217993570241 ) ) ;
#28240 = CARTESIAN_POINT ( 'NONE',  ( 48.47823774206090519, 22.94606279175510011, -55.31601837894829998 ) ) ;
#28241 = ORIENTED_EDGE ( 'NONE', *, *, #9121, .F. ) ;
#28242 = CARTESIAN_POINT ( 'NONE',  ( 52.86566477306229928, -49.66304969232309929, -48.91558077290370221 ) ) ;
#28243 = VERTEX_POINT ( 'NONE', #48114 ) ;
#28244 = CARTESIAN_POINT ( 'NONE',  ( 53.58923637029294440, -18.19535155712478414, -15.94606409914099210 ) ) ;
#28245 = DIRECTION ( 'NONE',  ( 0.000000000000000000, -1.000000000000000000, 0.000000000000000000 ) ) ;
#28246 = CYLINDRICAL_SURFACE ( 'NONE', #47179, 40.00000000000000000 ) ;
#28248 = CARTESIAN_POINT ( 'NONE',  ( 56.12979400316489631, 14.82013761545010055, -26.01948386542559888 ) ) ;
#28247 = CARTESIAN_POINT ( 'NONE',  ( 83.84636189228659475, 13.10553490620129935, -46.70679156566500012 ) ) ;
#28249 = CARTESIAN_POINT ( 'NONE',  ( 22.96386447642289852, -13.85702584936900017, -66.37257821948358583 ) ) ;
#28250 = CARTESIAN_POINT ( 'NONE',  ( 52.66149042093859123, 18.55528232251300125, -48.73886901161859697 ) ) ;
#28251 = CARTESIAN_POINT ( 'NONE',  ( 56.87874324233769840, -45.12877571808259347, -16.32799602576229958 ) ) ;
#28252 = DIRECTION ( 'NONE',  ( -0.1175431456444872985, -0.8277005620457519308, -0.5487215947100543278 ) ) ;
#28253 = ORIENTED_EDGE ( 'NONE', *, *, #2527, .F. ) ;
#28254 = CARTESIAN_POINT ( 'NONE',  ( 20.60515567366930156, -22.06560405860919971, -41.59454668711060066 ) ) ;
#28255 = ORIENTED_EDGE ( 'NONE', *, *, #7759, .T. ) ;
#28256 = CARTESIAN_POINT ( 'NONE',  ( 12.04669084400330092, -65.33956968768698914, -17.12210552323070090 ) ) ;
#28257 = CARTESIAN_POINT ( 'NONE',  ( 11.70044915406800001, 33.92707456368980701, -46.82636340333009883 ) ) ;
#28258 = LINE ( 'NONE', #13093, #39931 ) ;
#28259 = CARTESIAN_POINT ( 'NONE',  ( 48.22648091640650136, -53.97280751374249519, -53.84476208330389824 ) ) ;
#28260 = CARTESIAN_POINT ( 'NONE',  ( 8.784728771177219286, 31.88305279678909443, -46.67204636144870022 ) ) ;
#28261 = CARTESIAN_POINT ( 'NONE',  ( 20.99566313739885715, -21.94231611088021339, -63.79933632437322188 ) ) ;
#28262 = ORIENTED_EDGE ( 'NONE', *, *, #11733, .T. ) ;
#28263 = DIRECTION ( 'NONE',  ( 4.718060457820110146E-11, -8.281540456132319756E-12, 1.000000000000000000 ) ) ;
#28264 = CARTESIAN_POINT ( 'NONE',  ( 11.13393739769619906, -63.34493739649700927, -43.91716459650320559 ) ) ;
#28265 = DIRECTION ( 'NONE',  ( -0.8660254037844387076, -0.4999999999999998890, 1.110223024625155678E-16 ) ) ;
#28266 = ORIENTED_EDGE ( 'NONE', *, *, #7799, .T. ) ;
#28267 = ADVANCED_FACE ( 'NONE', ( #37095 ), #19789, .T. ) ;
#28268 = CARTESIAN_POINT ( 'NONE',  ( 71.42967573711919727, 1.404650034021559968, -70.20402782815220633 ) ) ;
#28269 = CARTESIAN_POINT ( 'NONE',  ( 51.02818947082050016, -50.88302571328060253, -76.14999999999999147 ) ) ;
#28270 = B_SPLINE_CURVE_WITH_KNOTS ( 'NONE', 3,
 ( #29208, #21596, #42323, #33134, #49159, #34168, #5896, #45216, #21341, #30245, #9324, #25784, #42059, #17688, #10089, #38128, #37348, #25271 ),
 .UNSPECIFIED., .F., .F.,
 ( 4, 2, 2, 2, 2, 2, 2, 2, 4 ),
 ( 0.4999984312796272867, 0.5624986273696739314, 0.6249988234597205761, 0.6874990195497672207, 0.7499992156398138654, 0.8124994117298603991, 0.8749996078199069327, 0.9374998039099534664, 1.000000000000000000 ),
 .UNSPECIFIED. ) ;
#28271 = DIRECTION ( 'NONE',  ( -1.000000000000000000, 0.000000000000000000, 0.000000000000000000 ) ) ;
#28272 = ORIENTED_EDGE ( 'NONE', *, *, #28237, .T. ) ;
#28273 = CARTESIAN_POINT ( 'NONE',  ( 20.99559717909331624, -21.94236875847741075, -62.08399597771296641 ) ) ;
#28274 = CARTESIAN_POINT ( 'NONE',  ( 21.38393739769620083, -15.61618894467929941, -18.58999999999999986 ) ) ;
#28275 = DIRECTION ( 'NONE',  ( 1.000000000000000000, 0.000000000000000000, 0.000000000000000000 ) ) ;
#28276 = DIRECTION ( 'NONE',  ( -0.8545454545454587159, 0.000000000000000000, -0.5193766129849277657 ) ) ;
#28277 = CARTESIAN_POINT ( 'NONE',  ( 21.83276634445940090, -9.657492049260909539, -75.53523696341960658 ) ) ;
#28278 = CARTESIAN_POINT ( 'NONE',  ( 11.92983776680180341, -9.953318164944898072, -38.14390150139128366 ) ) ;
#28279 = EDGE_CURVE ( 'NONE', #35815, #38000, #33059, .T. ) ;
#28280 = DIRECTION ( 'NONE',  ( 0.000000000000000000, 0.000000000000000000, 1.000000000000000000 ) ) ;
#28281 = APPLICATION_PROTOCOL_DEFINITION ( 'draft international standard', 'automotive_design', 1998, #16716 ) ;
#28282 = EDGE_LOOP ( 'NONE', ( #30786, #46588, #43756, #8766 ) ) ;
#28283 = CARTESIAN_POINT ( 'NONE',  ( 23.52193300906940010, -14.65482811154960174, -62.19146876365169874 ) ) ;
#28284 = DIRECTION ( 'NONE',  ( 5.878706999999999976E-17, 3.795112000000000086E-17, 1.000000000000000000 ) ) ;
#28285 = CARTESIAN_POINT ( 'NONE',  ( 12.29223489819977821, 34.10423391560534156, -23.62127221463904547 ) ) ;
#28286 = CARTESIAN_POINT ( 'NONE',  ( 47.13612099939350486, 23.16257524069679974, -75.29255935572381020 ) ) ;
#28287 = DIRECTION ( 'NONE',  ( 0.000000000000000000, 0.000000000000000000, -1.000000000000000000 ) ) ;
#28288 = DIRECTION ( 'NONE',  ( 0.000000000000000000, -1.000000000000000000, 0.000000000000000000 ) ) ;
#28289 = CARTESIAN_POINT ( 'NONE',  ( 62.63393739769619373, 21.88381105532059934, 16.35000000000000142 ) ) ;
#28290 = CARTESIAN_POINT ( 'NONE',  ( 18.15912969681970068, -7.623610082976019164, -75.08666063648169597 ) ) ;
#28291 = CARTESIAN_POINT ( 'NONE',  ( 57.21097685450429537, -50.61618800939579899, -74.14879615022279324 ) ) ;
#28293 = CARTESIAN_POINT ( 'NONE',  ( 30.72739985827759313, -35.67572234546251764, -84.61750747199793921 ) ) ;
#28292 = LINE ( 'NONE', #44819, #45806 ) ;
#28294 = EDGE_CURVE ( 'NONE', #9275, #12303, #28052, .T. ) ;
#28295 = CARTESIAN_POINT ( 'NONE',  ( 63.04573361361109818, 1.102581332775300016, -68.74251431096891451 ) ) ;
#28296 = CARTESIAN_POINT ( 'NONE',  ( 61.38286689828800036, 13.95525073026689888, -46.52105988975220185 ) ) ;
#28297 = CARTESIAN_POINT ( 'NONE',  ( 18.20466777478382880, -7.911103216214283584, -79.09100292823505640 ) ) ;
#28298 = CARTESIAN_POINT ( 'NONE',  ( -0.2991137081908959994, -62.12324524158640315, -48.78634498590130164 ) ) ;
#28299 = ADVANCED_FACE ( 'NONE', ( #25788 ), #26054, .T. ) ;
#28300 = ORIENTED_EDGE ( 'NONE', *, *, #21617, .F. ) ;
#28301 = CARTESIAN_POINT ( 'NONE',  ( 52.85165694913099799, -49.64944609877660042, -48.64955875961400267 ) ) ;
#28302 = EDGE_CURVE ( 'NONE', #2651, #2348, #51591, .T. ) ;
#28303 = AXIS2_PLACEMENT_3D ( 'NONE', #30078, #29815, #18557 ) ;
#28304 = CARTESIAN_POINT ( 'NONE',  ( 61.14783123884740235, -45.23924466744810502, -27.62102214444609771 ) ) ;
#28305 = CARTESIAN_POINT ( 'NONE',  ( 37.33393739769619657, -15.61618894467929941, -11.54999999999999893 ) ) ;
#28306 = CARTESIAN_POINT ( 'NONE',  ( 56.33185943253500483, 14.93937505072510064, -26.19910003242920027 ) ) ;
#28307 = VECTOR ( 'NONE', #14711, 1000.000000000000000 ) ;
#28308 = CARTESIAN_POINT ( 'NONE',  ( 22.17630248670440096, -19.25372891403399933, -32.62531358638169365 ) ) ;
#28309 = EDGE_CURVE ( 'NONE', #41238, #23939, #42824, .T. ) ;
#28310 = CARTESIAN_POINT ( 'NONE',  ( 50.81500901600419695, 18.46718465057229963, -76.22412500802471413 ) ) ;
#28311 = CARTESIAN_POINT ( 'NONE',  ( 52.83030979110780123, 18.43029764974290075, -48.71029753094079950 ) ) ;
#28312 = CARTESIAN_POINT ( 'NONE',  ( 71.03155062328740144, 1.383928098097870096, -70.33743540642140601 ) ) ;
#28313 = DIRECTION ( 'NONE',  ( -0.000000000000000000, 1.000000000000000000, 0.000000000000000000 ) ) ;
#28314 = ORIENTED_EDGE ( 'NONE', *, *, #36077, .T. ) ;
#28315 = LINE ( 'NONE', #4223, #42888 ) ;
#28316 = CARTESIAN_POINT ( 'NONE',  ( 47.66097882627480686, -54.52613192741829096, -55.10530119525199666 ) ) ;
#28317 = CARTESIAN_POINT ( 'NONE',  ( 0.3209249304026170480, -46.25141913721060405, -34.64999999999999858 ) ) ;
#28318 = CARTESIAN_POINT ( 'NONE',  ( 58.92073396209919878, -28.11618894467929763, -18.64999999999999858 ) ) ;
#28319 = CARTESIAN_POINT ( 'NONE',  ( 57.65805802474199737, 18.65029578125960086, -52.34980151920610325 ) ) ;
#28320 = CARTESIAN_POINT ( 'NONE',  ( 71.41841232404479456, 1.186701509386330011, -60.73797667709639825 ) ) ;
#28321 = CYLINDRICAL_SURFACE ( 'NONE', #40894, 0.4999999999999982236 ) ;
#28322 = CARTESIAN_POINT ( 'NONE',  ( 71.64275587478520890, 1.313759828078409964, -60.99019652856610207 ) ) ;
#28323 = EDGE_CURVE ( 'NONE', #25686, #31172, #44035, .T. ) ;
#28324 = CARTESIAN_POINT ( 'NONE',  ( 20.99557608044584001, -21.94238580726353049, -71.79928481050744438 ) ) ;
#28325 = CARTESIAN_POINT ( 'NONE',  ( 64.99525386628140211, 0.8838110553206759423, -70.76364393196210756 ) ) ;
#28326 = ORIENTED_EDGE ( 'NONE', *, *, #38814, .T. ) ;
#28327 = VERTEX_POINT ( 'NONE', #29726 ) ;
#28328 = CARTESIAN_POINT ( 'NONE',  ( 8.222923941706072881, -14.58073999030537848, -54.83399627919607155 ) ) ;
#28329 = CARTESIAN_POINT ( 'NONE',  ( 49.85658880370656476, -29.63768744850618475, -15.88711799670739921 ) ) ;
#28330 = ORIENTED_EDGE ( 'NONE', *, *, #6889, .T. ) ;
#28331 = ADVANCED_FACE ( 'NONE', ( #25534 ), #41281, .T. ) ;
#28332 = CARTESIAN_POINT ( 'NONE',  ( 57.22943158897479776, -45.13409722695310222, -25.31259632064490006 ) ) ;
#28333 = CARTESIAN_POINT ( 'NONE',  ( 9.366918910324010028, -14.88264276746137682, -49.48733500142635222 ) ) ;
#28334 = ORIENTED_EDGE ( 'NONE', *, *, #20561, .T. ) ;
#28335 = DIRECTION ( 'NONE',  ( 0.000000000000000000, 0.000000000000000000, 1.000000000000000000 ) ) ;
#28336 = CARTESIAN_POINT ( 'NONE',  ( 12.69092708031987016, -9.723879944688558652, -71.78431635714069614 ) ) ;
#28337 = CARTESIAN_POINT ( 'NONE',  ( 17.17653815174671550, -23.52626367551765796, -65.96613581823291383 ) ) ;
#28338 = CARTESIAN_POINT ( 'NONE',  ( 24.37832766821379948, -15.50327692879579899, -41.78797233031760072 ) ) ;
#28339 = LINE ( 'NONE', #40412, #21290 ) ;
#28340 = CARTESIAN_POINT ( 'NONE',  ( 41.67047660715986979, -37.56944021528936872, -81.96730251586943439 ) ) ;
#28341 = ORIENTED_EDGE ( 'NONE', *, *, #35012, .F. ) ;
#28342 = CARTESIAN_POINT ( 'NONE',  ( 10.64252135837869950, -63.58685848925379958, -23.65858396068239955 ) ) ;
#28343 = CARTESIAN_POINT ( 'NONE',  ( 9.234060601172799920, -12.80577920849349915, -33.35577785649419980 ) ) ;
#28344 = AXIS2_PLACEMENT_3D ( 'NONE', #28473, #40539, #44472 ) ;
#28345 = ADVANCED_FACE ( 'NONE', ( #6166 ), #16423, .T. ) ;
#28346 = AXIS2_PLACEMENT_3D ( 'NONE', #18892, #37332, #17420 ) ;
#28347 = CARTESIAN_POINT ( 'NONE',  ( 12.14972585590047238, -8.703711119338285229, -32.84099998782102858 ) ) ;
#28348 = CONICAL_SURFACE ( 'NONE', #22516, 1.587553672713209574, 1.249045772398249987 ) ;
#28349 = CIRCLE ( 'NONE', #9150, 0.5000000000000004441 ) ;
#28350 = CARTESIAN_POINT ( 'NONE',  ( 13.87433288923529950, 20.87662390947729918, -75.53341961486960088 ) ) ;
#28351 = DIRECTION ( 'NONE',  ( 0.000000000000000000, 0.000000000000000000, -1.000000000000000000 ) ) ;
#28352 = CARTESIAN_POINT ( 'NONE',  ( 13.63393739769619906, -45.61618894467940066, -34.64999999999999858 ) ) ;
#28353 = CARTESIAN_POINT ( 'NONE',  ( 63.56282646728049457, 1.400446387219270061, -68.89724194849250694 ) ) ;
#28354 = CARTESIAN_POINT ( 'NONE',  ( 22.67586280804129828, -20.63474776514319586, -43.71596393528839286 ) ) ;
#28355 = VERTEX_POINT ( 'NONE', #1970 ) ;
#28356 = CARTESIAN_POINT ( 'NONE',  ( 56.05191282448750201, -45.91615162336719891, -25.80821051545110123 ) ) ;
#28357 = B_SPLINE_CURVE_WITH_KNOTS ( 'NONE', 3,
 ( #8885, #17012, #45041, #29045, #36639, #9140, #44518, #28781, #40584, #4682, #24837 ),
 .UNSPECIFIED., .F., .F.,
 ( 4, 1, 1, 1, 1, 1, 1, 1, 4 ),
 ( 0.000000000000000000, 0.1249968820770194777, 0.2499966053408283206, 0.3749963286046372191, 0.4999960518684460342, 0.6249957751322549049, 0.7499954983960637200, 0.8749952216598726462, 1.000000000000000000 ),
 .UNSPECIFIED. ) ;
#28358 = CARTESIAN_POINT ( 'NONE',  ( 15.80832228677149942, -50.93044681828930464, -20.21644471496500017 ) ) ;
#28359 = CARTESIAN_POINT ( 'NONE',  ( 57.32828653034189870, 19.18168419026400073, -53.00038473087150237 ) ) ;
#28360 = CARTESIAN_POINT ( 'NONE',  ( 75.47577596059235816, 12.24922386242644023, -13.41863335767928334 ) ) ;
#28361 = CARTESIAN_POINT ( 'NONE',  ( 13.73527022026340028, -50.20735447812900532, -20.93080062776369843 ) ) ;
#28362 = EDGE_LOOP ( 'NONE', ( #23268, #25021, #9743, #21489, #29296 ) ) ;
#28363 = CARTESIAN_POINT ( 'NONE',  ( 16.13393739769620083, -15.61618894467929941, -22.14999999999999858 ) ) ;
#28364 = EDGE_CURVE ( 'NONE', #31550, #14613, #15496, .T. ) ;
#28365 = CARTESIAN_POINT ( 'NONE',  ( 47.32528955519509850, 23.46751979651900299, -54.64535935344500217 ) ) ;
#28366 = CARTESIAN_POINT ( 'NONE',  ( 17.00276768726040899, 18.38376088500272587, -83.22678919096382799 ) ) ;
#28367 = CARTESIAN_POINT ( 'NONE',  ( 63.04027743911709791, 0.9947083095259759977, -62.49453424214399888 ) ) ;
#28368 = CARTESIAN_POINT ( 'NONE',  ( -0.007164427059776000244, -22.82436266295209748, -34.77269723891829756 ) ) ;
#28369 = CARTESIAN_POINT ( 'NONE',  ( 41.23309865046339695, 13.48886119783190018, -5.265645747893129780 ) ) ;
#28370 = EDGE_CURVE ( 'NONE', #46428, #21893, #26319, .T. ) ;
#28371 = FACE_OUTER_BOUND ( 'NONE', #48910, .T. ) ;
#28372 = CARTESIAN_POINT ( 'NONE',  ( 11.27229802542173331, -9.289994498170599968, -61.08399727017809511 ) ) ;
#28373 = CARTESIAN_POINT ( 'NONE',  ( 71.98371235365300436, 1.451792515613489876, -61.38183652702590365 ) ) ;
#28374 = CARTESIAN_POINT ( 'NONE',  ( 58.40467996479630131, -46.88273201699870185, -48.03872346596099874 ) ) ;
#28375 = CARTESIAN_POINT ( 'NONE',  ( 24.04493739777547390, -15.61328088927116475, -75.79220904166886896 ) ) ;
#28376 = CARTESIAN_POINT ( 'NONE',  ( 64.64302830678678902, 0.9098571636355680115, -60.77008670988870165 ) ) ;
#28377 = CARTESIAN_POINT ( 'NONE',  ( 56.46551568209640237, 19.54378693895939989, -53.85224189773119718 ) ) ;
#28378 = DIRECTION ( 'NONE',  ( 0.000000000000000000, -1.000000000000000000, 0.000000000000000000 ) ) ;
#28379 = VECTOR ( 'NONE', #47203, 1000.000000000000227 ) ;
#28380 = DIRECTION ( 'NONE',  ( 0.000000000000000000, 0.000000000000000000, -1.000000000000000000 ) ) ;
#28381 = EDGE_LOOP ( 'NONE', ( #42048, #748, #3551, #26579 ) ) ;
#28382 = DIRECTION ( 'NONE',  ( 1.000000000000000000, 0.000000000000000000, 0.000000000000000000 ) ) ;
#28383 = CARTESIAN_POINT ( 'NONE',  ( 9.281825854502979922, 31.93825977863309973, -46.53126684085379594 ) ) ;
#28384 = CARTESIAN_POINT ( 'NONE',  ( 22.21599079217217465, -18.67024064526685123, -34.60078485984914920 ) ) ;
#28385 = VECTOR ( 'NONE', #48059, 1000.000000000000000 ) ;
#28386 = CARTESIAN_POINT ( 'NONE',  ( 9.068231266001319568, -13.91742136908450078, -81.23899999999999011 ) ) ;
#28387 = ORIENTED_EDGE ( 'NONE', *, *, #51512, .F. ) ;
#28388 = CARTESIAN_POINT ( 'NONE',  ( 17.78605519637239851, 20.27135023148479576, -75.33782839756391070 ) ) ;
#28389 = VERTEX_POINT ( 'NONE', #38132 ) ;
#28390 = EDGE_LOOP ( 'NONE', ( #14887, #28718, #14111, #9903 ) ) ;
#28391 = AXIS2_PLACEMENT_3D ( 'NONE', #35754, #19507, #116 ) ;
#28392 = ORIENTED_EDGE ( 'NONE', *, *, #12854, .T. ) ;
#28393 = EDGE_CURVE ( 'NONE', #10857, #4677, #26479, .T. ) ;
#28394 = CYLINDRICAL_SURFACE ( 'NONE', #5955, 6.099999999999994316 ) ;
#28395 = CARTESIAN_POINT ( 'NONE',  ( 19.45428832600709868, -21.61900137026959712, -81.23899999999999011 ) ) ;
#28396 =( BOUNDED_CURVE ( )  B_SPLINE_CURVE ( 3, ( #27331, #36939, #7429, #11111 ),
 .UNSPECIFIED., .F., .T. ) 
 B_SPLINE_CURVE_WITH_KNOTS ( ( 4, 4 ),
 ( 2.795354856560299694, 3.141592653589793116 ),
 .UNSPECIFIED. ) 
 CURVE ( )  GEOMETRIC_REPRESENTATION_ITEM ( )  RATIONAL_B_SPLINE_CURVE ( ( 1.000000000000000000, 0.9900348743600091428, 0.9900348743600091428, 1.000000000000000000 ) ) 
 REPRESENTATION_ITEM ( '' )  );
#28397 = CARTESIAN_POINT ( 'NONE',  ( 61.75019864826120397, 13.88381105542450022, -46.37201226983719948 ) ) ;
#28398 = ORIENTED_EDGE ( 'NONE', *, *, #25109, .F. ) ;
#28399 = CARTESIAN_POINT ( 'NONE',  ( 68.13393739769620083, -42.11618894467930119, -71.15000000000000568 ) ) ;
#28400 = DIRECTION ( 'NONE',  ( 0.000000000000000000, 0.000000000000000000, 1.000000000000000000 ) ) ;
#28401 = ORIENTED_EDGE ( 'NONE', *, *, #7933, .T. ) ;
#28402 = DIRECTION ( 'NONE',  ( -0.000000000000000000, 1.000000000000000000, 0.000000000000000000 ) ) ;
#28403 = CARTESIAN_POINT ( 'NONE',  ( 14.13393739769619906, -37.52509124488599923, -54.64999999999999858 ) ) ;
#28404 = EDGE_LOOP ( 'NONE', ( #410, #25929, #27643, #7259, #11457 ) ) ;
#28405 = VERTEX_POINT ( 'NONE', #37351 ) ;
#28406 = CARTESIAN_POINT ( 'NONE',  ( 0.3188076311095650595, -10.53374720320550040, -34.65000336222090027 ) ) ;
#28407 = CARTESIAN_POINT ( 'NONE',  ( 51.13393739769620083, 19.38381105532069881, 17.35000000000000142 ) ) ;
#28408 = CARTESIAN_POINT ( 'NONE',  ( 60.72740590574490227, 14.39261883701170142, -47.54234311855110207 ) ) ;
#28409 = ADVANCED_FACE ( 'NONE', ( #6427 ), #5654, .F. ) ;
#28410 = EDGE_CURVE ( 'NONE', #5215, #46792, #2489, .T. ) ;
#28411 = CARTESIAN_POINT ( 'NONE',  ( 54.17079961804279975, 14.38146746993139935, -15.02185247389039979 ) ) ;
#28412 = DIRECTION ( 'NONE',  ( -1.000000000000000000, 0.000000000000000000, 0.000000000000000000 ) ) ;
#28413 = CARTESIAN_POINT ( 'NONE',  ( -9.468778084194710232, 12.47338336425449867, -5.557361635588190296 ) ) ;
#28414 = AXIS2_PLACEMENT_3D ( 'NONE', #49254, #8376, #45049 ) ;
#28415 = CIRCLE ( 'NONE', #35981, 5.500000000000000000 ) ;
#28416 = CIRCLE ( 'NONE', #17555, 6.999999999999999112 ) ;
#28417 = CARTESIAN_POINT ( 'NONE',  ( 10.37125623313378497, 23.96744338674034935, -21.14999999999999858 ) ) ;
#28418 = CARTESIAN_POINT ( 'NONE',  ( 59.47927764971650078, 14.15550012739879904, -26.60797151098220326 ) ) ;
#28419 = CIRCLE ( 'NONE', #5855, 1.999999999999997558 ) ;
#28420 = CARTESIAN_POINT ( 'NONE',  ( 9.710243317568311383, -20.12428195038719991, -64.09272310917839377 ) ) ;
#28421 = VERTEX_POINT ( 'NONE', #14024 ) ;
#28422 = CARTESIAN_POINT ( 'NONE',  ( 55.13210266565960893, 17.31833316781790089, -48.68958776747170702 ) ) ;
#28424 = VECTOR ( 'NONE', #6832, 1000.000000000000000 ) ;
#28423 = CARTESIAN_POINT ( 'NONE',  ( 41.56838531616119781, 14.44787509676280024, -6.472129036803299762 ) ) ;
#28425 = CARTESIAN_POINT ( 'NONE',  ( 54.08397353797261786, -50.62656311257075714, -76.77908082735504536 ) ) ;
#28426 = CARTESIAN_POINT ( 'NONE',  ( 72.66187716250549045, 1.030858001319959971, -69.58776317408900525 ) ) ;
#28427 = CARTESIAN_POINT ( 'NONE',  ( 42.58520944582495815, -39.82551429970306600, -73.50479774005893319 ) ) ;
#28428 = ADVANCED_FACE ( 'NONE', ( #2231 ), #41537, .T. ) ;
#28429 = DIRECTION ( 'NONE',  ( 0.000000000000000000, 0.000000000000000000, -1.000000000000000000 ) ) ;
#28430 = EDGE_CURVE ( 'NONE', #25775, #17902, #18046, .T. ) ;
#28431 = CARTESIAN_POINT ( 'NONE',  ( 46.46557555578730359, 21.92956842995989675, -76.13729948603509001 ) ) ;
#28432 = CARTESIAN_POINT ( 'NONE',  ( 49.09311242517659934, -53.78968938430409708, -54.56531883649019932 ) ) ;
#28433 = CARTESIAN_POINT ( 'NONE',  ( 71.33393739769628894, 1.883811055320669947, -61.44999999999999574 ) ) ;
#28434 = CARTESIAN_POINT ( 'NONE',  ( 14.92658367925920615, -23.46628484408796922, -34.05631316871021141 ) ) ;
#28435 = CARTESIAN_POINT ( 'NONE',  ( 18.11900864776900022, 1.362847559348050019, -35.02873218748179340 ) ) ;
#28436 = CARTESIAN_POINT ( 'NONE',  ( 17.98749078828947745, -32.58675169315650066, -34.79644660940672907 ) ) ;
#28437 = ORIENTED_EDGE ( 'NONE', *, *, #46645, .T. ) ;
#28438 = CARTESIAN_POINT ( 'NONE',  ( 10.37278528681540024, -10.89222655134519968, -46.28595751040398909 ) ) ;
#28439 = CARTESIAN_POINT ( 'NONE',  ( 64.59570122278479687, 0.9170823515331248954, -60.80394275157770068 ) ) ;
#28440 = ORIENTED_EDGE ( 'NONE', *, *, #51526, .F. ) ;
#28441 = DIRECTION ( 'NONE',  ( 0.000000000000000000, 0.7071067811865463515, -0.7071067811865487940 ) ) ;
#28442 = CARTESIAN_POINT ( 'NONE',  ( 60.72928671769479791, -45.53983519128849622, -47.27644420220809707 ) ) ;
#28443 = CARTESIAN_POINT ( 'NONE',  ( 23.53017837589144889, 17.70577807492161071, -34.78557451168261849 ) ) ;
#28444 = LINE ( 'NONE', #5399, #19381 ) ;
#28446 = CARTESIAN_POINT ( 'NONE',  ( 19.26373325286755644, 18.14234304701946243, -34.70142521051218409 ) ) ;
#28445 = CARTESIAN_POINT ( 'NONE',  ( 42.31769135335058252, 8.566187770374650512, -74.79605566854385756 ) ) ;
#28447 = DIRECTION ( 'NONE',  ( -1.000000000000000000, 0.000000000000000000, 0.000000000000000000 ) ) ;
#28448 = DIRECTION ( 'NONE',  ( 0.000000000000000000, -1.000000000000000000, 0.000000000000000000 ) ) ;
#28449 = ORIENTED_EDGE ( 'NONE', *, *, #5914, .F. ) ;
#28450 = CARTESIAN_POINT ( 'NONE',  ( 84.09627682649329472, -44.51519333368669606, -47.44643906338429673 ) ) ;
#28451 = ORIENTED_EDGE ( 'NONE', *, *, #29453, .T. ) ;
#28452 = EDGE_LOOP ( 'NONE', ( #30029, #20126, #9850, #49498 ) ) ;
#28453 = EDGE_LOOP ( 'NONE', ( #15857, #6441, #6323, #37283 ) ) ;
#28454 = FACE_BOUND ( 'NONE', #31421, .T. ) ;
#28455 = CIRCLE ( 'NONE', #39334, 6.000000000000005329 ) ;
#28456 = CARTESIAN_POINT ( 'NONE',  ( 52.26504646883520167, -49.78354544620959388, -77.19463087837650050 ) ) ;
#28457 = VECTOR ( 'NONE', #42709, 1000.000000000000000 ) ;
#28458 = CARTESIAN_POINT ( 'NONE',  ( 76.40827150342700236, -20.78360806407327743, -12.83216708051279653 ) ) ;
#28459 = CARTESIAN_POINT ( 'NONE',  ( 50.25479149875150142, -53.19950294433710525, -54.04777103931960625 ) ) ;
#28460 = VECTOR ( 'NONE', #31225, 1000.000000000000000 ) ;
#28461 = ORIENTED_EDGE ( 'NONE', *, *, #22695, .F. ) ;
#28462 = EDGE_LOOP ( 'NONE', ( #23529, #46351, #32766, #10784, #3854, #17816, #14145 ) ) ;
#28463 = CIRCLE ( 'NONE', #48537, 15.56227766016840164 ) ;
#28464 = AXIS2_PLACEMENT_3D ( 'NONE', #48214, #32444, #12314 ) ;
#28465 = CARTESIAN_POINT ( 'NONE',  ( 48.03928511041160476, 23.04428228824039948, -54.71294081448219515 ) ) ;
#28466 = CARTESIAN_POINT ( 'NONE',  ( -15.36168286337127853, 7.384389844490065080, -48.43517473143955243 ) ) ;
#28467 = CARTESIAN_POINT ( 'NONE',  ( 14.32270318449056035, 18.38377289504289180, -83.16479114466771705 ) ) ;
#28468 = DIRECTION ( 'NONE',  ( -0.000000000000000000, -0.000000000000000000, -1.000000000000000000 ) ) ;
#28469 = DIRECTION ( 'NONE',  ( 0.000000000000000000, -0.7071067811865466846, -0.7071067811865483499 ) ) ;
#28470 = DIRECTION ( 'NONE',  ( -1.000000000000000000, 0.000000000000000000, 0.000000000000000000 ) ) ;
#28471 = B_SPLINE_CURVE_WITH_KNOTS ( 'NONE', 3,
 ( #29519, #14576, #25826, #30541, #37648, #10135, #26350, #1497, #26612, #42362 ),
 .UNSPECIFIED., .F., .F.,
 ( 4, 2, 2, 2, 4 ),
 ( 0.000000000000000000, 0.1746266369381154759, 0.6794498943083844278, 0.9949644301648022937, 1.000000000000000000 ),
 .UNSPECIFIED. ) ;
#28472 = ORIENTED_EDGE ( 'NONE', *, *, #19390, .T. ) ;
#28473 = CARTESIAN_POINT ( 'NONE',  ( 16.13393739769620083, -15.61618894467929941, -8.849999999999999645 ) ) ;
#28474 = CARTESIAN_POINT ( 'NONE',  ( 52.26113438680789613, -49.98075224355449819, -76.96437239583239887 ) ) ;
#28475 = CARTESIAN_POINT ( 'NONE',  ( 13.29067414848886308, -9.445305870462737730, -33.81532646017170407 ) ) ;
#28476 = CARTESIAN_POINT ( 'NONE',  ( 12.42856185862050111, -8.698317906129821253, -51.35596909847569691 ) ) ;
#28477 = EDGE_CURVE ( 'NONE', #26529, #33379, #40806, .T. ) ;
#28478 = DIRECTION ( 'NONE',  ( 1.000000000000000000, 0.000000000000000000, 0.000000000000000000 ) ) ;
#28479 = CARTESIAN_POINT ( 'NONE',  ( 3.633937397696199056, -15.61618894467929763, -1.149999999999999911 ) ) ;
#28480 = CARTESIAN_POINT ( 'NONE',  ( 42.16594882433619773, -43.97269357279350288, -4.735301442609650024 ) ) ;
#28481 = CARTESIAN_POINT ( 'NONE',  ( 18.40646359431065449, -51.24009245543214774, -15.69870911006933767 ) ) ;
#28482 = EDGE_CURVE ( 'NONE', #48450, #18259, #21424, .T. ) ;
#28483 = AXIS2_PLACEMENT_3D ( 'NONE', #17484, #34212, #41844 ) ;
#28484 = CARTESIAN_POINT ( 'NONE',  ( 66.72561048563099462, 1.883811055320649963, -20.64999999980150136 ) ) ;
#28485 = CARTESIAN_POINT ( 'NONE',  ( 21.54529553476142922, -19.77480928362585999, -38.66115602709810872 ) ) ;
#28486 = CARTESIAN_POINT ( 'NONE',  ( 18.14390284338869819, -22.37655861516129718, -55.25519061113289609 ) ) ;
#28487 = CARTESIAN_POINT ( 'NONE',  ( 47.60722588394180121, -55.47029091092869635, 10.84999999999999964 ) ) ;
#28488 = ORIENTED_EDGE ( 'NONE', *, *, #44655, .T. ) ;
#28489 = CARTESIAN_POINT ( 'NONE',  ( 14.47398509914520126, -51.62356816798740056, -75.48775473117470369 ) ) ;
#28490 = CARTESIAN_POINT ( 'NONE',  ( 47.37754115064079485, -54.66825602412330198, -54.73097957181000339 ) ) ;
#28491 = CARTESIAN_POINT ( 'NONE',  ( 16.13393739769620083, -15.61618894467929941, -16.88999999999999702 ) ) ;
#28492 = CIRCLE ( 'NONE', #22621, 15.24604989415149703 ) ;
#28493 = CARTESIAN_POINT ( 'NONE',  ( 10.97012820822068058, 33.88053142170652166, -47.22757037140836189 ) ) ;
#28494 = FACE_BOUND ( 'NONE', #29430, .T. ) ;
#28495 = CARTESIAN_POINT ( 'NONE',  ( 60.98630419630155330, -45.44769370713505907, -47.30728599211079910 ) ) ;
#28497 = VECTOR ( 'NONE', #49769, 1000.000000000000000 ) ;
#28496 = CARTESIAN_POINT ( 'NONE',  ( 55.58073395081326851, -45.98461186095343578, -16.80393320440050076 ) ) ;
#28498 = ADVANCED_FACE ( 'NONE', ( #50959 ), #41442, .T. ) ;
#28499 = DIRECTION ( 'NONE',  ( 1.000000000000000000, 0.000000000000000000, 0.000000000000000000 ) ) ;
#28501 = CARTESIAN_POINT ( 'NONE',  ( -4.162377065922562736, -48.30017088459130292, -5.617364974929863308 ) ) ;
#28500 = CYLINDRICAL_SURFACE ( 'NONE', #46608, 38.00000000000000711 ) ;
#28502 = CARTESIAN_POINT ( 'NONE',  ( 16.13393761331730047, -15.61618923485050026, -20.64999983909400072 ) ) ;
#28503 = CARTESIAN_POINT ( 'NONE',  ( 48.81893253562370205, 22.77627760781700061, -54.98725303027700306 ) ) ;
#28504 = ORIENTED_EDGE ( 'NONE', *, *, #51637, .T. ) ;
#28505 = CARTESIAN_POINT ( 'NONE',  ( 12.74054237724960004, -9.433355499594508586, -66.18740309791249388 ) ) ;
#28506 = B_SPLINE_CURVE_WITH_KNOTS ( 'NONE', 3,
 ( #42775, #2156, #38844, #35143, #22823, #34624, #2933, #18136, #38317, #23082, #22309, #2405, #50628, #18903, #50887, #6874 ),
 .UNSPECIFIED., .F., .F.,
 ( 4, 2, 2, 2, 2, 2, 2, 4 ),
 ( 0.000000000000000000, 0.1750000000000006828, 0.3750000000000011102, 0.5000000000000003331, 0.5625000000000003331, 0.6625000000000006439, 0.8225000000000002309, 1.000000000000000000 ),
 .UNSPECIFIED. ) ;
#28507 = VERTEX_POINT ( 'NONE', #797 ) ;
#28508 = CARTESIAN_POINT ( 'NONE',  ( 2.488944341170579833, -5.725871553929439806, -34.70985242058479514 ) ) ;
#28509 = CARTESIAN_POINT ( 'NONE',  ( 65.16938214696820353, 1.384887413063060180, -60.98363600610959878 ) ) ;
#28510 = DIRECTION ( 'NONE',  ( -1.000000000000000000, 1.330268894940021809E-33, -1.060511545910580040E-15 ) ) ;
#28512 = CARTESIAN_POINT ( 'NONE',  ( 54.39595473835359485, 16.76334922740620215, -26.49617834758590007 ) ) ;
#28511 = CARTESIAN_POINT ( 'NONE',  ( 83.45566905280598746, 13.44200627990649899, -46.48561260377739757 ) ) ;
#28513 = CARTESIAN_POINT ( 'NONE',  ( 22.53532168237200395, -18.57673584289430124, -68.59070828926491004 ) ) ;
#28514 = CARTESIAN_POINT ( 'NONE',  ( 52.95065142214180298, 18.41081157851500194, -49.05053735721260466 ) ) ;
#28515 = CARTESIAN_POINT ( 'NONE',  ( 56.39822365214870104, -45.27769210685230661, -16.54940569508480053 ) ) ;
#28516 = FACE_OUTER_BOUND ( 'NONE', #1144, .T. ) ;
#28517 = ORIENTED_EDGE ( 'NONE', *, *, #23237, .T. ) ;
#28518 = ORIENTED_EDGE ( 'NONE', *, *, #41560, .F. ) ;
#28519 = CARTESIAN_POINT ( 'NONE',  ( 11.92234616936549862, -65.02420767682468750, -16.43998781665510123 ) ) ;
#28520 = CARTESIAN_POINT ( 'NONE',  ( 10.63343953641030026, 32.99774508120760430, -46.06167227688830224 ) ) ;
#28521 = CARTESIAN_POINT ( 'NONE',  ( 18.58015777933965751, 20.12863169291996712, -15.71908887857641623 ) ) ;
#28522 = CARTESIAN_POINT ( 'NONE',  ( 51.93112808046510054, -50.81522873917079863, -50.63472941081700185 ) ) ;
#28523 = CARTESIAN_POINT ( 'NONE',  ( 11.57443829055679352, -65.35522060805175215, -22.57612245162195208 ) ) ;
#28524 = CARTESIAN_POINT ( 'NONE',  ( 0.1457840918200039859, -10.50670027737364620, -34.68167776469301344 ) ) ;
#28525 = ORIENTED_EDGE ( 'NONE', *, *, #29715, .F. ) ;
#28526 = CARTESIAN_POINT ( 'NONE',  ( 66.63393739769620083, 11.88381105532070059, -71.50000000000000000 ) ) ;
#28527 = CARTESIAN_POINT ( 'NONE',  ( 11.13393739769619906, -63.39706025650779253, -43.75139571400850258 ) ) ;
#28528 = CARTESIAN_POINT ( 'NONE',  ( 13.67087992646597527, 20.77208395194776713, -75.25166008038891619 ) ) ;
#28529 = LINE ( 'NONE', #32701, #3276 ) ;
#28530 = CARTESIAN_POINT ( 'NONE',  ( 50.38251485953870201, -49.88132833114089948, -76.14999999999999147 ) ) ;
#28531 = CARTESIAN_POINT ( 'NONE',  ( 8.428838513752189954, -17.68687267757047721, -44.42434460177876332 ) ) ;
#28532 = AXIS2_PLACEMENT_3D ( 'NONE', #3077, #6751, #14084 ) ;
#28533 = EDGE_LOOP ( 'NONE', ( #47576, #24108, #48388, #20062 ) ) ;
#28534 = CARTESIAN_POINT ( 'NONE',  ( 19.54197404232941793, -9.703304558279992165, -68.11948528069008546 ) ) ;
#28535 = CARTESIAN_POINT ( 'NONE',  ( 16.13393739769620083, -15.61618894467929941, -18.58999999999999986 ) ) ;
#28536 = LINE ( 'NONE', #20669, #38594 ) ;
#28537 = CARTESIAN_POINT ( 'NONE',  ( 52.60283376768439467, 22.91519262962889769, -56.84002502892810327 ) ) ;
#28538 = AXIS2_PLACEMENT_3D ( 'NONE', #44857, #29116, #1084 ) ;
#28539 = CARTESIAN_POINT ( 'NONE',  ( 23.37753514989420012, -19.55484501754060034, -73.95085834214698650 ) ) ;
#28540 = EDGE_CURVE ( 'NONE', #34565, #12115, #45526, .T. ) ;
#28541 = CARTESIAN_POINT ( 'NONE',  ( 10.62805030875319012, -55.23623230473515378, -21.20049831036011412 ) ) ;
#28542 = CARTESIAN_POINT ( 'NONE',  ( 54.85910183373169247, 19.81893354343910119, -75.32013207243669228 ) ) ;
#28543 = APPLICATION_PROTOCOL_DEFINITION ( 'draft international standard', 'automotive_design', 1998, #38860 ) ;
#28544 = CARTESIAN_POINT ( 'NONE',  ( 47.19371938996459903, -54.14421669766970524, -75.51723258725520793 ) ) ;
#28545 = ORIENTED_EDGE ( 'NONE', *, *, #31291, .F. ) ;
#28546 = CARTESIAN_POINT ( 'NONE',  ( 11.49411317949089906, -9.787061648994210827, -65.51866386832369926 ) ) ;
#28547 = CARTESIAN_POINT ( 'NONE',  ( 11.79459217608825483, 10.62527906362197605, -34.70142521051213436 ) ) ;
#28548 = CARTESIAN_POINT ( 'NONE',  ( 66.10673863877181589, -1.463538230407920082, -16.72118890776879852 ) ) ;
#28549 = CARTESIAN_POINT ( 'NONE',  ( 47.50309824425600169, 23.36724547216629944, -74.14999584438369595 ) ) ;
#28550 = FACE_OUTER_BOUND ( 'NONE', #41766, .T. ) ;
#28551 = ADVANCED_FACE ( 'NONE', ( #48510 ), #13147, .T. ) ;
#28552 = CARTESIAN_POINT ( 'NONE',  ( 60.68762404489650919, -30.63429797783443931, -16.28103577270612590 ) ) ;
#28553 = CARTESIAN_POINT ( 'NONE',  ( 12.36320305067610015, 33.31445045643330616, -15.76422791930239953 ) ) ;
#28554 = CARTESIAN_POINT ( 'NONE',  ( 14.86785676567460079, -49.61616128341084675, -83.20618638372945952 ) ) ;
#28555 = EDGE_CURVE ( 'NONE', #6777, #43941, #5560, .T. ) ;
#28556 = B_SPLINE_CURVE_WITH_KNOTS ( 'NONE', 3,
 ( #46390, #3129, #34560, #30625, #26686, #42710, #19098, #35073, #51079, #15177, #8862, #12801, #32156, #28757, #44498, #44758 ),
 .UNSPECIFIED., .F., .F.,
 ( 4, 2, 2, 2, 2, 2, 2, 4 ),
 ( 0.000000000000000000, 0.04580887700494568754, 0.3154492010360799292, 0.4839744035555390567, 0.6054138568059892478, 0.7268533100564364968, 0.8786526266194979451, 1.000000000000000000 ),
 .UNSPECIFIED. ) ;
#28557 = CARTESIAN_POINT ( 'NONE',  ( 44.40502284445533832, -15.61618894467929763, 9.349999999999999645 ) ) ;
#28559 = EDGE_CURVE ( 'NONE', #9084, #17470, #17320, .T. ) ;
#28558 = CARTESIAN_POINT ( 'NONE',  ( 63.18711801607420142, 1.188042061556800144, -68.87465088918141021 ) ) ;
#28560 = CARTESIAN_POINT ( 'NONE',  ( 61.49802603650289257, 13.92071365815219863, -46.55134034995590042 ) ) ;
#28561 = CARTESIAN_POINT ( 'NONE',  ( 13.04555273158159956, -65.52070318195430332, -47.48197110827570100 ) ) ;
#28562 = ORIENTED_EDGE ( 'NONE', *, *, #23403, .T. ) ;
#28563 = CARTESIAN_POINT ( 'NONE',  ( 52.81767045377850422, -49.66725257592850085, -48.48656228474339969 ) ) ;
#28564 = AXIS2_PLACEMENT_3D ( 'NONE', #49368, #45427, #25480 ) ;
#28565 = CARTESIAN_POINT ( 'NONE',  ( 57.76710182873919308, -45.11618912136610504, -25.37614636620249797 ) ) ;
#28566 = LINE ( 'NONE', #44566, #29362 ) ;
#28567 = CARTESIAN_POINT ( 'NONE',  ( 57.13943934813359959, 14.62469886311279943, -26.25200977877019781 ) ) ;
#28568 = TOROIDAL_SURFACE ( 'NONE', #41985, 15.56227766016839986, 1.399999999999999911 ) ;
#28569 = CARTESIAN_POINT ( 'NONE',  ( 11.66494716225189876, -10.15993774188009979, -33.73437862127239839 ) ) ;
#28570 = CARTESIAN_POINT ( 'NONE',  ( 50.72812903946289254, 18.91210722878299677, -76.16412222909750085 ) ) ;
#28571 = CARTESIAN_POINT ( 'NONE',  ( 52.75740204447090065, 18.47005112969250007, -48.47378032971769812 ) ) ;
#28572 = CARTESIAN_POINT ( 'NONE',  ( 71.12477309692330607, 1.336371993404949832, -70.52842906692660563 ) ) ;
#28573 = CARTESIAN_POINT ( 'NONE',  ( 41.83063930241069528, -43.61086970063350066, -3.362295850879169823 ) ) ;
#28574 = DIRECTION ( 'NONE',  ( 1.000000000000000000, 2.460964292799963328E-14, 0.000000000000000000 ) ) ;
#28575 = ORIENTED_EDGE ( 'NONE', *, *, #25860, .T. ) ;
#28576 = CARTESIAN_POINT ( 'NONE',  ( 73.13683269167130163, 0.9254905997697669973, -68.96226957534490509 ) ) ;
#28577 = CARTESIAN_POINT ( 'NONE',  ( 47.55278177603999978, -54.57312067195669414, -54.95467727275750747 ) ) ;
#28578 = FACE_BOUND ( 'NONE', #4997, .T. ) ;
#28579 = CARTESIAN_POINT ( 'NONE',  ( 16.13393739769620083, -15.61618894467929941, -32.14999999999999858 ) ) ;
#28580 = CARTESIAN_POINT ( 'NONE',  ( 41.36298005976649961, 12.80050257910570011, -3.553636961524439641 ) ) ;
#28581 = CARTESIAN_POINT ( 'NONE',  ( 59.03790284062520044, -28.86438846994849783, -15.69185385446090031 ) ) ;
#28582 = CARTESIAN_POINT ( 'NONE',  ( 71.45393474093610564, 0.9259537755896120048, -60.65222959644560063 ) ) ;
#28583 = CARTESIAN_POINT ( 'NONE',  ( 46.81384049422970151, 7.939671762211538919, -34.68207991959079806 ) ) ;
#28584 = CARTESIAN_POINT ( 'NONE',  ( 71.64047750585169183, 1.027568165751340024, -60.79177686748120379 ) ) ;
#28585 = DIRECTION ( 'NONE',  ( -1.000000000000000000, 0.000000000000000000, 0.000000000000000000 ) ) ;
#28586 = CARTESIAN_POINT ( 'NONE',  ( 65.03067915409710054, 1.194703186106680137, -70.66446396659920026 ) ) ;
#28587 = ORIENTED_EDGE ( 'NONE', *, *, #36658, .F. ) ;
#28588 = ORIENTED_EDGE ( 'NONE', *, *, #37281, .F. ) ;
#28589 = CARTESIAN_POINT ( 'NONE',  ( 57.20288281111999851, 18.94155152855249824, -52.64687565416169690 ) ) ;
#28590 = CARTESIAN_POINT ( 'NONE',  ( 15.53930990683081070, 7.815833215755628061, 4.943674098299959851 ) ) ;
#28591 = ORIENTED_EDGE ( 'NONE', *, *, #50569, .F. ) ;
#28592 = CARTESIAN_POINT ( 'NONE',  ( 11.32941480849519955, -64.39195845186381462, -44.31825940040779699 ) ) ;
#28593 = LINE ( 'NONE', #39639, #31889 ) ;
#28594 = FACE_OUTER_BOUND ( 'NONE', #20853, .T. ) ;
#28595 = CARTESIAN_POINT ( 'NONE',  ( 51.82948429423599634, 19.25463815188989969, -76.37482632157400531 ) ) ;
#28596 = EDGE_LOOP ( 'NONE', ( #1602, #23225 ) ) ;
#28597 = CARTESIAN_POINT ( 'NONE',  ( 19.50681848041033106, -9.682899184164803330, -72.11765224560839727 ) ) ;
#28598 = CARTESIAN_POINT ( 'NONE',  ( 23.04647303881236553, -11.63208075929189356, -35.34099930627255759 ) ) ;
#28599 = CARTESIAN_POINT ( 'NONE',  ( 22.44565080833970327, -10.31100337979670023, -39.56984226053619835 ) ) ;
#28600 = EDGE_CURVE ( 'NONE', #42649, #14039, #44968, .T. ) ;
#28601 = DIRECTION ( 'NONE',  ( -1.224646799147357151E-16, 1.000000000000000000, 3.740764114965448302E-16 ) ) ;
#28602 = CARTESIAN_POINT ( 'NONE',  ( 42.30137742020378511, -37.67163298317260001, -78.81279910741842798 ) ) ;
#28603 = VERTEX_POINT ( 'NONE', #22774 ) ;
#28604 = VECTOR ( 'NONE', #15905, 999.9999999999998863 ) ;
#28605 = CARTESIAN_POINT ( 'NONE',  ( 11.39018864042530055, -63.93570751189418644, -24.36152679348629846 ) ) ;
#28606 = B_SPLINE_CURVE_WITH_KNOTS ( 'NONE', 3,
 ( #24941, #5587, #41215, #13708, #37286, #5068, #21025, #25466 ),
 .UNSPECIFIED., .F., .F.,
 ( 4, 2, 2, 4 ),
 ( 0.08616863070364449984, 0.1028498217467809922, 0.1208689123369260099, 0.1272047750342873151 ),
 .UNSPECIFIED. ) ;
#28607 = CARTESIAN_POINT ( 'NONE',  ( 14.87826689285460091, -8.191960251112410774, -81.45916290265100201 ) ) ;
#28608 = VECTOR ( 'NONE', #29793, 1000.000000000000000 ) ;
#28609 = CARTESIAN_POINT ( 'NONE',  ( 14.06316976997283064, -7.911111869945884223, -32.92433297370318712 ) ) ;
#28610 = CARTESIAN_POINT ( 'NONE',  ( 14.69599431308540005, 20.96156756881190120, -75.93682688742939035 ) ) ;
#28611 = CARTESIAN_POINT ( 'NONE',  ( 24.04486774516310277, -15.65047751723203362, -59.79370488822283392 ) ) ;
#28612 = CARTESIAN_POINT ( 'NONE',  ( 83.23750369908759694, -44.81947700284720781, -46.42259446247490473 ) ) ;
#28613 = CARTESIAN_POINT ( 'NONE',  ( 45.34397758664299971, -33.92854118026809829, -34.64999999999999858 ) ) ;
#28614 = CARTESIAN_POINT ( 'NONE',  ( 24.27816550820259778, -16.90237291014140197, -43.55752607316119906 ) ) ;
#28615 = EDGE_LOOP ( 'NONE', ( #50528, #46132, #46361, #12237 ) ) ;
#28616 = CARTESIAN_POINT ( 'NONE',  ( 52.81789460724309748, -49.66430887009229878, -28.03531209662209989 ) ) ;
#28617 = CARTESIAN_POINT ( 'NONE',  ( 15.00539844364359965, -50.92316721421990167, -21.20430891277609931 ) ) ;
#28618 = CARTESIAN_POINT ( 'NONE',  ( 50.60551416901743238, -35.90772131913882248, -76.23178625769983796 ) ) ;
#28619 = CARTESIAN_POINT ( 'NONE',  ( 24.04493739769619864, -15.61618894467929941, -32.14999999999999858 ) ) ;
#28621 = EDGE_CURVE ( 'NONE', #50052, #51387, #39892, .T. ) ;
#28620 = CARTESIAN_POINT ( 'NONE',  ( 22.90120720387987774, -15.61618909956830770, -56.84718059981966576 ) ) ;
#28622 = DIRECTION ( 'NONE',  ( -1.000000000000000000, 0.000000000000000000, 0.000000000000000000 ) ) ;
#28623 = CIRCLE ( 'NONE', #40462, 6.099999999999994316 ) ;
#28624 = EDGE_LOOP ( 'NONE', ( #28903, #51872, #46007, #31045, #12187, #34974, #34458, #49140, #21883, #48375, #42749, #37021, #5868 ) ) ;
#28625 = CARTESIAN_POINT ( 'NONE',  ( -5.256770087461370089, -47.44903047538170426, -5.577592548843699483 ) ) ;
#28626 = CARTESIAN_POINT ( 'NONE',  ( 47.30384360797479815, 23.48520776747849936, -54.69971079365609512 ) ) ;
#28627 = CARTESIAN_POINT ( 'NONE',  ( 63.11947343109709863, 1.194703186106690129, -62.54674175640080591 ) ) ;
#28628 = CARTESIAN_POINT ( 'NONE',  ( 18.47369125467839979, -4.651823196201450017, -35.14999999999999858 ) ) ;
#28629 = CARTESIAN_POINT ( 'NONE',  ( 10.85466582836039962, 33.73459203646100235, -17.55961494274570001 ) ) ;
#28630 = PLANE ( 'NONE',  #9378 ) ;
#28631 = CARTESIAN_POINT ( 'NONE',  ( 21.50893739769619728, 1.920825481955539926, -35.14999999999999858 ) ) ;
#28632 = CARTESIAN_POINT ( 'NONE',  ( 72.17449546179830122, 1.458407608744489936, -61.54081785568290286 ) ) ;
#28633 = CARTESIAN_POINT ( 'NONE',  ( 55.16746451318910260, -48.53221452072369857, -48.68584014076520106 ) ) ;
#28634 = CARTESIAN_POINT ( 'NONE',  ( 23.04644708940202591, -11.63203215977157257, -75.62569094467853859 ) ) ;
#28635 = DIRECTION ( 'NONE',  ( -1.224646799147353207E-16, 1.000000000000000000, 0.000000000000000000 ) ) ;
#28636 = LINE ( 'NONE', #40195, #32931 ) ;
#28637 = CARTESIAN_POINT ( 'NONE',  ( 22.90073451867936072, -15.61618922653637931, -60.45281425156898791 ) ) ;
#28638 = CARTESIAN_POINT ( 'NONE',  ( 17.90521964142824274, -9.025325540544024250, -48.03615471533210268 ) ) ;
#28639 = EDGE_LOOP ( 'NONE', ( #369, #38085, #3814, #12601, #46459 ) ) ;
#28640 = DIRECTION ( 'NONE',  ( 0.000000000000000000, 0.7071067811865475727, 0.7071067811865475727 ) ) ;
#28641 = CARTESIAN_POINT ( 'NONE',  ( 9.287871870417321318, 31.98002424137379762, -46.53019454594979720 ) ) ;
#28642 = AXIS2_PLACEMENT_3D ( 'NONE', #17284, #49770, #13862 ) ;
#28643 = CARTESIAN_POINT ( 'NONE',  ( 16.13393739769620083, -15.61618894467929941, -10.44999999999999929 ) ) ;
#28644 = CARTESIAN_POINT ( 'NONE',  ( 14.30294810761210123, -7.958315104980580479, -81.23899999999999011 ) ) ;
#28645 = ORIENTED_EDGE ( 'NONE', *, *, #51530, .F. ) ;
#28646 = CARTESIAN_POINT ( 'NONE',  ( 18.63937188518799815, 20.22628383398659935, -74.56034069004439857 ) ) ;
#28647 = ORIENTED_EDGE ( 'NONE', *, *, #18490, .F. ) ;
#28648 = ORIENTED_EDGE ( 'NONE', *, *, #15582, .T. ) ;
#28649 = ORIENTED_EDGE ( 'NONE', *, *, #29390, .F. ) ;
#28650 = CARTESIAN_POINT ( 'NONE',  ( 11.36715134725919896, -64.83549888376190040, -46.20270877207719451 ) ) ;
#28651 = DIRECTION ( 'NONE',  ( 0.6676418852213051869, -0.2329255526947263677, -0.7071067811865459074 ) ) ;
#28652 = CARTESIAN_POINT ( 'NONE',  ( 23.18878377121089684, -17.50908265191390001, -81.23899999999999011 ) ) ;
#28653 = CARTESIAN_POINT ( 'NONE',  ( 61.60982433611909670, 13.90674965645299821, -46.62866983784309838 ) ) ;
#28654 = EDGE_LOOP ( 'NONE', ( #45175, #30882, #6601, #39083 ) ) ;
#28655 = CARTESIAN_POINT ( 'NONE',  ( 22.90097009252848892, -15.61618913824531418, -68.84717732178738459 ) ) ;
#28656 = B_SPLINE_SURFACE_WITH_KNOTS ( 'NONE', 3, 3, ( 
 ( #44320, #29363, #40650, #45368, #550, #24894, #41169, #16283 ),
 ( #9472, #1340, #20715, #28844, #33293, #8685, #32488, #25420 ),
 ( #24376, #16807, #12621, #48260, #49309, #17073, #33024, #49049 ),
 ( #40391, #44847, #29105, #36705, #45104, #5281, #4748, #13404 ),
 ( #32237, #24637, #41423, #301, #12354, #28319, #8952, #8430 ),
 ( #20454, #21232, #48516, #4485, #32756, #36444, #16536, #38016 ) ),
 .UNSPECIFIED., .F., .F., .F.,
 ( 4, 1, 1, 4 ),
 ( 4, 2, 2, 4 ),
 ( 0.000000000000000000, 0.3333333333333329818, 0.6666666666666670737, 1.000000000000000000 ),
 ( -18.06426057213299785, -15.10764099038530084, -11.44518256847369919, -9.383697485516369952 ),
 .UNSPECIFIED. ) ;
#28657 = CARTESIAN_POINT ( 'NONE',  ( 16.13393739769620083, -15.61618894467929941, -15.18999999999999950 ) ) ;
#28658 = ORIENTED_EDGE ( 'NONE', *, *, #9758, .F. ) ;
#28659 = CARTESIAN_POINT ( 'NONE',  ( 52.23246088134759901, -46.22137412629599851, -14.08618647836389925 ) ) ;
#28660 = EDGE_CURVE ( 'NONE', #42919, #36517, #34816, .T. ) ;
#28661 = DIRECTION ( 'NONE',  ( 1.000000000000000000, 0.000000000000000000, 0.000000000000000000 ) ) ;
#28662 = CARTESIAN_POINT ( 'NONE',  ( 2.277530937145189949, -15.61618894467929941, -24.15000000000000213 ) ) ;
#28663 = VERTEX_POINT ( 'NONE', #50581 ) ;
#28664 = ORIENTED_EDGE ( 'NONE', *, *, #32495, .F. ) ;
#28665 = ADVANCED_FACE ( 'NONE', ( #9967 ), #42984, .T. ) ;
#28666 = CARTESIAN_POINT ( 'NONE',  ( 72.13393739769617241, 0.6411703679100281272, -20.65000000000000924 ) ) ;
#28667 = CARTESIAN_POINT ( 'NONE',  ( 73.38393739769610136, 4.883811055320659733, -84.94863984844540994 ) ) ;
#28668 = DIRECTION ( 'NONE',  ( 0.000000000000000000, 0.000000000000000000, 1.000000000000000000 ) ) ;
#28669 = EDGE_CURVE ( 'NONE', #40528, #9856, #42726, .T. ) ;
#28670 = CARTESIAN_POINT ( 'NONE',  ( 50.02872888617959291, 13.97177871515139991, -11.19014215844219962 ) ) ;
#28671 = CARTESIAN_POINT ( 'NONE',  ( 12.63673238537484345, 34.26275087728654256, -22.96425606342529946 ) ) ;
#28672 = CARTESIAN_POINT ( 'NONE',  ( -3.772792344368970152, 16.77021858688409850, -4.559953443787880367 ) ) ;
#28673 = VECTOR ( 'NONE', #42100, 1000.000000000000000 ) ;
#28674 = CARTESIAN_POINT ( 'NONE',  ( 8.223596773276058869, -15.61622589296290009, -36.79233150823699816 ) ) ;
#28675 = ADVANCED_FACE ( 'NONE', ( #50061 ), #10494, .F. ) ;
#28676 = CARTESIAN_POINT ( 'NONE',  ( 55.89838737928348422, 14.67644932428170534, -17.62829472177295642 ) ) ;
#28677 = CARTESIAN_POINT ( 'NONE',  ( 20.66963613231810015, -9.211957127206400031, -62.98365807428779561 ) ) ;
#28678 = ORIENTED_EDGE ( 'NONE', *, *, #21347, .F. ) ;
#28679 = CARTESIAN_POINT ( 'NONE',  ( 18.00872666787291365, 1.264432139860217852, -34.81767276520689336 ) ) ;
#28680 = CARTESIAN_POINT ( 'NONE',  ( 28.63393739769619728, -8.399310579809030841, -34.64999999999999858 ) ) ;
#28681 = CARTESIAN_POINT ( 'NONE',  ( 11.14789759608520114, 32.56083963058139830, -43.84340685660220061 ) ) ;
#28683 = EDGE_CURVE ( 'NONE', #24767, #46747, #3040, .T. ) ;
#28682 = CARTESIAN_POINT ( 'NONE',  ( 72.47840029513230320, 1.274155933524790063, -69.69643145772678849 ) ) ;
#28684 = CARTESIAN_POINT ( 'NONE',  ( 43.02789550845886168, -39.86892128716395689, -71.36382768978903357 ) ) ;
#28685 = CARTESIAN_POINT ( 'NONE',  ( 14.49955684666403144, 10.74943050428832869, -34.64999999999999858 ) ) ;
#28686 = CARTESIAN_POINT ( 'NONE',  ( 46.38667117663079864, 21.75602067995220068, -76.14873014785041505 ) ) ;
#28687 = CARTESIAN_POINT ( 'NONE',  ( 49.71697407881319464, -53.65078623385990397, -55.07777775019589939 ) ) ;
#28688 = FACE_OUTER_BOUND ( 'NONE', #36790, .T. ) ;
#28689 = AXIS2_PLACEMENT_3D ( 'NONE', #50875, #19666, #11045 ) ;
#28690 = CARTESIAN_POINT ( 'NONE',  ( 76.77796743388176992, -43.16487758388229423, -14.54547455625814045 ) ) ;
#28691 = CARTESIAN_POINT ( 'NONE',  ( 8.428876971878688451, -17.68701251098292815, -38.42433540610390708 ) ) ;
#28692 = CARTESIAN_POINT ( 'NONE',  ( 8.222950854910955343, -16.65183494035026612, -54.75066497266151799 ) ) ;
#28693 = ORIENTED_EDGE ( 'NONE', *, *, #23919, .F. ) ;
#28694 = CARTESIAN_POINT ( 'NONE',  ( 8.683664543233660993, -15.60484291453579964, -44.06782744062269330 ) ) ;
#28695 =( BOUNDED_CURVE ( )  B_SPLINE_CURVE ( 3, ( #761, #12069, #16757, #23819 ),
 .UNSPECIFIED., .F., .T. ) 
 B_SPLINE_CURVE_WITH_KNOTS ( ( 4, 4 ),
 ( 4.712388980384691450, 5.497787143782140618 ),
 .UNSPECIFIED. ) 
 CURVE ( )  GEOMETRIC_REPRESENTATION_ITEM ( )  RATIONAL_B_SPLINE_CURVE ( ( 1.000000000000000000, 0.9492530216741910110, 0.9492530216741910110, 1.000000000000000000 ) ) 
 REPRESENTATION_ITEM ( '' )  );
#28696 = CARTESIAN_POINT ( 'NONE',  ( 64.45046735905599178, 1.051325075268649822, -60.92209273815699788 ) ) ;
#28697 = ORIENTED_EDGE ( 'NONE', *, *, #16192, .T. ) ;
#28698 = CARTESIAN_POINT ( 'NONE',  ( 8.222268241235530795, -15.61616536502389962, -60.50766849176299900 ) ) ;
#28699 = CARTESIAN_POINT ( 'NONE',  ( 60.87556493381669753, -45.60883372431879224, -47.59991427375260287 ) ) ;
#28700 = CARTESIAN_POINT ( 'NONE',  ( 8.222732946675209931, -15.61637358666110131, -80.79233150823698395 ) ) ;
#28701 = DIRECTION ( 'NONE',  ( 0.000000000000000000, 0.000000000000000000, -1.000000000000000000 ) ) ;
#28703 = CARTESIAN_POINT ( 'NONE',  ( 24.04490680206547992, -15.61618865440000192, -77.79233401716611240 ) ) ;
#28702 = CARTESIAN_POINT ( 'NONE',  ( 42.92778368268686506, 8.626831504079211399, -71.84863307370312668 ) ) ;
#28704 = EDGE_CURVE ( 'NONE', #33893, #38344, #10748, .T. ) ;
#28705 = DIRECTION ( 'NONE',  ( 0.000000000000000000, 0.000000000000000000, 1.000000000000000000 ) ) ;
#28706 = CARTESIAN_POINT ( 'NONE',  ( 20.11807062262020551, -22.52871098524190785, -51.84099987359497419 ) ) ;
#28707 = ORIENTED_EDGE ( 'NONE', *, *, #40702, .F. ) ;
#28708 = CARTESIAN_POINT ( 'NONE',  ( 82.73840718283260287, -45.54981251556409916, -47.62304481396609646 ) ) ;
#28709 = VERTEX_POINT ( 'NONE', #6043 ) ;
#28710 = ORIENTED_EDGE ( 'NONE', *, *, #49208, .T. ) ;
#28711 = ORIENTED_EDGE ( 'NONE', *, *, #5097, .T. ) ;
#28712 = DIRECTION ( 'NONE',  ( 0.000000000000000000, 0.000000000000000000, 1.000000000000000000 ) ) ;
#28713 = CARTESIAN_POINT ( 'NONE',  ( 23.04646684753098995, -11.63206918574938875, -79.62566678159748790 ) ) ;
#28714 = CIRCLE ( 'NONE', #49662, 29.70020322226740106 ) ;
#28715 = CARTESIAN_POINT ( 'NONE',  ( 76.42336834388106581, -22.53308218664625073, -12.89720526797597522 ) ) ;
#28716 = CARTESIAN_POINT ( 'NONE',  ( 53.21998863634129151, -52.13732859160620592, -53.98245948904320812 ) ) ;
#28717 = CIRCLE ( 'NONE', #46329, 17.09468304687040785 ) ;
#28718 = ORIENTED_EDGE ( 'NONE', *, *, #43773, .T. ) ;
#28719 = ORIENTED_EDGE ( 'NONE', *, *, #14566, .T. ) ;
#28720 = CARTESIAN_POINT ( 'NONE',  ( 14.06313845534990037, -23.32125801677240062, -56.09093780913883620 ) ) ;
#28721 = CARTESIAN_POINT ( 'NONE',  ( -8.460328592820898663, 14.65132278408173860, -42.51048757408748457 ) ) ;
#28722 = CARTESIAN_POINT ( 'NONE',  ( 14.53805447820786512, 18.38379093432319422, -83.18296600395719054 ) ) ;
#28723 = CARTESIAN_POINT ( 'NONE',  ( 49.72648160330889766, -53.64673639094029767, -55.11972614036120177 ) ) ;
#28724 = CARTESIAN_POINT ( 'NONE',  ( 23.94343574623035664, -14.32673947065577202, -59.74025267311575504 ) ) ;
#28725 = B_SPLINE_CURVE_WITH_KNOTS ( 'NONE', 3,
 ( #30634, #18593, #19107, #14923, #31146, #7073, #25920, #39045, #38522, #26697, #46658 ),
 .UNSPECIFIED., .F., .F.,
 ( 4, 1, 1, 1, 1, 1, 1, 1, 4 ),
 ( 0.000000000000000000, 0.01976910049033019090, 0.09898803155395019537, 0.1782069626175702137, 0.2574258936811890663, 0.3366448247448090569, 0.4158637558084279373, 0.4950826868720638041, 0.5000016690426868360 ),
 .UNSPECIFIED. ) ;
#28726 = B_SPLINE_CURVE_WITH_KNOTS ( 'NONE', 3,
 ( #24953, #40965, #9274, #26264, #34642, #26781, #30713, #41744, #34906, #6113, #42536, #42796, #2695, #2175, #46476, #18668, #46735, #50647 ),
 .UNSPECIFIED., .F., .F.,
 ( 4, 2, 2, 2, 2, 2, 2, 2, 4 ),
 ( 0.5000000032451481502, 0.5625000028395046314, 0.6250000024338611126, 0.6875000020282175939, 0.7500000016225740751, 0.8125000012169305563, 0.8750000008112870375, 0.9375000004056435188, 1.000000000000000000 ),
 .UNSPECIFIED. ) ;
#28727 = EDGE_CURVE ( 'NONE', #29939, #50146, #48038, .T. ) ;
#28728 = EDGE_LOOP ( 'NONE', ( #38473, #23019, #37108, #40793 ) ) ;
#28729 = CARTESIAN_POINT ( 'NONE',  ( -110.7194986169279929, 1.883811055205739882, -112.4763993716680091 ) ) ;
#28730 = CARTESIAN_POINT ( 'NONE',  ( 52.22858155659860557, -49.81590603655720173, -77.10495058180190142 ) ) ;
#28731 = CARTESIAN_POINT ( 'NONE',  ( 68.13393739769620083, 16.88381105532069881, -71.50000000000000000 ) ) ;
#28732 = CARTESIAN_POINT ( 'NONE',  ( 47.40322300430410252, -54.65574458090419796, -54.88279555090289819 ) ) ;
#28733 = EDGE_CURVE ( 'NONE', #14240, #30697, #36501, .T. ) ;
#28734 = CARTESIAN_POINT ( 'NONE',  ( 13.40148368168809867, -22.97284880370879989, -68.62569607034480157 ) ) ;
#28735 = LINE ( 'NONE', #36871, #9632 ) ;
#28736 = CIRCLE ( 'NONE', #38794, 16.00000000000000000 ) ;
#28737 = CARTESIAN_POINT ( 'NONE',  ( 54.17303629415799548, 19.38381105532069881, -77.01199944720809754 ) ) ;
#28738 = B_SPLINE_CURVE_WITH_KNOTS ( 'NONE', 3,
 ( #14327, #30298, #17742, #33455, #18517, #46316, #10143, #1758, #13815, #10666 ),
 .UNSPECIFIED., .F., .F.,
 ( 4, 2, 2, 2, 4 ),
 ( 0.000000000000000000, 0.2538046189272509245, 0.5511430180573008153, 0.8049079287776087499, 1.000000000000000000 ),
 .UNSPECIFIED. ) ;
#28739 = CARTESIAN_POINT ( 'NONE',  ( 41.40756461421400303, -44.77159006877079861, -5.393981499654329603 ) ) ;
#28740 = CYLINDRICAL_SURFACE ( 'NONE', #38552, 0.5000000000000014433 ) ;
#28741 = VECTOR ( 'NONE', #40418, 1000.000000000000000 ) ;
#28742 = CARTESIAN_POINT ( 'NONE',  ( 61.04001029137710077, -45.35933836075930259, -46.86320535112459851 ) ) ;
#28743 = CARTESIAN_POINT ( 'NONE',  ( 61.41208173005990290, -45.43591354592849996, -47.45931927210430246 ) ) ;
#28744 = CARTESIAN_POINT ( 'NONE',  ( 64.28413441608979895, 1.451794159057709921, -69.91814348332408713 ) ) ;
#28745 = DIRECTION ( 'NONE',  ( -1.000000000000000000, 0.000000000000000000, 0.000000000000000000 ) ) ;
#28746 = CARTESIAN_POINT ( 'NONE',  ( 65.34027601680769237, 0.8063996746146668837, -17.56710917073600342 ) ) ;
#28747 = ORIENTED_EDGE ( 'NONE', *, *, #11532, .T. ) ;
#28748 = CARTESIAN_POINT ( 'NONE',  ( 13.58892339565109886, -51.93864758878270038, -75.09854824053589084 ) ) ;
#28749 = CARTESIAN_POINT ( 'NONE',  ( 47.38131715433139846, -54.66763248196649982, -54.77717321816150076 ) ) ;
#28750 = CARTESIAN_POINT ( 'NONE',  ( 22.72480996509791851, -13.84493836002453016, -38.36948975162746223 ) ) ;
#28751 = CARTESIAN_POINT ( 'NONE',  ( 61.13393739769620083, 4.883811055320659733, -84.38499399519520239 ) ) ;
#28752 = CIRCLE ( 'NONE', #48874, 9.999999999999998224 ) ;
#28753 = CARTESIAN_POINT ( 'NONE',  ( 19.28335304380221160, -8.292279851470313545, -55.13679355289837503 ) ) ;
#28754 = CARTESIAN_POINT ( 'NONE',  ( 23.34518454799010101, -17.37660377373440213, -32.14999999999999858 ) ) ;
#28755 = CARTESIAN_POINT ( 'NONE',  ( 22.13393739769619728, -54.15188668067469990, -54.64999999999999858 ) ) ;
#28756 = CARTESIAN_POINT ( 'NONE',  ( 47.74681726949440019, -54.47399125802040487, -54.93559451776580005 ) ) ;
#28758 = CARTESIAN_POINT ( 'NONE',  ( -6.924536278744959361, -46.06766666375389718, -5.623594431461650167 ) ) ;
#28757 = CARTESIAN_POINT ( 'NONE',  ( 47.32200658827643025, 22.89650621548869225, -75.47293010799739932 ) ) ;
#28759 = DIRECTION ( 'NONE',  ( 0.000000000000000000, 0.000000000000000000, 1.000000000000000000 ) ) ;
#28760 = CARTESIAN_POINT ( 'NONE',  ( 48.64758560217519801, 22.70397928459539827, -54.52813621919599996 ) ) ;
#28761 = EDGE_LOOP ( 'NONE', ( #3485, #2501 ) ) ;
#28762 = CARTESIAN_POINT ( 'NONE',  ( 12.24635195013770073, -21.50085024014760293, -59.53301288856830098 ) ) ;
#28763 = ORIENTED_EDGE ( 'NONE', *, *, #34538, .T. ) ;
#28764 = CARTESIAN_POINT ( 'NONE',  ( 72.38393739883420608, 4.883811055320659733, -61.34712802272770915 ) ) ;
#28765 = CARTESIAN_POINT ( 'NONE',  ( 23.62413055734840128, 17.52287609088140030, -35.14999999999999858 ) ) ;
#28766 = DIRECTION ( 'NONE',  ( 0.5112408204145768575, 0.8594375041513085955, 0.000000000000000000 ) ) ;
#28768 = CARTESIAN_POINT ( 'NONE',  ( 52.92551367776950144, 18.26402201841269957, -27.38996126115440077 ) ) ;
#28767 = CARTESIAN_POINT ( 'NONE',  ( 84.23484834998549786, 12.58064488669169911, -47.06355581890329631 ) ) ;
#28769 = EDGE_CURVE ( 'NONE', #39784, #25775, #9740, .T. ) ;
#28770 = CARTESIAN_POINT ( 'NONE',  ( 20.30862021219660107, -9.931597306316877649, -64.15444814970220477 ) ) ;
#28771 = DIRECTION ( 'NONE',  ( 0.000000000000000000, 5.782411586589432581E-16, -1.000000000000000000 ) ) ;
#28772 = CARTESIAN_POINT ( 'NONE',  ( 57.30396242925620243, -45.11618894467940066, -16.63931852905170317 ) ) ;
#28773 = EDGE_CURVE ( 'NONE', #37113, #41542, #17296, .T. ) ;
#28774 = CIRCLE ( 'NONE', #2914, 0.9999999999999974465 ) ;
#28775 = ORIENTED_EDGE ( 'NONE', *, *, #34757, .T. ) ;
#28776 = ORIENTED_EDGE ( 'NONE', *, *, #26820, .T. ) ;
#28777 = AXIS2_PLACEMENT_3D ( 'NONE', #8318, #4635, #20608 ) ;
#28778 = EDGE_CURVE ( 'NONE', #1009, #42867, #23949, .T. ) ;
#28779 = CARTESIAN_POINT ( 'NONE',  ( 12.12214211477839854, -65.05677813791820085, -16.43788246316010060 ) ) ;
#28780 = CARTESIAN_POINT ( 'NONE',  ( 12.93642320027750081, 34.28151823598130221, -47.70347891814760288 ) ) ;
#28781 = CARTESIAN_POINT ( 'NONE',  ( 61.37881371176925427, -45.32822124412814446, -47.24538866281226746 ) ) ;
#28782 = CARTESIAN_POINT ( 'NONE',  ( 47.18323533445099827, -54.80730216070119809, -54.61058630203390152 ) ) ;
#28783 = B_SPLINE_CURVE_WITH_KNOTS ( 'NONE', 3,
 ( #6019, #21976, #34286, #14131, #30099, #46124, #10208, #6279, #22494, #22237, #34554, #18312, #26426, #42444, #38503, #15941, #35067, #31129 ),
 .UNSPECIFIED., .F., .F.,
 ( 4, 2, 2, 2, 2, 2, 2, 2, 4 ),
 ( 0.000000000000000000, 0.06393429766015837346, 0.09590144649023724099, 0.1278685953203161085, 0.1918028929804706795, 0.2557371906406252227, 0.3836057859609320331, 0.4475400836210886024, 0.5114743812812451162 ),
 .UNSPECIFIED. ) ;
#28784 = CARTESIAN_POINT ( 'NONE',  ( 14.06336563596984313, -23.32131676130726561, -64.09100251094548639 ) ) ;
#28785 = VERTEX_POINT ( 'NONE', #17825 ) ;
#28786 = CARTESIAN_POINT ( 'NONE',  ( 16.13393739769620083, -15.61618894467929941, -10.90000000000000036 ) ) ;
#28787 = DIRECTION ( 'NONE',  ( 0.000000000000000000, 0.000000000000000000, -1.000000000000000000 ) ) ;
#28788 = CIRCLE ( 'NONE', #30478, 1.000000000000000888 ) ;
#28789 = DIRECTION ( 'NONE',  ( 0.000000000000000000, -1.000000000000000000, 0.000000000000000000 ) ) ;
#28790 = CARTESIAN_POINT ( 'NONE',  ( 50.39203494574510245, -49.33609294867260076, -76.16300746230109553 ) ) ;
#28791 = DIRECTION ( 'NONE',  ( 0.000000000000000000, 0.000000000000000000, -1.000000000000000000 ) ) ;
#28792 = CIRCLE ( 'NONE', #2019, 33.00000000000000000 ) ;
#28793 = ORIENTED_EDGE ( 'NONE', *, *, #12374, .F. ) ;
#28794 = CARTESIAN_POINT ( 'NONE',  ( 55.01074116390070401, -47.06068843752009911, -25.62222821926219751 ) ) ;
#28795 = CARTESIAN_POINT ( 'NONE',  ( 16.13393739769620083, -15.61618894467929941, -17.93019253464870033 ) ) ;
#28796 = EDGE_LOOP ( 'NONE', ( #376, #21379, #562, #14170 ) ) ;
#28797 = CARTESIAN_POINT ( 'NONE',  ( 57.07894516969589915, -50.21246463426640361, -52.67137581470450414 ) ) ;
#28798 = CARTESIAN_POINT ( 'NONE',  ( 52.90945400079600347, 18.90700577772100033, -50.10580952084150397 ) ) ;
#28799 = ADVANCED_FACE ( 'NONE', ( #42203 ), #6821, .F. ) ;
#28800 = CARTESIAN_POINT ( 'NONE',  ( 23.10711481198539730, -20.01590724778190022, -79.97149710298219816 ) ) ;
#28801 = LINE ( 'NONE', #5239, #11294 ) ;
#28802 = CARTESIAN_POINT ( 'NONE',  ( 53.79001371717119895, 20.06659692491659897, -75.54591657906719604 ) ) ;
#28803 = CARTESIAN_POINT ( 'NONE',  ( 46.61193351516349992, -53.28955996511189852, -76.10144452841760199 ) ) ;
#28804 = ORIENTED_EDGE ( 'NONE', *, *, #35846, .F. ) ;
#28805 = CARTESIAN_POINT ( 'NONE',  ( 22.13393739769619728, -54.15188668067469990, -34.64999999999999858 ) ) ;
#28806 = CARTESIAN_POINT ( 'NONE',  ( 23.34874387044599686, -13.75789365977069956, -66.15241531683260234 ) ) ;
#28807 = CARTESIAN_POINT ( 'NONE',  ( 13.63393739769599833, 14.38381105532070059, -35.14999999999999858 ) ) ;
#28808 = CARTESIAN_POINT ( 'NONE',  ( -13.39236625349549925, -0.8785706602474870897, -54.64999999999999858 ) ) ;
#28809 = CIRCLE ( 'NONE', #27136, 0.9999999999999974465 ) ;
#28810 = CARTESIAN_POINT ( 'NONE',  ( 46.49861198364799719, 21.90968872996920069, -76.13710305591399674 ) ) ;
#28811 = CARTESIAN_POINT ( 'NONE',  ( 16.13393739769620083, -15.61618894467929941, 2.750000000000000000 ) ) ;
#28812 = CARTESIAN_POINT ( 'NONE',  ( 12.32380480340579965, 33.40949394495549285, -15.85794303743209888 ) ) ;
#28813 = VECTOR ( 'NONE', #16191, 1000.000000000000000 ) ;
#28814 = DIRECTION ( 'NONE',  ( 0.000000000000000000, 0.000000000000000000, 1.000000000000000000 ) ) ;
#28815 = FACE_OUTER_BOUND ( 'NONE', #11206, .T. ) ;
#28816 = DIRECTION ( 'NONE',  ( 0.000000000000000000, 0.000000000000000000, 1.000000000000000000 ) ) ;
#28818 = FACE_OUTER_BOUND ( 'NONE', #2733, .T. ) ;
#28817 = CARTESIAN_POINT ( 'NONE',  ( 50.03007040746459921, 5.621799825072190337, -76.14999999999999147 ) ) ;
#28819 = TOROIDAL_SURFACE ( 'NONE', #43911, 15.56227766016839986, 1.399999999999999911 ) ;
#28820 = CARTESIAN_POINT ( 'NONE',  ( 63.13104210372130609, 0.9254905997697669973, -68.96226957534490509 ) ) ;
#28821 = DIRECTION ( 'NONE',  ( 0.000000000000000000, 0.000000000000000000, 1.000000000000000000 ) ) ;
#28822 = CARTESIAN_POINT ( 'NONE',  ( 8.223600577592289795, -15.61621812327629932, -68.50766849176299900 ) ) ;
#28823 = CARTESIAN_POINT ( 'NONE',  ( -32.29328640865499978, -20.30120719130589890, -55.80050612416169997 ) ) ;
#28824 = EDGE_LOOP ( 'NONE', ( #3323, #26384, #11988, #35347 ) ) ;
#28825 = CARTESIAN_POINT ( 'NONE',  ( 52.75763549665710173, -49.70454645220410583, -48.62438309228340216 ) ) ;
#28826 = CARTESIAN_POINT ( 'NONE',  ( 58.79269946044950501, -45.11618907922949973, -25.61455272403410177 ) ) ;
#28827 = CARTESIAN_POINT ( 'NONE',  ( 48.50471607674010244, -54.16716192014190057, -55.31622937648409533 ) ) ;
#28828 = CARTESIAN_POINT ( 'NONE',  ( 57.35648317541490115, 14.51146209784109864, -26.25116064136519967 ) ) ;
#28829 = CARTESIAN_POINT ( 'NONE',  ( 22.93861538555659862, -13.76175748592850034, -34.36813006978140095 ) ) ;
#28830 = CARTESIAN_POINT ( 'NONE',  ( 51.24890051900759858, 19.15053050095109910, -76.23258468917369157 ) ) ;
#28831 = CARTESIAN_POINT ( 'NONE',  ( 52.75620127927579972, 18.48103312263130249, -48.74711883110850152 ) ) ;
#28832 = CARTESIAN_POINT ( 'NONE',  ( 71.09473187122610227, 1.382830464309369844, -70.35440931850220636 ) ) ;
#28833 = PLANE ( 'NONE',  #8353 ) ;
#28834 = CARTESIAN_POINT ( 'NONE',  ( 64.89116046657669301, -43.41583358990930464, -10.41655519546019981 ) ) ;
#28835 = EDGE_CURVE ( 'NONE', #29183, #20094, #23689, .T. ) ;
#28836 = ORIENTED_EDGE ( 'NONE', *, *, #3663, .F. ) ;
#28837 = CARTESIAN_POINT ( 'NONE',  ( 16.13393739566809870, -15.61618894418049841, 9.349999999609689638 ) ) ;
#28838 = CARTESIAN_POINT ( 'NONE',  ( 12.17768353250039937, -9.303127112852680014, -76.38915131457939367 ) ) ;
#28839 = ADVANCED_FACE ( 'NONE', ( #7332 ), #40068, .T. ) ;
#28840 = CARTESIAN_POINT ( 'NONE',  ( 72.99790115655470402, 1.264791438333819906, -68.87905435786350949 ) ) ;
#28841 = CARTESIAN_POINT ( 'NONE',  ( 47.42962603948429745, -54.62656463334229784, -54.65340493925440057 ) ) ;
#28842 = FACE_BOUND ( 'NONE', #2062, .T. ) ;
#28843 = DIRECTION ( 'NONE',  ( 1.000000000000000000, 0.000000000000000000, -1.224646799147353207E-16 ) ) ;
#28844 = CARTESIAN_POINT ( 'NONE',  ( 58.76033327212790169, 16.72714852453529844, -50.08083992869450185 ) ) ;
#28845 = CARTESIAN_POINT ( 'NONE',  ( 71.23034918703520191, 1.369664981662519931, -60.92138556078450051 ) ) ;
#28846 = DIRECTION ( 'NONE',  ( -1.224646799147353700E-16, 1.000000000000000000, 5.351958659602136763E-17 ) ) ;
#28847 = CARTESIAN_POINT ( 'NONE',  ( 71.43600178900840092, 1.367958924391370124, -60.98859505255219915 ) ) ;
#28848 = CARTESIAN_POINT ( 'NONE',  ( 24.04215780991690110, -15.84268857627947646, -71.51678454628235215 ) ) ;
#28849 = CARTESIAN_POINT ( 'NONE',  ( 65.21688447373020381, 1.383136297697689976, -70.36878149631539259 ) ) ;
#28850 = VERTEX_POINT ( 'NONE', #24048 ) ;
#28851 = ORIENTED_EDGE ( 'NONE', *, *, #11370, .T. ) ;
#28852 = VECTOR ( 'NONE', #29000, 1000.000000000000000 ) ;
#28853 = CARTESIAN_POINT ( 'NONE',  ( 9.283462026593010563, -63.18182653024980056, -46.53091203316120072 ) ) ;
#28854 = DIRECTION ( 'NONE',  ( 0.000000000000000000, 0.000000000000000000, 1.000000000000000000 ) ) ;
#28855 = ORIENTED_EDGE ( 'NONE', *, *, #34098, .F. ) ;
#28856 = CARTESIAN_POINT ( 'NONE',  ( 13.14827817127709864, -9.226478610231410471, -72.20804185874739289 ) ) ;
#28857 = CARTESIAN_POINT ( 'NONE',  ( 19.54190978043818916, -9.703266135105563350, -70.11948897317647322 ) ) ;
#28858 = CARTESIAN_POINT ( 'NONE',  ( 20.85900685591025550, -10.71576073910020099, -50.19691013058185547 ) ) ;
#28859 = CARTESIAN_POINT ( 'NONE',  ( 53.20629916227129996, 19.50996791044699918, -76.43613545957519761 ) ) ;
#28860 = VERTEX_POINT ( 'NONE', #3406 ) ;
#28861 = DIRECTION ( 'NONE',  ( 1.060511545910580040E-15, 5.351958659602149705E-17, -1.000000000000000000 ) ) ;
#28862 = CARTESIAN_POINT ( 'NONE',  ( 22.55005608494040104, -13.41974511834900774, -72.34789028957942492 ) ) ;
#28863 = CARTESIAN_POINT ( 'NONE',  ( 9.221475126720598325, -11.63195346281944786, -34.67433465466491072 ) ) ;
#28864 = EDGE_CURVE ( 'NONE', #49018, #1956, #3660, .T. ) ;
#28865 = B_SPLINE_SURFACE_WITH_KNOTS ( 'NONE', 3, 3, ( 
 ( #41013, #17174, #9826, #25777, #37340, #6153, #49412, #5125 ),
 ( #41784, #21855, #9319, #32858, #33905, #49919, #17426, #5643 ),
 ( #45989, #14011, #22110, #29971, #918, #10082, #13508, #1700 ),
 ( #37081, #45468, #1179, #21589, #37587, #48888, #17682, #26040 ),
 ( #12992, #28942, #44947, #9047, #24994, #21079, #6412, #22632 ),
 ( #22885, #26828, #38903, #31258, #35209, #14271, #42314, #50686 ),
 ( #10344, #42836, #10605, #30751, #14782, #38121, #18455, #34158 ),
 ( #50173, #19223, #18708, #2993, #15304, #34424, #15038, #38647 ),
 ( #46773, #50435, #30494, #34943, #34684, #27343, #43092, #39155 ),
 ( #10859, #18963, #6667, #14524, #2466, #22370, #7184, #47290 ),
 ( #46516, #11380, #2216, #30237, #43347, #26302, #3250, #11119 ),
 ( #50944, #26560, #51210, #31008, #42574, #6931, #47035, #7441 ),
 ( #18194, #23140, #38376, #46254, #2735, #27088, #31769, #19738 ),
 ( #19481, #4520, #4020, #24153, #588, #35731, #338, #23899 ) ),
 .UNSPECIFIED., .F., .F., .F.,
 ( 4, 2, 2, 2, 2, 2, 4 ),
 ( 4, 1, 1, 1, 1, 4 ),
 ( 3.901346948265469905, 4.407177605192729608, 8.834505823316810336, 16.99747883129379744, 26.70074659151990204, 31.55238047163300052, 38.13654360031040369 ),
 ( -1.140694639499999985E-05, 0.2000000000000000111, 0.4000000000000000222, 0.5999999999999999778, 0.8000000000000000444, 1.000037278610800051 ),
 .UNSPECIFIED. ) ;
#28866 = CARTESIAN_POINT ( 'NONE',  ( 7.971080360336099346, -14.45408523004980061, -40.83734515755419636 ) ) ;
#28867 = CARTESIAN_POINT ( 'NONE',  ( 22.90093739619960900, -15.61165398910431179, -56.45261194681012284 ) ) ;
#28868 = CARTESIAN_POINT ( 'NONE',  ( 53.62552786343490396, 20.09834016026489678, -75.58099297212140755 ) ) ;
#28869 = EDGE_CURVE ( 'NONE', #31144, #18163, #13933, .T. ) ;
#28870 = ORIENTED_EDGE ( 'NONE', *, *, #6384, .F. ) ;
#28871 = CARTESIAN_POINT ( 'NONE',  ( 11.62168671107460050, -64.72337088029789243, -24.07512666974249882 ) ) ;
#28872 = CARTESIAN_POINT ( 'NONE',  ( 23.25862214412349971, -12.32596019608740079, -79.87478428137859510 ) ) ;
#28873 = CARTESIAN_POINT ( 'NONE',  ( 11.29067012326649966, -10.76071234358520101, -32.14999999999999858 ) ) ;
#28874 = CARTESIAN_POINT ( 'NONE',  ( 14.62118626177969993, 20.66382337739360153, -75.74020909530109691 ) ) ;
#28875 = CARTESIAN_POINT ( 'NONE',  ( 24.04493741964421361, -14.58064922431956667, -51.75066236550382115 ) ) ;
#28876 = B_SPLINE_CURVE_WITH_KNOTS ( 'NONE', 3,
 ( #15898, #11977, #12223, #27932, #43934, #8031, #49688, #17450, #14035, #41807, #17705, #25799, #2242, #21878, #49944, #17959, #13782, #5913 ),
 .UNSPECIFIED., .F., .F.,
 ( 4, 2, 2, 2, 2, 2, 2, 2, 4 ),
 ( 0.5000013706141720471, 0.5625011992874004996, 0.6250010279606290631, 0.6875008566338575156, 0.7500006853070859680, 0.8125005139803145315, 0.8750003426535429840, 0.9375001713267714365, 1.000000000000000000 ),
 .UNSPECIFIED. ) ;
#28877 = CARTESIAN_POINT ( 'NONE',  ( 84.37258452300260103, -43.45091051789750480, -47.24504068948050417 ) ) ;
#28878 = CARTESIAN_POINT ( 'NONE',  ( 22.39113274415149846, -10.24681029298479906, -55.28192787057689372 ) ) ;
#28879 = ORIENTED_EDGE ( 'NONE', *, *, #13735, .F. ) ;
#28880 = CARTESIAN_POINT ( 'NONE',  ( 52.89242001099999868, -49.58003531765110239, -27.72111690325079891 ) ) ;
#28881 = CIRCLE ( 'NONE', #46507, 0.5000000000336679573 ) ;
#28882 = CARTESIAN_POINT ( 'NONE',  ( 15.85308752006570110, -51.11618894234659649, -21.66365682949659899 ) ) ;
#28883 = FACE_OUTER_BOUND ( 'NONE', #26100, .T. ) ;
#28884 = FACE_OUTER_BOUND ( 'NONE', #35093, .T. ) ;
#28885 = CARTESIAN_POINT ( 'NONE',  ( 16.13393739769599833, 14.38381105532070059, -34.64999999999999858 ) ) ;
#28886 = ORIENTED_EDGE ( 'NONE', *, *, #46861, .T. ) ;
#28887 = CARTESIAN_POINT ( 'NONE',  ( -9.076360731184159647, -44.08689318531880730, -5.731288650940340013 ) ) ;
#28888 = CARTESIAN_POINT ( 'NONE',  ( 47.25362900639890285, 23.52000032359880066, -54.62089388818540669 ) ) ;
#28889 = CARTESIAN_POINT ( 'NONE',  ( 56.42249722295453296, -45.43314942095580733, -25.29439854063558357 ) ) ;
#28890 = CARTESIAN_POINT ( 'NONE',  ( 63.25085271618998917, 1.186614556332920234, -62.31696408872340243 ) ) ;
#28891 = CARTESIAN_POINT ( 'NONE',  ( 24.04481203031673076, -15.61619115162449312, -61.50767625960597229 ) ) ;
#28892 = CARTESIAN_POINT ( 'NONE',  ( 42.05805489943670494, 13.23020005123530041, -5.167112210102939862 ) ) ;
#28893 = DIRECTION ( 'NONE',  ( 1.000000000000000000, 0.000000000000000000, 0.000000000000000000 ) ) ;
#28894 = CARTESIAN_POINT ( 'NONE',  ( 10.72267370182032309, -19.77493159281586088, -65.24448734500967362 ) ) ;
#28895 = CARTESIAN_POINT ( 'NONE',  ( 72.46078431608199821, 1.446932438105759999, -61.88285690311300158 ) ) ;
#28896 = CARTESIAN_POINT ( 'NONE',  ( 53.97790768284939844, -49.20362396525460014, -49.10634432982389797 ) ) ;
#28897 = CARTESIAN_POINT ( 'NONE',  ( 22.89703504567739856, -15.86470445441918642, -66.46450912331485483 ) ) ;
#28898 = EDGE_CURVE ( 'NONE', #5276, #19930, #41118, .T. ) ;
#28899 = CARTESIAN_POINT ( 'NONE',  ( 64.70533732122679282, 1.100585178972000033, -60.77016257896750062 ) ) ;
#28900 = CARTESIAN_POINT ( 'NONE',  ( 17.43325189934310160, -52.80674074535590279, -76.12862656241330228 ) ) ;
#28901 = CARTESIAN_POINT ( 'NONE',  ( 12.72591286716733805, -21.52908169620734924, -61.11950314682426466 ) ) ;
#28902 = CARTESIAN_POINT ( 'NONE',  ( 14.22831053668800116, -22.40670773495260093, -61.43426723409519496 ) ) ;
#28903 = ORIENTED_EDGE ( 'NONE', *, *, #26788, .F. ) ;
#28904 = FACE_OUTER_BOUND ( 'NONE', #49878, .T. ) ;
#28905 = CARTESIAN_POINT ( 'NONE',  ( 9.729176998844950575, 31.90615194671379840, -46.30113559920939537 ) ) ;
#28906 = CARTESIAN_POINT ( 'NONE',  ( 41.50322886078625828, 13.56217550620411672, -5.449103212913565031 ) ) ;
#28907 = CARTESIAN_POINT ( 'NONE',  ( 13.13393739769619906, 32.28996932333459569, -46.39999999999999858 ) ) ;
#28908 = ORIENTED_EDGE ( 'NONE', *, *, #4010, .F. ) ;
#28909 = CARTESIAN_POINT ( 'NONE',  ( 18.48574654752910007, 20.09246212084070038, -74.56515407679859209 ) ) ;
#28910 = EDGE_LOOP ( 'NONE', ( #26482, #9018, #14351, #34040 ) ) ;
#28911 = ORIENTED_EDGE ( 'NONE', *, *, #1727, .T. ) ;
#28912 = VERTEX_POINT ( 'NONE', #20136 ) ;
#28913 = CARTESIAN_POINT ( 'NONE',  ( 12.86012610505919973, -65.50554804669809528, -47.57962905350179739 ) ) ;
#28914 = CARTESIAN_POINT ( 'NONE',  ( 57.38580998192630034, -45.30275844272679819, -25.91614474311650085 ) ) ;
#28915 = CARTESIAN_POINT ( 'NONE',  ( 21.41354075005730095, -20.28432539553539726, -81.23899999999999011 ) ) ;
#28916 = CARTESIAN_POINT ( 'NONE',  ( 61.42450914986659427, 14.00539997787450019, -46.99871816792220613 ) ) ;
#28917 = CARTESIAN_POINT ( 'NONE',  ( 16.13393739769620083, -15.61618894467929941, -9.721247897589949005 ) ) ;
#28918 = VERTEX_POINT ( 'NONE', #19632 ) ;
#28919 = VERTEX_POINT ( 'NONE', #32171 ) ;
#28920 = AXIS2_PLACEMENT_3D ( 'NONE', #6873, #11835, #22822 ) ;
#28921 = CARTESIAN_POINT ( 'NONE',  ( 12.13696580915320311, 33.93507363936925003, -16.64705451129685443 ) ) ;
#28922 = ORIENTED_EDGE ( 'NONE', *, *, #39208, .F. ) ;
#28923 = CARTESIAN_POINT ( 'NONE',  ( 22.90079931266048874, -15.61618915558698184, -42.84717230777439312 ) ) ;
#28924 = CIRCLE ( 'NONE', #22222, 0.9999999999999995559 ) ;
#28925 = CARTESIAN_POINT ( 'NONE',  ( 24.04379852435330989, -15.76128024319491772, -33.79816624355701293 ) ) ;
#28926 = EDGE_CURVE ( 'NONE', #14552, #14297, #20594, .T. ) ;
#28927 = CARTESIAN_POINT ( 'NONE',  ( 8.784728771152170879, -54.93525725209899235, -46.67204636145419983 ) ) ;
#28928 = ORIENTED_EDGE ( 'NONE', *, *, #25195, .F. ) ;
#28929 = ORIENTED_EDGE ( 'NONE', *, *, #5353, .T. ) ;
#28930 = CARTESIAN_POINT ( 'NONE',  ( 0.3209249304026170480, -10.53407907283069989, -34.64999999999999858 ) ) ;
#28931 = DIRECTION ( 'NONE',  ( 1.000000000000000000, 0.000000000000000000, 0.000000000000000000 ) ) ;
#28932 = CARTESIAN_POINT ( 'NONE',  ( 60.47553822224839593, 14.59310891045189962, -47.74689862142960095 ) ) ;
#28933 = CARTESIAN_POINT ( 'NONE',  ( 51.02726976822560090, 14.97164679345370075, -13.20165271163509857 ) ) ;
#28934 = CARTESIAN_POINT ( 'NONE',  ( 22.46011036989908760, -20.47785625781408214, -68.00066293900144387 ) ) ;
#28935 = CARTESIAN_POINT ( 'NONE',  ( -9.464298943378709694, 12.47750318557470095, -5.578887212681300056 ) ) ;
#28937 = AXIS2_PLACEMENT_3D ( 'NONE', #1525, #8617, #32954 ) ;
#28936 = CARTESIAN_POINT ( 'NONE',  ( -2.927979189508790103, -49.19984425798019601, -5.740620115512199639 ) ) ;
#28938 = CARTESIAN_POINT ( 'NONE',  ( 55.83253168230204011, 14.69212688956227986, -17.34603649656557778 ) ) ;
#28939 = CARTESIAN_POINT ( 'NONE',  ( 9.981643928145130573, -20.48815294779980078, -74.07430842319449482 ) ) ;
#28940 = EDGE_LOOP ( 'NONE', ( #23121, #2836, #3738, #22261, #8438, #48852, #37964, #10060 ) ) ;
#28941 = CARTESIAN_POINT ( 'NONE',  ( 57.37174218388170033, 16.14477099907140101, -48.15837671390720232 ) ) ;
#28942 = CARTESIAN_POINT ( 'NONE',  ( -8.925905124820840086, -44.39248591613520034, -6.403223950166009537 ) ) ;
#28943 = CARTESIAN_POINT ( 'NONE',  ( 11.39852503586600108, 33.29352875594079819, -44.68676662896000096 ) ) ;
#28944 = CARTESIAN_POINT ( 'NONE',  ( 72.40605974471309025, 1.033004162168289941, -69.86315739208521336 ) ) ;
#28945 = CARTESIAN_POINT ( 'NONE',  ( 11.60439326024719975, -64.93477792032190621, -16.46429631545650096 ) ) ;
#28946 = AXIS2_PLACEMENT_3D ( 'NONE', #43921, #660, #8016 ) ;
#28947 = CARTESIAN_POINT ( 'NONE',  ( 16.65420337941059969, -49.11618894467930829, -17.90311212357429937 ) ) ;
#28948 = CARTESIAN_POINT ( 'NONE',  ( 12.61030219803810049, 18.86097712249150149, -21.13761110129019727 ) ) ;
#28949 = CARTESIAN_POINT ( 'NONE',  ( -0.8602693046289622281, -12.42650008425934693, -35.51452756723926996 ) ) ;
#28950 = CARTESIAN_POINT ( 'NONE',  ( 49.54598800151290305, -53.61194117850519802, -54.50101998263480141 ) ) ;
#28951 = CIRCLE ( 'NONE', #4689, 16.60961179679779676 ) ;
#28952 = CARTESIAN_POINT ( 'NONE',  ( 42.48652067527369525, -44.25687345361960467, -5.094659063150840161 ) ) ;
#28953 = EDGE_CURVE ( 'NONE', #21893, #11156, #27307, .T. ) ;
#28954 = CARTESIAN_POINT ( 'NONE',  ( 20.77870735952862091, -22.07375217990394489, -33.80906069049880358 ) ) ;
#28955 = CARTESIAN_POINT ( 'NONE',  ( 12.06284766121009966, 32.21085600226960111, -22.25048313876769868 ) ) ;
#28956 = CARTESIAN_POINT ( 'NONE',  ( 64.93393739769619799, 1.530257664727400879, -61.30355339059330078 ) ) ;
#28957 = ORIENTED_EDGE ( 'NONE', *, *, #6557, .F. ) ;
#28958 = EDGE_CURVE ( 'NONE', #37692, #23421, #33988, .T. ) ;
#28959 = CARTESIAN_POINT ( 'NONE',  ( 11.33709965304220013, -21.31680662961520056, -39.79000516318719605 ) ) ;
#28960 = EDGE_CURVE ( 'NONE', #4297, #37620, #15191, .T. ) ;
#28961 = CARTESIAN_POINT ( 'NONE',  ( 64.56659382095870114, 1.382578538659519962, -61.11374307182889254 ) ) ;
#28962 = ORIENTED_EDGE ( 'NONE', *, *, #43077, .T. ) ;
#28963 = CARTESIAN_POINT ( 'NONE',  ( 84.22672017746327811, -43.79043011566170662, -46.99906225576258834 ) ) ;
#28964 = CARTESIAN_POINT ( 'NONE',  ( 60.58228858412009998, -45.68472658336609982, -47.55887949375219392 ) ) ;
#28965 = CARTESIAN_POINT ( 'NONE',  ( 17.63393739769620083, -42.11618894467939356, -34.64999999999999858 ) ) ;
#28966 = CARTESIAN_POINT ( 'NONE',  ( 13.19614975339650087, 18.82172381217750257, -21.01902014737410340 ) ) ;
#28968 = CARTESIAN_POINT ( 'NONE',  ( 19.21265657477716005, 18.23736444591407135, -34.79644660940672907 ) ) ;
#28967 = CARTESIAN_POINT ( 'NONE',  ( 43.14635114408183370, 8.647671771403498298, -70.79083171591096857 ) ) ;
#28969 = EDGE_CURVE ( 'NONE', #41896, #30141, #35623, .T. ) ;
#28970 = CARTESIAN_POINT ( 'NONE',  ( 9.366361720925400647, -15.59697802929608024, -59.84808272681433294 ) ) ;
#28971 = CARTESIAN_POINT ( 'NONE',  ( 37.63393739769620083, -15.61618894467929941, -11.05000000000000071 ) ) ;
#28972 = ORIENTED_EDGE ( 'NONE', *, *, #15303, .T. ) ;
#28973 = CARTESIAN_POINT ( 'NONE',  ( 84.30744353797240365, -43.93553367712969759, -47.37637942009979497 ) ) ;
#28974 = ORIENTED_EDGE ( 'NONE', *, *, #22235, .F. ) ;
#28975 = EDGE_LOOP ( 'NONE', ( #23240, #41494, #14703, #9701 ) ) ;
#28976 = EDGE_LOOP ( 'NONE', ( #45871, #24932, #18573, #26792, #16831 ) ) ;
#28977 = DIRECTION ( 'NONE',  ( 0.9805806756909202226, 0.000000000000000000, -0.1961161351381840445 ) ) ;
#28978 = CARTESIAN_POINT ( 'NONE',  ( 52.60089517322759889, -49.82971139612260458, -48.60938815635680044 ) ) ;
#28979 = CARTESIAN_POINT ( 'NONE',  ( 24.04493737386696139, -14.58064414827727084, -79.75066707260157273 ) ) ;
#28980 = CARTESIAN_POINT ( 'NONE',  ( 76.42335353787902363, -22.53155339109895650, -12.89714147592827942 ) ) ;
#28981 = CARTESIAN_POINT ( 'NONE',  ( 54.97710707581860134, -51.41017014255020001, -53.92626239532030041 ) ) ;
#28982 = ORIENTED_EDGE ( 'NONE', *, *, #50752, .T. ) ;
#28983 = ORIENTED_EDGE ( 'NONE', *, *, #29136, .T. ) ;
#28984 = FACE_OUTER_BOUND ( 'NONE', #26194, .T. ) ;
#28985 = AXIS2_PLACEMENT_3D ( 'NONE', #25927, #34314, #46143 ) ;
#28986 = CARTESIAN_POINT ( 'NONE',  ( 56.72395159686060140, 19.45340621921160107, -53.71484871595450272 ) ) ;
#28987 = CARTESIAN_POINT ( 'NONE',  ( -9.252977670667002386, 13.99041838265985582, -43.19094538359154711 ) ) ;
#28988 = DIRECTION ( 'NONE',  ( -0.5516667872527503125, 0.8340645993220362486, -1.942890293094025918E-16 ) ) ;
#28989 = CARTESIAN_POINT ( 'NONE',  ( 22.90093741420372098, -14.73039702075610968, -36.41115092250901597 ) ) ;
#28990 = EDGE_CURVE ( 'NONE', #7271, #45182, #51355, .T. ) ;
#28991 = CARTESIAN_POINT ( 'NONE',  ( 11.97527360937055363, -10.20486319393767793, -53.74448780049490182 ) ) ;
#28992 = ORIENTED_EDGE ( 'NONE', *, *, #4402, .F. ) ;
#28993 = CYLINDRICAL_SURFACE ( 'NONE', #15797, 0.4999999999999994449 ) ;
#28994 = CARTESIAN_POINT ( 'NONE',  ( 53.57535180181819356, -50.54591161070089811, -77.11818236577570929 ) ) ;
#28995 = CARTESIAN_POINT ( 'NONE',  ( 62.50953355103300169, -29.38356811901130072, -16.13223000750240388 ) ) ;
#28996 = PLANE ( 'NONE',  #50479 ) ;
#28997 = AXIS2_PLACEMENT_3D ( 'NONE', #11069, #23338, #19173 ) ;
#28998 = CARTESIAN_POINT ( 'NONE',  ( 17.74647322415179929, -23.29645429165649873, -62.44661944738230375 ) ) ;
#28999 = AXIS2_PLACEMENT_3D ( 'NONE', #41291, #33927, #37361 ) ;
#29000 = DIRECTION ( 'NONE',  ( 0.000000000000000000, -1.000000000000000000, 0.000000000000000000 ) ) ;
#29001 = B_SPLINE_CURVE_WITH_KNOTS ( 'NONE', 3,
 ( #10610, #34948, #39418, #42319 ),
 .UNSPECIFIED., .F., .F.,
 ( 4, 4 ),
 ( 0.000000000000000000, 1.000000000000000000 ),
 .UNSPECIFIED. ) ;
#29002 = CARTESIAN_POINT ( 'NONE',  ( 41.53147706019129970, -44.71252858122500129, -5.331435815133920286 ) ) ;
#29003 = FACE_OUTER_BOUND ( 'NONE', #12043, .T. ) ;
#29004 = CARTESIAN_POINT ( 'NONE',  ( 69.22748654599975282, -50.70395984887971252, -73.25000000000218847 ) ) ;
#29005 = DIRECTION ( 'NONE',  ( 0.000000000000000000, 0.000000000000000000, -1.000000000000000000 ) ) ;
#29006 = ADVANCED_FACE ( 'NONE', ( #27486 ), #47684, .T. ) ;
#29007 = CARTESIAN_POINT ( 'NONE',  ( 63.95040967837109491, 1.031857118852239852, -69.95114096137160686 ) ) ;
#29008 = CARTESIAN_POINT ( 'NONE',  ( 23.04647701948986338, -11.63208821185457253, -41.62566436189668195 ) ) ;
#29009 = CARTESIAN_POINT ( 'NONE',  ( 66.85053883392829732, 1.883667400092539967, -20.46403502974369815 ) ) ;
#29010 = ORIENTED_EDGE ( 'NONE', *, *, #46888, .T. ) ;
#29011 = CARTESIAN_POINT ( 'NONE',  ( 13.94090093824480014, -51.82372487085179813, -75.44171726276898937 ) ) ;
#29012 = AXIS2_PLACEMENT_3D ( 'NONE', #47295, #31525, #35984 ) ;
#29013 = CARTESIAN_POINT ( 'NONE',  ( 47.25382592556910311, -54.75228172359690149, -54.62311712267080566 ) ) ;
#29014 = FACE_OUTER_BOUND ( 'NONE', #45910, .T. ) ;
#29015 = DIRECTION ( 'NONE',  ( 0.000000000000000000, -1.000000000000000000, 0.000000000000000000 ) ) ;
#29016 =( BOUNDED_CURVE ( )  B_SPLINE_CURVE ( 3, ( #29542, #45028, #13325, #37672 ),
 .UNSPECIFIED., .F., .T. ) 
 B_SPLINE_CURVE_WITH_KNOTS ( ( 4, 4 ),
 ( 2.356194490192332403, 3.141592653589799777 ),
 .UNSPECIFIED. ) 
 CURVE ( )  GEOMETRIC_REPRESENTATION_ITEM ( )  RATIONAL_B_SPLINE_CURVE ( ( 1.000000000000000000, 0.9492530216741885685, 0.9492530216741885685, 1.000000000000000000 ) ) 
 REPRESENTATION_ITEM ( '' )  );
#29017 = CARTESIAN_POINT ( 'NONE',  ( 21.72146850305579591, -9.937738037311971695, -55.25497476500451910 ) ) ;
#29018 = CONICAL_SURFACE ( 'NONE', #50768, 36.50000000000000000, 0.1651486774146265213 ) ;
#29019 = CARTESIAN_POINT ( 'NONE',  ( 23.44917627852430186, -16.12890410639889893, -32.14999999999999858 ) ) ;
#29020 = CARTESIAN_POINT ( 'NONE',  ( -21.36606260230379917, -62.11618894467930119, 16.35000000000000142 ) ) ;
#29021 = CARTESIAN_POINT ( 'NONE',  ( 11.93174526809839975, 34.20691394249479345, -17.93019253464870033 ) ) ;
#29023 = CARTESIAN_POINT ( 'NONE',  ( -10.86918838363719964, -42.36073152548370047, -6.289582464405770068 ) ) ;
#29022 = CARTESIAN_POINT ( 'NONE',  ( 13.81950199196250040, 20.03075999784159933, -23.06529969907609967 ) ) ;
#29024 = CARTESIAN_POINT ( 'NONE',  ( 56.31131329977899469, 19.32763365105479636, -52.86805933726900264 ) ) ;
#29025 = B_SPLINE_CURVE_WITH_KNOTS ( 'NONE', 3,
 ( #44572, #32230, #8421, #40898, #5008, #28573, #33283, #40640, #48253, #12877, #20968, #36969, #24369, #24107, #45094, #17062 ),
 .UNSPECIFIED., .F., .F.,
 ( 4, 2, 2, 2, 2, 2, 2, 4 ),
 ( -3.863343447353519977, -3.187258344066659976, -2.414589654595949764, -1.931671723676759989, -1.690212758217169764, -1.313423695611310116, -0.7105611954419281950, 0.000000000000000000 ),
 .UNSPECIFIED. ) ;
#29026 = CARTESIAN_POINT ( 'NONE',  ( 48.62459252948669786, 22.87471263156120216, -55.12045204165480072 ) ) ;
#29027 = VERTEX_POINT ( 'NONE', #33482 ) ;
#29028 = CARTESIAN_POINT ( 'NONE',  ( 10.36088797006879858, -19.66766515473189969, -63.65239730387659023 ) ) ;
#29029 = EDGE_LOOP ( 'NONE', ( #46586, #20416, #1478, #17455, #50491, #49438 ) ) ;
#29030 = CARTESIAN_POINT ( 'NONE',  ( 18.52891444416632538, -52.05916771839714841, -75.36997958377639861 ) ) ;
#29031 = AXIS2_PLACEMENT_3D ( 'NONE', #10743, #7842, #30636 ) ;
#29032 = CARTESIAN_POINT ( 'NONE',  ( 57.55751162049570269, -50.09049722528730086, -52.57651812429949700 ) ) ;
#29033 = CARTESIAN_POINT ( 'NONE',  ( 17.01980114826354296, -22.38317958693441057, -42.91115323773419021 ) ) ;
#29035 = CARTESIAN_POINT ( 'NONE',  ( 54.44101168542169944, 16.53500074836000167, -26.08961774644910392 ) ) ;
#29034 = CARTESIAN_POINT ( 'NONE',  ( 82.46791274550251671, 13.86095180792300141, -46.45744338702559872 ) ) ;
#29036 = CARTESIAN_POINT ( 'NONE',  ( 11.09931817734580051, -10.67704245943470021, -69.69977332415560056 ) ) ;
#29038 = EDGE_CURVE ( 'NONE', #50796, #25606, #20548, .T. ) ;
#29037 = CARTESIAN_POINT ( 'NONE',  ( 16.13393739769620083, -15.61618894467929941, -28.45282021618999835 ) ) ;
#29039 = CARTESIAN_POINT ( 'NONE',  ( 72.76396860142250489, 1.388715606738730068, -68.72506404892941134 ) ) ;
#29040 = DIRECTION ( 'NONE',  ( -0.7071067811865476838, -0.7071067811865473507, 0.000000000000000000 ) ) ;
#29041 = ORIENTED_EDGE ( 'NONE', *, *, #10278, .T. ) ;
#29042 = ORIENTED_EDGE ( 'NONE', *, *, #19288, .F. ) ;
#29043 = CARTESIAN_POINT ( 'NONE',  ( 11.73811129725980074, -65.16604538643500177, -16.79398347925659962 ) ) ;
#29044 = CARTESIAN_POINT ( 'NONE',  ( 11.08014211953469896, 32.97560943143620449, -45.24939445730449705 ) ) ;
#29045 = CARTESIAN_POINT ( 'NONE',  ( 61.14298689117413943, -45.32073797555708694, -46.99579994825386109 ) ) ;
#29046 = CARTESIAN_POINT ( 'NONE',  ( 51.43602479376819758, -51.03778538747950222, -50.03115562382680537 ) ) ;
#29047 = CARTESIAN_POINT ( 'NONE',  ( 8.428889251930748117, -17.68705715933444722, -64.42433529559949079 ) ) ;
#29048 = EDGE_CURVE ( 'NONE', #4830, #8473, #21423, .T. ) ;
#29049 = ORIENTED_EDGE ( 'NONE', *, *, #40157, .T. ) ;
#29050 = CARTESIAN_POINT ( 'NONE',  ( 10.57660162720581454, 23.99589349179882092, -45.49284114600560969 ) ) ;
#29051 = CARTESIAN_POINT ( 'NONE',  ( 0.1457841021255935343, -26.78123956999450428, -34.68167779225149161 ) ) ;
#29052 = CARTESIAN_POINT ( 'NONE',  ( 16.65420337941489848, 17.88381105532299742, -20.15000000000000213 ) ) ;
#29053 = CARTESIAN_POINT ( 'NONE',  ( 72.24311954201340313, 1.458407608744489936, -69.69055806410209186 ) ) ;
#29054 = ADVANCED_FACE ( 'NONE', ( #36375 ), #4938, .T. ) ;
#29055 = CARTESIAN_POINT ( 'NONE',  ( 63.48441347673288959, 1.386342629514219826, -62.63353618948930546 ) ) ;
#29056 = CARTESIAN_POINT ( 'NONE',  ( 12.14980512970851301, -22.52871163933854248, -44.17436150934778993 ) ) ;
#29057 = ORIENTED_EDGE ( 'NONE', *, *, #23589, .F. ) ;
#29058 = CARTESIAN_POINT ( 'NONE',  ( 68.13393739769620083, -49.36618894467930829, -73.25000000000000000 ) ) ;
#29059 = DIRECTION ( 'NONE',  ( 0.000000000000000000, -1.000000000000000000, 0.000000000000000000 ) ) ;
#29060 = ORIENTED_EDGE ( 'NONE', *, *, #18866, .F. ) ;
#29061 = CARTESIAN_POINT ( 'NONE',  ( 14.06336471865839144, -7.911061366011778340, -56.92433474434999852 ) ) ;
#29062 = DIRECTION ( 'NONE',  ( 0.000000000000000000, -1.000000000000000000, 0.000000000000000000 ) ) ;
#29063 = CARTESIAN_POINT ( 'NONE',  ( 17.35390478220470101, -23.36850648025069788, -36.46281005851519552 ) ) ;
#29064 = CARTESIAN_POINT ( 'NONE',  ( 15.07367541409510814, -22.58887879155687273, -65.39521378728271372 ) ) ;
#29065 = DIRECTION ( 'NONE',  ( -1.000000000000000000, 0.000000000000000000, 0.000000000000000000 ) ) ;
#29066 = CARTESIAN_POINT ( 'NONE',  ( 47.26969180900909606, -54.15383702437160451, -75.47109442055590023 ) ) ;
#29067 = ORIENTED_EDGE ( 'NONE', *, *, #36672, .T. ) ;
#29068 = CARTESIAN_POINT ( 'NONE',  ( 54.68760100489050302, 14.48868831793499901, -15.47702518080039980 ) ) ;
#29069 = CARTESIAN_POINT ( 'NONE',  ( 57.20288283122350492, -50.17392941253179828, -52.64687565050539320 ) ) ;
#29070 = AXIS2_PLACEMENT_3D ( 'NONE', #29143, #13194, #40689 ) ;
#29071 = EDGE_CURVE ( 'NONE', #998, #51191, #26390, .T. ) ;
#29072 = CARTESIAN_POINT ( 'NONE',  ( 10.14762331803439821, -11.88703313963030084, -34.02451708608289493 ) ) ;
#29073 = CARTESIAN_POINT ( 'NONE',  ( 12.30798784977628735, 34.11147262445096828, -23.61458995968919083 ) ) ;
#29074 = VERTEX_POINT ( 'NONE', #12551 ) ;
#29075 = ADVANCED_FACE ( 'NONE', ( #28516 ), #7190, .F. ) ;
#29076 = CARTESIAN_POINT ( 'NONE',  ( 47.39377455479480261, 23.20627220416080050, -75.00416199656089589 ) ) ;
#29077 = CARTESIAN_POINT ( 'NONE',  ( 71.29447239804829906, 1.393731187554809958, -61.04935521477050031 ) ) ;
#29078 = FACE_OUTER_BOUND ( 'NONE', #25550, .T. ) ;
#29079 = CARTESIAN_POINT ( 'NONE',  ( 12.36320305067610015, 33.31445045643330616, -15.76422791930239953 ) ) ;
#29080 = CARTESIAN_POINT ( 'NONE',  ( 23.18176326819819977, -19.89530930007790133, -79.68135863817160214 ) ) ;
#29081 = DIRECTION ( 'NONE',  ( 0.000000000000000000, 0.000000000000000000, -1.000000000000000000 ) ) ;
#29082 = CARTESIAN_POINT ( 'NONE',  ( 30.52248363924751828, -35.64217098745972123, -84.61231660026447798 ) ) ;
#29083 = DIRECTION ( 'NONE',  ( 0.000000000000000000, -1.000000000000000000, 0.000000000000000000 ) ) ;
#29084 = CARTESIAN_POINT ( 'NONE',  ( -26.15868020285170203, -41.19545595665919535, -54.51850539491499603 ) ) ;
#29085 = EDGE_LOOP ( 'NONE', ( #31523, #7484, #1260, #382, #47011 ) ) ;
#29086 = EDGE_CURVE ( 'NONE', #31947, #48088, #37172, .T. ) ;
#29087 = CARTESIAN_POINT ( 'NONE',  ( 52.73517777097259795, -49.71750526155659600, -48.54845401890089818 ) ) ;
#29088 = CARTESIAN_POINT ( 'NONE',  ( 61.18381089449600552, -45.13403188722560344, -27.16748766345810040 ) ) ;
#29089 = CARTESIAN_POINT ( 'NONE',  ( 9.221491627360364873, -19.60045263248064629, -74.62566484353840224 ) ) ;
#29090 = CARTESIAN_POINT ( 'NONE',  ( 56.55569464329139606, 14.33745061368849960, -25.88752018553109835 ) ) ;
#29091 = CARTESIAN_POINT ( 'NONE',  ( 19.70635122345840173, -21.69738725281480285, -32.78375144850900114 ) ) ;
#29092 = CARTESIAN_POINT ( 'NONE',  ( 51.14620401246810388, 18.52529079830420145, -76.32769624451800894 ) ) ;
#29094 = ADVANCED_FACE ( 'NONE', ( #17007 ), #24831, .T. ) ;
#29093 = CARTESIAN_POINT ( 'NONE',  ( 53.14225946812250356, 18.28234889893970205, -48.98057205063000197 ) ) ;
#29095 = CARTESIAN_POINT ( 'NONE',  ( 71.34267188602969156, 0.8850831926798630178, -70.72000234600830026 ) ) ;
#29096 = LINE ( 'NONE', #8673, #10868 ) ;
#29097 = DIRECTION ( 'NONE',  ( 0.000000000000000000, 0.000000000000000000, -1.000000000000000000 ) ) ;
#29098 = ORIENTED_EDGE ( 'NONE', *, *, #43418, .T. ) ;
#29099 = CARTESIAN_POINT ( 'NONE',  ( 13.42399758170009960, -8.676237899047920976, -78.44884352223340329 ) ) ;
#29100 = ORIENTED_EDGE ( 'NONE', *, *, #47661, .T. ) ;
#29101 = CARTESIAN_POINT ( 'NONE',  ( 72.82889308507860449, 1.369976237678180109, -68.83116145970220146 ) ) ;
#29102 = CARTESIAN_POINT ( 'NONE',  ( 47.47677450096290386, -54.59520210331019285, -54.66133488802340423 ) ) ;
#29103 = CARTESIAN_POINT ( 'NONE',  ( 24.03071935106534696, -15.12947789652383079, -49.77274206133255063 ) ) ;
#29104 = CARTESIAN_POINT ( 'NONE',  ( 73.23405285996879854, 0.9209334348186318797, -62.48938310929649731 ) ) ;
#29105 = CARTESIAN_POINT ( 'NONE',  ( 60.18524539318269717, 15.49018248464509995, -48.88483521943319232 ) ) ;
#29106 = CARTESIAN_POINT ( 'NONE',  ( 53.11114665040049942, 18.28111428451719789, -48.80212166739769941 ) ) ;
#29107 = DIRECTION ( 'NONE',  ( 0.4156269377774486906, 0.5720614028176872479, -0.7071067811865479058 ) ) ;
#29108 = CARTESIAN_POINT ( 'NONE',  ( 72.12565519439380068, 1.270920007605170099, -61.25800542990180730 ) ) ;
#29109 = MECHANICAL_DESIGN_GEOMETRIC_PRESENTATION_REPRESENTATION (  '', ( #13240 ), #49218 ) ;
#29110 = CARTESIAN_POINT ( 'NONE',  ( 37.88393739769619373, -42.11618894467939356, -35.14999999999999858 ) ) ;
#29111 = CARTESIAN_POINT ( 'NONE',  ( 65.19851456808879675, 1.374300485541529948, -70.43861994117489189 ) ) ;
#29112 = ORIENTED_EDGE ( 'NONE', *, *, #32512, .F. ) ;
#29113 = VERTEX_POINT ( 'NONE', #17258 ) ;
#29114 = CARTESIAN_POINT ( 'NONE',  ( 8.788636732660460638, -63.13527780971870129, -46.67124789091300130 ) ) ;
#29115 = AXIS2_PLACEMENT_3D ( 'NONE', #44441, #3587, #20061 ) ;
#29116 = DIRECTION ( 'NONE',  ( 0.000000000000000000, 0.000000000000000000, 1.000000000000000000 ) ) ;
#29117 = VERTEX_POINT ( 'NONE', #25352 ) ;
#29118 = CARTESIAN_POINT ( 'NONE',  ( 11.49293692653489884, -64.67039193628410487, -44.68941390596329910 ) ) ;
#29119 = PLANE ( 'NONE',  #10145 ) ;
#29120 = CARTESIAN_POINT ( 'NONE',  ( 13.24776434638835632, -17.71311640963744338, -643.2998782751060389 ) ) ;
#29121 = CARTESIAN_POINT ( 'NONE',  ( 53.61341609220770010, 19.44707778802039755, -76.60108244557071089 ) ) ;
#29122 = ORIENTED_EDGE ( 'NONE', *, *, #34207, .F. ) ;
#29123 = DIRECTION ( 'NONE',  ( 0.000000000000000000, -1.000000000000000000, 0.000000000000000000 ) ) ;
#29124 = CARTESIAN_POINT ( 'NONE',  ( 9.540065987903542322, -13.85895121319336809, -71.53551241591725329 ) ) ;
#29125 = CARTESIAN_POINT ( 'NONE',  ( 17.16941332651105867, -7.705178615749455950, -43.33403995393874197 ) ) ;
#29126 = CARTESIAN_POINT ( 'NONE',  ( 12.24090637955089989, -8.347968423279731098, -51.13580619582459974 ) ) ;
#29127 = CARTESIAN_POINT ( 'NONE',  ( 22.90092786074403719, -15.60305501299737507, -56.45220756279023533 ) ) ;
#29128 = CARTESIAN_POINT ( 'NONE',  ( 42.30441222516678579, -37.67211025355430110, -78.79762527759561408 ) ) ;
#29129 = ORIENTED_EDGE ( 'NONE', *, *, #12294, .T. ) ;
#29130 = B_SPLINE_CURVE_WITH_KNOTS ( 'NONE', 3,
 ( #39498, #34769, #19569, #27934, #3596, #19313, #35558, #43936 ),
 .UNSPECIFIED., .F., .F.,
 ( 4, 2, 2, 4 ),
 ( 1.104809738474189951, 1.178746485095780061, 1.463424881496269814, 1.779239977503060066 ),
 .UNSPECIFIED. ) ;
#29131 = CARTESIAN_POINT ( 'NONE',  ( 10.64863409883700029, -63.44323389162830296, -23.66469670114080159 ) ) ;
#29132 = CARTESIAN_POINT ( 'NONE',  ( 9.655419314464330327, -11.93712693781080070, -45.39705537816439573 ) ) ;
#29133 = CARTESIAN_POINT ( 'NONE',  ( 12.20479792536879948, -10.10644435241950134, -32.14999999999999858 ) ) ;
#29134 = ADVANCED_FACE ( 'NONE', ( #13333 ), #48714, .F. ) ;
#29135 = CARTESIAN_POINT ( 'NONE',  ( 14.58508199943239880, 20.56214955651219967, -75.65676662446099954 ) ) ;
#29136 = EDGE_CURVE ( 'NONE', #17773, #17470, #20429, .T. ) ;
#29137 = DIRECTION ( 'NONE',  ( 0.000000000000000000, 0.000000000000000000, -1.000000000000000000 ) ) ;
#29138 = CARTESIAN_POINT ( 'NONE',  ( 82.79586663885591236, -45.02293793585479875, -46.43485061813910164 ) ) ;
#29139 = CARTESIAN_POINT ( 'NONE',  ( 20.45336392292970018, -8.592993432514999697, -57.18318221610369534 ) ) ;
#29140 = EDGE_LOOP ( 'NONE', ( #9890, #1300, #9083, #559, #28449 ) ) ;
#29141 = CARTESIAN_POINT ( 'NONE',  ( 56.18973212658190164, -45.98240354813589903, -26.01119312686520146 ) ) ;
#29142 = CARTESIAN_POINT ( 'NONE',  ( 16.33846296856719960, -51.11618894303549610, -21.13414048024940328 ) ) ;
#29143 = CARTESIAN_POINT ( 'NONE',  ( 16.13393739769620083, -15.61618894467929941, -28.45282021618999835 ) ) ;
#29144 = CARTESIAN_POINT ( 'NONE',  ( 10.72251233321565778, -19.77472457186372168, -57.24444900321750396 ) ) ;
#29145 = CARTESIAN_POINT ( 'NONE',  ( 53.92601233233809666, 15.01256046956459933, -15.35059813110260052 ) ) ;
#29146 = ORIENTED_EDGE ( 'NONE', *, *, #33998, .F. ) ;
#29147 = CARTESIAN_POINT ( 'NONE',  ( -8.078265854356109443, -44.94086578754730255, -5.419177366022879916 ) ) ;
#29148 = CARTESIAN_POINT ( 'NONE',  ( 47.25108210846270396, 23.52211893725460001, -54.62737137215419381 ) ) ;
#29149 = CARTESIAN_POINT ( 'NONE',  ( 56.59979300609889208, -45.33386959848365194, -25.29349730390593365 ) ) ;
#29150 = CARTESIAN_POINT ( 'NONE',  ( 63.40811083734029552, 1.369613126987619944, -62.54642937019949755 ) ) ;
#29151 = DIRECTION ( 'NONE',  ( 0.000000000000000000, 1.000000000000000000, 0.000000000000000000 ) ) ;
#29152 = CARTESIAN_POINT ( 'NONE',  ( 10.97564820803400032, 33.77114500669409836, -17.33480536923670101 ) ) ;
#29153 = CARTESIAN_POINT ( 'NONE',  ( 22.90121965235462653, -15.61618904849089340, -42.45282069170939110 ) ) ;
#29155 = EDGE_CURVE ( 'NONE', #50553, #16762, #16734, .T. ) ;
#29154 = FACE_OUTER_BOUND ( 'NONE', #27131, .T. ) ;
#29156 = DIRECTION ( 'NONE',  ( -0.7071067811865470176, 0.000000000000000000, 0.7071067811865480168 ) ) ;
#29157 = CARTESIAN_POINT ( 'NONE',  ( 56.66044069829109731, -47.79715243440499961, -48.40052123592339939 ) ) ;
#29158 = CARTESIAN_POINT ( 'NONE',  ( 10.91612620756760066, 33.86326241729176445, -18.17421237796254019 ) ) ;
#29159 = CARTESIAN_POINT ( 'NONE',  ( 52.62905305334270167, 20.95810661167350020, -53.53065356658779450 ) ) ;
#29160 = EDGE_CURVE ( 'NONE', #51314, #309, #35658, .T. ) ;
#29161 = CARTESIAN_POINT ( 'NONE',  ( 8.222948829813766736, -14.58055777486210225, -76.83399804417695123 ) ) ;
#29162 = CARTESIAN_POINT ( 'NONE',  ( 16.13393739769620083, -15.61618894467929941, -28.45282021618999835 ) ) ;
#29163 = ORIENTED_EDGE ( 'NONE', *, *, #5638, .T. ) ;
#29164 = CYLINDRICAL_SURFACE ( 'NONE', #34667, 6.766999999999998572 ) ;
#29165 = CARTESIAN_POINT ( 'NONE',  ( 8.971085476333328756, 32.00512979024770033, -46.63277124569800236 ) ) ;
#29166 = LINE ( 'NONE', #9014, #8394 ) ;
#29167 = CARTESIAN_POINT ( 'NONE',  ( 66.65424818669949047, -29.91331004332360166, -16.99686723155519985 ) ) ;
#29168 = ORIENTED_EDGE ( 'NONE', *, *, #48028, .F. ) ;
#29169 = CARTESIAN_POINT ( 'NONE',  ( 17.91441070958899928, 19.90988454773669858, -74.52171359303420672 ) ) ;
#29170 = ORIENTED_EDGE ( 'NONE', *, *, #11528, .T. ) ;
#29171 = ORIENTED_EDGE ( 'NONE', *, *, #14967, .F. ) ;
#29172 = CARTESIAN_POINT ( 'NONE',  ( 48.42521416700790127, -56.37491125791819968, -74.14999999999999147 ) ) ;
#29173 = ORIENTED_EDGE ( 'NONE', *, *, #23960, .F. ) ;
#29174 = CARTESIAN_POINT ( 'NONE',  ( 11.85109790645039851, -65.12712902498141432, -46.35237351896630287 ) ) ;
#29175 = CARTESIAN_POINT ( 'NONE',  ( 56.57808279982729971, -46.09595787718389204, -26.23509901551880219 ) ) ;
#29176 = CARTESIAN_POINT ( 'NONE',  ( 22.63681060059330008, -18.70819294529809795, -81.23899999999999011 ) ) ;
#29177 = CARTESIAN_POINT ( 'NONE',  ( 61.31732609679450263, 14.08360619472680142, -47.18614283445869972 ) ) ;
#29178 = DIRECTION ( 'NONE',  ( 0.2201791028319839971, 0.9741803703773870282, 0.04993764759657599861 ) ) ;
#29179 = ORIENTED_EDGE ( 'NONE', *, *, #6688, .F. ) ;
#29180 = AXIS2_PLACEMENT_3D ( 'NONE', #42038, #13747, #38363 ) ;
#29181 = ORIENTED_EDGE ( 'NONE', *, *, #24513, .F. ) ;
#29182 = VECTOR ( 'NONE', #25368, 1000.000000000000000 ) ;
#29183 = VERTEX_POINT ( 'NONE', #5213 ) ;
#29184 = CARTESIAN_POINT ( 'NONE',  ( 54.31501561488440188, -45.11618894460480078, -13.70601682451409964 ) ) ;
#29185 = CARTESIAN_POINT ( 'NONE',  ( 9.366937397696199596, -15.61618894467949836, -28.45282021618999835 ) ) ;
#29186 = DIRECTION ( 'NONE',  ( 1.000000000000000000, 0.000000000000000000, 0.000000000000000000 ) ) ;
#29187 = VERTEX_POINT ( 'NONE', #33221 ) ;
#29188 = CARTESIAN_POINT ( 'NONE',  ( 0.2007819157892938577, -10.51527493241353994, -34.66110989977890000 ) ) ;
#29189 = CARTESIAN_POINT ( 'NONE',  ( 46.59543176902850092, -53.41648962811289891, -76.07661161287319374 ) ) ;
#29190 = DIRECTION ( 'NONE',  ( 1.000000000000000000, 0.000000000000000000, 0.000000000000000000 ) ) ;
#29191 = CARTESIAN_POINT ( 'NONE',  ( 51.09228874323290626, 14.75465462415100149, -13.11143323170220043 ) ) ;
#29192 = EDGE_CURVE ( 'NONE', #28663, #28355, #13045, .T. ) ;
#29193 = DIRECTION ( 'NONE',  ( 0.000000000000000000, 0.000000000000000000, -1.000000000000000000 ) ) ;
#29194 = CARTESIAN_POINT ( 'NONE',  ( 56.17779366879769753, 14.41653637947479893, -28.15000000000000213 ) ) ;
#29195 = CARTESIAN_POINT ( 'NONE',  ( 9.725847485215973975, -18.39314784772030720, -55.71658343890410237 ) ) ;
#29196 = CARTESIAN_POINT ( 'NONE',  ( 61.26764236240780548, 13.92023311689909804, -27.40800516196399883 ) ) ;
#29197 = CARTESIAN_POINT ( 'NONE',  ( 14.19552728039930045, -8.011630154036440743, -74.70805987170351159 ) ) ;
#29198 = ORIENTED_EDGE ( 'NONE', *, *, #16834, .T. ) ;
#29199 = DIRECTION ( 'NONE',  ( 0.000000000000000000, 0.000000000000000000, -1.000000000000000000 ) ) ;
#29200 = CARTESIAN_POINT ( 'NONE',  ( 73.10855093309899644, 0.8936201581567920771, -62.29538467389520662 ) ) ;
#29201 = CARTESIAN_POINT ( 'NONE',  ( 76.63910211808688189, -43.27582581740930578, -14.20153314710789871 ) ) ;
#29202 = CARTESIAN_POINT ( 'NONE',  ( 18.70688454841999970, -48.06418385137889970, -35.14999999999999858 ) ) ;
#29203 = AXIS2_PLACEMENT_3D ( 'NONE', #36459, #16298, #8703 ) ;
#29204 = VECTOR ( 'NONE', #37003, 1000.000000000000000 ) ;
#29205 = CIRCLE ( 'NONE', #32517, 39.00000000000000711 ) ;
#29206 = FACE_OUTER_BOUND ( 'NONE', #42715, .T. ) ;
#29207 = CIRCLE ( 'NONE', #39262, 4.999999999969890752 ) ;
#29209 = ADVANCED_FACE ( 'NONE', ( #37947 ), #10689, .F. ) ;
#29208 = CARTESIAN_POINT ( 'NONE',  ( 22.90091122653545241, -15.61618862529044804, -78.45282272177526295 ) ) ;
#29210 = CARTESIAN_POINT ( 'NONE',  ( 49.09930102447209777, -53.90153221160279884, -55.03246651661279998 ) ) ;
#29211 = CARTESIAN_POINT ( 'NONE',  ( 24.04497561966918440, -15.61618908881887080, -69.50766602643473391 ) ) ;
#29212 = CARTESIAN_POINT ( 'NONE',  ( 59.36844839577301514, -1.819775244482397580, -15.80989836302429730 ) ) ;
#29213 = CARTESIAN_POINT ( 'NONE',  ( 18.32671964139129983, -51.19324711185789312, -74.36773579015570590 ) ) ;
#29214 = ADVANCED_FACE ( 'NONE', ( #34514 ), #30579, .T. ) ;
#29215 = CARTESIAN_POINT ( 'NONE',  ( 16.13393739769620083, -15.61618894467929941, -81.23899999999999011 ) ) ;
#29216 = ORIENTED_EDGE ( 'NONE', *, *, #47575, .F. ) ;
#29217 = CARTESIAN_POINT ( 'NONE',  ( 14.19299298219679883, -8.423176424581528821, -42.48344881935029349 ) ) ;
#29218 = CARTESIAN_POINT ( 'NONE',  ( 64.07736091498190945, 1.409766894666529824, -61.45836428367329773 ) ) ;
#29219 = VERTEX_POINT ( 'NONE', #50520 ) ;
#29220 = CARTESIAN_POINT ( 'NONE',  ( 20.43063756541187814, -15.61618894467929941, -22.14999999999999858 ) ) ;
#29221 = CARTESIAN_POINT ( 'NONE',  ( 60.97736607362909922, -45.52420556272499397, -47.49337238818740303 ) ) ;
#29222 = CARTESIAN_POINT ( 'NONE',  ( 23.32493948456750132, 18.10006093832409491, -34.64999999999999858 ) ) ;
#29223 = DIRECTION ( 'NONE',  ( 0.8204012560548800126, 0.5717882292104090602, 0.000000000000000000 ) ) ;
#29225 = CARTESIAN_POINT ( 'NONE',  ( 16.13393739769620083, -15.61618894467929941, -74.14999999999999147 ) ) ;
#29224 = CARTESIAN_POINT ( 'NONE',  ( 43.63119145555815237, 8.691161901990289707, -68.44539823191810513 ) ) ;
#29226 = DIRECTION ( 'NONE',  ( 0.000000000000000000, -1.000000000000000000, 0.000000000000000000 ) ) ;
#29227 = CARTESIAN_POINT ( 'NONE',  ( 87.61621807841599718, -48.61618894467930119, -61.12885639714370001 ) ) ;
#29228 = EDGE_LOOP ( 'NONE', ( #27310, #14362, #1575, #25143 ) ) ;
#29229 = EDGE_LOOP ( 'NONE', ( #18351, #45447, #29797, #29782 ) ) ;
#29230 = ORIENTED_EDGE ( 'NONE', *, *, #23796, .T. ) ;
#29231 = ORIENTED_EDGE ( 'NONE', *, *, #23527, .F. ) ;
#29232 = CARTESIAN_POINT ( 'NONE',  ( 61.61695481319249978, -45.18470336428949707, -46.90708922469920594 ) ) ;
#29233 = CARTESIAN_POINT ( 'NONE',  ( -3.839728563314020349, -6.393788602144800493, -54.64999999999999858 ) ) ;
#29234 = CARTESIAN_POINT ( 'NONE',  ( 53.82348698186820002, -51.68201745328180152, -53.31677710839019824 ) ) ;
#29235 = ORIENTED_EDGE ( 'NONE', *, *, #21227, .T. ) ;
#29236 = ORIENTED_EDGE ( 'NONE', *, *, #131, .F. ) ;
#29237 = CYLINDRICAL_SURFACE ( 'NONE', #22506, 1.000000000000001332 ) ;
#29238 = VERTEX_POINT ( 'NONE', #45815 ) ;
#29239 = CARTESIAN_POINT ( 'NONE',  ( 8.222940294821349028, -15.07895016470535943, -76.52928890672468754 ) ) ;
#29240 = CARTESIAN_POINT ( 'NONE',  ( -11.60499810224809103, 11.81104071652318410, -45.20979172290213199 ) ) ;
#29241 = FACE_OUTER_BOUND ( 'NONE', #7384, .T. ) ;
#29242 = CARTESIAN_POINT ( 'NONE',  ( 8.815605938724019097, -63.28267558148569094, -46.67186391142220003 ) ) ;
#29243 = CARTESIAN_POINT ( 'NONE',  ( 16.13393739769620083, -29.47259540523037202, -35.01561944896766221 ) ) ;
#29244 = AXIS2_PLACEMENT_3D ( 'NONE', #2532, #34483, #50489 ) ;
#29245 = AXIS2_PLACEMENT_3D ( 'NONE', #38035, #2382, #13928 ) ;
#29246 = ORIENTED_EDGE ( 'NONE', *, *, #15270, .T. ) ;
#29247 = DIRECTION ( 'NONE',  ( 0.000000000000000000, -0.7071067811865492381, 0.7071067811865457964 ) ) ;
#29248 = CARTESIAN_POINT ( 'NONE',  ( 53.75480394220020486, -50.98814891280600392, -75.91868723642510020 ) ) ;
#29249 = CARTESIAN_POINT ( 'NONE',  ( 19.11395969596977906, -21.71459350761253759, -46.80819746545874693 ) ) ;
#29250 = CIRCLE ( 'NONE', #8347, 0.5000000000000004441 ) ;
#29251 = CARTESIAN_POINT ( 'NONE',  ( 47.55940288235914437, -54.56982865077419120, -55.06178236366046974 ) ) ;
#29252 = CIRCLE ( 'NONE', #35170, 2.999999999999999112 ) ;
#29253 = VECTOR ( 'NONE', #50123, 1000.000000000000000 ) ;
#29254 = CARTESIAN_POINT ( 'NONE',  ( 8.601692148444030295, -17.81892113373459807, -62.92193303376410540 ) ) ;
#29255 = DIRECTION ( 'NONE',  ( 0.000000000000000000, 0.000000000000000000, -1.000000000000000000 ) ) ;
#29256 = CARTESIAN_POINT ( 'NONE',  ( 41.86538216647980448, 13.73410068919089966, -5.828812016449009370 ) ) ;
#29257 = EDGE_CURVE ( 'NONE', #27765, #5705, #21384, .T. ) ;
#29258 = CARTESIAN_POINT ( 'NONE',  ( 43.27773194996530037, -42.90569250231440179, -4.515873930613719445 ) ) ;
#29259 = CARTESIAN_POINT ( 'NONE',  ( 72.94555459751978788, 0.9254890127240629205, -62.06507410682309711 ) ) ;
#29261 = EDGE_CURVE ( 'NONE', #49525, #11148, #34779, .T. ) ;
#29260 = CARTESIAN_POINT ( 'NONE',  ( 61.15824941542350501, -45.61002793583419646, -47.69140330884709300 ) ) ;
#29262 = CARTESIAN_POINT ( 'NONE',  ( 64.27186769037609793, 1.261434405545410087, -70.14834382225429010 ) ) ;
#29263 = LINE ( 'NONE', #42365, #21784 ) ;
#29264 = CARTESIAN_POINT ( 'NONE',  ( 65.46220881590400609, 1.315651889596580082, -18.25468295616219905 ) ) ;
#29265 = EDGE_LOOP ( 'NONE', ( #42398, #7280, #29445, #22729 ) ) ;
#29266 = CARTESIAN_POINT ( 'NONE',  ( 14.47068264623949929, -51.84692819978400280, -75.69083100613939052 ) ) ;
#29267 = CARTESIAN_POINT ( 'NONE',  ( 47.18324198357289845, -54.80726809202429450, -54.61058319554170026 ) ) ;
#29268 = CARTESIAN_POINT ( 'NONE',  ( 63.78749078828948882, 1.530257664727401767, -65.65000000000000568 ) ) ;
#29269 = DIRECTION ( 'NONE',  ( 0.000000000000000000, 0.000000000000000000, 1.000000000000000000 ) ) ;
#29270 = EDGE_CURVE ( 'NONE', #13277, #45223, #24219, .T. ) ;
#29271 = CARTESIAN_POINT ( 'NONE',  ( 23.31866335234750309, -17.53501162367199839, -32.14999999999999858 ) ) ;
#29272 = CARTESIAN_POINT ( 'NONE',  ( 54.62220045163225279, -46.21585040664924549, -15.85440674217626977 ) ) ;
#29273 = CARTESIAN_POINT ( 'NONE',  ( 47.79868757135139390, -54.43094906366430052, -54.82870257381310353 ) ) ;
#29275 = DIRECTION ( 'NONE',  ( -0.3294064756442134922, -0.9441882088882800339, 8.551492847173809175E-14 ) ) ;
#29274 = CARTESIAN_POINT ( 'NONE',  ( -18.86606260230390220, 24.88381105532059934, 14.21249999999999858 ) ) ;
#29276 = CARTESIAN_POINT ( 'NONE',  ( 19.37546814487692615, -55.48492500472980993, -75.71737149041572934 ) ) ;
#29277 = DIRECTION ( 'NONE',  ( -0.5109955813515499878, -0.8595833385072046973, 0.000000000000000000 ) ) ;
#29278 = EDGE_CURVE ( 'NONE', #17140, #22022, #43027, .T. ) ;
#29279 = CARTESIAN_POINT ( 'NONE',  ( 48.76292579026059570, 22.72389827073419966, -54.68972791661200006 ) ) ;
#29280 = CIRCLE ( 'NONE', #30145, 2.000000000000001776 ) ;
#29281 = VERTEX_POINT ( 'NONE', #30320 ) ;
#29282 = CARTESIAN_POINT ( 'NONE',  ( 15.52768592298719952, -22.64292490982440142, -59.37457502644110008 ) ) ;
#29283 = VERTEX_POINT ( 'NONE', #22453 ) ;
#29284 = VECTOR ( 'NONE', #22909, 1000.000000000000000 ) ;
#29285 = CARTESIAN_POINT ( 'NONE',  ( 12.36320305029179956, 33.31445045633500257, -15.76422791923680045 ) ) ;
#29286 = CARTESIAN_POINT ( 'NONE',  ( 53.59003930803689997, -49.40628012469949937, -49.22510501142529904 ) ) ;
#29287 = CARTESIAN_POINT ( 'NONE',  ( 15.24821661813249030, -22.38319830166902946, -42.99448661903509361 ) ) ;
#29289 = CARTESIAN_POINT ( 'NONE',  ( 55.45527622853430216, 15.26954464707670134, -25.53657833487140394 ) ) ;
#29288 = CARTESIAN_POINT ( 'NONE',  ( 82.81544245083719602, 14.09548530567630031, -47.32222464724239330 ) ) ;
#29290 = CARTESIAN_POINT ( 'NONE',  ( 16.27092104377510040, -22.66769900829920203, -64.94663746033859297 ) ) ;
#29291 = CARTESIAN_POINT ( 'NONE',  ( 9.183937397696297467, -15.61618894467929941, -20.75000000000000711 ) ) ;
#29292 = DIRECTION ( 'NONE',  ( 1.000000000000000000, 0.000000000000000000, 0.000000000000000000 ) ) ;
#29293 = B_SPLINE_SURFACE_WITH_KNOTS ( 'NONE', 3, 3, ( 
 ( #40479, #32845, #1428, #37579, #1685, #12980 ),
 ( #33642, #4570, #20542, #21068, #1166, #24726 ),
 ( #36537, #17163, #641, #20807, #16628, #48612 ),
 ( #12715, #36798, #33114, #2727, #45714, #29959 ),
 ( #42303, #14259, #26550, #30484, #1947, #2206 ),
 ( #6402, #18438, #5877, #22100, #42566, #34934 ),
 ( #50935, #45977, #42040, #38365, #6658, #22618 ),
 ( #34149, #18183, #30228, #38635, #26814, #21845 ),
 ( #18698, #41774, #34676, #37851, #33896, #46246 ),
 ( #10069, #50676, #14774, #30743, #46765, #46505 ),
 ( #14515, #10852, #42828, #26031, #25767, #6921 ),
 ( #17925, #22874, #22361, #10333, #26294, #2982 ),
 ( #38894, #50162, #2458, #49907, #18956, #6141 ),
 ( #15031, #9815, #14000, #38109, #34415, #50426 ) ),
 .UNSPECIFIED., .F., .F., .F.,
 ( 4, 2, 2, 2, 2, 2, 4 ),
 ( 4, 1, 1, 4 ),
 ( 11.91694619464080063, 18.73771508486100146, 24.98362011314799958, 28.10657262729149863, 33.10329664992109855, 41.09805508612850389, 46.81668623818470110 ),
 ( -4.801081116000000185E-06, 0.3333333333333329818, 0.6666666666666670737, 1.000005332741559894 ),
 .UNSPECIFIED. ) ;
#29294 = DIRECTION ( 'NONE',  ( 0.000000000000000000, 0.000000000000000000, -1.000000000000000000 ) ) ;
#29295 = VERTEX_POINT ( 'NONE', #50002 ) ;
#29296 = ORIENTED_EDGE ( 'NONE', *, *, #30553, .F. ) ;
#29297 = CARTESIAN_POINT ( 'NONE',  ( 11.85902006004669929, -65.16986276887600127, -16.73665430629710116 ) ) ;
#29298 = CARTESIAN_POINT ( 'NONE',  ( 12.03830950846760039, 34.00854491475119801, -46.58869671456609751 ) ) ;
#29299 = CARTESIAN_POINT ( 'NONE',  ( 9.728155433668721486, -10.93576152856158856, -38.70851398578017921 ) ) ;
#29300 = DIRECTION ( 'NONE',  ( 0.000000000000000000, 0.7071067811865475727, 0.7071067811865475727 ) ) ;
#29301 = CARTESIAN_POINT ( 'NONE',  ( 11.09843493734689979, -65.15652262471280665, -47.26083285670119949 ) ) ;
#29302 = ORIENTED_EDGE ( 'NONE', *, *, #43773, .F. ) ;
#29303 = CARTESIAN_POINT ( 'NONE',  ( 0.8105618841727830759, -51.44517397597059727, -34.28607352350360316 ) ) ;
#29304 = CARTESIAN_POINT ( 'NONE',  ( 16.13393739769620083, -15.61618894467919816, -82.14319696191608955 ) ) ;
#29305 = CARTESIAN_POINT ( 'NONE',  ( 68.13393739769618662, -0.3411889446793609504, -65.65000000000000568 ) ) ;
#29306 = CARTESIAN_POINT ( 'NONE',  ( 52.26132335211670465, 19.59060111016600203, -50.93306148729159588 ) ) ;
#29307 = CARTESIAN_POINT ( 'NONE',  ( 70.99050876911339003, 1.383811055320669947, -70.34999999999999432 ) ) ;
#29308 = CARTESIAN_POINT ( 'NONE',  ( 50.03007021624649298, -48.76508975269899793, -76.14999999999999147 ) ) ;
#29309 = DIRECTION ( 'NONE',  ( -1.000000000000000000, 0.000000000000000000, 0.000000000000000000 ) ) ;
#29310 = ORIENTED_EDGE ( 'NONE', *, *, #25860, .F. ) ;
#29311 = CARTESIAN_POINT ( 'NONE',  ( 53.95391475063919984, -48.32190372696410208, -26.18290555829399935 ) ) ;
#29312 = CARTESIAN_POINT ( 'NONE',  ( 68.13393739769810509, 19.38381105532030091, -71.50000000000198952 ) ) ;
#29313 = VERTEX_POINT ( 'NONE', #6762 ) ;
#29314 = CARTESIAN_POINT ( 'NONE',  ( 23.83903434524771470, -13.54549697515503759, -53.70900105890960674 ) ) ;
#29315 = DIRECTION ( 'NONE',  ( 0.000000000000000000, 0.000000000000000000, -1.000000000000000000 ) ) ;
#29316 = CARTESIAN_POINT ( 'NONE',  ( 23.70552850492139996, -13.55275599941940001, -33.92780426447939846 ) ) ;
#29317 = CARTESIAN_POINT ( 'NONE',  ( 13.99027006517380123, -51.18075678683580776, -22.90513384373820216 ) ) ;
#29318 = CARTESIAN_POINT ( 'NONE',  ( 54.58684629315739301, 19.57352726647010144, -75.90306255601998942 ) ) ;
#29319 = EDGE_CURVE ( 'NONE', #51110, #34913, #38461, .T. ) ;
#29320 = CARTESIAN_POINT ( 'NONE',  ( 47.34252490452630724, -54.36320411571839628, -75.17211772295890171 ) ) ;
#29321 = VERTEX_POINT ( 'NONE', #49747 ) ;
#29322 = AXIS2_PLACEMENT_3D ( 'NONE', #23942, #4058, #36531 ) ;
#29323 = CARTESIAN_POINT ( 'NONE',  ( 55.94863681995290250, 14.49335208508280104, -17.16538366520289927 ) ) ;
#29324 = EDGE_CURVE ( 'NONE', #33273, #33944, #33734, .T. ) ;
#29325 = VECTOR ( 'NONE', #13050, 1000.000000000000000 ) ;
#29326 =( BOUNDED_CURVE ( )  B_SPLINE_CURVE ( 2, ( #28114, #24687, #40701, #18147, #37542 ),
 .UNSPECIFIED., .F., .T. ) 
 B_SPLINE_CURVE_WITH_KNOTS ( ( 3, 2, 3 ),
 ( -0.003205554297748039981, 0.8238407534185530068, 1.650887061134849843 ),
 .UNSPECIFIED. ) 
 CURVE ( )  GEOMETRIC_REPRESENTATION_ITEM ( )  RATIONAL_B_SPLINE_CURVE ( ( 1.000000000000000000, 0.9157107718030679244, 1.000000000000000000, 0.9157107718030469412, 1.000000000000000000 ) ) 
 REPRESENTATION_ITEM ( '' )  );
#29327 = EDGE_CURVE ( 'NONE', #25231, #41523, #47414, .T. ) ;
#29328 = CARTESIAN_POINT ( 'NONE',  ( 56.93701003825890439, -50.64063337602780024, -53.86363391182649707 ) ) ;
#29329 = TOROIDAL_SURFACE ( 'NONE', #46948, 5.500000000000000000, 0.5000000000000000000 ) ;
#29330 = CARTESIAN_POINT ( 'NONE',  ( 10.16236763787109965, -19.36890979467510121, -37.66858791500939674 ) ) ;
#29331 = CARTESIAN_POINT ( 'NONE',  ( 12.72191543439365979, 34.25104481395036515, -23.44039337806447065 ) ) ;
#29332 = CONICAL_SURFACE ( 'NONE', #20118, 0.2705324999999987323, 1.029744258676660307 ) ;
#29333 = ADVANCED_FACE ( 'NONE', ( #46083 ), #50778, .T. ) ;
#29334 = CARTESIAN_POINT ( 'NONE',  ( 46.98721080798319605, 22.60815134751159761, -75.82248416561151316 ) ) ;
#29335 = CARTESIAN_POINT ( 'NONE',  ( 64.99878011502339348, 1.099973129953850215, -60.58645605602389850 ) ) ;
#29336 = CARTESIAN_POINT ( 'NONE',  ( 41.42082069171990355, -45.63313572307169608, -6.346463263985820724 ) ) ;
#29337 = CARTESIAN_POINT ( 'NONE',  ( 16.13393739769620083, -15.61618894467929941, -84.65000000000000568 ) ) ;
#29338 = CARTESIAN_POINT ( 'NONE',  ( 13.60966998086417590, -49.61618894467943619, -83.09320499168605068 ) ) ;
#29339 = DIRECTION ( 'NONE',  ( 0.000000000000000000, 0.000000000000000000, -1.000000000000000000 ) ) ;
#29341 = CARTESIAN_POINT ( 'NONE',  ( 44.97440182180130108, -40.14835006695389552, -61.45165435098494555 ) ) ;
#29340 = CARTESIAN_POINT ( 'NONE',  ( 64.66447934098370354, 0.9065823421260940096, -60.75474143511929981 ) ) ;
#29342 = CARTESIAN_POINT ( 'NONE',  ( 61.34010671551649807, 13.97110126853510081, -46.40635191164569306 ) ) ;
#29343 = EDGE_CURVE ( 'NONE', #40171, #32200, #30054, .T. ) ;
#29344 = CARTESIAN_POINT ( 'NONE',  ( -29.08731580419370033, -35.60745549472860461, -55.16774717297709429 ) ) ;
#29345 = ORIENTED_EDGE ( 'NONE', *, *, #18189, .T. ) ;
#29346 = CARTESIAN_POINT ( 'NONE',  ( 53.10940566897379966, -49.51509250019670105, -48.84491346710589710 ) ) ;
#29347 = CARTESIAN_POINT ( 'NONE',  ( 57.49269918002690360, -45.11614594041920157, -25.40091178144869843 ) ) ;
#29348 = CARTESIAN_POINT ( 'NONE',  ( 49.24754892657740157, -53.85074344983969752, -55.23177050136099808 ) ) ;
#29349 = CARTESIAN_POINT ( 'NONE',  ( 56.04577029392780219, 14.63406453562459930, -25.72783580284800209 ) ) ;
#29350 = CARTESIAN_POINT ( 'NONE',  ( 9.933815087369589847, -19.74726581762220334, -81.04557435679309663 ) ) ;
#29351 = CARTESIAN_POINT ( 'NONE',  ( 50.31596464670999325, 18.73470065217860281, -76.14999999999999147 ) ) ;
#29352 = CARTESIAN_POINT ( 'NONE',  ( 52.76604400197739864, 18.47565711339310113, -48.76247536867809629 ) ) ;
#29353 = CARTESIAN_POINT ( 'NONE',  ( 71.45393474093620512, 0.9259537755896120048, -70.64777040355440363 ) ) ;
#29354 = CARTESIAN_POINT ( 'NONE',  ( 60.54711305708200086, -45.61758103184519797, -47.15425142490470023 ) ) ;
#29355 = CARTESIAN_POINT ( 'NONE',  ( 46.35275103504439898, 21.67755452994670406, -76.14999999999999147 ) ) ;
#29356 = EDGE_LOOP ( 'NONE', ( #9295, #46101, #4755, #29524 ) ) ;
#29357 = CARTESIAN_POINT ( 'NONE',  ( 9.075377375428610449, -13.23219549871780032, -74.17102124479808367 ) ) ;
#29358 = CARTESIAN_POINT ( 'NONE',  ( 73.12814476249489815, 0.9958340104639701318, -68.96201750760249638 ) ) ;
#29359 = CARTESIAN_POINT ( 'NONE',  ( 47.42186964816270489, -54.64465214730000042, -54.90471645379279408 ) ) ;
#29360 = CARTESIAN_POINT ( 'NONE',  ( 24.04493006531424726, -15.60506294570754982, -49.79188297642375005 ) ) ;
#29361 = CARTESIAN_POINT ( 'NONE',  ( 72.85934862407960111, 1.383411777981069957, -62.75344103383148564 ) ) ;
#29362 = VECTOR ( 'NONE', #8667, 1000.000000000000000 ) ;
#29363 = CARTESIAN_POINT ( 'NONE',  ( 60.18629601137560314, 14.85053287620760010, -47.96423632185339869 ) ) ;
#29364 = CARTESIAN_POINT ( 'NONE',  ( 52.83531650484950148, 18.42562942600509857, -48.55819829956829636 ) ) ;
#29365 = CARTESIAN_POINT ( 'NONE',  ( 2.488944341170570063, -25.50650633542909773, -34.70985242058479514 ) ) ;
#29366 = CARTESIAN_POINT ( 'NONE',  ( 71.87288967509290671, 1.328802495349950208, -61.13208180354720156 ) ) ;
#29367 = AXIS2_PLACEMENT_3D ( 'NONE', #46909, #6807, #14915 ) ;
#29368 = EDGE_CURVE ( 'NONE', #22408, #17966, #50732, .T. ) ;
#29369 = AXIS2_PLACEMENT_3D ( 'NONE', #31114, #47394, #43199 ) ;
#29370 = DIRECTION ( 'NONE',  ( 1.000000000000000000, 0.000000000000000000, 0.000000000000000000 ) ) ;
#29371 = ORIENTED_EDGE ( 'NONE', *, *, #51140, .T. ) ;
#29372 = CARTESIAN_POINT ( 'NONE',  ( 64.80222656955079685, 0.9966178393190270324, -70.63122704464430512 ) ) ;
#29373 = ORIENTED_EDGE ( 'NONE', *, *, #36551, .F. ) ;
#29374 = CARTESIAN_POINT ( 'NONE',  ( 9.296350058830100238, -63.27348387625509929, -46.53013307742669724 ) ) ;
#29375 = FACE_OUTER_BOUND ( 'NONE', #12122, .T. ) ;
#29376 = ORIENTED_EDGE ( 'NONE', *, *, #3179, .T. ) ;
#29377 = DIRECTION ( 'NONE',  ( 0.000000000000000000, 0.000000000000000000, 1.000000000000000000 ) ) ;
#29378 = CARTESIAN_POINT ( 'NONE',  ( 84.13393739769618662, -1.166188944679350081, -65.65000000000000568 ) ) ;
#29379 = CARTESIAN_POINT ( 'NONE',  ( 22.90065299155850198, -15.61618013372109637, -50.45281880338879432 ) ) ;
#29380 = CARTESIAN_POINT ( 'NONE',  ( 52.90771571177940302, 19.45349931027849877, -76.48668076088111434 ) ) ;
#29381 = ORIENTED_EDGE ( 'NONE', *, *, #51305, .F. ) ;
#29382 = CARTESIAN_POINT ( 'NONE',  ( 16.13393739769609780, -15.61618894467929941, 7.919999999999999929 ) ) ;
#29383 = CARTESIAN_POINT ( 'NONE',  ( 13.13393739769600010, 18.38381105532060289, -35.14999999999999858 ) ) ;
#29384 = CYLINDRICAL_SURFACE ( 'NONE', #45432, 1.000000000000000888 ) ;
#29385 = CARTESIAN_POINT ( 'NONE',  ( 24.22405364513110015, -14.02473075832179994, -55.73050419751459827 ) ) ;
#29386 = B_SPLINE_CURVE_WITH_KNOTS ( 'NONE', 3,
 ( #6757, #42136, #19049, #6235, #35024, #22711, #26125, #22191, #34511, #38201, #18270, #50775, #14865, #40007, #31859, #28187 ),
 .UNSPECIFIED., .F., .F.,
 ( 4, 2, 2, 2, 2, 2, 2, 4 ),
 ( -1.892930000000000094E-14, 0.07319275283554899092, 0.1391693187718359981, 0.1804046724820149994, 0.2061767685508769932, 0.2577209606886010085, 0.3401916681089590111, 0.4123535371017730267 ),
 .UNSPECIFIED. ) ;
#29387 = CYLINDRICAL_SURFACE ( 'NONE', #356, 3.000000000000000444 ) ;
#29388 = CARTESIAN_POINT ( 'NONE',  ( 42.97889992224431666, -37.77457641634045160, -75.42518632368958720 ) ) ;
#29389 = VERTEX_POINT ( 'NONE', #33987 ) ;
#29390 = EDGE_CURVE ( 'NONE', #29313, #3712, #29795, .T. ) ;
#29391 = CARTESIAN_POINT ( 'NONE',  ( 56.55820758832960138, -46.20897426240800598, -26.26650421730799678 ) ) ;
#29392 = CARTESIAN_POINT ( 'NONE',  ( 23.19678285945379770, -13.24492181749289976, -44.12955248114639772 ) ) ;
#29393 = CARTESIAN_POINT ( 'NONE',  ( 52.63953642234350383, -49.80174121720269653, -48.69586908824970095 ) ) ;
#29394 = CARTESIAN_POINT ( 'NONE',  ( 23.04644940922143093, -11.63203671537942974, -33.34099856603324952 ) ) ;
#29395 = EDGE_CURVE ( 'NONE', #40267, #51110, #3861, .T. ) ;
#29396 = CARTESIAN_POINT ( 'NONE',  ( 13.87643720199350028, 20.51618323985760028, -75.32473453343510528 ) ) ;
#29397 = CARTESIAN_POINT ( 'NONE',  ( 16.13393739769620083, -15.61618894467929941, -32.14999999999999858 ) ) ;
#29398 = AXIS2_PLACEMENT_3D ( 'NONE', #29786, #5969, #38195 ) ;
#29399 = CIRCLE ( 'NONE', #43640, 5.500000000000005329 ) ;
#29400 = LINE ( 'NONE', #36477, #30620 ) ;
#29401 = VECTOR ( 'NONE', #15652, 1000.000000000000000 ) ;
#29402 = CARTESIAN_POINT ( 'NONE',  ( 24.37674430018200056, -15.41907203188980091, -57.50005794035820372 ) ) ;
#29403 = ORIENTED_EDGE ( 'NONE', *, *, #28294, .F. ) ;
#29404 = CARTESIAN_POINT ( 'NONE',  ( 52.61201418140420571, -49.81418459234139817, -28.15000000000000213 ) ) ;
#29405 = CARTESIAN_POINT ( 'NONE',  ( 16.58032161480830169, -51.11619067739219702, -20.45514663783470155 ) ) ;
#29406 = CARTESIAN_POINT ( 'NONE',  ( 10.35837886327420065, 33.32232037452499895, -17.68810962647529905 ) ) ;
#29407 = DIRECTION ( 'NONE',  ( -0.2260571801428130634, -5.828670879282072626E-15, 0.9741140340359951688 ) ) ;
#29408 = DIRECTION ( 'NONE',  ( 1.000000000000000000, 0.000000000000000000, 0.000000000000000000 ) ) ;
#29409 = ORIENTED_EDGE ( 'NONE', *, *, #46100, .T. ) ;
#29410 = CARTESIAN_POINT ( 'NONE',  ( -11.32734370190460105, -41.88171845330919751, -6.430192534648670133 ) ) ;
#29411 = CARTESIAN_POINT ( 'NONE',  ( 47.43185934795429404, 23.40577861522420022, -54.84779215339789715 ) ) ;
#29412 = CARTESIAN_POINT ( 'NONE',  ( 63.32276749867028798, 1.263823323415670163, -62.32316323322979912 ) ) ;
#29413 = CARTESIAN_POINT ( 'NONE',  ( 57.32763708541499881, -50.39928489432909942, -53.00790317329960288 ) ) ;
#29414 = CARTESIAN_POINT ( 'NONE',  ( 11.44080308043550076, 34.06382446123569707, -17.48917067575129991 ) ) ;
#29415 = CARTESIAN_POINT ( 'NONE',  ( 16.13393739769620083, -15.61618894467929941, -81.23899999999999011 ) ) ;
#29416 = CYLINDRICAL_SURFACE ( 'NONE', #13377, 0.4999999999999982236 ) ;
#29417 = CARTESIAN_POINT ( 'NONE',  ( 8.784728771177219286, 31.88305279678909443, -46.67204636144870022 ) ) ;
#29418 = CARTESIAN_POINT ( 'NONE',  ( 53.59007319635580302, -49.40623578145689976, -49.22505640097240587 ) ) ;
#29419 = PLANE ( 'NONE',  #3880 ) ;
#29420 = CARTESIAN_POINT ( 'NONE',  ( 52.93160674638770047, 21.02777951207980323, -54.03607036502950223 ) ) ;
#29421 = CARTESIAN_POINT ( 'NONE',  ( 63.56282646728049457, 1.400446387219270061, -68.89724194849250694 ) ) ;
#29422 = CARTESIAN_POINT ( 'NONE',  ( 14.36273799164256815, -9.025303278630660841, -47.86948771557721471 ) ) ;
#29423 = VERTEX_POINT ( 'NONE', #19571 ) ;
#29424 = FACE_OUTER_BOUND ( 'NONE', #21675, .T. ) ;
#29425 = CARTESIAN_POINT ( 'NONE',  ( 9.733202698440479139, 31.94412001969340054, -46.29921928092249317 ) ) ;
#29426 = CARTESIAN_POINT ( 'NONE',  ( 43.87445613097960262, 13.83391143939489965, -6.621204841358950155 ) ) ;
#29427 = ADVANCED_FACE ( 'NONE', ( #31090 ), #25595, .T. ) ;
#29428 = CARTESIAN_POINT ( 'NONE',  ( 66.37091707294710830, -30.63654346061790079, -16.96663971210719879 ) ) ;
#29429 = CARTESIAN_POINT ( 'NONE',  ( 18.50147319020889825, 20.38774172224130155, -75.08736963500949457 ) ) ;
#29430 = EDGE_LOOP ( 'NONE', ( #16038, #379, #43319, #33867 ) ) ;
#29431 = EDGE_CURVE ( 'NONE', #43147, #32833, #36675, .T. ) ;
#29432 = EDGE_LOOP ( 'NONE', ( #46179, #40398, #13693, #14094, #26401, #15694 ) ) ;
#29433 = LINE ( 'NONE', #49889, #19487 ) ;
#29434 = ORIENTED_EDGE ( 'NONE', *, *, #34150, .F. ) ;
#29435 = CARTESIAN_POINT ( 'NONE',  ( 11.71313963123279933, -65.09861111722139526, -46.54370187508719425 ) ) ;
#29436 = CARTESIAN_POINT ( 'NONE',  ( 57.06654200124710030, -45.67870534195919419, -26.17304345835309931 ) ) ;
#29437 = CARTESIAN_POINT ( 'NONE',  ( 24.04493712615994028, -15.61869300327582977, -77.50777460550092712 ) ) ;
#29438 = EDGE_CURVE ( 'NONE', #36069, #26276, #43220, .T. ) ;
#29439 = CARTESIAN_POINT ( 'NONE',  ( 16.13393739769620083, -15.61618894467929941, -32.14999999999999858 ) ) ;
#29440 = CARTESIAN_POINT ( 'NONE',  ( 61.73008982643180076, 13.88381104171409852, -46.37201266034419689 ) ) ;
#29441 = DIRECTION ( 'NONE',  ( -1.000000000000000000, 0.000000000000000000, 0.000000000000000000 ) ) ;
#29442 = ORIENTED_EDGE ( 'NONE', *, *, #17154, .F. ) ;
#29443 = VECTOR ( 'NONE', #44148, 1000.000000000000114 ) ;
#29444 = CARTESIAN_POINT ( 'NONE',  ( 75.04939620295748171, -15.61618894467929941, -11.30491871076499955 ) ) ;
#29445 = ORIENTED_EDGE ( 'NONE', *, *, #38949, .F. ) ;
#29446 = CARTESIAN_POINT ( 'NONE',  ( 54.17850344129180229, -45.61389549855280023, -15.02769642854620002 ) ) ;
#29447 = CARTESIAN_POINT ( 'NONE',  ( 9.582536624350547427, -20.09909968766171318, -34.60122671728029786 ) ) ;
#29448 = CARTESIAN_POINT ( 'NONE',  ( 9.367479025678566273, -16.58895892350905399, -49.80140833476744433 ) ) ;
#29449 = ORIENTED_EDGE ( 'NONE', *, *, #45844, .T. ) ;
#29450 = DIRECTION ( 'NONE',  ( 0.4145156864928219997, -0.9100421669633689259, 0.000000000000000000 ) ) ;
#29451 = CARTESIAN_POINT ( 'NONE',  ( 46.81364246026949871, -53.87014086992079598, -75.86283294038038605 ) ) ;
#29452 = DIRECTION ( 'NONE',  ( 0.000000000000000000, 0.000000000000000000, 1.000000000000000000 ) ) ;
#29453 = EDGE_CURVE ( 'NONE', #49316, #38190, #31862, .T. ) ;
#29454 = CARTESIAN_POINT ( 'NONE',  ( 50.78057069950819624, 14.75089828130050051, -12.88396743804300115 ) ) ;
#29455 = CARTESIAN_POINT ( 'NONE',  ( 19.53299567489768407, -55.47150705052180086, -75.56421958049284626 ) ) ;
#29456 = CARTESIAN_POINT ( 'NONE',  ( 41.64265090550289727, 15.19461330350370076, -4.296538310234210734 ) ) ;
#29457 = PRODUCT_DEFINITION_SHAPE ( 'NONE', 'NONE',  #51877 ) ;
#29458 = CARTESIAN_POINT ( 'NONE',  ( 11.11660069372041804, -63.29819265419726548, -14.66254990259057855 ) ) ;
#29459 = CARTESIAN_POINT ( 'NONE',  ( 57.45421615888909628, 13.89859616986070101, -25.53723535916439857 ) ) ;
#29460 = CARTESIAN_POINT ( 'NONE',  ( 10.79995697763059859, -9.859853212502130759, -74.54962200957619700 ) ) ;
#29461 = EDGE_LOOP ( 'NONE', ( #22715, #10058, #30654, #25092, #45787 ) ) ;
#29462 = DIRECTION ( 'NONE',  ( 1.000000000000000000, 0.000000000000000000, 0.000000000000000000 ) ) ;
#29463 = DIRECTION ( 'NONE',  ( 0.000000000000000000, 0.000000000000000000, 1.000000000000000000 ) ) ;
#29464 = CARTESIAN_POINT ( 'NONE',  ( 15.67962062535580081, -50.86266781815560023, -15.65622421709140077 ) ) ;
#29465 = CARTESIAN_POINT ( 'NONE',  ( 72.68863061175819951, 1.254613999359699861, -69.43746191119949174 ) ) ;
#29466 = AXIS2_PLACEMENT_3D ( 'NONE', #13989, #21568, #38093 ) ;
#29467 =( BOUNDED_CURVE ( )  B_SPLINE_CURVE ( 3, ( #25212, #17120, #48309, #4278 ),
 .UNSPECIFIED., .F., .T. ) 
 B_SPLINE_CURVE_WITH_KNOTS ( ( 4, 4 ),
 ( 2.356194490192353719, 3.141592653589795781 ),
 .UNSPECIFIED. ) 
 CURVE ( )  GEOMETRIC_REPRESENTATION_ITEM ( )  RATIONAL_B_SPLINE_CURVE ( ( 1.000000000000000000, 0.9492530216741918991, 0.9492530216741918991, 1.000000000000000000 ) ) 
 REPRESENTATION_ITEM ( '' )  );
#29468 = CARTESIAN_POINT ( 'NONE',  ( 11.74347662706570006, -64.88511784619510081, -16.31133514117630057 ) ) ;
#29469 = DIRECTION ( 'NONE',  ( -0.3535533905932738974, 0.6123724356957941373, 0.7071067811865477948 ) ) ;
#29470 = DIRECTION ( 'NONE',  ( 0.000000000000000000, 0.000000000000000000, -1.000000000000000000 ) ) ;
#29471 = CARTESIAN_POINT ( 'NONE',  ( 48.92567656525680064, -53.97674872320250472, -55.07030108398770096 ) ) ;
#29472 = B_SPLINE_CURVE_WITH_KNOTS ( 'NONE', 3,
 ( #40285, #4897, #8578, #5172, #4376, #41312, #48405, #965, #8835, #32645, #20865, #12504 ),
 .UNSPECIFIED., .F., .F.,
 ( 4, 2, 2, 2, 2, 4 ),
 ( 0.000000000000000000, 0.1250000000000001110, 0.2500000000000002220, 0.5000000000000001110, 0.7500000000000001110, 1.000000000000000000 ),
 .UNSPECIFIED. ) ;
#29473 = CARTESIAN_POINT ( 'NONE',  ( 24.04466642925503095, -15.61618863334376250, -55.79233649161735542 ) ) ;
#29474 = CARTESIAN_POINT ( 'NONE',  ( 16.13393739769620083, -15.61618894467929941, -643.2998782751060389 ) ) ;
#29475 = CARTESIAN_POINT ( 'NONE',  ( 18.66237388361239624, -51.43165038652999499, -74.14992922886710858 ) ) ;
#29476 = DIRECTION ( 'NONE',  ( 0.000000000000000000, 0.000000000000000000, -1.000000000000000000 ) ) ;
#29477 = VERTEX_POINT ( 'NONE', #26914 ) ;
#29478 = CARTESIAN_POINT ( 'NONE',  ( 16.94034526300609755, -23.02269964089170173, -41.53282164658679676 ) ) ;
#29479 = B_SPLINE_CURVE_WITH_KNOTS ( 'NONE', 3,
 ( #51677, #16282, #23606, #11595, #24375, #36443, #19443, #31725, #43562, #27300, #48259, #31986, #35936, #56, #40390, #35426, #23861, #47497 ),
 .UNSPECIFIED., .F., .F.,
 ( 4, 2, 2, 2, 2, 2, 2, 2, 4 ),
 ( 0.5000015677398489400, 0.5625013717723678086, 0.6250011758048866772, 0.6875009798374056569, 0.7500007838699245255, 0.8125005879024433941, 0.8750003919349622628, 0.9375001959674811314, 1.000000000000000000 ),
 .UNSPECIFIED. ) ;
#29480 = CARTESIAN_POINT ( 'NONE',  ( 64.06712595014920453, 1.275252243133929930, -61.32327465822529433 ) ) ;
#29481 = VERTEX_POINT ( 'NONE', #3855 ) ;
#29482 = CARTESIAN_POINT ( 'NONE',  ( 11.13393739769619906, 32.24968758154479787, -24.15000000000000213 ) ) ;
#29483 = CARTESIAN_POINT ( 'NONE',  ( 61.13062736222009619, -45.51825399203449507, -47.54701560607519895 ) ) ;
#29484 = CARTESIAN_POINT ( 'NONE',  ( 62.63393739769619373, 21.88381105532059934, 16.35000000000000142 ) ) ;
#29485 = CARTESIAN_POINT ( 'NONE',  ( 12.16981617636350066, 18.81688479155219795, -21.14999999999999858 ) ) ;
#29487 = CARTESIAN_POINT ( 'NONE',  ( 9.840592242581751137, -12.50199903054207695, -53.99366435805588083 ) ) ;
#29486 = CARTESIAN_POINT ( 'NONE',  ( 44.26178562846939002, 8.743315224798376306, -65.39183186454530983 ) ) ;
#29488 = CARTESIAN_POINT ( 'NONE',  ( 71.83393739769618946, 10.88381105532070059, -68.84999999999999432 ) ) ;
#29489 = CARTESIAN_POINT ( 'NONE',  ( 68.13393739769620083, -50.61618894467930119, -73.25000000000000000 ) ) ;
#29490 = VERTEX_POINT ( 'NONE', #47370 ) ;
#29491 = ORIENTED_EDGE ( 'NONE', *, *, #37633, .T. ) ;
#29492 = EDGE_CURVE ( 'NONE', #13640, #51441, #42356, .T. ) ;
#29493 = ORIENTED_EDGE ( 'NONE', *, *, #4832, .T. ) ;
#29494 = EDGE_LOOP ( 'NONE', ( #46879, #37224, #12645, #32020, #34025, #30831 ) ) ;
#29495 = FACE_OUTER_BOUND ( 'NONE', #22413, .T. ) ;
#29496 = EDGE_CURVE ( 'NONE', #27321, #27249, #21052, .T. ) ;
#29497 = CARTESIAN_POINT ( 'NONE',  ( 52.65975762845060615, -49.78933466291119458, -48.73990261843160710 ) ) ;
#29498 = DIRECTION ( 'NONE',  ( 0.000000000000000000, 0.000000000000000000, 1.000000000000000000 ) ) ;
#29499 = CARTESIAN_POINT ( 'NONE',  ( 68.13393739769620083, 1.883811055320649963, -65.65000000000000568 ) ) ;
#29500 = ORIENTED_EDGE ( 'NONE', *, *, #6568, .F. ) ;
#29501 = VERTEX_POINT ( 'NONE', #8035 ) ;
#29502 = ORIENTED_EDGE ( 'NONE', *, *, #51411, .F. ) ;
#29503 = CARTESIAN_POINT ( 'NONE',  ( 22.90093739799785766, -15.62120111656948218, -72.45306145236200734 ) ) ;
#29504 = CARTESIAN_POINT ( 'NONE',  ( -15.55064706627671356, 7.123802962138601202, -48.59731086643836306 ) ) ;
#29505 = CARTESIAN_POINT ( 'NONE',  ( 28.28038400710289935, -8.603434725040973063, -34.79644660940672907 ) ) ;
#29506 = CARTESIAN_POINT ( 'NONE',  ( 1.027904703268269992, 11.45423359053189927, -15.65000000000000036 ) ) ;
#29507 = EDGE_LOOP ( 'NONE', ( #51357, #33973, #27625, #40522 ) ) ;
#29508 = CARTESIAN_POINT ( 'NONE',  ( 16.13393739769620083, -15.61618894467929941, -23.74958330439410048 ) ) ;
#29510 = CARTESIAN_POINT ( 'NONE',  ( 52.96554027761909822, -50.86173948047620286, -76.26079925769791146 ) ) ;
#29509 = AXIS2_PLACEMENT_3D ( 'NONE', #7553, #3621, #15925 ) ;
#29511 = CARTESIAN_POINT ( 'NONE',  ( 14.23931515459916319, -32.51455091268737618, -34.84133294386910507 ) ) ;
#29512 = CARTESIAN_POINT ( 'NONE',  ( 9.337061569587699950, -11.69327847299420142, -61.17911655036439811 ) ) ;
#29513 = EDGE_CURVE ( 'NONE', #38136, #51719, #27936, .T. ) ;
#29514 = CARTESIAN_POINT ( 'NONE',  ( 47.18324198357289845, 23.57489020266570279, -74.14999999999999147 ) ) ;
#29515 = CARTESIAN_POINT ( 'NONE',  ( 41.31713230452019303, 13.54959124757960076, -5.389667122562360468 ) ) ;
#29516 = ADVANCED_FACE ( 'NONE', ( #10950 ), #31344, .T. ) ;
#29517 = CARTESIAN_POINT ( 'NONE',  ( 43.52753934306360151, -43.62935524535279797, -5.023899789736471000 ) ) ;
#29518 = CARTESIAN_POINT ( 'NONE',  ( 28.13393739769620439, -12.40079863550581862, -22.14999999999998792 ) ) ;
#29519 = CARTESIAN_POINT ( 'NONE',  ( 55.91596999402320023, 14.67228162054319895, -25.32543311652580087 ) ) ;
#29520 = CARTESIAN_POINT ( 'NONE',  ( 63.78541443256050059, 1.197079622115780007, -69.74590901733688497 ) ) ;
#29521 = DIRECTION ( 'NONE',  ( -1.000000000000000000, 0.000000000000000000, 0.000000000000000000 ) ) ;
#29522 = CARTESIAN_POINT ( 'NONE',  ( 67.87922885512119819, -0.5138706640943320192, -17.86501260203199948 ) ) ;
#29523 = B_SPLINE_SURFACE_WITH_KNOTS ( 'NONE', 3, 3, ( 
 ( #14936, #23287, #15973, #30901, #47948, #12050, #47441, #46930 ),
 ( #26986, #7088, #3413, #15712, #15463, #39564, #19640, #23039 ),
 ( #47692, #11795, #27756, #43752, #3153, #44259, #20655, #13341 ),
 ( #8367, #24573, #28522, #45042, #32961, #20919, #44008, #32179 ),
 ( #8111, #4684, #36913, #48721, #4944, #40076, #1017, #20145 ),
 ( #44520, #48195, #24315, #40845, #24057, #36136, #16224, #4168 ),
 ( #12824, #17013, #48990, #9142, #13095, #28259, #40334, #32432 ),
 ( #36640, #37179, #29046, #49246, #25097, #239, #41109, #48454 ),
 ( #16741, #12559, #20396, #743, #5220, #32695, #12300, #28782 ) ),
 .UNSPECIFIED., .F., .F., .F.,
 ( 4, 1, 1, 1, 1, 1, 4 ),
 ( 4, 2, 2, 4 ),
 ( -1.933923635888309730E-05, 0.1666666666666670182, 0.3333333333333329818, 0.5000000000000000000, 0.6666666666666670737, 0.8333333333333330373, 1.000023964450169833 ),
 ( -10.25171765628389942, -6.367128310144029690, -2.534746465614240218, -0.1881082593979860051 ),
 .UNSPECIFIED. ) ;
#29524 = ORIENTED_EDGE ( 'NONE', *, *, #36610, .T. ) ;
#29525 = CARTESIAN_POINT ( 'NONE',  ( 13.95043133595810048, -52.17403775882060302, -75.62474771911479365 ) ) ;
#29526 = CIRCLE ( 'NONE', #44609, 2.000000000000002220 ) ;
#29527 = CARTESIAN_POINT ( 'NONE',  ( 47.18324198357289845, -54.80726809202429450, -54.61058319554170026 ) ) ;
#29528 = LINE ( 'NONE', #29268, #35635 ) ;
#29529 = DIRECTION ( 'NONE',  ( 0.000000000000000000, 0.000000000000000000, -1.000000000000000000 ) ) ;
#29530 = CARTESIAN_POINT ( 'NONE',  ( 23.35725391028839937, -17.30451495249259963, -32.14999999999999858 ) ) ;
#29531 = CARTESIAN_POINT ( 'NONE',  ( 13.00893739769619906, -65.51843714052719747, -23.32157302967710422 ) ) ;
#29532 = CARTESIAN_POINT ( 'NONE',  ( 10.85466640526500015, 33.73459223953250330, -17.55961383757770022 ) ) ;
#29533 = CARTESIAN_POINT ( 'NONE',  ( 10.75327222894697776, -9.738703401990544961, -44.77156291098159357 ) ) ;
#29534 = CARTESIAN_POINT ( 'NONE',  ( 8.222924357332910716, -16.65164095223361684, -46.75067280918717216 ) ) ;
#29535 = CARTESIAN_POINT ( 'NONE',  ( 48.36908225894410407, 22.86152331119799896, -54.63163985339289752 ) ) ;
#29536 = ORIENTED_EDGE ( 'NONE', *, *, #20164, .T. ) ;
#29537 = AXIS2_PLACEMENT_3D ( 'NONE', #9395, #20378, #13576 ) ;
#29538 = CARTESIAN_POINT ( 'NONE',  ( 12.34706755911540021, -9.666216171624100184, -60.16676433707719696 ) ) ;
#29539 = AXIS2_PLACEMENT_3D ( 'NONE', #41515, #40740, #44936 ) ;
#29540 = EDGE_LOOP ( 'NONE', ( #17512, #5866, #16945, #7530 ) ) ;
#29541 = CARTESIAN_POINT ( 'NONE',  ( 23.13393739769620083, -2.337132753317950229, -62.14999999999999858 ) ) ;
#29542 = CARTESIAN_POINT ( 'NONE',  ( 19.21265657477752598, -49.46974233527256359, -34.79644660940672907 ) ) ;
#29543 = DIRECTION ( 'NONE',  ( 0.000000000000000000, 0.000000000000000000, 1.000000000000000000 ) ) ;
#29545 = CARTESIAN_POINT ( 'NONE',  ( 52.57331519483629734, 18.62081213560140114, -27.97396291639740085 ) ) ;
#29544 = CARTESIAN_POINT ( 'NONE',  ( 83.51014914612841267, 13.55547819151079914, -46.95038033932869581 ) ) ;
#29546 = CARTESIAN_POINT ( 'NONE',  ( 9.084739283574659652, -15.84282663900890142, -71.44258980755509469 ) ) ;
#29547 = DIRECTION ( 'NONE',  ( 0.000000000000000000, 0.000000000000000000, -1.000000000000000000 ) ) ;
#29548 = CARTESIAN_POINT ( 'NONE',  ( 72.78346131865960444, 1.386342629514219826, -68.66646381051069170 ) ) ;
#29549 = CARTESIAN_POINT ( 'NONE',  ( 0.3209249304026170480, -15.61618894467929941, -35.14999999999999858 ) ) ;
#29550 = EDGE_LOOP ( 'NONE', ( #20600, #31829, #3086, #43947 ) ) ;
#29551 = ADVANCED_FACE ( 'NONE', ( #40010 ), #4097, .T. ) ;
#29552 = ORIENTED_EDGE ( 'NONE', *, *, #38044, .T. ) ;
#29553 = CARTESIAN_POINT ( 'NONE',  ( 12.16177399482889854, -65.11171494345551025, -16.53048058985559976 ) ) ;
#29554 = CARTESIAN_POINT ( 'NONE',  ( 11.13615425759000033, 32.70713249819939961, -44.52190971338829684 ) ) ;
#29555 = CARTESIAN_POINT ( 'NONE',  ( 16.63095995406284899, -7.653195049244535753, -39.02733329801645823 ) ) ;
#29556 = CARTESIAN_POINT ( 'NONE',  ( 12.45971295103579912, 34.17435175697750083, -46.68166270225199810 ) ) ;
#29557 = LINE ( 'NONE', #49247, #21646 ) ;
#29558 = ORIENTED_EDGE ( 'NONE', *, *, #20657, .F. ) ;
#29559 = CARTESIAN_POINT ( 'NONE',  ( -13.72343451011500015, -40.91412750062520587, -46.69925608350429513 ) ) ;
#29560 = DIRECTION ( 'NONE',  ( -2.840828347717470042E-11, 6.470619327693540153E-12, 1.000000000000000000 ) ) ;
#29561 = CIRCLE ( 'NONE', #46355, 10.27649999999999864 ) ;
#29562 = CARTESIAN_POINT ( 'NONE',  ( 49.63827221850689853, 21.52948366499370181, -52.16690606469470026 ) ) ;
#29563 = DIRECTION ( 'NONE',  ( 1.000000000000000000, 0.000000000000000000, 0.000000000000000000 ) ) ;
#29564 = CARTESIAN_POINT ( 'NONE',  ( 51.29313475710210213, -49.49861581368470098, -76.46030551791849916 ) ) ;
#29565 = CARTESIAN_POINT ( 'NONE',  ( 10.61751707702999958, -64.82563018156609758, -18.17419295931939871 ) ) ;
#29566 = ORIENTED_EDGE ( 'NONE', *, *, #16591, .T. ) ;
#29567 = CARTESIAN_POINT ( 'NONE',  ( 52.87639532687909849, -49.52782412333860407, -27.19604750702719898 ) ) ;
#29568 = LINE ( 'NONE', #45574, #24205 ) ;
#29569 = ORIENTED_EDGE ( 'NONE', *, *, #26257, .F. ) ;
#29570 = CARTESIAN_POINT ( 'NONE',  ( 68.13393739769620083, 0.8838110553206759423, -65.65000000000000568 ) ) ;
#29571 = CYLINDRICAL_SURFACE ( 'NONE', #1883, 21.50000000000000000 ) ;
#29572 = CARTESIAN_POINT ( 'NONE',  ( 20.50561976785459706, -9.485587557738790920, -31.70967419469809201 ) ) ;
#29573 = CARTESIAN_POINT ( 'NONE',  ( 68.13393739769769297, 18.72622661238300168, -73.39853292320978539 ) ) ;
#29574 = CARTESIAN_POINT ( 'NONE',  ( 53.84012107995949492, 19.74703357530859904, -75.89928047384410092 ) ) ;
#29575 = ADVANCED_FACE ( 'NONE', ( #42920 ), #22968, .T. ) ;
#29576 = CARTESIAN_POINT ( 'NONE',  ( 47.51793463416109375, -54.37766850872819901, -75.00961804031550173 ) ) ;
#29577 = ORIENTED_EDGE ( 'NONE', *, *, #38270, .T. ) ;
#29578 = CARTESIAN_POINT ( 'NONE',  ( 55.84963547784990112, 14.51039859417369904, -16.94429277193919958 ) ) ;
#29579 = CARTESIAN_POINT ( 'NONE',  ( 22.90091122653545241, -15.61618862529044804, -78.45282272177526295 ) ) ;
#29580 = AXIS2_PLACEMENT_3D ( 'NONE', #49991, #10419, #10679 ) ;
#29581 = B_SPLINE_CURVE_WITH_KNOTS ( 'NONE', 3,
 ( #27437, #8050, #3866, #20088, #43440, #36079, #16164, #7543, #47630, #23487, #3611, #32121, #19581, #31612, #34402, #38355, #33430, #8828, #13034, #29504, #36859, #24515, #28466, #40531, #10323, #9087, #29240, #6392, #24779, #5417, #28987, #13544, #37124, #40788, #20857, #28721, #1480, #33171, #4889, #46235, #41308, #690, #26284 ),
 .UNSPECIFIED., .F., .F.,
 ( 4, 2, 2, 1, 1, 1, 2, 2, 2, 2, 1, 1, 1, 1, 2, 2, 2, 2, 2, 1, 1, 1, 1, 2, 2, 2, 4 ),
 ( 0.000000000000000000, 0.1249999999999913958, 0.1874999999999870937, 0.2187499999999848455, 0.2343749999999837907, 0.2421874999999832079, 0.2460937499999829858, 0.2499999999999827360, 0.3749999999999771849, 0.4374999999999744094, 0.4687499999999731326, 0.4843749999999725220, 0.4921874999999722444, 0.4960937499999720779, 0.4980468749999720224, 0.4999999999999720224, 0.6249999999999749090, 0.6874999999999764633, 0.7187499999999771294, 0.7343749999999775735, 0.7421874999999777955, 0.7460937499999776845, 0.7480468749999776845, 0.7490234374999776845, 0.7499999999999775735, 0.8749999999999887867, 1.000000000000000000 ),
 .UNSPECIFIED. ) ;
#29582 = CARTESIAN_POINT ( 'NONE',  ( 57.04000892342570239, -50.62678238285099752, -53.73354994388930095 ) ) ;
#29583 = CARTESIAN_POINT ( 'NONE',  ( 15.14368416393440064, -8.633212666080371633, -38.30233936351839219 ) ) ;
#29584 = DIRECTION ( 'NONE',  ( -0.6676418852213141797, -0.2329255526946994725, -0.7071067811865463515 ) ) ;
#29585 = CARTESIAN_POINT ( 'NONE',  ( 47.03708331872790183, 22.68146662604199548, -75.76197391125640479 ) ) ;
#29586 = CARTESIAN_POINT ( 'NONE',  ( 65.05533261316259086, 1.330484379554840002, -60.80906431331560213 ) ) ;
#29587 = CARTESIAN_POINT ( 'NONE',  ( 75.29711369228711249, -36.44373308530014555, -12.51629082861420983 ) ) ;
#29588 = FACE_OUTER_BOUND ( 'NONE', #12217, .T. ) ;
#29589 = CARTESIAN_POINT ( 'NONE',  ( 29.11414631625610028, -4.499707858305580288, -35.00928286143069812 ) ) ;
#29590 = CARTESIAN_POINT ( 'NONE',  ( 18.27002738368036461, -49.61612325953908709, -83.13257468804646066 ) ) ;
#29591 = VECTOR ( 'NONE', #16234, 1000.000000000000000 ) ;
#29592 = CARTESIAN_POINT ( 'NONE',  ( 60.24058964203519650, -45.77817723718867171, -47.32689780713828753 ) ) ;
#29594 = CARTESIAN_POINT ( 'NONE',  ( 46.38238331322911279, -40.25953821574219660, -54.52185312847988286 ) ) ;
#29593 = CARTESIAN_POINT ( 'NONE',  ( 88.13393739769620083, -48.61618894467930119, -65.65000000000000568 ) ) ;
#29595 = CARTESIAN_POINT ( 'NONE',  ( 61.30391822008160574, 13.98869160185730109, -46.40371986329420650 ) ) ;
#29596 = CARTESIAN_POINT ( 'NONE',  ( 9.133937397696200833, -15.61618894467929941, -82.15000000000000568 ) ) ;
#29597 = CARTESIAN_POINT ( 'NONE',  ( -28.48658230523989943, 4.086499779700029755, -54.95457219459440523 ) ) ;
#29598 = ORIENTED_EDGE ( 'NONE', *, *, #48869, .F. ) ;
#29599 = CARTESIAN_POINT ( 'NONE',  ( 52.80835662174770562, -49.67696413664329924, -48.72774921968630224 ) ) ;
#29600 = ORIENTED_EDGE ( 'NONE', *, *, #41852, .F. ) ;
#29601 = CARTESIAN_POINT ( 'NONE',  ( 61.72354181936940165, -45.11618267485779654, -28.15139908431080329 ) ) ;
#29602 = CARTESIAN_POINT ( 'NONE',  ( 16.13393739769620083, -30.04994567442000175, -34.64999999999999858 ) ) ;
#29603 = CARTESIAN_POINT ( 'NONE',  ( 13.41560639233609997, 19.85270852858930013, -21.91538712361600005 ) ) ;
#29604 = DIRECTION ( 'NONE',  ( 0.3618033988749886909, 0.2628655560595663521, 0.8944271909999162995 ) ) ;
#29605 = CARTESIAN_POINT ( 'NONE',  ( 9.378617007155710894, -17.64305971455430111, -47.36003476421489466 ) ) ;
#29606 = CARTESIAN_POINT ( 'NONE',  ( 50.04022686075009574, 17.68250774392249980, -76.14999999999999147 ) ) ;
#29607 = CARTESIAN_POINT ( 'NONE',  ( 53.23191249145569515, 18.23954733812280082, -48.99600492437400590 ) ) ;
#29608 = CARTESIAN_POINT ( 'NONE',  ( 60.83775786089130122, -45.46530407581749955, -47.05478991720049464 ) ) ;
#29609 = CARTESIAN_POINT ( 'NONE',  ( 47.26610112325450075, 22.82567072896360116, -75.56421356201970241 ) ) ;
#29610 = VERTEX_POINT ( 'NONE', #3085 ) ;
#29611 = EDGE_CURVE ( 'NONE', #36176, #40719, #1627, .T. ) ;
#29612 = CARTESIAN_POINT ( 'NONE',  ( 8.793629121247519720, -16.89155898707499759, -74.01258338267071224 ) ) ;
#29613 = CARTESIAN_POINT ( 'NONE',  ( 73.11007580172049813, 0.9281439705311279598, -69.00235340255149197 ) ) ;
#29614 = CARTESIAN_POINT ( 'NONE',  ( 47.42536334077440330, -54.63837742691509902, -54.75923846447550147 ) ) ;
#29615 = CARTESIAN_POINT ( 'NONE',  ( 8.871876924530811337, -12.37411265878318289, -48.92611659854718198 ) ) ;
#29616 = CARTESIAN_POINT ( 'NONE',  ( 73.19885236215881719, 0.9940695285616559795, -62.44811160372290004 ) ) ;
#29617 = CARTESIAN_POINT ( 'NONE',  ( 11.75767683379359951, -65.42451930117039183, -18.01774807210410145 ) ) ;
#29619 = ADVANCED_FACE ( 'NONE', ( #11207 ), #17606, .T. ) ;
#29618 = CARTESIAN_POINT ( 'NONE',  ( 53.26662649590710430, 18.19965403720820163, -48.79175420715159817 ) ) ;
#29620 = CARTESIAN_POINT ( 'NONE',  ( 23.98099588838510599, -16.65306419375328417, -75.83413829860595001 ) ) ;
#29621 = CARTESIAN_POINT ( 'NONE',  ( 20.99562822605996004, -9.290033917162169530, -45.50063643852418238 ) ) ;
#29622 = CARTESIAN_POINT ( 'NONE',  ( 48.82567944655220060, -28.11618894467929763, -15.65000000000000036 ) ) ;
#29623 = EDGE_CURVE ( 'NONE', #31353, #28785, #44891, .T. ) ;
#29624 = CARTESIAN_POINT ( 'NONE',  ( 64.79388653638659434, 0.9272522097097989358, -70.63440435907199344 ) ) ;
#29625 = ORIENTED_EDGE ( 'NONE', *, *, #35181, .F. ) ;
#29626 = CARTESIAN_POINT ( 'NONE',  ( 9.281183340106311519, -63.16631044210069490, -46.53144401359779891 ) ) ;
#29627 = CARTESIAN_POINT ( 'NONE',  ( 16.13393739566809870, -15.61618894418049841, 9.349999999609689638 ) ) ;
#29628 = VERTEX_POINT ( 'NONE', #28352 ) ;
#29629 = CARTESIAN_POINT ( 'NONE',  ( 8.222937397696199469, -15.61618894467929941, -32.14999999999999858 ) ) ;
#29630 = CARTESIAN_POINT ( 'NONE',  ( 67.56344246713349833, -30.11618894467929763, -21.20855465508889992 ) ) ;
#29631 = CARTESIAN_POINT ( 'NONE',  ( 9.366438350291463877, -15.74334315553391939, -53.84120313986934292 ) ) ;
#29632 = CARTESIAN_POINT ( 'NONE',  ( 52.83096320285449821, 19.79380150020979912, -76.09006749206929499 ) ) ;
#29633 = EDGE_LOOP ( 'NONE', ( #42483, #14581, #23991, #34065 ) ) ;
#29634 = FACE_OUTER_BOUND ( 'NONE', #34305, .T. ) ;
#29635 = CARTESIAN_POINT ( 'NONE',  ( 11.63393739769621682, -41.61618894467939356, -35.01561944896766221 ) ) ;
#29636 = CARTESIAN_POINT ( 'NONE',  ( 23.40487804057610077, -19.50413727556700039, -57.94863426729589406 ) ) ;
#29637 = AXIS2_PLACEMENT_3D ( 'NONE', #7169, #30736, #34928 ) ;
#29638 = CARTESIAN_POINT ( 'NONE',  ( 16.13393739769620083, -15.61618894467929941, -10.90000000000000036 ) ) ;
#29639 = CARTESIAN_POINT ( 'NONE',  ( 44.28551402523930847, -37.95431502561086035, -68.89210660893036220 ) ) ;
#29640 = EDGE_CURVE ( 'NONE', #9028, #51719, #32789, .T. ) ;
#29641 = EDGE_LOOP ( 'NONE', ( #29129, #35875, #8975, #40902, #48522, #36130 ) ) ;
#29642 = CARTESIAN_POINT ( 'NONE',  ( 57.11003303655699881, -45.86943814250939511, -26.25113407850079739 ) ) ;
#29643 = CARTESIAN_POINT ( 'NONE',  ( 9.253865619591300273, -12.75763928912490108, -49.35800193134529934 ) ) ;
#29644 = CARTESIAN_POINT ( 'NONE',  ( 8.864140624387911060, -15.38326400578280051, -32.14999999999999858 ) ) ;
#29645 = VECTOR ( 'NONE', #24417, 1000.000000000000000 ) ;
#29646 = B_SPLINE_CURVE_WITH_KNOTS ( 'NONE', 3,
 ( #46778, #43097, #38651, #19486, #2740, #51469, #50690, #15044 ),
 .UNSPECIFIED., .F., .F.,
 ( 4, 2, 2, 4 ),
 ( -0.1350635247393814631, -0.1243669311585589993, -0.1075965482633170073, -0.1052074838078570079 ),
 .UNSPECIFIED. ) ;
#29647 = CARTESIAN_POINT ( 'NONE',  ( 14.13833034204109929, 19.89798265472740013, -74.14993923597710079 ) ) ;
#29648 = CARTESIAN_POINT ( 'NONE',  ( 12.84688943576609788, -51.59382062313621020, -21.73578643762666474 ) ) ;
#29649 = CARTESIAN_POINT ( 'NONE',  ( 43.56376642346300798, -45.24482142066580792, -7.028087995143840416 ) ) ;
#29650 = CARTESIAN_POINT ( 'NONE',  ( 24.03277050005166515, -15.16864035720454140, -61.48966201727984071 ) ) ;
#29651 = EDGE_CURVE ( 'NONE', #13682, #25181, #37272, .T. ) ;
#29652 = CARTESIAN_POINT ( 'NONE',  ( 14.42519478801719934, -23.68234784485250088, -56.07411718121299771 ) ) ;
#29653 = VERTEX_POINT ( 'NONE', #24667 ) ;
#29654 = CARTESIAN_POINT ( 'NONE',  ( 54.30624051828319665, -47.99265254736189945, -26.34811334082180068 ) ) ;
#29655 = CARTESIAN_POINT ( 'NONE',  ( 15.24233146011200013, -51.07047254194969810, -21.55962016779339763 ) ) ;
#29657 = CARTESIAN_POINT ( 'NONE',  ( 45.83414061996360545, -15.61618894467929586, 7.944363289481099599 ) ) ;
#29656 = CARTESIAN_POINT ( 'NONE',  ( 0.07122129016301401161, 22.52064049785749944, -9.361296192847889941 ) ) ;
#29658 = CARTESIAN_POINT ( 'NONE',  ( 9.543024404835053431, -17.38729190938108360, -57.36946905751702275 ) ) ;
#29659 = CARTESIAN_POINT ( 'NONE',  ( 8.784728771152170879, -54.93525725209899235, -46.67204636145419983 ) ) ;
#29660 = ORIENTED_EDGE ( 'NONE', *, *, #23058, .F. ) ;
#29661 = CARTESIAN_POINT ( 'NONE',  ( -9.530397888691508612, -43.65111778182789948, -5.718006680799840424 ) ) ;
#29662 = CARTESIAN_POINT ( 'NONE',  ( 47.42537234911539912, 23.41034979696710039, -54.89678846924610411 ) ) ;
#29663 = CARTESIAN_POINT ( 'NONE',  ( 63.32591849070559675, 1.327322800621349996, -62.49772215509980100 ) ) ;
#29664 = CARTESIAN_POINT ( 'NONE',  ( 61.05528012745969590, 14.12195704883330194, -46.96576354475939752 ) ) ;
#29665 = CARTESIAN_POINT ( 'NONE',  ( 43.91474985106849971, 12.31375205234749970, -5.093415854460159764 ) ) ;
#29666 = CARTESIAN_POINT ( 'NONE',  ( 51.99247920141849733, 18.26518619690140000, -77.11023342130459923 ) ) ;
#29667 = CARTESIAN_POINT ( 'NONE',  ( 53.41693480164800434, 18.12090330447900044, -48.75416851879799651 ) ) ;
#29668 = DIRECTION ( 'NONE',  ( -0.6911981449639439390, -0.7226652920947588266, 0.000000000000000000 ) ) ;
#29669 = CARTESIAN_POINT ( 'NONE',  ( -10.98055936835113577, -21.27930790530396266, -84.65000000000000568 ) ) ;
#29670 = CARTESIAN_POINT ( 'NONE',  ( 22.90085138535262743, -15.65142864927533317, -66.45447747818334960 ) ) ;
#29671 = AXIS2_PLACEMENT_3D ( 'NONE', #38694, #46042, #2785 ) ;
#29672 = CARTESIAN_POINT ( 'NONE',  ( 53.42290160909190178, 20.83982452118389972, -54.29362578891399949 ) ) ;
#29673 = CARTESIAN_POINT ( 'NONE',  ( 63.28456881472469320, 0.9543419100865909721, -69.18369337885960135 ) ) ;
#29674 = DIRECTION ( 'NONE',  ( 0.000000000000000000, 0.000000000000000000, -1.000000000000000000 ) ) ;
#29675 = ORIENTED_EDGE ( 'NONE', *, *, #19847, .T. ) ;
#29676 = CARTESIAN_POINT ( 'NONE',  ( 19.71487976213365201, 22.98215037303318553, -17.34801211495729234 ) ) ;
#29677 = CARTESIAN_POINT ( 'NONE',  ( 10.97982412035660005, 32.17011673400409677, -44.74671143413180374 ) ) ;
#29678 = CARTESIAN_POINT ( 'NONE',  ( 16.13393739769620083, -15.61618894467929941, -28.45282021618999835 ) ) ;
#29679 = CARTESIAN_POINT ( 'NONE',  ( 66.39754877122931020, -33.04911773559199872, -19.74076586694979696 ) ) ;
#29680 = EDGE_CURVE ( 'NONE', #40270, #51808, #49084, .T. ) ;
#29681 = AXIS2_PLACEMENT_3D ( 'NONE', #41582, #18508, #21644 ) ;
#29682 = CARTESIAN_POINT ( 'NONE',  ( 22.21314585784342199, -19.19191036455051247, -47.01642178051652365 ) ) ;
#29683 = ORIENTED_EDGE ( 'NONE', *, *, #34222, .T. ) ;
#29684 = ORIENTED_EDGE ( 'NONE', *, *, #43084, .T. ) ;
#29685 = CARTESIAN_POINT ( 'NONE',  ( 48.76908445385270596, 22.82217318232569880, -55.30112621652450144 ) ) ;
#29686 = VECTOR ( 'NONE', #45467, 1000.000000000000000 ) ;
#29687 = ORIENTED_EDGE ( 'NONE', *, *, #4891, .F. ) ;
#29688 = CARTESIAN_POINT ( 'NONE',  ( 12.11637196722969989, -65.28199310085939544, -46.68580356066069470 ) ) ;
#29689 = CARTESIAN_POINT ( 'NONE',  ( 57.46694081946250066, -45.43955118043039931, -26.08166122527880049 ) ) ;
#29690 = CARTESIAN_POINT ( 'NONE',  ( 22.90075166721855737, -15.61618922411645727, -44.45281379938008115 ) ) ;
#29691 = CARTESIAN_POINT ( 'NONE',  ( 23.62400244246340009, -48.75656286698960429, -35.12503119152809461 ) ) ;
#29692 = VERTEX_POINT ( 'NONE', #25453 ) ;
#29693 = CARTESIAN_POINT ( 'NONE',  ( 46.45338246003043992, 6.966592679198189586, -58.05277450657466431 ) ) ;
#29694 = VERTEX_POINT ( 'NONE', #21268 ) ;
#29695 = CARTESIAN_POINT ( 'NONE',  ( 48.64442696764240281, -45.11618894461089724, -9.632282537063208139 ) ) ;
#29696 = CARTESIAN_POINT ( 'NONE',  ( 14.57822604302202585, -23.39323822619865823, -34.35516676250910706 ) ) ;
#29697 = CARTESIAN_POINT ( 'NONE',  ( 15.36633100621490122, 19.87547805676619816, -21.74512139206969863 ) ) ;
#29698 = CARTESIAN_POINT ( 'NONE',  ( 22.90088880405416205, -15.64389692910371821, -50.45412216600715993 ) ) ;
#29699 = EDGE_CURVE ( 'NONE', #21348, #30264, #1373, .T. ) ;
#29700 = VERTEX_POINT ( 'NONE', #24409 ) ;
#29701 = DIRECTION ( 'NONE',  ( 0.000000000000000000, 0.000000000000000000, -1.000000000000000000 ) ) ;
#29702 = CARTESIAN_POINT ( 'NONE',  ( 46.89823403300989924, -54.16139584019150277, -75.66073271794819277 ) ) ;
#29703 = DIRECTION ( 'NONE',  ( 1.000000000000000000, 0.000000000000000000, 0.000000000000000000 ) ) ;
#29704 = CARTESIAN_POINT ( 'NONE',  ( 49.01168265687110193, 13.88381105532070059, -9.596379464110540880 ) ) ;
#29705 = AXIS2_PLACEMENT_3D ( 'NONE', #31056, #47080, #39200 ) ;
#29706 = DIRECTION ( 'NONE',  ( 0.000000000000000000, 0.000000000000000000, 1.000000000000000000 ) ) ;
#29707 = AXIS2_PLACEMENT_3D ( 'NONE', #18693, #14769, #30737 ) ;
#29708 = CARTESIAN_POINT ( 'NONE',  ( 50.96210802353969882, 19.72521229730620007, -76.15000017728949899 ) ) ;
#29709 = CARTESIAN_POINT ( 'NONE',  ( 61.66992079451529918, 13.88595891104769997, -28.08578151254650024 ) ) ;
#29710 = EDGE_CURVE ( 'NONE', #24630, #28785, #29400, .T. ) ;
#29711 = CARTESIAN_POINT ( 'NONE',  ( 8.402054737090029590, -16.95959458178240098, -74.23274628532179520 ) ) ;
#29712 = B_SPLINE_SURFACE_WITH_KNOTS ( 'NONE', 3, 3, ( 
 ( #19432, #11844, #31462, #39359, #19933, #39612, #43799, #27802, #51157, #47486, #11324, #15251 ),
 ( #32222, #31712, #41, #28304, #11582, #28047, #51665, #36178, #7899, #27543, #19687, #47993 ),
 ( #40373, #4214, #285, #12093, #23845, #31973, #35680, #15759, #15508, #35411, #35924, #44051 ),
 ( #47737, #44305, #31204, #27288, #24360, #51413, #16269, #24100, #39869, #16017, #8156, #40121 ),
 ( #20188, #48246, #12340, #8414, #4471, #20440, #43296, #7388, #37226, #33536, #12870, #45352 ),
 ( #20697, #40631, #25146, #44829, #29088, #8666, #21479, #49554, #37479, #8935, #1579, #13388 ),
 ( #13138, #41406, #41150, #5524, #17569, #33275, #17312, #1323, #13642, #16522, #9194, #9455 ),
 ( #29601, #48501, #36688, #49291, #32738, #45605, #20961, #36961, #9702, #1059, #25663, #29347 ),
 ( #25404, #41666, #48766, #5264, #5770, #36427, #12603, #535, #28826, #32470, #28565, #44565 ) ),
 .UNSPECIFIED., .F., .F., .F.,
 ( 4, 1, 1, 1, 1, 1, 4 ),
 ( 4, 2, 2, 2, 2, 4 ),
 ( -0.0004221351757990000008, 0.1666666666666670182, 0.3333333333333329818, 0.5000000000000000000, 0.6666666666666670737, 0.8333333333333330373, 1.000484995316600179 ),
 ( -0.0004754643611709999948, 0.1427389027784959907, 0.4935706371843600060, 0.8180431554277900474, 1.090724207237049992, 1.220493132826130145 ),
 .UNSPECIFIED. ) ;
#29713 = ORIENTED_EDGE ( 'NONE', *, *, #10774, .F. ) ;
#29715 = EDGE_CURVE ( 'NONE', #23939, #38446, #5573, .T. ) ;
#29714 = CARTESIAN_POINT ( 'NONE',  ( 49.40552051342540096, 22.26542118999089936, -54.15739458345379376 ) ) ;
#29716 = CARTESIAN_POINT ( 'NONE',  ( 73.02919596257699197, 0.9065823421260940096, -62.18054194328749418 ) ) ;
#29717 = DIRECTION ( 'NONE',  ( 0.000000000000000000, 0.000000000000000000, 1.000000000000000000 ) ) ;
#29718 = CARTESIAN_POINT ( 'NONE',  ( 73.01385068780759013, 0.9098571636355720083, -69.14090909090960224 ) ) ;
#29719 = EDGE_CURVE ( 'NONE', #11933, #45450, #25710, .T. ) ;
#29720 = DIRECTION ( 'NONE',  ( 0.2260571801428161443, 0.000000000000000000, -0.9741140340359945027 ) ) ;
#29721 = CARTESIAN_POINT ( 'NONE',  ( 11.27217872414320077, -9.290084753452736877, -42.79930174472833926 ) ) ;
#29722 = CARTESIAN_POINT ( 'NONE',  ( 8.223295469878840080, -15.61636541503349918, -58.79233150823709764 ) ) ;
#29723 = DIRECTION ( 'NONE',  ( 0.000000000000000000, 0.000000000000000000, -1.000000000000000000 ) ) ;
#29724 = DIRECTION ( 'NONE',  ( 0.5720614028176865817, 0.4156269377774496343, 0.7071067811865480168 ) ) ;
#29725 = CARTESIAN_POINT ( 'NONE',  ( 76.48559721756747365, -43.24489215890645966, -14.05942286515468709 ) ) ;
#29726 = CARTESIAN_POINT ( 'NONE',  ( -6.866062602303800055, -15.61618894467929586, -15.65000000000000036 ) ) ;
#29727 = VERTEX_POINT ( 'NONE', #34355 ) ;
#29728 = CARTESIAN_POINT ( 'NONE',  ( 9.178575242519139366, -18.28632595027880114, -55.95066710016559597 ) ) ;
#29729 = CARTESIAN_POINT ( 'NONE',  ( 64.71095929546520154, 1.416242794300709873, -61.14503753232310146 ) ) ;
#29730 = VERTEX_POINT ( 'NONE', #26237 ) ;
#29731 = CARTESIAN_POINT ( 'NONE',  ( 54.47259832750690123, -46.25232753665150653, -15.76422791930239953 ) ) ;
#29732 = CARTESIAN_POINT ( 'NONE',  ( 60.82047572193099683, -45.70664521776530620, -47.72863310528089897 ) ) ;
#29733 = CARTESIAN_POINT ( 'NONE',  ( 9.669467020143732938, -13.02337471114221756, -73.96911144341058275 ) ) ;
#29734 = CARTESIAN_POINT ( 'NONE',  ( 21.72939861980660581, -21.20857138557213872, -61.75757471702103629 ) ) ;
#29736 = DIRECTION ( 'NONE',  ( 0.000000000000000000, 1.000000000000000000, 0.000000000000000000 ) ) ;
#29735 = CARTESIAN_POINT ( 'NONE',  ( 44.34764830394051671, 8.750173897780856080, -64.97525299307636715 ) ) ;
#29737 = AXIS2_PLACEMENT_3D ( 'NONE', #4724, #12864, #41143 ) ;
#29738 = LINE ( 'NONE', #4873, #30151 ) ;
#29739 = CARTESIAN_POINT ( 'NONE',  ( 40.82288980517279953, -45.39598238709950095, -5.804594144209599627 ) ) ;
#29740 = EDGE_CURVE ( 'NONE', #4643, #42078, #40495, .T. ) ;
#29741 = EDGE_LOOP ( 'NONE', ( #17108, #233, #13367, #2972 ) ) ;
#29742 = AXIS2_PLACEMENT_3D ( 'NONE', #18314, #50309, #18579 ) ;
#29743 = ORIENTED_EDGE ( 'NONE', *, *, #33998, .T. ) ;
#29744 = B_SPLINE_CURVE_WITH_KNOTS ( 'NONE', 3,
 ( #39140, #26807, #50928, #3232, #15287, #35189, #35451, #51193, #15024, #30992, #47270, #46239, #2975, #11358, #43330, #14251, #26287, #30220, #42296, #10327, #42819, #27069 ),
 .UNSPECIFIED., .F., .F.,
 ( 4, 2, 1, 1, 2, 2, 2, 2, 1, 1, 2, 2, 4 ),
 ( 0.5278395012772089112, 0.5352170090697533356, 0.5425945168622977599, 0.5573495324473857204, 0.5868595636175617525, 0.6458796259579139276, 0.7639197506386171677, 0.7712972584311608149, 0.7786747662237045731, 0.7934297818087913123, 0.8229398129789644578, 0.8819598753193100826, 1.000000000000000000 ),
 .UNSPECIFIED. ) ;
#29745 = EDGE_LOOP ( 'NONE', ( #29098, #10448, #8465, #33223, #40723 ) ) ;
#29746 = CARTESIAN_POINT ( 'NONE',  ( -22.83415939270349782, -16.77728946961760670, -54.74109773066948037 ) ) ;
#29747 = DIRECTION ( 'NONE',  ( 0.3535533905932799481, 0.6123724356957926940, 0.7071067811865460184 ) ) ;
#29748 = ORIENTED_EDGE ( 'NONE', *, *, #3600, .T. ) ;
#29749 = ORIENTED_EDGE ( 'NONE', *, *, #31496, .F. ) ;
#29750 = DIRECTION ( 'NONE',  ( 0.000000000000000000, 0.000000000000000000, 1.000000000000000000 ) ) ;
#29751 = CARTESIAN_POINT ( 'NONE',  ( 7.853097003783789276, 29.28805065900050053, -20.86915960608759946 ) ) ;
#29752 = CARTESIAN_POINT ( 'NONE',  ( 16.13393739769620083, -29.64169738395614218, -34.79644660940672907 ) ) ;
#29753 = ORIENTED_EDGE ( 'NONE', *, *, #5581, .F. ) ;
#29754 = CARTESIAN_POINT ( 'NONE',  ( 0.1457839871805953758, -45.96255801450852374, -34.68167748489142355 ) ) ;
#29755 = CARTESIAN_POINT ( 'NONE',  ( 52.21153808996899670, -50.42173267543250148, -76.55085343181869462 ) ) ;
#29756 = CARTESIAN_POINT ( 'NONE',  ( 14.28038030992529528, -32.47778390180254604, -34.79644291222909658 ) ) ;
#29757 = CARTESIAN_POINT ( 'NONE',  ( 13.35425103422070059, -8.277245470834399654, -63.39724662014580048 ) ) ;
#29758 = CIRCLE ( 'NONE', #9692, 2.999999999999999112 ) ;
#29759 = CARTESIAN_POINT ( 'NONE',  ( 2.434269054290310041, -5.465919710348150495, -34.90839531524139971 ) ) ;
#29760 = CARTESIAN_POINT ( 'NONE',  ( 43.56381279507350257, 14.01244564278079885, -7.028114315100149945 ) ) ;
#29761 = CARTESIAN_POINT ( 'NONE',  ( 42.15277068293529794, -43.77269754269769919, -4.489091470016449925 ) ) ;
#29762 = LINE ( 'NONE', #37140, #17805 ) ;
#29763 = CARTESIAN_POINT ( 'NONE',  ( -6.923935172077830380, 14.83398127567929947, -5.625849176739690094 ) ) ;
#29764 = SHAPE_REPRESENTATION ( 'MAS-691', ( #11805, #9301, #23463, #5109, #31042, #41945, #86 ), #38585 ) ;
#29765 = CARTESIAN_POINT ( 'NONE',  ( 63.94229026696169882, 1.409766646916870148, -69.70656394866479388 ) ) ;
#29766 = AXIS2_PLACEMENT_3D ( 'NONE', #23458, #34751, #2543 ) ;
#29767 = DIRECTION ( 'NONE',  ( 0.000000000000000000, 1.000000000000000000, 0.000000000000000000 ) ) ;
#29768 = CARTESIAN_POINT ( 'NONE',  ( 66.23675738725249573, 0.5074413136232309718, -17.49605282672580131 ) ) ;
#29769 = ORIENTED_EDGE ( 'NONE', *, *, #38654, .F. ) ;
#29771 = EDGE_CURVE ( 'NONE', #50414, #5441, #16419, .T. ) ;
#29770 = CARTESIAN_POINT ( 'NONE',  ( 14.90064049178520023, -52.99263752172900155, -76.14999999999999147 ) ) ;
#29772 = CARTESIAN_POINT ( 'NONE',  ( 47.18324198357289845, -54.80726809202429450, -54.61058319554170026 ) ) ;
#29773 = ADVANCED_FACE ( 'NONE', ( #42244 ), #38308, .T. ) ;
#29774 = DIRECTION ( 'NONE',  ( 0.000000000000000000, -1.000000000000000000, 0.000000000000000000 ) ) ;
#29775 = CARTESIAN_POINT ( 'NONE',  ( 57.55751162049570269, -48.61618894467930119, -53.92796738110899923 ) ) ;
#29776 = CARTESIAN_POINT ( 'NONE',  ( -1.839728563314010135, -2.929686987007059873, -54.64999999999999858 ) ) ;
#29777 = CARTESIAN_POINT ( 'NONE',  ( 63.36539477273620236, 1.325715844996850024, -68.88725199158329815 ) ) ;
#29778 = CARTESIAN_POINT ( 'NONE',  ( 47.68932896513950226, -54.51079220110009516, -55.03972088635050142 ) ) ;
#29779 = CARTESIAN_POINT ( 'NONE',  ( 47.40322300430479885, 23.42336669154508755, -60.76348542011150045 ) ) ;
#29780 = DIRECTION ( 'NONE',  ( 1.000000000000000000, 0.000000000000000000, 0.000000000000000000 ) ) ;
#29781 = CARTESIAN_POINT ( 'NONE',  ( 48.05009841671569859, 23.12298604439770244, -55.13457781729299967 ) ) ;
#29782 = ORIENTED_EDGE ( 'NONE', *, *, #10177, .T. ) ;
#29783 = CARTESIAN_POINT ( 'NONE',  ( 22.27312146484720046, -12.14444901143390076, -72.68335544512909507 ) ) ;
#29784 = VERTEX_POINT ( 'NONE', #30424 ) ;
#29785 = CYLINDRICAL_SURFACE ( 'NONE', #9515, 0.4999999999999982236 ) ;
#29786 = CARTESIAN_POINT ( 'NONE',  ( 16.13393739769620083, -15.61618894467929941, 6.850000000000000533 ) ) ;
#29787 = CARTESIAN_POINT ( 'NONE',  ( 22.04686114124215379, -19.02415750966752483, -42.61948640318105674 ) ) ;
#29789 = CARTESIAN_POINT ( 'NONE',  ( 54.53415579258169998, 16.40665704925320156, -25.91141317301960001 ) ) ;
#29788 = CARTESIAN_POINT ( 'NONE',  ( 83.30448183675929386, 14.00823756214430027, -47.41172112684520101 ) ) ;
#29790 = CARTESIAN_POINT ( 'NONE',  ( 10.53269849474080111, -11.33031896897490043, -73.66071987733648996 ) ) ;
#29791 = FACE_OUTER_BOUND ( 'NONE', #43676, .T. ) ;
#29792 = DIRECTION ( 'NONE',  ( -1.000000000000000000, 0.000000000000000000, 0.000000000000000000 ) ) ;
#29793 = DIRECTION ( 'NONE',  ( 0.000000000000000000, 0.000000000000000000, -1.000000000000000000 ) ) ;
#29794 = EDGE_CURVE ( 'NONE', #17232, #45765, #26428, .T. ) ;
#29795 = LINE ( 'NONE', #18274, #27305 ) ;
#29796 = AXIS2_PLACEMENT_3D ( 'NONE', #23794, #43745, #39810 ) ;
#29797 = ORIENTED_EDGE ( 'NONE', *, *, #21269, .F. ) ;
#29798 = ADVANCED_FACE ( 'NONE', ( #10011 ), #1890, .T. ) ;
#29799 = EDGE_LOOP ( 'NONE', ( #49707, #6319, #30907, #38405, #16246 ) ) ;
#29800 = CARTESIAN_POINT ( 'NONE',  ( 12.26707159644750078, -64.72375542069319465, -15.95265749177709935 ) ) ;
#29801 = CARTESIAN_POINT ( 'NONE',  ( 11.09709394051290055, 32.24280216238350505, -44.33319920883189980 ) ) ;
#29802 = CARTESIAN_POINT ( 'NONE',  ( 24.04454178464035152, -15.53069869766736311, -39.50423254393393080 ) ) ;
#29803 = CARTESIAN_POINT ( 'NONE',  ( 9.366455112259469473, -15.61627688590920116, -55.45282021618999835 ) ) ;
#29804 = CARTESIAN_POINT ( 'NONE',  ( 68.13393739769618662, -0.1661889446793599900, -65.65000000000000568 ) ) ;
#29805 = VECTOR ( 'NONE', #25068, 1000.000000000000000 ) ;
#29806 = VERTEX_POINT ( 'NONE', #41984 ) ;
#29807 = CARTESIAN_POINT ( 'NONE',  ( -22.79226920359159791, -13.71770807034589978, -54.60327039117859727 ) ) ;
#29808 = AXIS2_PLACEMENT_3D ( 'NONE', #10354, #31271, #30763 ) ;
#29809 = DIRECTION ( 'NONE',  ( 1.000000000000000000, 0.000000000000000000, 0.000000000000000000 ) ) ;
#29810 = CARTESIAN_POINT ( 'NONE',  ( 48.66127576079219352, 22.44898377099470110, -53.72649052181260032 ) ) ;
#29811 = CARTESIAN_POINT ( 'NONE',  ( 59.28329934267080148, -2.939009483360070174, -15.67174078617610000 ) ) ;
#29812 = CARTESIAN_POINT ( 'NONE',  ( 51.02429472136520161, -50.08032363113679963, -76.22815769145680065 ) ) ;
#29813 = CARTESIAN_POINT ( 'NONE',  ( 57.23219029305369787, -49.86398702007070227, -52.24802155864789910 ) ) ;
#29814 = VERTEX_POINT ( 'NONE', #10535 ) ;
#29815 = DIRECTION ( 'NONE',  ( 0.000000000000000000, 1.000000000000000000, 0.000000000000000000 ) ) ;
#29816 = CARTESIAN_POINT ( 'NONE',  ( 66.23540447448930024, 18.72622661238580122, -71.50000000000139266 ) ) ;
#29817 = EDGE_LOOP ( 'NONE', ( #42759, #10892, #40468, #24187, #29181, #20515 ) ) ;
#29818 = CARTESIAN_POINT ( 'NONE',  ( 12.40077350670613043, -55.44147723767447644, -75.14570525077779450 ) ) ;
#29819 = CARTESIAN_POINT ( 'NONE',  ( 9.366937397696199596, -15.61618894467949836, -28.45282021618999835 ) ) ;
#29820 = CARTESIAN_POINT ( 'NONE',  ( 8.309212758712860136, -15.01582912232649925, -35.03686929937009609 ) ) ;
#29821 = CARTESIAN_POINT ( 'NONE',  ( 13.47931665894660114, -51.05589467822899508, -21.90688212588430162 ) ) ;
#29822 = CIRCLE ( 'NONE', #29012, 6.999999999999999112 ) ;
#29823 = CARTESIAN_POINT ( 'NONE',  ( 56.90565801091290155, 19.41243383275969947, -74.14906031689440624 ) ) ;
#29824 = CARTESIAN_POINT ( 'NONE',  ( 46.35275103504449845, -52.90993241930539881, -76.14999999999999147 ) ) ;
#29825 = VERTEX_POINT ( 'NONE', #26493 ) ;
#29826 = CARTESIAN_POINT ( 'NONE',  ( 55.52096773173170163, 14.56742854200139980, -16.43721700016279996 ) ) ;
#29827 = DIRECTION ( 'NONE',  ( 1.000000000000000000, 0.000000000000000000, 0.000000000000000000 ) ) ;
#29828 = CARTESIAN_POINT ( 'NONE',  ( 56.89013221634429840, -50.62054540486399645, -53.45144266526210686 ) ) ;
#29829 = CARTESIAN_POINT ( 'NONE',  ( 52.82296810369110318, -49.70143565027870380, -48.95261578732520036 ) ) ;
#29830 = AXIS2_PLACEMENT_3D ( 'NONE', #50558, #37989, #38245 ) ;
#29831 = CARTESIAN_POINT ( 'NONE',  ( 20.49757756391890240, -10.07532225487519817, -36.55952288011869911 ) ) ;
#29832 = LINE ( 'NONE', #34277, #23104 ) ;
#29833 = ORIENTED_EDGE ( 'NONE', *, *, #15270, .F. ) ;
#29835 = EDGE_CURVE ( 'NONE', #23688, #14490, #8043, .T. ) ;
#29834 = CARTESIAN_POINT ( 'NONE',  ( 46.89990028981509340, 22.38086965127029870, -75.96273535411170030 ) ) ;
#29836 = CARTESIAN_POINT ( 'NONE',  ( 64.95336252238109864, 1.097895768572089814, -60.61330028352099930 ) ) ;
#29837 = CARTESIAN_POINT ( 'NONE',  ( 61.28085240419530066, -45.60177449860450594, -47.67834116410560341 ) ) ;
#29838 = CARTESIAN_POINT ( 'NONE',  ( 31.58225770014201572, -28.80002732851900049, -102.2016796975550079 ) ) ;
#29839 = DIRECTION ( 'NONE',  ( 0.000000000000000000, 0.000000000000000000, 1.000000000000000000 ) ) ;
#29840 = CYLINDRICAL_SURFACE ( 'NONE', #14721, 0.4999999999999982236 ) ;
#29841 = CARTESIAN_POINT ( 'NONE',  ( 71.62484648860579739, 0.9098571636355720083, -60.77008670988870165 ) ) ;
#29842 = FACE_OUTER_BOUND ( 'NONE', #34128, .T. ) ;
#29844 = CARTESIAN_POINT ( 'NONE',  ( 47.18591479748049267, -39.34332397330658182, -54.67514754180037784 ) ) ;
#29843 = CARTESIAN_POINT ( 'NONE',  ( 68.13393739845098196, -29.66618894499051962, -89.14999999951589871 ) ) ;
#29845 = CARTESIAN_POINT ( 'NONE',  ( 61.33741810518110071, 13.97252490929749946, -46.44068268147909606 ) ) ;
#29846 = CARTESIAN_POINT ( 'NONE',  ( -29.85095995338080144, 4.820344610801059915, -56.22640780866669985 ) ) ;
#29847 = ORIENTED_EDGE ( 'NONE', *, *, #23864, .T. ) ;
#29848 = CARTESIAN_POINT ( 'NONE',  ( 52.78558355087229614, -49.68653575824099988, -48.61478092265500095 ) ) ;
#29849 = VERTEX_POINT ( 'NONE', #30351 ) ;
#29850 = CARTESIAN_POINT ( 'NONE',  ( 47.23550238413793068, 8.041347586024643945, -54.68809082614725980 ) ) ;
#29851 = CARTESIAN_POINT ( 'NONE',  ( 24.04493739809674580, -15.62506615101500529, -65.79268861494041687 ) ) ;
#29852 = CARTESIAN_POINT ( 'NONE',  ( 13.64707893708750142, 19.57323805727630273, -21.56006118760380019 ) ) ;
#29853 = CARTESIAN_POINT ( 'NONE',  ( 56.70066228015040366, 14.05114599519139951, -25.36386621698419930 ) ) ;
#29854 = CARTESIAN_POINT ( 'NONE',  ( 15.71925719199229832, -8.575549838488520038, -45.93409400506989471 ) ) ;
#29855 = CARTESIAN_POINT ( 'NONE',  ( 50.77827180918709615, 19.51522592562140090, -76.14999999999999147 ) ) ;
#29856 = CARTESIAN_POINT ( 'NONE',  ( 53.31861474840820136, 18.21232818371930051, -49.05456087792640574 ) ) ;
#29857 = CARTESIAN_POINT ( 'NONE',  ( 64.91441195039588763, 1.390806392144110060, -61.03748192468240319 ) ) ;
#29858 = CARTESIAN_POINT ( 'NONE',  ( 60.45089258339159954, -45.66799363392549793, -47.18958319368170606 ) ) ;
#29859 = CARTESIAN_POINT ( 'NONE',  ( 16.13393739769620083, -15.61618894467929941, -54.64999999999999858 ) ) ;
#29860 = ORIENTED_EDGE ( 'NONE', *, *, #24455, .F. ) ;
#29861 = CARTESIAN_POINT ( 'NONE',  ( 14.53903968535739999, -22.89375691932010071, -71.63601545076220134 ) ) ;
#29862 = EDGE_CURVE ( 'NONE', #27228, #5608, #17248, .T. ) ;
#29863 = CARTESIAN_POINT ( 'NONE',  ( 73.08495881288720852, 1.096305581841150012, -68.96938879548969226 ) ) ;
#29864 = CARTESIAN_POINT ( 'NONE',  ( 13.50570672964423125, -8.124416908735485165, -81.18499873804080380 ) ) ;
#29865 = CARTESIAN_POINT ( 'NONE',  ( 72.87088340658550578, 1.369885150286800135, -62.57510434557890733 ) ) ;
#29866 = CARTESIAN_POINT ( 'NONE',  ( 10.61751707702999958, -64.82563018156609758, -18.17421237900310160 ) ) ;
#29867 = CARTESIAN_POINT ( 'NONE',  ( 71.31427394968270050, 1.395196698723390138, -61.05633982442969909 ) ) ;
#29868 = DIRECTION ( 'NONE',  ( 0.6415444970810870728, -0.4854844151940968522, 0.5939070136550171908 ) ) ;
#29869 = CARTESIAN_POINT ( 'NONE',  ( 18.20464558802392219, -7.911096944365791472, -45.37562956944282888 ) ) ;
#29870 = CARTESIAN_POINT ( 'NONE',  ( 14.36278247063658320, -9.025291760554305043, -57.86948676491621057 ) ) ;
#29871 = ORIENTED_EDGE ( 'NONE', *, *, #39671, .F. ) ;
#29872 = CARTESIAN_POINT ( 'NONE',  ( 65.00039235738410071, 1.369544300367000034, -70.36404682606520566 ) ) ;
#29873 = ORIENTED_EDGE ( 'NONE', *, *, #40742, .T. ) ;
#29874 = CARTESIAN_POINT ( 'NONE',  ( 13.81959240480470008, -51.26308380621749450, -23.06522850035179673 ) ) ;
#29875 = CARTESIAN_POINT ( 'NONE',  ( 20.71801037028389914, -10.57375650054692073, -32.18785271271227799 ) ) ;
#29876 = VERTEX_POINT ( 'NONE', #50552 ) ;
#29877 = DIRECTION ( 'NONE',  ( -0.7226652920947592706, 0.6911981449639433839, 0.000000000000000000 ) ) ;
#29878 = CYLINDRICAL_SURFACE ( 'NONE', #48643, 20.00000000000000000 ) ;
#29879 = CARTESIAN_POINT ( 'NONE',  ( 22.13942092184361954, -12.44121325561192570, -50.29796736139999069 ) ) ;
#29880 = CARTESIAN_POINT ( 'NONE',  ( 52.96724627483459358, 19.31611233144339934, -76.71296415647860556 ) ) ;
#29881 = ORIENTED_EDGE ( 'NONE', *, *, #18450, .F. ) ;
#29882 = CARTESIAN_POINT ( 'NONE',  ( 24.04493739769619864, -15.61618894467929941, -32.14999999999999858 ) ) ;
#29883 = PRODUCT_DEFINITION_SHAPE ( 'NONE', 'NONE',  #51876 ) ;
#29884 = FACE_BOUND ( 'NONE', #35512, .T. ) ;
#29885 = CARTESIAN_POINT ( 'NONE',  ( 22.90033352662897670, -15.51853657338904391, -72.44823326450749335 ) ) ;
#29886 = VECTOR ( 'NONE', #16513, 1000.000000000000000 ) ;
#29887 = CARTESIAN_POINT ( 'NONE',  ( 22.46008563728267049, -10.75448725963247476, -43.58402342215438097 ) ) ;
#29888 = CARTESIAN_POINT ( 'NONE',  ( 24.10393840806110077, -13.50389068195270070, -49.70986543667950031 ) ) ;
#29889 = CARTESIAN_POINT ( 'NONE',  ( 0.1375711481827747995, -20.72695808371032200, -34.68474920830817609 ) ) ;
#29890 = CARTESIAN_POINT ( 'NONE',  ( 44.10600500027882021, -37.93128479403036835, -69.78959966447122554 ) ) ;
#29891 = ORIENTED_EDGE ( 'NONE', *, *, #28393, .T. ) ;
#29892 = CARTESIAN_POINT ( 'NONE',  ( 18.13393739769619728, -45.61618894467940066, -35.14999999999999858 ) ) ;
#29893 = CARTESIAN_POINT ( 'NONE',  ( 13.18813369118609913, -22.45935592553379934, -42.86204958412849919 ) ) ;
#29894 = B_SPLINE_CURVE_WITH_KNOTS ( 'NONE', 3,
 ( #44387, #49369, #5598, #4809, #36765, #21554, #8488, #40449, #1655, #16596, #45428, #1396, #876, #24434, #17385, #16869 ),
 .UNSPECIFIED., .F., .F.,
 ( 4, 2, 2, 2, 2, 2, 2, 4 ),
 ( 0.000000000000000000, 2.041349754395100025, 4.374320902275210088, 5.832427869700280709, 6.561481353412809803, 7.727966927352870385, 9.594343845656959857, 11.66485573940060050 ),
 .UNSPECIFIED. ) ;
#29895 = CARTESIAN_POINT ( 'NONE',  ( 9.114425618932170181, -18.21946245242060058, -32.14999999999999858 ) ) ;
#29896 = ADVANCED_FACE ( 'NONE', ( #13874 ), #34814, .F. ) ;
#29897 = CARTESIAN_POINT ( 'NONE',  ( 14.41160410444349793, 20.07361457936550053, -75.01675372117850316 ) ) ;
#29898 = EDGE_CURVE ( 'NONE', #21076, #50035, #31758, .T. ) ;
#29899 = FACE_OUTER_BOUND ( 'NONE', #17648, .T. ) ;
#29900 = EDGE_CURVE ( 'NONE', #15981, #46925, #29832, .T. ) ;
#29901 = CARTESIAN_POINT ( 'NONE',  ( 42.61259335559390138, -45.06347766768709562, -6.251417111687170625 ) ) ;
#29902 = DIRECTION ( 'NONE',  ( 0.000000000000000000, 0.000000000000000000, -1.000000000000000000 ) ) ;
#29903 = ADVANCED_FACE ( 'NONE', ( #21971 ), #50300, .T. ) ;
#29904 = CARTESIAN_POINT ( 'NONE',  ( 7.949225475402950103, -16.61278889352830035, -48.46909979910559230 ) ) ;
#29905 = EDGE_LOOP ( 'NONE', ( #12417, #6960, #2680, #32357 ) ) ;
#29906 = CARTESIAN_POINT ( 'NONE',  ( 55.70826441393730022, -46.17759071057790266, -25.46014295398670058 ) ) ;
#29907 = CARTESIAN_POINT ( 'NONE',  ( 15.36633100619899928, -51.10785594612259786, -21.74512139207759986 ) ) ;
#29909 = CARTESIAN_POINT ( 'NONE',  ( 46.63393739769619373, -39.11086919362080039, -34.64999999999999858 ) ) ;
#29908 = CARTESIAN_POINT ( 'NONE',  ( 4.370623416934749095, 25.31564308878670033, -9.528750125106599356 ) ) ;
#29910 = CARTESIAN_POINT ( 'NONE',  ( 9.366916053341348913, -16.50183103721897737, -57.41114402924350202 ) ) ;
#29911 = DIRECTION ( 'NONE',  ( 0.000000000000000000, 0.000000000000000000, -1.000000000000000000 ) ) ;
#29912 = ORIENTED_EDGE ( 'NONE', *, *, #18378, .F. ) ;
#29913 = CARTESIAN_POINT ( 'NONE',  ( -9.520856997028319668, -43.66653613195550321, -5.779509720377040694 ) ) ;
#29914 = CARTESIAN_POINT ( 'NONE',  ( 47.47148429121339319, 23.37856424063020100, -54.78605424627399856 ) ) ;
#29915 = AXIS2_PLACEMENT_3D ( 'NONE', #36105, #28228, #44230 ) ;
#29916 = DIRECTION ( 'NONE',  ( -0.8857883891771956009, -0.4640893551880597712, 0.000000000000000000 ) ) ;
#29917 = CARTESIAN_POINT ( 'NONE',  ( 63.46499832689001153, 1.383922910988889976, -62.58539998085741018 ) ) ;
#29918 = DIRECTION ( 'NONE',  ( -0.8090169943749477843, -0.5877852522924728040, 0.000000000000000000 ) ) ;
#29919 = CARTESIAN_POINT ( 'NONE',  ( 11.82286116601290082, 33.96844483572419904, -16.82382485988169663 ) ) ;
#29920 = DIRECTION ( 'NONE',  ( 0.000000000000000000, -1.000000000000000000, 0.000000000000000000 ) ) ;
#29921 = CARTESIAN_POINT ( 'NONE',  ( 4.133937397696209715, -8.687985714403829718, -35.14999999999999858 ) ) ;
#29922 = SPHERICAL_SURFACE ( 'NONE', #20040, 3.000000000000000000 ) ;
#29923 = CARTESIAN_POINT ( 'NONE',  ( 10.61754762155600140, 33.59328422689429772, -18.17417937929459981 ) ) ;
#29924 = CIRCLE ( 'NONE', #48351, 22.00000000000000000 ) ;
#29925 = CARTESIAN_POINT ( 'NONE',  ( 52.97539169126969938, 21.03044668291709840, -54.26108799293329810 ) ) ;
#29926 = EDGE_CURVE ( 'NONE', #3031, #36842, #4857, .T. ) ;
#29927 = CARTESIAN_POINT ( 'NONE',  ( 63.51710413059809213, 1.389801772588449946, -68.87277968851719834 ) ) ;
#29928 = CARTESIAN_POINT ( 'NONE',  ( 16.13393739769620083, -15.61618894467929941, -5.690000000000000391 ) ) ;
#29929 = CARTESIAN_POINT ( 'NONE',  ( 18.13393739769620083, -32.61307204591476250, -35.10658870008960974 ) ) ;
#29930 = ORIENTED_EDGE ( 'NONE', *, *, #20225, .T. ) ;
#29931 = CARTESIAN_POINT ( 'NONE',  ( 19.95098317553492251, 23.65890106099656620, -18.38988218853045709 ) ) ;
#29932 = CARTESIAN_POINT ( 'NONE',  ( 10.48989095044620079, 31.99911048416310422, -45.62579085507780974 ) ) ;
#29933 = CARTESIAN_POINT ( 'NONE',  ( 72.60391569211400054, 1.424120032878380071, -62.14639092277510457 ) ) ;
#29934 = CARTESIAN_POINT ( 'NONE',  ( 65.89614409097049474, -31.41618784131230413, -17.15307145949229906 ) ) ;
#29935 = ORIENTED_EDGE ( 'NONE', *, *, #47508, .F. ) ;
#29936 = B_SPLINE_CURVE_WITH_KNOTS ( 'NONE', 3,
 ( #50150, #2445, #30217, #37569, #1677, #41763, #10059, #45964, #46494, #14247, #6645, #18428, #45448, #38354, #5867, #18173, #26019, #21834, #29693, #42032, #42291, #9550, #22607, #45703, #46234, #30473, #6390, #37841, #29951, #25501, #6131, #10322, #49897, #22088, #21572, #5618, #10583, #1934, #26540, #17664, #38101, #13992, #49648, #13739, #9805, #25753, #17916, #33886, #34140, #22350, #34401, #50417, #42554, #19719, #19200, #39388, #15788, #34924, #15539, #39136, #23627, #42815, #47265, #31491, #23118, #23365, #47516, #43069, #51694, #38881, #18687, #11101, #47770, #7931, #31746, #39643, #11353, #11876, #10839, #35710, #27832, #50667, #43831, #26803, #3749, #11611, #15020, #34661, #27575, #30987, #43579, #3228, #3492, #2970, #15283, #38623, #7680, #18944, #35185, #51188, #2714, #50923, #47013, #14762, #27064, #30731, #43325, #31237, #46757, #7165, #6911, #27318, #22860, #7419, #19460, #35445, #51443, #20736, #24913, #827, #8188, #24130, #36723, #20219, #40925, #8448, #24394, #33043, #40408, #4766, #16299, #4249, #39904, #74, #36460, #44866, #36996, #5037, #16047, #45121, #32255, #44599, #4502, #8704, #49068, #8969 ),
 .UNSPECIFIED., .F., .F.,
 ( 4, 2, 2, 2, 2, 2, 2, 2, 1, 2, 2, 2, 2, 2, 2, 2, 2, 1, 2, 2, 2, 2, 2, 2, 2, 2, 2, 1, 2, 2, 2, 2, 2, 2, 2, 2, 2, 2, 2, 2, 2, 2, 2, 2, 2, 2, 2, 2, 1, 2, 2, 2, 2, 1, 1, 2, 2, 2, 2, 2, 1, 1, 2, 2, 2, 2, 1, 2, 2, 2, 2, 2, 2, 2, 1, 2, 2, 4 ),
 ( 0.000000000000000000, 0.03125000000001593170, 0.04687500000002425837, 0.05468750000002842171, 0.05859375000003026746, 0.06250000000003211320, 0.09375000000004794776, 0.1093750000000559414, 0.1171875000000599382, 0.1210937500000619366, 0.1250000000000639211, 0.1562500000000854872, 0.1718750000000967004, 0.1796875000001026401, 0.1875000000001085521, 0.2187500000001322553, 0.2343750000001444678, 0.2421875000001501577, 0.2460937500001528777, 0.2500000000001555978, 0.2812500000001789124, 0.2968750000001905143, 0.3046875000001968981, 0.3085937500002001177, 0.3125000000002033373, 0.3437500000002295386, 0.3593750000002427503, 0.3671875000002494116, 0.3710937500002527423, 0.3750000000002560729, 0.4062500000002683964, 0.4218750000002753353, 0.4296875000002787215, 0.4335937500002811085, 0.4375000000002834954, 0.4687500000002967626, 0.4843750000003033684, 0.4921875000003056999, 0.5000000000003080869, 0.5312500000003175238, 0.5468750000003227418, 0.5625000000003280709, 0.5937500000003388401, 0.6093750000003441691, 0.6250000000003496092, 0.6562500000003629319, 0.6718750000003695932, 0.6796875000003735900, 0.6835937500003755884, 0.6855468750003766987, 0.6875000000003778089, 0.7187500000003954614, 0.7343750000004034550, 0.7421875000004075629, 0.7460937500004085621, 0.7480468750004091172, 0.7500000000004096723, 0.7812500000003940182, 0.7968750000003855805, 0.8046875000003813616, 0.8085937500003786971, 0.8105468750003768097, 0.8115234375003753664, 0.8125000000003738121, 0.8437500000003221867, 0.8593750000002956524, 0.8671875000002816636, 0.8710937500002746692, 0.8730468750002721157, 0.8740234375002708944, 0.8750000000002695622, 0.9062500000001992850, 0.9218750000001649791, 0.9296875000001472156, 0.9335937500001383338, 0.9355468750001344480, 0.9375000000001305622, 1.000000000000000000 ),
 .UNSPECIFIED. ) ;
#29937 = CARTESIAN_POINT ( 'NONE',  ( 14.34417029198879945, -52.11618894467940066, -21.14999999999999858 ) ) ;
#29938 = ORIENTED_EDGE ( 'NONE', *, *, #39124, .T. ) ;
#29939 = VERTEX_POINT ( 'NONE', #10203 ) ;
#29940 = CARTESIAN_POINT ( 'NONE',  ( 48.63696446388820505, 22.87845126040220123, -55.31022682284890379 ) ) ;
#29941 = DIRECTION ( 'NONE',  ( 1.147431558122957675E-27, 2.220771714818679968E-11, -1.000000000000000000 ) ) ;
#29942 = B_SPLINE_CURVE_WITH_KNOTS ( 'NONE', 3,
 ( #27299, #11078, #27553, #39625 ),
 .UNSPECIFIED., .F., .F.,
 ( 4, 4 ),
 ( 0.000000000000000000, 0.1924323111301881328 ),
 .UNSPECIFIED. ) ;
#29943 = ORIENTED_EDGE ( 'NONE', *, *, #49162, .F. ) ;
#29944 = CARTESIAN_POINT ( 'NONE',  ( 11.22793056427740055, -64.23882544888471102, -44.76071414201179977 ) ) ;
#29945 = CARTESIAN_POINT ( 'NONE',  ( 57.18966657269059795, -45.47098121815820093, -26.05770951134740088 ) ) ;
#29946 = CARTESIAN_POINT ( 'NONE',  ( 17.01971542465727438, -22.38319182777647143, -44.91117421213777305 ) ) ;
#29947 = CARTESIAN_POINT ( 'NONE',  ( 24.04521450903870061, -15.61618868716203501, -63.50766715510244609 ) ) ;
#29948 = CYLINDRICAL_SURFACE ( 'NONE', #11727, 7.910999999999997812 ) ;
#29949 = EDGE_LOOP ( 'NONE', ( #40059, #4108, #10769, #21064, #14869, #44455, #50779 ) ) ;
#29950 = EDGE_CURVE ( 'NONE', #12868, #48498, #26419, .T. ) ;
#29951 = CARTESIAN_POINT ( 'NONE',  ( 46.02161178372806916, 6.923385635729644605, -60.21157151071680858 ) ) ;
#29952 = ORIENTED_EDGE ( 'NONE', *, *, #37487, .F. ) ;
#29953 = CARTESIAN_POINT ( 'NONE',  ( 45.70938948723410533, -45.91915171081740255, -9.310335717235579622 ) ) ;
#29954 = CARTESIAN_POINT ( 'NONE',  ( 8.222623404330700936, -15.61601543569009820, -34.79233150823699816 ) ) ;
#29955 = CARTESIAN_POINT ( 'NONE',  ( 16.36412298844330238, 19.86444457474319947, -20.14982337726289785 ) ) ;
#29956 = DIRECTION ( 'NONE',  ( 0.000000000000000000, 0.000000000000000000, -1.000000000000000000 ) ) ;
#29957 = CARTESIAN_POINT ( 'NONE',  ( 16.13393739769620083, -15.61618894467929941, -54.64999999999999858 ) ) ;
#29958 = CARTESIAN_POINT ( 'NONE',  ( 46.67460823329760444, -53.58126690376659695, -76.01632185952030341 ) ) ;
#29959 = CARTESIAN_POINT ( 'NONE',  ( 66.90311506357139137, 12.17475057385900072, -10.97232589725430074 ) ) ;
#29960 = AXIS2_PLACEMENT_3D ( 'NONE', #10775, #50351, #38291 ) ;
#29961 = CARTESIAN_POINT ( 'NONE',  ( 50.52803994521560327, -50.37895321258069714, -76.14999999999999147 ) ) ;
#29962 = CARTESIAN_POINT ( 'NONE',  ( 30.13393739769619728, 7.383811055320659733, -84.65000000000000568 ) ) ;
#29963 = EDGE_CURVE ( 'NONE', #51314, #48585, #37459, .T. ) ;
#29964 = EDGE_CURVE ( 'NONE', #24962, #35625, #44875, .T. ) ;
#29965 = CARTESIAN_POINT ( 'NONE',  ( 68.13393739769620083, 0.8838110553206759423, -65.65000000000000568 ) ) ;
#29966 = CARTESIAN_POINT ( 'NONE',  ( 59.52731112870050367, 14.05929059590050123, -26.49927307267730114 ) ) ;
#29967 = ADVANCED_FACE ( 'NONE', ( #10720 ), #2079, .T. ) ;
#29968 = CARTESIAN_POINT ( 'NONE',  ( 23.90530189779430259, -14.52410745055090047, -77.24306566573919497 ) ) ;
#29969 = ORIENTED_EDGE ( 'NONE', *, *, #17194, .F. ) ;
#29970 = CARTESIAN_POINT ( 'NONE',  ( -19.86606260230379917, -15.61618894467933671, -21.14999999999999858 ) ) ;
#29971 = CARTESIAN_POINT ( 'NONE',  ( -10.98534442662180055, -42.03317511222970637, -5.475918862938390141 ) ) ;
#29972 = CYLINDRICAL_SURFACE ( 'NONE', #24485, 0.4999999999999980571 ) ;
#29973 = CARTESIAN_POINT ( 'NONE',  ( 72.88952751928479756, 0.9755120847786619143, -69.30957930923889876 ) ) ;
#29974 = CARTESIAN_POINT ( 'NONE',  ( 19.55709641456319403, -55.46944509157171410, -75.54041227948108883 ) ) ;
#29975 = DIRECTION ( 'NONE',  ( 0.6676418852213139576, 0.2329255526947012489, -0.7071067811865460184 ) ) ;
#29976 = CARTESIAN_POINT ( 'NONE',  ( 18.20456863547079962, -7.911075193718300369, -43.09096072954493906 ) ) ;
#29977 = CARTESIAN_POINT ( 'NONE',  ( 42.78269188002550294, 11.47418234317799879, -3.305184689555149991 ) ) ;
#29978 = CARTESIAN_POINT ( 'NONE',  ( 65.11747358718560008, 1.386342629514219826, -70.29952392096339508 ) ) ;
#29979 = CARTESIAN_POINT ( 'NONE',  ( 9.895693118437540292, -53.60956520270919867, -34.65000333313919612 ) ) ;
#29980 = DIRECTION ( 'NONE',  ( 1.000000000000000000, 0.000000000000000000, 0.000000000000000000 ) ) ;
#29981 = CARTESIAN_POINT ( 'NONE',  ( 22.90093474979461519, -15.62310337989116249, -62.45315357117970478 ) ) ;
#29983 = EDGE_CURVE ( 'NONE', #29692, #11865, #6527, .T. ) ;
#29982 = CARTESIAN_POINT ( 'NONE',  ( -1.120159439602289808, -49.66006368695019546, -9.067476037955330526 ) ) ;
#29984 = ORIENTED_EDGE ( 'NONE', *, *, #23679, .F. ) ;
#29985 = CARTESIAN_POINT ( 'NONE',  ( 9.798314152055999315, -19.53621093793969976, -53.89097489251149398 ) ) ;
#29986 = CARTESIAN_POINT ( 'NONE',  ( 63.60599763288880837, 1.030858001320269945, -61.71223682590910187 ) ) ;
#29987 = VERTEX_POINT ( 'NONE', #17546 ) ;
#29988 = CARTESIAN_POINT ( 'NONE',  ( 10.81033552764291272, 32.22462020258605264, -23.82639812994671402 ) ) ;
#29989 = DIRECTION ( 'NONE',  ( 0.6888026391158250661, 0.7071067811865571207, 0.1598465650148950534 ) ) ;
#29990 = CARTESIAN_POINT ( 'NONE',  ( 9.366376358913971245, -15.61615244833809868, -75.84717978381000592 ) ) ;
#29991 = VECTOR ( 'NONE', #48873, 1000.000000000000000 ) ;
#29992 = DIRECTION ( 'NONE',  ( 0.000000000000000000, 0.000000000000000000, 1.000000000000000000 ) ) ;
#29994 = CARTESIAN_POINT ( 'NONE',  ( 16.13393739769620083, -15.61618894467929941, 4.349999999999999645 ) ) ;
#29993 = CARTESIAN_POINT ( 'NONE',  ( 43.85570627947347333, 8.710526304754909077, -67.35765774891521573 ) ) ;
#29995 = AXIS2_PLACEMENT_3D ( 'NONE', #40586, #4945, #20920 ) ;
#29996 = CARTESIAN_POINT ( 'NONE',  ( 9.231727895759359370, -16.96735512897419795, -81.23899999999999011 ) ) ;
#29997 = CARTESIAN_POINT ( 'NONE',  ( 22.90111010729205177, -15.61618905465553553, -68.45282213299155671 ) ) ;
#29998 = ORIENTED_EDGE ( 'NONE', *, *, #3366, .T. ) ;
#29999 = ORIENTED_EDGE ( 'NONE', *, *, #21617, .T. ) ;
#30000 = VERTEX_POINT ( 'NONE', #49531 ) ;
#30001 = CARTESIAN_POINT ( 'NONE',  ( 61.21388880716399683, -45.26823853505940320, -46.65571761428090269 ) ) ;
#30002 = CARTESIAN_POINT ( 'NONE',  ( 52.97643284592769675, -49.63320651957250362, -49.06923426146740042 ) ) ;
#30003 = CARTESIAN_POINT ( 'NONE',  ( 17.89246938939507103, 10.62527906362202756, -34.70142521051214857 ) ) ;
#30004 = DIRECTION ( 'NONE',  ( -0.8660254037844390407, -0.4999999999999995004, -5.551115123125774074E-17 ) ) ;
#30005 = ADVANCED_FACE ( 'NONE', ( #34024 ), #2598, .T. ) ;
#30006 = EDGE_LOOP ( 'NONE', ( #49987, #48661, #33691, #28928 ) ) ;
#30007 = ORIENTED_EDGE ( 'NONE', *, *, #32623, .F. ) ;
#30008 = CARTESIAN_POINT ( 'NONE',  ( 12.72585596997502577, -21.52904951597577465, -73.11944019431979314 ) ) ;
#30009 = ADVANCED_FACE ( 'NONE', ( #38239 ), #2332, .T. ) ;
#30010 = DIRECTION ( 'NONE',  ( 0.000000000000000000, 0.000000000000000000, -1.000000000000000000 ) ) ;
#30011 = CYLINDRICAL_SURFACE ( 'NONE', #46897, 3.500000000000003109 ) ;
#30012 = ORIENTED_EDGE ( 'NONE', *, *, #4174, .F. ) ;
#30013 = LINE ( 'NONE', #14052, #3274 ) ;
#30014 = CARTESIAN_POINT ( 'NONE',  ( 52.76002515207090937, -50.82837137994670229, -76.29651900278329890 ) ) ;
#30015 = CARTESIAN_POINT ( 'NONE',  ( 61.06275439614230294, 14.21153323506290000, -47.36994811082230683 ) ) ;
#30016 = CARTESIAN_POINT ( 'NONE',  ( 9.121612794133520552, -12.09283099439219988, -71.16070186438049916 ) ) ;
#30017 = PLANE ( 'NONE',  #7990 ) ;
#30018 = CARTESIAN_POINT ( 'NONE',  ( 41.59981129736410566, 13.80564489721079902, -5.840260397566160222 ) ) ;
#30019 = CARTESIAN_POINT ( 'NONE',  ( 41.15934782240720580, -44.50582977593190037, -4.800414935823390294 ) ) ;
#30020 = LINE ( 'NONE', #9618, #47127 ) ;
#30021 = DIRECTION ( 'NONE',  ( 1.000000000000000000, 0.000000000000000000, 0.000000000000000000 ) ) ;
#30022 = ADVANCED_FACE ( 'NONE', ( #43717 ), #42953, .T. ) ;
#30023 = CIRCLE ( 'NONE', #34210, 3.000000000000000000 ) ;
#30024 = CARTESIAN_POINT ( 'NONE',  ( 64.60839616882741154, 0.9151442779661249638, -70.50513874227569033 ) ) ;
#30025 = CARTESIAN_POINT ( 'NONE',  ( 16.13393739769620083, -15.61618894467929941, -28.45282021618999835 ) ) ;
#30026 = AXIS2_PLACEMENT_3D ( 'NONE', #9730, #46683, #50347 ) ;
#30027 = CARTESIAN_POINT ( 'NONE',  ( 11.63393739769600010, 10.38381105532060111, -35.14999999999999858 ) ) ;
#30028 = EDGE_CURVE ( 'NONE', #40719, #42065, #16315, .T. ) ;
#30029 = ORIENTED_EDGE ( 'NONE', *, *, #31022, .F. ) ;
#30030 = CARTESIAN_POINT ( 'NONE',  ( 15.05440318628160057, -53.11618894467930119, -76.14999999999999147 ) ) ;
#30031 = CARTESIAN_POINT ( 'NONE',  ( 57.28516360415049746, 19.36107379616109725, -53.60266086058560120 ) ) ;
#30032 = UNCERTAINTY_MEASURE_WITH_UNIT (LENGTH_MEASURE( 1.000000000000000082E-05 ), #38433, 'distance_accuracy_value', 'NONE');
#30033 = CARTESIAN_POINT ( 'NONE',  ( 29.13393739769619728, -33.11618894467940066, -53.85091742636659973 ) ) ;
#30034 = FACE_OUTER_BOUND ( 'NONE', #28940, .T. ) ;
#30035 = CARTESIAN_POINT ( 'NONE',  ( 9.205734167420699166, -27.61618894467930119, -32.14999999999999858 ) ) ;
#30036 = CARTESIAN_POINT ( 'NONE',  ( 63.46499832688989784, 1.383922910988889976, -68.71460001914260829 ) ) ;
#30037 = CARTESIAN_POINT ( 'NONE',  ( 47.95926718124390220, -54.39950235201539641, -55.26638612347959878 ) ) ;
#30038 = CARTESIAN_POINT ( 'NONE',  ( 15.23033464293179584, -7.689033395369536450, -44.97182431223551191 ) ) ;
#30039 = CARTESIAN_POINT ( 'NONE',  ( 56.48879402914250392, 19.47930851033790134, -53.39119800914449598 ) ) ;
#30040 = CARTESIAN_POINT ( 'NONE',  ( 48.03761785762620207, 23.05233837423439880, -54.73540592323089982 ) ) ;
#30041 = ORIENTED_EDGE ( 'NONE', *, *, #41194, .F. ) ;
#30042 = CARTESIAN_POINT ( 'NONE',  ( 12.59310188071810011, -21.71578262099550116, -69.51459820258429545 ) ) ;
#30043 = VERTEX_POINT ( 'NONE', #47149 ) ;
#30044 = DIRECTION ( 'NONE',  ( 0.000000000000000000, 1.000000000000000000, 0.000000000000000000 ) ) ;
#30045 = CARTESIAN_POINT ( 'NONE',  ( 83.95017420394412966, 13.51629706050414370, -47.46180916972096497 ) ) ;
#30046 = CARTESIAN_POINT ( 'NONE',  ( 22.46011261673628923, -10.75452470914569680, -77.58399569109577953 ) ) ;
#30048 = CARTESIAN_POINT ( 'NONE',  ( 54.39509416807689490, 16.57266139559970242, -25.91861715551289791 ) ) ;
#30047 = CARTESIAN_POINT ( 'NONE',  ( 83.58549413295790487, 13.67911557097859898, -47.23752224019400359 ) ) ;
#30049 = CARTESIAN_POINT ( 'NONE',  ( 14.50967856369199893, -8.752928645318320378, -75.87884994711791364 ) ) ;
#30050 = CARTESIAN_POINT ( 'NONE',  ( 19.26373325286787974, -49.37472093637801862, -34.70142521051216988 ) ) ;
#30051 = CARTESIAN_POINT ( 'NONE',  ( 24.04460909154476056, -15.61619055174803172, -33.79232989763376338 ) ) ;
#30052 = CARTESIAN_POINT ( 'NONE',  ( 22.04683993050034374, -19.02419775999589646, -40.61945535750037095 ) ) ;
#30053 = ORIENTED_EDGE ( 'NONE', *, *, #6557, .T. ) ;
#30054 = LINE ( 'NONE', #34241, #21414 ) ;
#30055 = ORIENTED_EDGE ( 'NONE', *, *, #10133, .T. ) ;
#30056 = EDGE_LOOP ( 'NONE', ( #48395, #619, #26013, #19774 ) ) ;
#30057 = CARTESIAN_POINT ( 'NONE',  ( 12.21895752911560074, -64.97095625756598736, -16.28177273609240316 ) ) ;
#30058 = CARTESIAN_POINT ( 'NONE',  ( 54.71777383033455777, 14.38501790966102867, -15.43675659586341453 ) ) ;
#30059 = CIRCLE ( 'NONE', #20035, 9.000000000000007105 ) ;
#30060 = CARTESIAN_POINT ( 'NONE',  ( 22.04685682393931145, -19.02416559795394946, -54.61948950468019603 ) ) ;
#30061 = CARTESIAN_POINT ( 'NONE',  ( 51.02533507254145206, 3.943601052197206247, -76.41499684325680164 ) ) ;
#30062 = AXIS2_PLACEMENT_3D ( 'NONE', #15744, #47722, #11826 ) ;
#30063 = ORIENTED_EDGE ( 'NONE', *, *, #23506, .T. ) ;
#30064 = EDGE_CURVE ( 'NONE', #46545, #23421, #42366, .T. ) ;
#30065 = VECTOR ( 'NONE', #8221, 1000.000000000000000 ) ;
#30066 = ORIENTED_EDGE ( 'NONE', *, *, #27906, .T. ) ;
#30067 = CARTESIAN_POINT ( 'NONE',  ( -1.534588559015300113, -50.44432100765110505, -36.31182994165819622 ) ) ;
#30068 = CARTESIAN_POINT ( 'NONE',  ( 56.91934464985369857, 14.71809440041320016, -26.24570009089640266 ) ) ;
#30069 = EDGE_CURVE ( 'NONE', #40977, #33168, #51740, .T. ) ;
#30070 = AXIS2_PLACEMENT_3D ( 'NONE', #7915, #3986, #48009 ) ;
#30071 = CARTESIAN_POINT ( 'NONE',  ( 52.58213039568269664, 18.91034102909139847, -49.81669729888150044 ) ) ;
#30072 = CARTESIAN_POINT ( 'NONE',  ( 64.86720007709558899, -0.7199623700256880809, -16.56806548657110412 ) ) ;
#30073 = CARTESIAN_POINT ( 'NONE',  ( 51.01628730930330136, -50.56319388302789974, -76.16510841824720046 ) ) ;
#30074 = EDGE_CURVE ( 'NONE', #15142, #12924, #39397, .T. ) ;
#30075 = CARTESIAN_POINT ( 'NONE',  ( 58.34741903115999406, -49.12389367403579854, -51.52204152293429473 ) ) ;
#30076 =( BOUNDED_CURVE ( )  B_SPLINE_CURVE ( 3, ( #12584, #3954, #28547, #8393 ),
 .UNSPECIFIED., .F., .T. ) 
 B_SPLINE_CURVE_WITH_KNOTS ( ( 4, 4 ),
 ( 1.570796326794903441, 2.356194490192073943 ),
 .UNSPECIFIED. ) 
 CURVE ( )  GEOMETRIC_REPRESENTATION_ITEM ( )  RATIONAL_B_SPLINE_CURVE ( ( 1.000000000000000000, 0.9492530216742265381, 0.9492530216742265381, 1.000000000000000000 ) ) 
 REPRESENTATION_ITEM ( '' )  );
#30077 = VERTEX_POINT ( 'NONE', #50810 ) ;
#30078 = CARTESIAN_POINT ( 'NONE',  ( 68.13393739769618662, -29.66618894467940137, -65.65000000000000568 ) ) ;
#30079 = CARTESIAN_POINT ( 'NONE',  ( 8.222963495597628736, -16.65192748015167723, -48.75066492484217662 ) ) ;
#30080 = ORIENTED_EDGE ( 'NONE', *, *, #21442, .T. ) ;
#30081 = CARTESIAN_POINT ( 'NONE',  ( 56.46551567295650642, -50.77616483221130750, -74.14999999999999147 ) ) ;
#30082 = CARTESIAN_POINT ( 'NONE',  ( 51.63377760598070410, -45.11618894467940066, -11.44539556650109979 ) ) ;
#30083 = CARTESIAN_POINT ( 'NONE',  ( 10.97867031235510105, -21.53311119111619831, -40.74063233595069988 ) ) ;
#30084 = CARTESIAN_POINT ( 'NONE',  ( 14.18741021285519999, -51.10643937792600155, -22.27245518747690056 ) ) ;
#30085 = CARTESIAN_POINT ( 'NONE',  ( 56.95199362970870283, 19.39688504427079963, -74.60677458063500467 ) ) ;
#30086 = CARTESIAN_POINT ( 'NONE',  ( 47.46019987341419721, -54.30427659254309702, -75.17791912558919876 ) ) ;
#30087 = EDGE_LOOP ( 'NONE', ( #49898, #1631, #9451, #23513, #51043, #44303, #33800, #9147, #50915, #49043, #13434, #5395, #34278, #38783, #6633, #14629, #39138, #10235, #4479, #3597, #48330, #21005, #23354 ) ) ;
#30088 = CARTESIAN_POINT ( 'NONE',  ( 55.68942512253350685, 14.36557237263189890, -16.32472732305740237 ) ) ;
#30089 = CARTESIAN_POINT ( 'NONE',  ( 9.367214120893741836, -15.15805200183645951, -77.86872148764932433 ) ) ;
#30090 = CARTESIAN_POINT ( 'NONE',  ( 57.34839258938159645, -50.23817553046570339, -52.73846305559919756 ) ) ;
#30091 = CARTESIAN_POINT ( 'NONE',  ( 16.46289132105319908, -8.571024043077699162, -40.36203157117240181 ) ) ;
#30092 = CARTESIAN_POINT ( 'NONE',  ( 19.02084999298380197, -9.181261218463509621, -44.48141598648069106 ) ) ;
#30093 = EDGE_CURVE ( 'NONE', #48924, #336, #14900, .T. ) ;
#30094 = CARTESIAN_POINT ( 'NONE',  ( 46.37667707902559755, 21.71256252826200139, -76.14999999999999147 ) ) ;
#30095 = CARTESIAN_POINT ( 'NONE',  ( 65.23632417210509971, 1.383928098097870096, -60.96256459357869772 ) ) ;
#30096 =( REPRESENTATION_RELATIONSHIP ('NONE','NONE', #29764, #19070 ) REPRESENTATION_RELATIONSHIP_WITH_TRANSFORMATION ( #2522 )SHAPE_REPRESENTATION_RELATIONSHIP( ) );
#30097 = AXIS2_PLACEMENT_3D ( 'NONE', #25561, #41567, #42089 ) ;
#30098 = CARTESIAN_POINT ( 'NONE',  ( 75.27858690284780607, -35.61663803900331970, -12.42467591162693807 ) ) ;
#30099 = CARTESIAN_POINT ( 'NONE',  ( 12.76222187884635240, -65.48774652861183654, -23.42344531452376799 ) ) ;
#30100 = CIRCLE ( 'NONE', #26779, 3.000000000000000888 ) ;
#30101 = CARTESIAN_POINT ( 'NONE',  ( 41.29354830052630376, -44.77576227574429879, -5.375173069188550201 ) ) ;
#30102 = CARTESIAN_POINT ( 'NONE',  ( 28.90964706005130225, -4.575559556054879629, -34.73148477628539865 ) ) ;
#30103 = CIRCLE ( 'NONE', #33471, 0.9999999999999974465 ) ;
#30104 = AXIS2_PLACEMENT_3D ( 'NONE', #36000, #117, #32049 ) ;
#30105 = CARTESIAN_POINT ( 'NONE',  ( 16.13393739846139852, -15.61618894397629909, 14.85000000048049884 ) ) ;
#30106 = CARTESIAN_POINT ( 'NONE',  ( 82.26799199803031115, 13.91172255425060023, -46.71841361690350425 ) ) ;
#30107 = CARTESIAN_POINT ( 'NONE',  ( 0.01417123839112280001, 19.49180391766380183, -34.75417992180849325 ) ) ;
#30109 = CARTESIAN_POINT ( 'NONE',  ( 42.10077372231668846, -38.84036518154631068, -79.87212092322644708 ) ) ;
#30108 = DIRECTION ( 'NONE',  ( 0.2260571801428161443, -2.775557561562891351E-17, -0.9741140340359945027 ) ) ;
#30110 = AXIS2_PLACEMENT_3D ( 'NONE', #14938, #42994, #39062 ) ;
#30111 = CYLINDRICAL_SURFACE ( 'NONE', #6791, 0.4999999999999994449 ) ;
#30112 = CARTESIAN_POINT ( 'NONE',  ( -12.01951210174030038, 24.16090772189719971, -51.29522465964500100 ) ) ;
#30113 = EDGE_LOOP ( 'NONE', ( #13422, #2770, #48322, #42866 ) ) ;
#30114 = CARTESIAN_POINT ( 'NONE',  ( 52.72967167102660113, -49.72828118800889996, -48.70010208928940187 ) ) ;
#30115 = VERTEX_POINT ( 'NONE', #31634 ) ;
#30116 = CARTESIAN_POINT ( 'NONE',  ( 72.07723754518156056, -8.533442488085691835, -19.87883576049206980 ) ) ;
#30117 = CARTESIAN_POINT ( 'NONE',  ( 53.65234805279081343, -51.32547278899044585, -75.57542635131952125 ) ) ;
#30118 = CARTESIAN_POINT ( 'NONE',  ( 13.86586360781780058, 20.00433391931990101, -22.87017487063610233 ) ) ;
#30119 = CARTESIAN_POINT ( 'NONE',  ( 56.52818367932749766, 14.13713193161779991, -25.29323032974989971 ) ) ;
#30120 = CARTESIAN_POINT ( 'NONE',  ( 11.50083822998139915, -20.93379656453479853, -41.18095814125259579 ) ) ;
#30121 = CARTESIAN_POINT ( 'NONE',  ( 50.90852063231859859, 19.66920620538740039, -76.14999999999999147 ) ) ;
#30122 = CARTESIAN_POINT ( 'NONE',  ( 53.35900413950319887, 18.24539451609189911, -49.18808545514919217 ) ) ;
#30123 = CARTESIAN_POINT ( 'NONE',  ( 64.81933968820109726, 1.186515949276290227, -60.75583815301620660 ) ) ;
#30124 = CARTESIAN_POINT ( 'NONE',  ( 16.65420337942459739, 19.88381105532299742, -15.67544741556190324 ) ) ;
#30125 = B_SPLINE_CURVE_WITH_KNOTS ( 'NONE', 3,
 ( #31303, #47583, #34986, #46817, #50986, #35776, #11163, #3557, #43899, #7994, #39966, #47332, #4061, #43648, #20027, #3815, #3292 ),
 .UNSPECIFIED., .F., .F.,
 ( 4, 2, 1, 1, 1, 1, 1, 1, 1, 2, 2, 4 ),
 ( 0.000000000000000000, 0.2499999999999136246, 0.3749999999998709921, 0.4374999999998502309, 0.4687499999998397948, 0.4843749999998340217, 0.4921874999998305800, 0.4960937499998287481, 0.4980468749998278599, 0.4990234374998280265, 0.4999999999998281375, 1.000000000000000000 ),
 .UNSPECIFIED. ) ;
#30126 = EDGE_LOOP ( 'NONE', ( #40643, #49055, #5010, #37823 ) ) ;
#30127 = CARTESIAN_POINT ( 'NONE',  ( 23.35600429417859658, -18.68677486991650483, -35.41547006414829468 ) ) ;
#30128 = CARTESIAN_POINT ( 'NONE',  ( 72.98101631171969927, 1.187931651339009909, -69.04190732916428885 ) ) ;
#30129 = CARTESIAN_POINT ( 'NONE',  ( 11.19961559249191652, 34.01497085325235759, -22.25048313876769868 ) ) ;
#30130 = CARTESIAN_POINT ( 'NONE',  ( 72.78346131865960444, 1.386342629514219826, -62.63353618948930546 ) ) ;
#30131 = CARTESIAN_POINT ( 'NONE',  ( 11.75081654933170050, -65.42392464281880393, -18.04875625368890013 ) ) ;
#30132 = CARTESIAN_POINT ( 'NONE',  ( 71.37283554222209148, 1.371509258145880095, -60.97885864891310348 ) ) ;
#30133 = CARTESIAN_POINT ( 'NONE',  ( 22.90105422030644533, -15.61618894250064571, -66.84718200393152188 ) ) ;
#30134 = CARTESIAN_POINT ( 'NONE',  ( 17.16950835854344248, -7.705192299006624168, -45.33396173990814049 ) ) ;
#30135 = LINE ( 'NONE', #46158, #30183 ) ;
#30136 = CARTESIAN_POINT ( 'NONE',  ( 64.82950905750199411, 0.9955677559369519036, -70.64918477200470193 ) ) ;
#30137 = VERTEX_POINT ( 'NONE', #51328 ) ;
#30138 = CARTESIAN_POINT ( 'NONE',  ( 9.737942574377051130, -63.22272823571240252, -46.29781469063039623 ) ) ;
#30139 = EDGE_CURVE ( 'NONE', #45765, #22075, #23510, .T. ) ;
#30140 = DIRECTION ( 'NONE',  ( 1.000000000000000000, 5.495516945195724241E-29, 2.619602780254359830E-11 ) ) ;
#30141 = VERTEX_POINT ( 'NONE', #47653 ) ;
#30142 = CARTESIAN_POINT ( 'NONE',  ( 27.13393739752232392, -15.61618894439989980, -19.08999999999999986 ) ) ;
#30143 = DIRECTION ( 'NONE',  ( 0.000000000000000000, 0.000000000000000000, -1.000000000000000000 ) ) ;
#30144 = CARTESIAN_POINT ( 'NONE',  ( 23.04647144370960632, -19.60030011359189928, -69.67433775227239323 ) ) ;
#30145 = AXIS2_PLACEMENT_3D ( 'NONE', #10903, #19781, #14567 ) ;
#30146 = CARTESIAN_POINT ( 'NONE',  ( 52.53691732766219502, 18.94171105001880306, -76.99573695378890648 ) ) ;
#30147 = VECTOR ( 'NONE', #44525, 1000.000000000000000 ) ;
#30148 = ORIENTED_EDGE ( 'NONE', *, *, #3623, .F. ) ;
#30149 = DIRECTION ( 'NONE',  ( 0.000000000000000000, 0.000000000000000000, -1.000000000000000000 ) ) ;
#30150 = CARTESIAN_POINT ( 'NONE',  ( 29.13393739769619728, -33.11618894467940066, -34.64999999999999858 ) ) ;
#30151 = VECTOR ( 'NONE', #41033, 1000.000000000000000 ) ;
#30152 = DIRECTION ( 'NONE',  ( 0.000000000000000000, 0.000000000000000000, -1.000000000000000000 ) ) ;
#30153 = CARTESIAN_POINT ( 'NONE',  ( 23.94343616722941093, -14.32674203509526301, -43.74025135623552529 ) ) ;
#30154 = AXIS2_PLACEMENT_3D ( 'NONE', #22859, #46233, #10582 ) ;
#30155 = B_SPLINE_SURFACE_WITH_KNOTS ( 'NONE', 3, 3, ( 
 ( #32870, #37877, #17436, #29475, #2487, #46005, #33140, #30248, #49165 ),
 ( #45480, #5653, #9579, #13259, #21600, #29213, #17947, #33915, #45220 ),
 ( #9328, #14023, #49678, #10094, #41280, #37601, #42063, #13769, #45740 ),
 ( #26053, #22123, #18206, #5390, #21345, #15580, #46531, #22645, #31024 ),
 ( #42589, #23154, #42851, #11135, #47048, #18467, #50701, #14539, #34440 ),
 ( #51481, #50958, #19241, #47553, #14799, #47306, #18980, #3529, #27104 ),
 ( #10878, #15320, #15057, #7722, #23409, #19500, #31274, #43108, #51227 ),
 ( #7200, #11395, #23667, #50450, #2750, #27357, #39429, #43364, #7456 ),
 ( #38662, #39171, #35490, #31535, #34700, #30508, #11649, #27614, #3265 ),
 ( #18722, #43620, #39683, #10620, #26574, #6685, #30765, #46787, #6948 ),
 ( #26841, #22900, #38917, #35223, #3008, #34959, #40447, #36762, #24432 ),
 ( #44126, #36504, #8744, #873, #40708, #358, #48318, #23917, #11913 ),
 ( #8224, #12944, #19998, #44384, #24692, #35748, #9007, #4806, #27869 ),
 ( #16867, #20773, #12164, #112, #28900, #24950, #43870, #20257, #32042 ),
 ( #32814, #20511, #4538, #607, #44901, #7968, #12413, #48840, #3787 ),
 ( #44637, #19757, #48065, #51731, #39942, #24171, #4038, #16340, #16593 ) ),
 .UNSPECIFIED., .F., .F., .F.,
 ( 4, 2, 2, 2, 2, 2, 2, 4 ),
 ( 4, 1, 1, 1, 1, 1, 4 ),
 ( -3.203522274700000420E-05, 0.2957445120129499894, 0.5890486225480859872, 0.7853981633974479459, 0.8835729338221289808, 1.040652566501619969, 1.291979978788799999, 1.570796326794899889 ),
 ( -3.203522273900000163E-05, 0.1666666666666670182, 0.3333333333333329818, 0.5000000000000000000, 0.6666666666666670737, 0.8333333333333330373, 1.000032035222750082 ),
 .UNSPECIFIED. ) ;
#30156 = CARTESIAN_POINT ( 'NONE',  ( 9.959172811698669747, -21.08016207450399904, -52.56174695496979865 ) ) ;
#30157 = CARTESIAN_POINT ( 'NONE',  ( 9.807872731394935428, -20.47799600457528513, -48.29933544732911344 ) ) ;
#30158 = CARTESIAN_POINT ( 'NONE',  ( 45.39015875754859053, -38.08747578716207727, -63.36883525997365041 ) ) ;
#30159 = CARTESIAN_POINT ( 'NONE',  ( 0.000000000000000000, 0.000000000000000000, 0.000000000000000000 ) ) ;
#30160 = VERTEX_POINT ( 'NONE', #11759 ) ;
#30161 = ADVANCED_FACE ( 'NONE', ( #16183, #12787 ), #20359, .T. ) ;
#30162 = FACE_OUTER_BOUND ( 'NONE', #4060, .T. ) ;
#30163 = CARTESIAN_POINT ( 'NONE',  ( 11.08775496079699963, -10.13506345636259987, -43.49580103263740227 ) ) ;
#30164 = CARTESIAN_POINT ( 'NONE',  ( 10.53549630783540181, -11.50741195615269952, -32.14999999999999858 ) ) ;
#30165 = EDGE_CURVE ( 'NONE', #17783, #41343, #24273, .T. ) ;
#30166 = ADVANCED_FACE ( 'NONE', ( #36606 ), #24392, .T. ) ;
#30167 = CARTESIAN_POINT ( 'NONE',  ( 13.42257523142330200, 20.48963776793129909, -74.14994161014911356 ) ) ;
#30168 = CIRCLE ( 'NONE', #45222, 25.00000000000000000 ) ;
#30169 = CARTESIAN_POINT ( 'NONE',  ( 12.14991428949967123, -8.703604497957496022, -51.12566398032977588 ) ) ;
#30170 = CARTESIAN_POINT ( 'NONE',  ( 42.05084668997409381, -45.26056779962699750, -6.331743932908059591 ) ) ;
#30171 = CARTESIAN_POINT ( 'NONE',  ( 24.04491700689571942, -15.59675040521408818, -61.50689416717609959 ) ) ;
#30172 = CARTESIAN_POINT ( 'NONE',  ( 10.38625880047930039, -21.52778022385869860, -62.25319380417529658 ) ) ;
#30173 = EDGE_LOOP ( 'NONE', ( #20522, #12435, #38797, #5105 ) ) ;
#30174 = CARTESIAN_POINT ( 'NONE',  ( 53.05686867825300368, -49.33660682032460443, -27.09038418901580059 ) ) ;
#30175 = CARTESIAN_POINT ( 'NONE',  ( 55.22131878237419755, -50.98712927677730278, -75.19523011523990874 ) ) ;
#30177 = CARTESIAN_POINT ( 'NONE',  ( 40.79482532997379707, -39.62505393422780031, -82.14319696191608955 ) ) ;
#30176 = CARTESIAN_POINT ( 'NONE',  ( 75.47966807050509885, 12.14072485751589880, -13.40512917118210012 ) ) ;
#30178 = CARTESIAN_POINT ( 'NONE',  ( 14.34417029198869820, -49.11618894467930829, -22.49240188329099865 ) ) ;
#30179 = CYLINDRICAL_SURFACE ( 'NONE', #39001, 1.999999999999997335 ) ;
#30180 = PRODUCT_DEFINITION_FORMATION_WITH_SPECIFIED_SOURCE ( 'ANY', '', #23918, .NOT_KNOWN. ) ;
#30181 = ORIENTED_EDGE ( 'NONE', *, *, #41812, .F. ) ;
#30182 = CARTESIAN_POINT ( 'NONE',  ( -6.918095167487591013, -45.82906477882070106, -4.824152819064210895 ) ) ;
#30183 = VECTOR ( 'NONE', #5793, 1000.000000000000000 ) ;
#30184 = CARTESIAN_POINT ( 'NONE',  ( 47.50894761223599261, 23.34495395406939977, -54.68833697881660072 ) ) ;
#30185 = DIRECTION ( 'NONE',  ( 0.000000000000000000, -1.000000000000000000, 0.000000000000000000 ) ) ;
#30186 = FACE_OUTER_BOUND ( 'NONE', #29265, .T. ) ;
#30187 = CARTESIAN_POINT ( 'NONE',  ( 13.20467960049900036, 19.37200555191600060, -21.36610105499189771 ) ) ;
#30188 = CARTESIAN_POINT ( 'NONE',  ( 57.50723798014340105, 13.88381064843590096, -25.33268340738889890 ) ) ;
#30189 = VECTOR ( 'NONE', #22476, 1000.000000000000000 ) ;
#30190 = CARTESIAN_POINT ( 'NONE',  ( 12.01906023897140052, 33.99185434501800529, -16.79721265541349950 ) ) ;
#30191 = CARTESIAN_POINT ( 'NONE',  ( 16.39527617993162423, -15.42631520516813204, -24.90346750000000142 ) ) ;
#30192 = FACE_OUTER_BOUND ( 'NONE', #28027, .T. ) ;
#30193 = DIRECTION ( 'NONE',  ( 1.000000000000000000, 0.000000000000000000, 0.000000000000000000 ) ) ;
#30194 = CARTESIAN_POINT ( 'NONE',  ( 63.88393739769619373, 4.883811055320659733, -61.44999999999999574 ) ) ;
#30195 = CARTESIAN_POINT ( 'NONE',  ( 56.32938366548789588, 14.88341733999840066, -26.17484211198950206 ) ) ;
#30196 = CARTESIAN_POINT ( 'NONE',  ( 53.40578033982649941, 20.84711752906830284, -54.18098735754220030 ) ) ;
#30197 = CARTESIAN_POINT ( 'NONE',  ( 63.75227860486319997, 1.439518482450359960, -69.32544932539248350 ) ) ;
#30198 = CARTESIAN_POINT ( 'NONE',  ( 64.43393739769619799, 10.88381105532070059, -68.84999999999999432 ) ) ;
#30199 = CARTESIAN_POINT ( 'NONE',  ( 18.12828521207214294, -32.60348064536626822, -35.06583844469491851 ) ) ;
#30200 = CARTESIAN_POINT ( 'NONE',  ( 10.60479889110639995, -19.99468030008900143, -73.63398261789269839 ) ) ;
#30201 = CARTESIAN_POINT ( 'NONE',  ( 11.10570036673579963, 32.20550737558679799, -44.25861501678190280 ) ) ;
#30202 = CARTESIAN_POINT ( 'NONE',  ( 3.633937397696210159, -19.08029055981709732, -35.14999999999999858 ) ) ;
#30203 = DIRECTION ( 'NONE',  ( 0.000000000000000000, -1.000000000000000000, 0.000000000000000000 ) ) ;
#30204 = CARTESIAN_POINT ( 'NONE',  ( 17.92366930135129977, 19.88381105676229765, -74.14994299942661371 ) ) ;
#30205 = ORIENTED_EDGE ( 'NONE', *, *, #20197, .F. ) ;
#30206 = ORIENTED_EDGE ( 'NONE', *, *, #40869, .F. ) ;
#30207 = CARTESIAN_POINT ( 'NONE',  ( 48.59288953467110161, 22.89722549970059617, -55.31247818475549849 ) ) ;
#30208 = EDGE_CURVE ( 'NONE', #8932, #37620, #37142, .T. ) ;
#30209 = CARTESIAN_POINT ( 'NONE',  ( 76.49393950927560581, -3.279981714206201993, -13.20130267904146848 ) ) ;
#30210 = VERTEX_POINT ( 'NONE', #4390 ) ;
#30211 = CARTESIAN_POINT ( 'NONE',  ( 11.13305467742809896, -63.61067243011080308, -43.97199255920600081 ) ) ;
#30212 = CARTESIAN_POINT ( 'NONE',  ( 56.50520158204290055, -45.38268761669329621, -25.36340749954939966 ) ) ;
#30213 = CARTESIAN_POINT ( 'NONE',  ( 17.90516752299720338, -22.20706707859404005, -44.86950677487307360 ) ) ;
#30214 = DIRECTION ( 'NONE',  ( 0.000000000000000000, -1.000000000000000000, 0.000000000000000000 ) ) ;
#30215 = VERTEX_POINT ( 'NONE', #28487 ) ;
#30216 = CYLINDRICAL_SURFACE ( 'NONE', #50259, 2.000000000000000444 ) ;
#30217 = CARTESIAN_POINT ( 'NONE',  ( 47.04596872651796247, 7.021586061845817461, -55.08983903758259260 ) ) ;
#30218 = VERTEX_POINT ( 'NONE', #36346 ) ;
#30219 = CARTESIAN_POINT ( 'NONE',  ( 52.29741850497030242, -46.00137683757239415, -13.99733621933699901 ) ) ;
#30220 = CARTESIAN_POINT ( 'NONE',  ( 51.99322682244601168, 1.709311056957359520, -19.32981441259133604 ) ) ;
#30221 = CARTESIAN_POINT ( 'NONE',  ( 14.83504272151670023, 19.88381105148139838, -22.28508381815080241 ) ) ;
#30222 = CARTESIAN_POINT ( 'NONE',  ( 16.13393739769620083, -29.47259540523039689, -35.14999999999999858 ) ) ;
#30223 = CARTESIAN_POINT ( 'NONE',  ( 16.89924507312233715, -22.34215272261101859, -46.91676882640332735 ) ) ;
#30224 = AXIS2_PLACEMENT_3D ( 'NONE', #40317, #19625, #43234 ) ;
#30225 = LINE ( 'NONE', #41772, #18294 ) ;
#30226 = CARTESIAN_POINT ( 'NONE',  ( 47.09676272639379846, -54.20071801015340185, -75.51614565244940991 ) ) ;
#30227 = AXIS2_PLACEMENT_3D ( 'NONE', #39700, #12428, #48332 ) ;
#30228 = CARTESIAN_POINT ( 'NONE',  ( 57.97374689176790241, 13.73536417335439985, -9.618885821366971456 ) ) ;
#30229 = VECTOR ( 'NONE', #36987, 1000.000000000000114 ) ;
#30230 = ADVANCED_FACE ( 'NONE', ( #9107 ), #1823, .F. ) ;
#30231 = CARTESIAN_POINT ( 'NONE',  ( 71.33393739769628894, 1.883811055320669947, -60.94999999999999574 ) ) ;
#30232 = CARTESIAN_POINT ( 'NONE',  ( 52.82838949928990502, 19.98853424248689947, -75.91622035586969730 ) ) ;
#30233 = CARTESIAN_POINT ( 'NONE',  ( 61.36905519990600055, 13.93820976684110136, -27.72184371702499917 ) ) ;
#30234 = CARTESIAN_POINT ( 'NONE',  ( 19.04480908643419923, -23.33043247825739996, -33.89281648339959929 ) ) ;
#30235 = ORIENTED_EDGE ( 'NONE', *, *, #44062, .F. ) ;
#30236 = CARTESIAN_POINT ( 'NONE',  ( 71.33393739769628894, 10.88381105532070059, -68.84999999999999432 ) ) ;
#30237 = CARTESIAN_POINT ( 'NONE',  ( 6.289752778132990052, -60.00340137394460527, -12.93848582979680018 ) ) ;
#30238 = FACE_OUTER_BOUND ( 'NONE', #51870, .T. ) ;
#30239 = CARTESIAN_POINT ( 'NONE',  ( 72.99271684938489102, 0.9525601718070090262, -69.17051385343440018 ) ) ;
#30240 = CARTESIAN_POINT ( 'NONE',  ( 19.53299567489768407, -55.47150705052180086, -75.56421958049284626 ) ) ;
#30241 = CARTESIAN_POINT ( 'NONE',  ( -0.9360626036098995684, -15.61618894434099758, -11.12000000062922922 ) ) ;
#30242 = CARTESIAN_POINT ( 'NONE',  ( 9.807704576006088359, -10.75459764923981965, -42.71597528472769056 ) ) ;
#30243 = LINE ( 'NONE', #18715, #13126 ) ;
#30244 = CARTESIAN_POINT ( 'NONE',  ( 40.60804131356049851, 13.51331262618320039, -4.641941792357469510 ) ) ;
#30245 = CARTESIAN_POINT ( 'NONE',  ( 15.24810741696761518, -22.38318510825263274, -78.99448544486300250 ) ) ;
#30246 = CARTESIAN_POINT ( 'NONE',  ( 17.25678305769729803, 12.72875286183739973, -62.64999999999999858 ) ) ;
#30247 = CARTESIAN_POINT ( 'NONE',  ( 22.90090026390140565, -15.64040415753374269, -62.45396734492114632 ) ) ;
#30248 = CARTESIAN_POINT ( 'NONE',  ( 17.99229598226500215, -51.11618622139260282, -74.14993436883820266 ) ) ;
#30249 = DIRECTION ( 'NONE',  ( 0.000000000000000000, 1.000000000000000000, 0.000000000000000000 ) ) ;
#30250 = ORIENTED_EDGE ( 'NONE', *, *, #45125, .T. ) ;
#30251 = VECTOR ( 'NONE', #22707, 1000.000000000000000 ) ;
#30252 = CARTESIAN_POINT ( 'NONE',  ( 8.904080688170550317, -17.41504032766459886, -51.98972054698469947 ) ) ;
#30253 = CARTESIAN_POINT ( 'NONE',  ( 63.61158869431360330, 1.412203896157240068, -62.26955982508579979 ) ) ;
#30254 = EDGE_LOOP ( 'NONE', ( #2372, #42873, #37622, #18227 ) ) ;
#30255 = CARTESIAN_POINT ( 'NONE',  ( -9.494463584530519640, 12.56566348097149977, -6.502759410847990473 ) ) ;
#30256 = AXIS2_PLACEMENT_3D ( 'NONE', #12708, #40216, #7989 ) ;
#30257 = DIRECTION ( 'NONE',  ( -0.000000000000000000, 1.000000000000000000, 0.000000000000000000 ) ) ;
#30258 = CARTESIAN_POINT ( 'NONE',  ( 20.92027185089429864, -10.43607681494890116, -74.58460979065598906 ) ) ;
#30259 = CARTESIAN_POINT ( 'NONE',  ( 47.80851828325950237, -54.40380972823489714, -54.72998258637920799 ) ) ;
#30260 = CARTESIAN_POINT ( 'NONE',  ( 22.04686229628420335, -12.20822253710021954, -74.28615355936335618 ) ) ;
#30261 = CIRCLE ( 'NONE', #21879, 2.000000000000000888 ) ;
#30262 = DIRECTION ( 'NONE',  ( 0.000000000000000000, 1.000000000000000000, 0.000000000000000000 ) ) ;
#30263 = CYLINDRICAL_SURFACE ( 'NONE', #49597, 3.000000000000000444 ) ;
#30264 = VERTEX_POINT ( 'NONE', #456 ) ;
#30265 = EDGE_LOOP ( 'NONE', ( #21317, #8962, #17282, #42647 ) ) ;
#30266 = EDGE_CURVE ( 'NONE', #5215, #42606, #1705, .T. ) ;
#30267 = ORIENTED_EDGE ( 'NONE', *, *, #17254, .F. ) ;
#30268 = CARTESIAN_POINT ( 'NONE',  ( -22.62439110747796889, -19.95374504816285466, -54.65132778005098402 ) ) ;
#30269 = CARTESIAN_POINT ( 'NONE',  ( -18.93711747768801956, -32.99710777797167083, -51.50532171058987529 ) ) ;
#30270 = EDGE_CURVE ( 'NONE', #31804, #7417, #16255, .T. ) ;
#30271 = ORIENTED_EDGE ( 'NONE', *, *, #8513, .F. ) ;
#30272 = EDGE_CURVE ( 'NONE', #15078, #29389, #30168, .T. ) ;
#30273 = ORIENTED_EDGE ( 'NONE', *, *, #14293, .F. ) ;
#30274 = CARTESIAN_POINT ( 'NONE',  ( 24.04455721578320038, -15.53241555943019669, -77.50430590993917690 ) ) ;
#30275 = CARTESIAN_POINT ( 'NONE',  ( 22.72481123428762118, -17.38743319054560743, -52.53615118110773352 ) ) ;
#30276 = DIRECTION ( 'NONE',  ( 0.8660254037844387076, -0.4999999999999998890, 0.000000000000000000 ) ) ;
#30277 = ORIENTED_EDGE ( 'NONE', *, *, #11071, .F. ) ;
#30278 = CARTESIAN_POINT ( 'NONE',  ( 19.74986264806196701, -22.71836713299729027, -49.85790434740009403 ) ) ;
#30279 = CARTESIAN_POINT ( 'NONE',  ( 53.20630144999590527, -50.74234614952320044, -76.43613505561189925 ) ) ;
#30280 = CARTESIAN_POINT ( 'NONE',  ( 60.94474915215740651, 14.18121638299069964, -47.07753893340860429 ) ) ;
#30281 = EDGE_CURVE ( 'NONE', #336, #24767, #15106, .T. ) ;
#30282 = CARTESIAN_POINT ( 'NONE',  ( 23.43694177994569827, -12.74340726407310065, -69.89319896736259352 ) ) ;
#30283 = DIRECTION ( 'NONE',  ( 0.9741140340359945027, 0.000000000000000000, 0.2260571801428156169 ) ) ;
#30284 = CARTESIAN_POINT ( 'NONE',  ( 42.75215489670460300, 13.74995302045830137, -6.093637046069630081 ) ) ;
#30285 = ADVANCED_FACE ( 'NONE', ( #32924 ), #13055, .T. ) ;
#30286 = CARTESIAN_POINT ( 'NONE',  ( 40.60988568039630309, -44.69613999932960269, -4.337423926737489666 ) ) ;
#30287 = CARTESIAN_POINT ( 'NONE',  ( -13.56626582457120023, -15.61618894467929941, 7.944363289481099599 ) ) ;
#30288 = CARTESIAN_POINT ( 'NONE',  ( -9.414006712227710238, 12.57454005906549988, -5.942694572982400558 ) ) ;
#30289 = AXIS2_PLACEMENT_3D ( 'NONE', #20329, #24243, #36318 ) ;
#30290 = AXIS2_PLACEMENT_3D ( 'NONE', #2500, #6438, #13784 ) ;
#30291 = CARTESIAN_POINT ( 'NONE',  ( 64.67544096520701657, 1.230988031922719994, -70.42401535379970312 ) ) ;
#30292 = CARTESIAN_POINT ( 'NONE',  ( 46.60156948537970578, 8.729780378598791302, -54.61635207866100217 ) ) ;
#30293 = CARTESIAN_POINT ( 'NONE',  ( 11.66815189201653347, 10.43523626583280617, -34.89146800830119588 ) ) ;
#30294 = ORIENTED_EDGE ( 'NONE', *, *, #48025, .F. ) ;
#30295 = CARTESIAN_POINT ( 'NONE',  ( 14.38860766206780184, -52.17875626651990473, -75.87012052777591009 ) ) ;
#30296 = CARTESIAN_POINT ( 'NONE',  ( 57.26876238482499559, 19.38381105532069881, -53.91656696360529821 ) ) ;
#30297 = CARTESIAN_POINT ( 'NONE',  ( 44.75408132727028487, -40.01302229878363903, -63.00536423570013511 ) ) ;
#30298 = CARTESIAN_POINT ( 'NONE',  ( 11.13393739769250068, 32.42518242043740884, -43.78800781015315380 ) ) ;
#30300 = EDGE_CURVE ( 'NONE', #17232, #10891, #22424, .T. ) ;
#30299 = DIRECTION ( 'NONE',  ( 1.000000000000000000, 0.000000000000000000, 0.000000000000000000 ) ) ;
#30301 = CARTESIAN_POINT ( 'NONE',  ( 63.17939165373819321, 0.9307121176571799825, -69.03423516236559010 ) ) ;
#30302 = CARTESIAN_POINT ( 'NONE',  ( 47.97259836220649731, -54.39289801412169822, -55.19635314194069764 ) ) ;
#30303 = CARTESIAN_POINT ( 'NONE',  ( 22.90132873572047600, -15.41596929237549674, -50.83776837827166872 ) ) ;
#30304 = CARTESIAN_POINT ( 'NONE',  ( 82.13853704237929776, -45.11618894467940066, -46.37203261889099792 ) ) ;
#30305 = CARTESIAN_POINT ( 'NONE',  ( 20.11803839206749345, -22.52873026110887267, -46.12571104359029306 ) ) ;
#30306 = CARTESIAN_POINT ( 'NONE',  ( 47.78181927210629709, 23.24271050597710087, -55.19076979248089998 ) ) ;
#30307 = ORIENTED_EDGE ( 'NONE', *, *, #32241, .F. ) ;
#30308 = CARTESIAN_POINT ( 'NONE',  ( 15.47860435268529855, -22.63851745982070085, -75.37679910129230620 ) ) ;
#30309 = ORIENTED_EDGE ( 'NONE', *, *, #46802, .F. ) ;
#30310 = CARTESIAN_POINT ( 'NONE',  ( 71.29339335573889969, 1.327097482837290121, -70.45474866971780159 ) ) ;
#30311 = CARTESIAN_POINT ( 'NONE',  ( 68.13393739769618662, -2.166188944679360073, -65.65000000000000568 ) ) ;
#30312 = DIRECTION ( 'NONE',  ( -0.4107275965530814421, -0.9117581046690669266, 0.000000000000000000 ) ) ;
#30313 = CARTESIAN_POINT ( 'NONE',  ( 46.99244837402765285, 8.000249783914572532, -34.80140398659610668 ) ) ;
#30315 = CARTESIAN_POINT ( 'NONE',  ( 53.48305084018470268, 17.62635399826340077, -26.58258335482339874 ) ) ;
#30314 = CARTESIAN_POINT ( 'NONE',  ( 83.86237639949339950, 13.50615999911470055, -47.35515635286719771 ) ) ;
#30316 = CARTESIAN_POINT ( 'NONE',  ( 23.13400276341360140, -14.75500164161349836, -78.41385574115379598 ) ) ;
#30317 = CARTESIAN_POINT ( 'NONE',  ( 22.46011903968922141, -20.47784435745758458, -41.71600081988199804 ) ) ;
#30318 = CARTESIAN_POINT ( 'NONE',  ( 15.24805187626227543, -22.38317847404922034, -40.99442667353930858 ) ) ;
#30319 = ORIENTED_EDGE ( 'NONE', *, *, #43530, .F. ) ;
#30320 = CARTESIAN_POINT ( 'NONE',  ( 57.55751162087899786, 19.38381105532069881, -53.92796738110899923 ) ) ;
#30321 = EDGE_LOOP ( 'NONE', ( #2028, #32716, #25635, #18512 ) ) ;
#30322 = ORIENTED_EDGE ( 'NONE', *, *, #43013, .F. ) ;
#30323 = CARTESIAN_POINT ( 'NONE',  ( 12.30638105235980007, -64.63429039334658910, -15.85198194118579984 ) ) ;
#30324 = CARTESIAN_POINT ( 'NONE',  ( 9.366937397696199596, -15.61618894467949836, -28.45282021618999835 ) ) ;
#30325 = CARTESIAN_POINT ( 'NONE',  ( 6.293131413230796056, 33.86298889378740995, -49.18705164837358268 ) ) ;
#30326 = LINE ( 'NONE', #13342, #20824 ) ;
#30327 = AXIS2_PLACEMENT_3D ( 'NONE', #47014, #11102, #39644 ) ;
#30328 = ORIENTED_EDGE ( 'NONE', *, *, #27890, .T. ) ;
#30329 = ORIENTED_EDGE ( 'NONE', *, *, #32834, .T. ) ;
#30330 = EDGE_CURVE ( 'NONE', #20584, #31550, #2009, .T. ) ;
#30331 = CARTESIAN_POINT ( 'NONE',  ( -1.533723836532590035, -50.07764524056720035, -36.10017410556069706 ) ) ;
#30332 = DIRECTION ( 'NONE',  ( 0.000000000000000000, 1.000000000000000000, 0.000000000000000000 ) ) ;
#30333 = CARTESIAN_POINT ( 'NONE',  ( 53.22811123321509541, -49.51495811786340084, -49.13101390776430577 ) ) ;
#30334 = CARTESIAN_POINT ( 'NONE',  ( 53.11054108117379258, 18.20428406185990156, -48.75085142486800294 ) ) ;
#30335 = CARTESIAN_POINT ( 'NONE',  ( 60.30051528721210019, -2.182703807405690366, -15.82000114403490265 ) ) ;
#30336 = CARTESIAN_POINT ( 'NONE',  ( 50.91412666581710056, -49.20888781110259202, -76.31682797935179963 ) ) ;
#30337 = CARTESIAN_POINT ( 'NONE',  ( 58.51614409837979736, -48.15979427076100450, -50.25351394005609507 ) ) ;
#30338 = EDGE_LOOP ( 'NONE', ( #13230, #48652, #34357, #422 ) ) ;
#30339 = CARTESIAN_POINT ( 'NONE',  ( 16.80019542733428750, -7.709322181342847635, -33.31905990858218303 ) ) ;
#30340 = CARTESIAN_POINT ( 'NONE',  ( 70.83745409581372598, 17.98087126524719892, -68.79648330188406646 ) ) ;
#30341 = EDGE_LOOP ( 'NONE', ( #41249, #1790, #14494, #6505 ) ) ;
#30342 = CARTESIAN_POINT ( 'NONE',  ( 30.13393739769619728, -38.61618894467930119, -59.64999999999999147 ) ) ;
#30343 = CARTESIAN_POINT ( 'NONE',  ( 51.23833939979579100, -45.11618894467940066, -11.16259862828139937 ) ) ;
#30344 = CARTESIAN_POINT ( 'NONE',  ( 8.287590648356600198, -15.46925262952789915, -45.01845461338609766 ) ) ;
#30345 = CARTESIAN_POINT ( 'NONE',  ( 13.34067758125200065, -51.12402484803250502, -21.90730111293149918 ) ) ;
#30346 = CARTESIAN_POINT ( 'NONE',  ( 55.18354902960369657, 19.47151978655200111, -75.88390424252150979 ) ) ;
#30347 = CARTESIAN_POINT ( 'NONE',  ( 47.61801185652239354, -54.54486410850540068, -74.14999999999999147 ) ) ;
#30348 = CARTESIAN_POINT ( 'NONE',  ( 56.70491206796489791, 13.95151597528120035, -16.59608766374520172 ) ) ;
#30349 = CARTESIAN_POINT ( 'NONE',  ( 9.525402744584583914, -13.57718879627017117, -77.94307581219771919 ) ) ;
#30350 = CARTESIAN_POINT ( 'NONE',  ( 9.206757876277350761, -14.29076710523099969, -45.90735674562569812 ) ) ;
#30351 = CARTESIAN_POINT ( 'NONE',  ( 71.33393739769628894, 1.883811055320669947, -69.84999999999999432 ) ) ;
#30352 = ORIENTED_EDGE ( 'NONE', *, *, #265, .T. ) ;
#30353 = CARTESIAN_POINT ( 'NONE',  ( 47.30391968620829601, 22.90394248747499617, -75.47331621149830028 ) ) ;
#30354 = CARTESIAN_POINT ( 'NONE',  ( 19.91788182092076553, -54.79639948975857067, -18.20736960311763397 ) ) ;
#30355 = CARTESIAN_POINT ( 'NONE',  ( 75.20727607192908692, -32.15526784732785615, -12.07513152916334498 ) ) ;
#30356 = AXIS2_PLACEMENT_3D ( 'NONE', #19490, #47544, #4029 ) ;
#30357 = CARTESIAN_POINT ( 'NONE',  ( 104.6856170952509757, -28.80002732851738045, -102.2016796975550079 ) ) ;
#30358 = AXIS2_PLACEMENT_3D ( 'NONE', #49397, #48876, #5368 ) ;
#30359 = CARTESIAN_POINT ( 'NONE',  ( 28.78179405415149716, -4.623252633501089726, -34.67096478998279707 ) ) ;
#30360 = EDGE_CURVE ( 'NONE', #218, #21076, #29263, .T. ) ;
#30361 = DIRECTION ( 'NONE',  ( -1.000000000000000000, 0.000000000000000000, 0.000000000000000000 ) ) ;
#30363 = EDGE_CURVE ( 'NONE', #36315, #367, #10056, .T. ) ;
#30362 = CARTESIAN_POINT ( 'NONE',  ( 82.13853704237929776, 14.04924524887199944, -47.17417977903829751 ) ) ;
#30364 = CARTESIAN_POINT ( 'NONE',  ( 0.2860235532455480123, 19.98438480351800095, -34.73917836322149810 ) ) ;
#30366 = CARTESIAN_POINT ( 'NONE',  ( 42.54838292251218235, -38.91056855093247435, -77.63407492224945372 ) ) ;
#30365 = DIRECTION ( 'NONE',  ( 1.000000000000000000, 2.460964292799963328E-14, 0.000000000000000000 ) ) ;
#30367 = CARTESIAN_POINT ( 'NONE',  ( 23.84888678603816814, -13.80674682629403804, -71.43433972173403390 ) ) ;
#30368 = CARTESIAN_POINT ( 'NONE',  ( -17.48391069661260033, 19.73109819378510110, -52.50953498851649925 ) ) ;
#30369 = EDGE_CURVE ( 'NONE', #10642, #23531, #38534, .T. ) ;
#30370 = EDGE_LOOP ( 'NONE', ( #42311, #51386, #39191, #50452 ) ) ;
#30371 = CARTESIAN_POINT ( 'NONE',  ( 52.68399239296920200, -49.75584776967829725, -48.59017835746970349 ) ) ;
#30372 = ORIENTED_EDGE ( 'NONE', *, *, #15158, .F. ) ;
#30373 = CARTESIAN_POINT ( 'NONE',  ( 17.34362241395794868, 21.51730928977416468, -76.12465453342632316 ) ) ;
#30374 = CARTESIAN_POINT ( 'NONE',  ( 44.13393739769620083, -33.11618894467940066, -54.35294145922159714 ) ) ;
#30375 = CARTESIAN_POINT ( 'NONE',  ( 14.04181524467029973, 19.90302481765870013, -22.40049071566960137 ) ) ;
#30376 = CARTESIAN_POINT ( 'NONE',  ( 55.88898274229019592, 14.70399348244479931, -25.39814755123949652 ) ) ;
#30377 = CARTESIAN_POINT ( 'NONE',  ( 16.32018716749529830, -22.66656976559070102, -48.94441338548719500 ) ) ;
#30378 = CARTESIAN_POINT ( 'NONE',  ( 50.67689124139590007, 19.37866773268710219, -76.14999999999999147 ) ) ;
#30379 = CARTESIAN_POINT ( 'NONE',  ( 52.66298057413799683, 18.54726979422290256, -48.68531361618759945 ) ) ;
#30380 = CARTESIAN_POINT ( 'NONE',  ( 55.72979527423980528, -45.76347876835659889, -16.72772322675590218 ) ) ;
#30381 = CARTESIAN_POINT ( 'NONE',  ( 15.01109173769499883, -43.96113075119600211, -62.64999999999999858 ) ) ;
#30382 = CIRCLE ( 'NONE', #7811, 1.999999999999998224 ) ;
#30383 = ORIENTED_EDGE ( 'NONE', *, *, #13130, .F. ) ;
#30384 = B_SPLINE_CURVE_WITH_KNOTS ( 'NONE', 3,
 ( #36864, #963, #16960, #44990, #32908, #28991, #13038, #5681, #17720, #38158, #49706, #2511, #18231, #46295, #34196, #5421, #33943, #33689 ),
 .UNSPECIFIED., .F., .F.,
 ( 4, 2, 2, 2, 2, 2, 2, 2, 4 ),
 ( 0.000000000000000000, 0.06250019663676391335, 0.1250003932735278267, 0.1875005899102917262, 0.2500007865470556534, 0.3125009831838195806, 0.3750011798205834523, 0.4375013764573473796, 0.5000015730941113068 ),
 .UNSPECIFIED. ) ;
#30385 = CARTESIAN_POINT ( 'NONE',  ( 23.34384601745220067, -12.51716234299430042, -37.15828654754790250 ) ) ;
#30386 = CARTESIAN_POINT ( 'NONE',  ( 72.75389709491450674, 1.389468113695450091, -68.84985728199801258 ) ) ;
#30387 = CARTESIAN_POINT ( 'NONE',  ( 9.367149215637390114, 32.06395859284570804, -46.50590274904199362 ) ) ;
#30388 = CARTESIAN_POINT ( 'NONE',  ( 73.10923647485390120, 1.096036836948820037, -62.36911566638589477 ) ) ;
#30389 =( BOUNDED_CURVE ( )  B_SPLINE_CURVE ( 3, ( #24081, #48225, #24, #51646 ),
 .UNSPECIFIED., .F., .T. ) 
 B_SPLINE_CURVE_WITH_KNOTS ( ( 4, 4 ),
 ( 5.070260775219138871, 5.428132570053650241 ),
 .UNSPECIFIED. ) 
 CURVE ( )  GEOMETRIC_REPRESENTATION_ITEM ( )  RATIONAL_B_SPLINE_CURVE ( ( 1.000000000000000000, 0.9893557610490316678, 0.9893557610490316678, 1.000000000000000000 ) ) 
 REPRESENTATION_ITEM ( '' )  );
#30390 = CARTESIAN_POINT ( 'NONE',  ( 10.80633501404929930, -64.99634644860429944, -17.92671787896209779 ) ) ;
#30391 = DIRECTION ( 'NONE',  ( -7.539420000000001133E-18, 1.452687000000000165E-17, 1.000000000000000000 ) ) ;
#30392 = CARTESIAN_POINT ( 'NONE',  ( 20.97958295125081563, -21.95497548660398479, -76.08475998165809528 ) ) ;
#30393 = CARTESIAN_POINT ( 'NONE',  ( 20.11808194642809866, -8.703673674707349761, -45.45896691875083206 ) ) ;
#30394 = CARTESIAN_POINT ( 'NONE',  ( 9.543104245580357414, -13.84479575616211733, -57.53615352593524079 ) ) ;
#30395 = EDGE_LOOP ( 'NONE', ( #7819, #27188, #44746, #24079, #37567, #44708, #15141 ) ) ;
#30396 = EDGE_CURVE ( 'NONE', #3068, #26084, #45525, .T. ) ;
#30397 = CARTESIAN_POINT ( 'NONE',  ( 64.85305306408218939, 1.096036836948810045, -70.62529907715770605 ) ) ;
#30398 = ORIENTED_EDGE ( 'NONE', *, *, #16005, .T. ) ;
#30399 = CARTESIAN_POINT ( 'NONE',  ( 9.738771746928540196, -63.23098275344089814, -46.29766285214619614 ) ) ;
#30400 = AXIS2_PLACEMENT_3D ( 'NONE', #10945, #42916, #7014 ) ;
#30401 = CARTESIAN_POINT ( 'NONE',  ( 22.75768029318954788, -17.21802539889342754, -32.52852712712287797 ) ) ;
#30402 = ORIENTED_EDGE ( 'NONE', *, *, #49903, .T. ) ;
#30403 = CARTESIAN_POINT ( 'NONE',  ( 57.32592487606110154, 19.18190549473660056, -53.00067887316149751 ) ) ;
#30404 = CARTESIAN_POINT ( 'NONE',  ( 53.99792397698860213, 19.38381073495739670, -77.02993432047880162 ) ) ;
#30405 = VERTEX_POINT ( 'NONE', #13809 ) ;
#30406 = CIRCLE ( 'NONE', #37118, 2.999999999999999112 ) ;
#30407 = CYLINDRICAL_SURFACE ( 'NONE', #3198, 21.19999999999999929 ) ;
#30408 = LINE ( 'NONE', #18623, #22550 ) ;
#30409 = CARTESIAN_POINT ( 'NONE',  ( -23.86606260230380272, -15.61618894467908092, -76.14999999999999147 ) ) ;
#30410 = CARTESIAN_POINT ( 'NONE',  ( 17.73647699123689847, -32.25138633525569531, -34.65800258959610147 ) ) ;
#30411 = CARTESIAN_POINT ( 'NONE',  ( 11.47147311421140081, -22.41649385410530115, -60.48364006133179771 ) ) ;
#30412 = DIRECTION ( 'NONE',  ( 1.000000000000000000, 0.000000000000000000, 0.000000000000000000 ) ) ;
#30413 = CARTESIAN_POINT ( 'NONE',  ( 45.02782540735238115, -38.04571132974656678, -65.18055859578058175 ) ) ;
#30414 = ORIENTED_EDGE ( 'NONE', *, *, #271, .T. ) ;
#30415 = CARTESIAN_POINT ( 'NONE',  ( -22.72558660355269566, -12.37859355894351410, -54.68545204612530597 ) ) ;
#30416 = CARTESIAN_POINT ( 'NONE',  ( 8.780985052446480310, -16.81651623905879589, -59.18114938323400054 ) ) ;
#30417 = CARTESIAN_POINT ( 'NONE',  ( 53.05489980299899599, -49.59988638911210046, -49.10811587859359406 ) ) ;
#30418 = CARTESIAN_POINT ( 'NONE',  ( 9.574329378931039969, -12.95124520122079836, -32.14999999999999858 ) ) ;
#30419 = AXIS2_PLACEMENT_3D ( 'NONE', #48708, #29543, #28766 ) ;
#30420 = CARTESIAN_POINT ( 'NONE',  ( 63.88393739769619373, 11.88381105532070059, -61.34712802272770915 ) ) ;
#30421 = CARTESIAN_POINT ( 'NONE',  ( 13.58922753005830053, 20.47004600267149854, -74.90176971618339508 ) ) ;
#30422 = CARTESIAN_POINT ( 'NONE',  ( 16.13393739769620083, -15.61618894467929941, -6.649999999999999467 ) ) ;
#30423 = CARTESIAN_POINT ( 'NONE',  ( 44.42514528531739870, -45.25992823897050243, -7.504186993430459474 ) ) ;
#30424 = CARTESIAN_POINT ( 'NONE',  ( 63.78749078828948882, 1.530257664727401767, -68.84999999999999432 ) ) ;
#30425 = CARTESIAN_POINT ( 'NONE',  ( 24.08194699500409897, -13.42259277626600067, -65.42195104672009620 ) ) ;
#30426 = ORIENTED_EDGE ( 'NONE', *, *, #41417, .T. ) ;
#30427 = CARTESIAN_POINT ( 'NONE',  ( 52.89134886112609735, -49.51162219831950040, -27.21802740595560266 ) ) ;
#30428 = EDGE_CURVE ( 'NONE', #9988, #13604, #13439, .T. ) ;
#30429 = CARTESIAN_POINT ( 'NONE',  ( 54.46275104342129936, -51.12164165988440345, -75.43974601459740370 ) ) ;
#30431 = CARTESIAN_POINT ( 'NONE',  ( 41.61216686777694918, -39.72206404522755463, -78.20190362087095082 ) ) ;
#30430 = CARTESIAN_POINT ( 'NONE',  ( 9.118782003106261413, 30.73934052534850281, -13.66830718943320022 ) ) ;
#30432 = VECTOR ( 'NONE', #40201, 1000.000000000000000 ) ;
#30433 = CARTESIAN_POINT ( 'NONE',  ( -23.86606260230380272, -15.61618894467908092, -53.92777777777782688 ) ) ;
#30434 = DIRECTION ( 'NONE',  ( 0.8204012560548787913, -0.5717882292104107256, 0.000000000000000000 ) ) ;
#30435 = EDGE_CURVE ( 'NONE', #45483, #34982, #6906, .T. ) ;
#30436 = AXIS2_PLACEMENT_3D ( 'NONE', #41661, #17811, #47927 ) ;
#30437 = ORIENTED_EDGE ( 'NONE', *, *, #22096, .T. ) ;
#30438 = CARTESIAN_POINT ( 'NONE',  ( 13.96111746457373215, 21.00530369382216023, -75.65677362358476898 ) ) ;
#30439 = CARTESIAN_POINT ( 'NONE',  ( 47.53131359496729402, 23.34191863293520086, -54.78660750946839642 ) ) ;
#30440 = CARTESIAN_POINT ( 'NONE',  ( 15.08138911710155128, -7.754377985150386898, -65.24995822591438355 ) ) ;
#30441 = CARTESIAN_POINT ( 'NONE',  ( 84.32823744787019393, -43.96174957359315982, -47.43651528332460288 ) ) ;
#30442 = CARTESIAN_POINT ( 'NONE',  ( 13.33369300875940056, 19.36669572017150287, -21.35583564802480083 ) ) ;
#30443 = DIRECTION ( 'NONE',  ( -1.000000000000000000, 0.000000000000000000, 0.000000000000000000 ) ) ;
#30444 = CARTESIAN_POINT ( 'NONE',  ( 11.59391792477759964, 33.72622688432610261, -16.50763286606089864 ) ) ;
#30445 = CARTESIAN_POINT ( 'NONE',  ( 51.73429015981039925, 17.92666341930739904, -76.96796945729541051 ) ) ;
#30446 = CARTESIAN_POINT ( 'NONE',  ( 52.96856317127399905, 18.35625398511779949, -48.80184351055599734 ) ) ;
#30447 = LINE ( 'NONE', #46469, #49303 ) ;
#30448 = CARTESIAN_POINT ( 'NONE',  ( 55.65109705446129595, -48.32796235437900378, -48.64566203011980150 ) ) ;
#30449 = CARTESIAN_POINT ( 'NONE',  ( 52.83394450884049576, 18.38007605328469651, -27.67493365076309786 ) ) ;
#30450 = CARTESIAN_POINT ( 'NONE',  ( 51.27175184527400376, 21.75613229864340070, -54.61634031474230255 ) ) ;
#30451 = CARTESIAN_POINT ( 'NONE',  ( 63.57990658082609770, 1.404649297339839897, -68.94572984764299406 ) ) ;
#30452 = CARTESIAN_POINT ( 'NONE',  ( 52.56949877374420055, 18.62486692341260053, -48.49331013451849515 ) ) ;
#30453 = CARTESIAN_POINT ( 'NONE',  ( 18.11900864776890074, -32.59522544870679894, -35.02873218748179340 ) ) ;
#30454 = CARTESIAN_POINT ( 'NONE',  ( 71.18923915728029783, 1.331842543267529821, -60.79893402932049895 ) ) ;
#30455 = CARTESIAN_POINT ( 'NONE',  ( 10.76935003792520007, 31.89982618482420307, -45.20657243697100114 ) ) ;
#30456 = CARTESIAN_POINT ( 'NONE',  ( 72.68796522584510456, 1.404650034022369987, -62.35426166056780062 ) ) ;
#30457 = CARTESIAN_POINT ( 'NONE',  ( 71.33393739769628894, 11.23736444591397543, -69.70355339059327093 ) ) ;
#30458 = ORIENTED_EDGE ( 'NONE', *, *, #37214, .F. ) ;
#30459 = EDGE_CURVE ( 'NONE', #4756, #14500, #51097, .T. ) ;
#30460 = CARTESIAN_POINT ( 'NONE',  ( 12.13393739769644419, 24.18330853958552851, -74.40622738399734715 ) ) ;
#30461 = ORIENTED_EDGE ( 'NONE', *, *, #48697, .F. ) ;
#30462 = VERTEX_POINT ( 'NONE', #33448 ) ;
#30463 = CARTESIAN_POINT ( 'NONE',  ( 16.13393739769620083, -15.61618894467929941, -54.64999999999999858 ) ) ;
#30464 = EDGE_CURVE ( 'NONE', #32888, #23485, #5902, .T. ) ;
#30465 = CARTESIAN_POINT ( 'NONE',  ( 76.55776859562905656, 0.1525228172217792388, -13.47635171202204241 ) ) ;
#30466 = ORIENTED_EDGE ( 'NONE', *, *, #19457, .F. ) ;
#30467 = CARTESIAN_POINT ( 'NONE',  ( 12.31664178984540037, -65.34953336804649382, -46.39762368350670130 ) ) ;
#30468 = CARTESIAN_POINT ( 'NONE',  ( 57.59886637785189833, -45.11801559808479567, -25.34084472867580118 ) ) ;
#30469 = CARTESIAN_POINT ( 'NONE',  ( 22.90093737940656027, -16.50198913682855562, -44.49448475077488041 ) ) ;
#30470 = CARTESIAN_POINT ( 'NONE',  ( 68.13393739769620083, -42.11618894467930119, -65.65000000000000568 ) ) ;
#30471 = ORIENTED_EDGE ( 'NONE', *, *, #19585, .T. ) ;
#30472 = DIRECTION ( 'NONE',  ( 1.000000000000000000, 0.000000000000000000, 0.000000000000000000 ) ) ;
#30473 = CARTESIAN_POINT ( 'NONE',  ( 46.17257466001858290, 6.938700589869487345, -59.45676296270231376 ) ) ;
#30474 = CARTESIAN_POINT ( 'NONE',  ( 12.43092062477990112, 34.07680541178370248, -23.93571342080350206 ) ) ;
#30475 = ORIENTED_EDGE ( 'NONE', *, *, #45140, .T. ) ;
#30476 = CARTESIAN_POINT ( 'NONE',  ( 54.46259150374739733, -45.11618894467940066, -13.50670530417659876 ) ) ;
#30477 = CARTESIAN_POINT ( 'NONE',  ( -18.86606260230380272, -15.61618894417760117, 9.349999999999999645 ) ) ;
#30478 = AXIS2_PLACEMENT_3D ( 'NONE', #42317, #10346, #26304 ) ;
#30479 = CARTESIAN_POINT ( 'NONE',  ( 16.08018489229900183, 19.80150390720080011, -20.24577016824859754 ) ) ;
#30480 = CARTESIAN_POINT ( 'NONE',  ( 22.89358800639388036, -15.93836948567792255, -50.46797458509442436 ) ) ;
#30481 = CARTESIAN_POINT ( 'NONE',  ( 65.47973875042168856, -29.76586224471849818, -16.55654698053239926 ) ) ;
#30482 = DIRECTION ( 'NONE',  ( 0.000000000000000000, 0.000000000000000000, -1.000000000000000000 ) ) ;
#30483 = CARTESIAN_POINT ( 'NONE',  ( 47.04916798186049931, -54.23042865507689925, -75.51723258725520793 ) ) ;
#30484 = CARTESIAN_POINT ( 'NONE',  ( 64.81411238528559693, 13.09683274588459945, -10.69644402401159944 ) ) ;
#30485 = B_SPLINE_CURVE_WITH_KNOTS ( 'NONE', 3,
 ( #48175, #11514, #44237, #27980, #19360, #31394, #47668, #16201, #8602, #48434 ),
 .UNSPECIFIED., .F., .F.,
 ( 4, 2, 2, 2, 4 ),
 ( 0.5000003605116074556, 0.5624999999994833022, 0.6624999999996041833, 0.8224999999997919531, 1.000000000000000000 ),
 .UNSPECIFIED. ) ;
#30486 = CARTESIAN_POINT ( 'NONE',  ( 55.53286968820209779, 19.65994446513209937, -52.96077464608250551 ) ) ;
#30487 = CARTESIAN_POINT ( 'NONE',  ( 52.09209162650440561, 20.06877058433559924, -75.99731153404469808 ) ) ;
#30488 = CARTESIAN_POINT ( 'NONE',  ( 58.01877172845900077, 13.88381123105269843, -25.42745524943100222 ) ) ;
#30489 = CARTESIAN_POINT ( 'NONE',  ( 23.97265246126819704, -15.99208020242580019, -79.30275787339340354 ) ) ;
#30490 = ORIENTED_EDGE ( 'NONE', *, *, #32751, .T. ) ;
#30491 = CARTESIAN_POINT ( 'NONE',  ( 9.367838033491670657, -14.76692425612211146, -47.88713617363420383 ) ) ;
#30492 = TOROIDAL_SURFACE ( 'NONE', #2042, 36.00000000000000000, 2.000000000000000000 ) ;
#30493 = EDGE_CURVE ( 'NONE', #8620, #25307, #12600, .T. ) ;
#30494 = CARTESIAN_POINT ( 'NONE',  ( 1.958201230952900218, -55.72338255999500234, -10.46106927051559943 ) ) ;
#30495 = CARTESIAN_POINT ( 'NONE',  ( 75.92152012689510343, 4.541771151542360663, -12.68757564883900102 ) ) ;
#30496 = CARTESIAN_POINT ( 'NONE',  ( 82.81464131963001307, -43.11618894467930119, -49.28546657628889704 ) ) ;
#30497 = FACE_OUTER_BOUND ( 'NONE', #44917, .T. ) ;
#30498 = CARTESIAN_POINT ( 'NONE',  ( 66.63393739769620083, -43.11618894467930119, -73.25000000000000000 ) ) ;
#30499 = DIRECTION ( 'NONE',  ( 0.8660254037844390407, 0.4999999999999995004, 2.775557561562887037E-17 ) ) ;
#30500 = CARTESIAN_POINT ( 'NONE',  ( 63.24698825150780124, 1.338092079250050137, -62.67980446285670126 ) ) ;
#30501 = CARTESIAN_POINT ( 'NONE',  ( 13.77293537813399915, 20.06110665059810216, -23.09858807645749934 ) ) ;
#30502 = CARTESIAN_POINT ( 'NONE',  ( 42.00588769599519878, 12.47412117931249931, -4.238533581052370103 ) ) ;
#30503 = DIRECTION ( 'NONE',  ( 1.000000000000000000, 0.000000000000000000, 0.000000000000000000 ) ) ;
#30504 = CARTESIAN_POINT ( 'NONE',  ( 50.95940558857264335, 4.060833044306336070, -76.37898308257572921 ) ) ;
#30505 = CARTESIAN_POINT ( 'NONE',  ( 70.03247032090770574, -49.95860450173900347, -75.14853292321149070 ) ) ;
#30506 = AXIS2_PLACEMENT_3D ( 'NONE', #46053, #26101, #42106 ) ;
#30507 = CARTESIAN_POINT ( 'NONE',  ( 76.59130978626896535, -43.22129931671369008, -14.19826186240517174 ) ) ;
#30508 = CARTESIAN_POINT ( 'NONE',  ( 17.91044080450719989, -51.90926368007729508, -75.71157996061791096 ) ) ;
#30509 = CARTESIAN_POINT ( 'NONE',  ( 20.59972290337569589, -41.66761415519157197, -34.89146800830128825 ) ) ;
#30510 = ORIENTED_EDGE ( 'NONE', *, *, #46802, .T. ) ;
#30511 = AXIS2_PLACEMENT_3D ( 'NONE', #38727, #2296, #6234 ) ;
#30512 = CARTESIAN_POINT ( 'NONE',  ( 21.15163403916380247, -10.10897415383030129, -58.80254861845600090 ) ) ;
#30513 = CARTESIAN_POINT ( 'NONE',  ( 63.43778145654719935, 0.9561296872662339297, -61.91446069548659636 ) ) ;
#30514 = ORIENTED_EDGE ( 'NONE', *, *, #45844, .F. ) ;
#30515 = CARTESIAN_POINT ( 'NONE',  ( 73.38393739769610136, 11.88381105532070059, -84.94863984844540994 ) ) ;
#30516 = DIRECTION ( 'NONE',  ( 0.000000000000000000, 0.000000000000000000, -1.000000000000000000 ) ) ;
#30517 = CARTESIAN_POINT ( 'NONE',  ( 22.90076005816202809, -15.61619656631699193, -74.84717351858182610 ) ) ;
#30518 = CARTESIAN_POINT ( 'NONE',  ( 23.06214062797170072, -3.616188944679339823, -32.14999999999999858 ) ) ;
#30519 = CARTESIAN_POINT ( 'NONE',  ( 9.115821549383319677, -16.48115037890739742, -81.23899999999999011 ) ) ;
#30520 = CARTESIAN_POINT ( 'NONE',  ( 44.34202791315729542, -46.09297532313080126, -8.529314961685768637 ) ) ;
#30521 = ORIENTED_EDGE ( 'NONE', *, *, #42522, .T. ) ;
#30522 = ORIENTED_EDGE ( 'NONE', *, *, #37598, .T. ) ;
#30523 = ADVANCED_FACE ( 'NONE', ( #37651 ), #5947, .T. ) ;
#30524 = ORIENTED_EDGE ( 'NONE', *, *, #31369, .F. ) ;
#30525 = DIRECTION ( 'NONE',  ( -0.8090169943749471182, 0.5877852522924732481, 0.000000000000000000 ) ) ;
#30526 = CARTESIAN_POINT ( 'NONE',  ( 61.38641268662350114, -45.22597443312260168, -46.91882270677900379 ) ) ;
#30527 = CARTESIAN_POINT ( 'NONE',  ( 82.51389170711580334, -45.11867408937381896, -46.70334177319745805 ) ) ;
#30528 = ORIENTED_EDGE ( 'NONE', *, *, #48396, .F. ) ;
#30529 = ORIENTED_EDGE ( 'NONE', *, *, #13276, .T. ) ;
#30530 = CARTESIAN_POINT ( 'NONE',  ( 10.61752692138360032, -64.82564047392860118, -18.17418372802830007 ) ) ;
#30531 = AXIS2_PLACEMENT_3D ( 'NONE', #31688, #33508, #13866 ) ;
#30532 = LINE ( 'NONE', #26868, #45240 ) ;
#30533 = EDGE_LOOP ( 'NONE', ( #15345, #6876, #30770, #23602, #35237 ) ) ;
#30534 = LINE ( 'NONE', #21894, #45920 ) ;
#30535 = CARTESIAN_POINT ( 'NONE',  ( 53.62559109365889753, -51.33070570257169862, -75.58097986874130925 ) ) ;
#30536 = CARTESIAN_POINT ( 'NONE',  ( 60.91286535189659901, 14.21542966090570204, -47.20799383203969768 ) ) ;
#30537 = DIRECTION ( 'NONE',  ( 0.000000000000000000, 0.000000000000000000, -1.000000000000000000 ) ) ;
#30538 = AXIS2_PLACEMENT_3D ( 'NONE', #7704, #19737, #15807 ) ;
#30539 = CARTESIAN_POINT ( 'NONE',  ( 42.00047115104329976, -43.88691491351350038, -4.514521081582199891 ) ) ;
#30540 = DIRECTION ( 'NONE',  ( -1.000000000000000000, 0.000000000000000000, 0.000000000000000000 ) ) ;
#30541 = CARTESIAN_POINT ( 'NONE',  ( 56.12094024660369485, 14.43398220991280034, -25.30520633357740223 ) ) ;
#30542 = B_SPLINE_CURVE_WITH_KNOTS ( 'NONE', 3,
 ( #17572, #2625, #6550, #50324, #33795, #25923, #14410, #21738, #25668, #22517, #18597, #33541, #13897, #41670, #49559, #38526, #46140, #18079, #10231, #13646, #37745, #1843, #2103, #17821, #49804 ),
 .UNSPECIFIED., .F., .F.,
 ( 4, 3, 3, 3, 3, 3, 3, 3, 4 ),
 ( -0.1626565276727789944, -0.1623185391170249847, -0.1505729783072729810, -0.1388990119013250035, -0.1281439427408750109, -0.1186168937590759975, -0.1079791825846370124, -0.09959263459902399640, -0.09350866753172300261 ),
 .UNSPECIFIED. ) ;
#30543 = CARTESIAN_POINT ( 'NONE',  ( 64.40305624006870744, 0.9897936423439808173, -70.34985062917159837 ) ) ;
#30544 = DIRECTION ( 'NONE',  ( 0.000000000000000000, 0.000000000000000000, -1.000000000000000000 ) ) ;
#30545 = LINE ( 'NONE', #18763, #36802 ) ;
#30546 = CARTESIAN_POINT ( 'NONE',  ( 23.94340337760679915, -16.39013292960409984, -53.31894848452630242 ) ) ;
#30547 = ORIENTED_EDGE ( 'NONE', *, *, #49978, .T. ) ;
#30548 = CARTESIAN_POINT ( 'NONE',  ( 14.60528279563649967, -52.33797002293529488, -75.98739629952659413 ) ) ;
#30549 = ADVANCED_FACE ( 'NONE', ( #27141 ), #14652, .F. ) ;
#30550 = CARTESIAN_POINT ( 'NONE',  ( 57.41104239909219586, 19.22742992429120079, -53.14439825748630142 ) ) ;
#30551 = CARTESIAN_POINT ( 'NONE',  ( 71.68355379101700464, 1.316034553465529999, -70.28644130772840981 ) ) ;
#30552 = CARTESIAN_POINT ( 'NONE',  ( 44.97387785896593471, -40.02856819528950183, -61.94005888394004700 ) ) ;
#30553 = EDGE_CURVE ( 'NONE', #35579, #21555, #23705, .T. ) ;
#30554 = DIRECTION ( 'NONE',  ( 0.000000000000000000, 1.000000000000000000, 0.000000000000000000 ) ) ;
#30555 = EDGE_CURVE ( 'NONE', #18232, #24151, #38701, .T. ) ;
#30556 = CARTESIAN_POINT ( 'NONE',  ( 83.89200044194980421, 17.38381105532069881, -53.92796738110899923 ) ) ;
#30557 = AXIS2_PLACEMENT_3D ( 'NONE', #5401, #29736, #21358 ) ;
#30558 = EDGE_CURVE ( 'NONE', #31153, #31690, #35571, .T. ) ;
#30559 = CARTESIAN_POINT ( 'NONE',  ( 63.53329261246669546, 1.393731187554809958, -68.81053500035210391 ) ) ;
#30560 = AXIS2_PLACEMENT_3D ( 'NONE', #35659, #4194, #48481 ) ;
#30561 = CARTESIAN_POINT ( 'NONE',  ( 22.99224927569089871, -17.26127340059479920, -80.92212427574548883 ) ) ;
#30562 = CARTESIAN_POINT ( 'NONE',  ( 56.43758032280099712, 19.38627829750620180, -53.06658686592589902 ) ) ;
#30563 = LINE ( 'NONE', #25337, #331 ) ;
#30564 = CARTESIAN_POINT ( 'NONE',  ( 48.18646040924789986, 23.06412321552320321, -55.14499207586399621 ) ) ;
#30565 = EDGE_LOOP ( 'NONE', ( #49410, #50210, #7896, #23044, #31039 ) ) ;
#30566 = CARTESIAN_POINT ( 'NONE',  ( 10.45980683277509904, -11.42729869705060075, -72.04960399662019199 ) ) ;
#30567 = ORIENTED_EDGE ( 'NONE', *, *, #19045, .F. ) ;
#30568 = CARTESIAN_POINT ( 'NONE',  ( 71.47772926835831697, 0.9971903505820688407, -70.62320069164850622 ) ) ;
#30569 = CARTESIAN_POINT ( 'NONE',  ( 14.34417029198879945, -51.11618894467930119, -22.49240188329099865 ) ) ;
#30570 = CARTESIAN_POINT ( 'NONE',  ( 71.33393739883419471, 11.38381102407070067, -61.94987500004730663 ) ) ;
#30572 = CARTESIAN_POINT ( 'NONE',  ( 14.32489919860654304, 1.205480371600849532, -34.75586992539665943 ) ) ;
#30571 = DIRECTION ( 'NONE',  ( 1.000000000000000000, 0.000000000000000000, 0.000000000000000000 ) ) ;
#30573 = CARTESIAN_POINT ( 'NONE',  ( 15.36183068599440027, -8.605738893336619455, -71.91790339393689635 ) ) ;
#30574 = FACE_OUTER_BOUND ( 'NONE', #7785, .T. ) ;
#30575 = CARTESIAN_POINT ( 'NONE',  ( 0.4420762188774020052, -22.38822566875639808, -35.01387690002259490 ) ) ;
#30576 = CARTESIAN_POINT ( 'NONE',  ( 9.367118387258660306, -15.61602127472129986, -41.45282021618999835 ) ) ;
#30577 = B_SPLINE_SURFACE_WITH_KNOTS ( 'NONE', 3, 3, ( 
 ( #27094, #7448, #7191, #19233, #11387, #6676, #30500, #23398, #19491, #34433 ),
 ( #50442, #44628, #48570, #4030, #12673, #24423, #23908, #24163, #598, #346 ),
 ( #16583, #44374, #28367, #48308, #28627, #27606, #20247, #4529, #8733, #32536 ),
 ( #31782, #8477, #43861, #24683, #32033, #48056, #4797, #12155, #40436, #39933 ),
 ( #11641, #35987, #36239, #16075, #20501, #40697, #23658, #16856, #19990, #36493 ),
 ( #20764, #103, #36752, #863, #47545, #43611, #44118, #40186, #7714, #39673 ),
 ( #51723, #16332, #28111, #4277, #19747, #3779, #35740, #15816, #8217, #47799 ),
 ( #32286, #12403, #11905, #27861, #7959, #37809, #29663, #13709, #33602, #13961 ),
 ( #5588, #41733, #49868, #1904, #44893, #17119, #45671, #29150, #29917, #17373 ),
 ( #45935, #32804, #17883, #21282, #49616, #21542, #33072, #37287, #49100, #33340 ),
 ( #48831, #17634, #10024, #1644, #49355, #9774, #42001, #13202, #5838, #1124 ),
 ( #25467, #45151, #40953, #25988, #1386, #6100, #9263, #37538, #33853, #12934 ),
 ( #22056, #5070, #38067, #2163, #28890, #41216, #25211, #8998, #24942, #21026 ),
 ( #5330, #37026, #13456, #25725, #21803, #29412, #45416, #9521, #41472, #39107 ),
 ( #47234, #7136, #23088, #10551, #14215, #42258, #22575, #38323, #14731, #50894 ),
 ( #42783, #11325, #6357, #51158, #27289, #30702, #11068, #38592, #14986, #2939 ) ),
 .UNSPECIFIED., .F., .F., .F.,
 ( 4, 2, 2, 2, 2, 2, 2, 4 ),
 ( 4, 1, 1, 1, 1, 1, 1, 4 ),
 ( -8.523275000000000432E-16, 0.07216186899280999101, 0.1546325764131659952, 0.2061767685508879844, 0.2319488646197490067, 0.2731842183299269533, 0.3391607842662109906, 0.4123535371017769680 ),
 ( 0.000000000000000000, 0.1428571428571430157, 0.2857142857142860315, 0.4285714285714289917, 0.5714285714285709528, 0.7142857142857139685, 0.8571428571428569843, 1.000000000000000000 ),
 .UNSPECIFIED. ) ;
#30578 = VERTEX_POINT ( 'NONE', #46569 ) ;
#30579 = CYLINDRICAL_SURFACE ( 'NONE', #50692, 1.999999999999997780 ) ;
#30580 = B_SPLINE_CURVE_WITH_KNOTS ( 'NONE', 3,
 ( #6493, #10946, #19312, #43174, #27165, #18790, #46597, #7015, #2297, #38457, #26639, #7267, #34768, #10427, #18535, #35293, #26910, #26379 ),
 .UNSPECIFIED., .F., .F.,
 ( 4, 2, 2, 2, 2, 2, 2, 2, 4 ),
 ( 0.5000012016224835154, 0.5625010514196729927, 0.6250009012168624700, 0.6875007510140520584, 0.7500006008112415357, 0.8125004506084312350, 0.8750003004056208233, 0.9375001502028104117, 1.000000000000000000 ),
 .UNSPECIFIED. ) ;
#30581 = VERTEX_POINT ( 'NONE', #15358 ) ;
#30582 = EDGE_CURVE ( 'NONE', #25261, #27489, #42312, .T. ) ;
#30583 = ORIENTED_EDGE ( 'NONE', *, *, #32218, .F. ) ;
#30584 = CARTESIAN_POINT ( 'NONE',  ( 11.97330428934050062, -64.78167623425329680, -16.08313759591939984 ) ) ;
#30585 = CARTESIAN_POINT ( 'NONE',  ( 7.635415421591210894, -60.86027260432054931, -20.56421356237310150 ) ) ;
#30586 = CARTESIAN_POINT ( 'NONE',  ( 22.40179979670677568, -12.43270815927585815, -62.69742595855866085 ) ) ;
#30587 = CARTESIAN_POINT ( 'NONE',  ( 11.78948683875339931, -65.25723971847149585, -47.10950715352170448 ) ) ;
#30588 = EDGE_LOOP ( 'NONE', ( #47444, #44462, #18208, #2917 ) ) ;
#30589 = EDGE_LOOP ( 'NONE', ( #29749, #37805, #38373, #47325 ) ) ;
#30590 = CARTESIAN_POINT ( 'NONE',  ( 71.52463645511689094, 1.229084191802120030, -60.83585027030739667 ) ) ;
#30591 = CARTESIAN_POINT ( 'NONE',  ( 16.13393739769620083, -15.61618894467929941, -18.10000000000000142 ) ) ;
#30592 = CARTESIAN_POINT ( 'NONE',  ( 52.42687975140989209, 18.94760833839670155, -49.65940143135599527 ) ) ;
#30593 = CARTESIAN_POINT ( 'NONE',  ( 59.34569085193420079, -3.119383829553379783, -15.68025057170479819 ) ) ;
#30594 = CARTESIAN_POINT ( 'NONE',  ( 51.24891283041849732, -50.38292309881020969, -76.23258493454248708 ) ) ;
#30595 = CARTESIAN_POINT ( 'NONE',  ( 60.21881437948049864, -46.03921328867149754, -47.91605915182169895 ) ) ;
#30596 = ORIENTED_EDGE ( 'NONE', *, *, #38281, .T. ) ;
#30597 = CARTESIAN_POINT ( 'NONE',  ( 24.03684650753359975, -15.24774525578274087, -33.77750442297574551 ) ) ;
#30598 = CARTESIAN_POINT ( 'NONE',  ( 14.06336364397819771, -23.32131624563684014, -48.37566567428872588 ) ) ;
#30599 = VERTEX_POINT ( 'NONE', #3302 ) ;
#30600 = DIRECTION ( 'NONE',  ( 1.000000000000000000, 0.000000000000000000, 0.000000000000000000 ) ) ;
#30601 = CARTESIAN_POINT ( 'NONE',  ( 56.37863599685000082, -47.94388181700620066, -48.46423989679689726 ) ) ;
#30602 = EDGE_CURVE ( 'NONE', #32056, #16369, #35784, .T. ) ;
#30603 = CONICAL_SURFACE ( 'NONE', #17229, 1.980489356881870222, 0.4636476090008052053 ) ;
#30604 = CARTESIAN_POINT ( 'NONE',  ( 8.364553939350129141, -14.51010202731669985, -41.05750806020520116 ) ) ;
#30605 = AXIS2_PLACEMENT_3D ( 'NONE', #33779, #6021, #14394 ) ;
#30606 = CARTESIAN_POINT ( 'NONE',  ( 13.48893846581560041, -50.82346698513120486, -21.59024777398839845 ) ) ;
#30607 = CARTESIAN_POINT ( 'NONE',  ( 47.40090504849130326, -54.33275752599000441, -75.17436503908771783 ) ) ;
#30608 = CARTESIAN_POINT ( 'NONE',  ( 56.08896608865399713, 14.05775919982069944, -16.05802721449649795 ) ) ;
#30609 = CARTESIAN_POINT ( 'NONE',  ( 9.746758075853771075, 32.08108121953329572, -46.29788637164419640 ) ) ;
#30610 = CARTESIAN_POINT ( 'NONE',  ( 70.99050876911339003, 1.383811055320669947, -70.34999999999999432 ) ) ;
#30611 = CARTESIAN_POINT ( 'NONE',  ( 22.77319179948189998, -17.99586542748549789, -44.95672957286230087 ) ) ;
#30612 = CARTESIAN_POINT ( 'NONE',  ( 13.05521822061487214, -49.46974233527257780, -34.79644660940672907 ) ) ;
#30613 = ORIENTED_EDGE ( 'NONE', *, *, #20421, .T. ) ;
#30614 = CARTESIAN_POINT ( 'NONE',  ( 47.58828887377080719, 23.23481553981489967, -74.72737448322331488 ) ) ;
#30615 = CARTESIAN_POINT ( 'NONE',  ( 64.87536617802101091, 1.096110717717199812, -60.66079369553730061 ) ) ;
#30616 = CARTESIAN_POINT ( 'NONE',  ( 42.86742020280579624, -45.95034697033790394, -7.481776181590609198 ) ) ;
#30617 = CARTESIAN_POINT ( 'NONE',  ( 31.58225770014201572, -28.80002732852027947, -29.09832030244561807 ) ) ;
#30618 = CARTESIAN_POINT ( 'NONE',  ( 15.00527039807065144, -50.63538892808460901, -20.65452793192670100 ) ) ;
#30619 = DIRECTION ( 'NONE',  ( 0.000000000000000000, 0.000000000000000000, -1.000000000000000000 ) ) ;
#30620 = VECTOR ( 'NONE', #45401, 1000.000000000000000 ) ;
#30621 = CARTESIAN_POINT ( 'NONE',  ( 46.42817262113109678, -53.00400577820990122, -76.14999999999999147 ) ) ;
#30622 = EDGE_CURVE ( 'NONE', #667, #38732, #50051, .T. ) ;
#30623 = CARTESIAN_POINT ( 'NONE',  ( 82.75411604745001171, 14.36250171077709936, -47.67220798777069746 ) ) ;
#30624 = CARTESIAN_POINT ( 'NONE',  ( -21.19111549538119732, -3.902638417377439772, -53.38966602606979706 ) ) ;
#30626 = CARTESIAN_POINT ( 'NONE',  ( 68.13393739769620083, 6.883811055320649963, -71.50000000000000000 ) ) ;
#30625 = CARTESIAN_POINT ( 'NONE',  ( 47.63737926530004785, 23.29734256229923872, -74.36261479904801774 ) ) ;
#30627 = CARTESIAN_POINT ( 'NONE',  ( 15.90957661418855551, -7.640854637591640852, -70.99854306824902039 ) ) ;
#30628 = CARTESIAN_POINT ( 'NONE',  ( -12.74467463197259853, 25.82472242301949805, -53.24963421316469692 ) ) ;
#30629 = ORIENTED_EDGE ( 'NONE', *, *, #31953, .T. ) ;
#30630 = CARTESIAN_POINT ( 'NONE',  ( 52.99414832248270812, -49.58664987881770259, -48.92816831207029793 ) ) ;
#30631 = EDGE_LOOP ( 'NONE', ( #6055, #17290 ) ) ;
#30632 = CARTESIAN_POINT ( 'NONE',  ( 46.37902371098480359, 9.012179193705595281, -54.60036856012990825 ) ) ;
#30633 = TOROIDAL_SURFACE ( 'NONE', #2196, 18.49999999936520112, 4.999999999969890752 ) ;
#30634 = CARTESIAN_POINT ( 'NONE',  ( 9.367002091613079173, -15.61601527432330094, -39.84717978380999881 ) ) ;
#30635 = CARTESIAN_POINT ( 'NONE',  ( 13.64779416524800126, 19.95252045979090028, -22.24581330589570172 ) ) ;
#30636 = DIRECTION ( 'NONE',  ( 1.000000000000000000, 0.000000000000000000, 0.000000000000000000 ) ) ;
#30637 = CARTESIAN_POINT ( 'NONE',  ( 20.05198078271940076, -21.48061515102730112, -42.76533676252499561 ) ) ;
#30638 = CARTESIAN_POINT ( 'NONE',  ( 64.83819905826869956, 1.404650034021960092, -61.09597217184949614 ) ) ;
#30639 = CARTESIAN_POINT ( 'NONE',  ( 52.69325989587510151, 18.52870131071809823, -48.74392489991350175 ) ) ;
#30640 = CARTESIAN_POINT ( 'NONE',  ( 55.96902894741660361, -45.83494304597260083, -17.77854326869700330 ) ) ;
#30641 = CARTESIAN_POINT ( 'NONE',  ( 16.23919312834854622, 19.84040911589776357, -15.67087998636921498 ) ) ;
#30642 = EDGE_LOOP ( 'NONE', ( #11151, #30273, #8634, #15036 ) ) ;
#30643 = CARTESIAN_POINT ( 'NONE',  ( 9.472942927203090946, -11.46674308091629868, -34.46484289138480506 ) ) ;
#30644 = EDGE_CURVE ( 'NONE', #19736, #44974, #39204, .T. ) ;
#30645 = FACE_OUTER_BOUND ( 'NONE', #3856, .T. ) ;
#30646 = CARTESIAN_POINT ( 'NONE',  ( 9.864589264534901147, 32.95178484568349830, -46.61883043024580076 ) ) ;
#30647 = CARTESIAN_POINT ( 'NONE',  ( 73.16231026946078941, 0.9234936569010840923, -62.37649816534809588 ) ) ;
#30648 = CARTESIAN_POINT ( 'NONE',  ( 10.83005342329749787, -65.00892210386099634, -17.86451960242310122 ) ) ;
#30649 = CARTESIAN_POINT ( 'NONE',  ( 16.65420337941059969, -49.11618894467930829, -20.15000000000000213 ) ) ;
#30650 = DIRECTION ( 'NONE',  ( 1.000000000000000000, 0.000000000000000000, 0.000000000000000000 ) ) ;
#30651 = CARTESIAN_POINT ( 'NONE',  ( 24.04478666521990959, -15.61618936535764668, -45.50767606031119783 ) ) ;
#30652 = ORIENTED_EDGE ( 'NONE', *, *, #8824, .T. ) ;
#30653 = CARTESIAN_POINT ( 'NONE',  ( 44.08684091409431005, -33.11618894467930119, -54.64999999999999858 ) ) ;
#30654 = ORIENTED_EDGE ( 'NONE', *, *, #15582, .F. ) ;
#30655 = CARTESIAN_POINT ( 'NONE',  ( 10.48988994695839949, -63.23148834558760001, -45.62580560565609744 ) ) ;
#30656 = AXIS2_PLACEMENT_3D ( 'NONE', #37869, #50691, #25527 ) ;
#30657 = CARTESIAN_POINT ( 'NONE',  ( 22.46011406273482081, -10.75452670129970123, -47.58399975706858953 ) ) ;
#30658 = VERTEX_POINT ( 'NONE', #42628 ) ;
#30659 = DIRECTION ( 'NONE',  ( 0.6918010270571950393, -0.3994115091971360276, 0.6015661104845220208 ) ) ;
#30660 = CARTESIAN_POINT ( 'NONE',  ( 57.32828653034189870, 19.18168419026400073, -53.00038473087150237 ) ) ;
#30661 = CARTESIAN_POINT ( 'NONE',  ( 52.14531167014489910, 18.65755136352539978, -76.93287919559629984 ) ) ;
#30662 = ORIENTED_EDGE ( 'NONE', *, *, #51047, .T. ) ;
#30663 = CARTESIAN_POINT ( 'NONE',  ( 68.13393739769618662, -2.032350560841069687, -65.65000000000000568 ) ) ;
#30664 = CARTESIAN_POINT ( 'NONE',  ( 12.36324357420019915, -64.54680782163349306, -15.76420532458509882 ) ) ;
#30666 = DIRECTION ( 'NONE',  ( 0.8090169943749457859, 0.5877852522924753575, 0.000000000000000000 ) ) ;
#30665 = VECTOR ( 'NONE', #45858, 1000.000000000000000 ) ;
#30667 = CARTESIAN_POINT ( 'NONE',  ( 17.83125332364289761, -32.33724466207230108, -34.68801049095930011 ) ) ;
#30668 = EDGE_CURVE ( 'NONE', #39880, #3031, #27478, .T. ) ;
#30669 = CARTESIAN_POINT ( 'NONE',  ( 21.01437418586129979, -8.970584622071779535, -63.49395944174919748 ) ) ;
#30670 = EDGE_CURVE ( 'NONE', #15778, #48656, #7494, .T. ) ;
#30671 = CARTESIAN_POINT ( 'NONE',  ( 18.20470709615282701, -23.32126356507290410, -47.92433596734809953 ) ) ;
#30672 = CARTESIAN_POINT ( 'NONE',  ( 43.57164778298420060, -37.85903016011967281, -72.46142985655266955 ) ) ;
#30673 = ORIENTED_EDGE ( 'NONE', *, *, #25529, .F. ) ;
#30674 = ORIENTED_EDGE ( 'NONE', *, *, #4580, .T. ) ;
#30675 = DIRECTION ( 'NONE',  ( 0.000000000000000000, -1.000000000000000000, 0.000000000000000000 ) ) ;
#30676 = CARTESIAN_POINT ( 'NONE',  ( 21.55045383549850158, -10.50071795129430008, -49.99175337985419532 ) ) ;
#30677 = AXIS2_PLACEMENT_3D ( 'NONE', #43981, #7833, #12532 ) ;
#30678 = CARTESIAN_POINT ( 'NONE',  ( 9.627072997565139900, -12.84800818159280134, -32.14999999999999858 ) ) ;
#30679 = CIRCLE ( 'NONE', #25653, 1.000000000000000888 ) ;
#30680 = CARTESIAN_POINT ( 'NONE',  ( 9.536969139191834088, -14.04286193784190928, -61.52738334231096928 ) ) ;
#30681 = CARTESIAN_POINT ( 'NONE',  ( 14.53093143839820911, 9.901543998477746911, -75.56421356237308373 ) ) ;
#30682 = B_SPLINE_CURVE_WITH_KNOTS ( 'NONE', 3,
 ( #9573, #9830, #49673, #13762, #30242, #29721, #37870, #41274, #1964, #46263, #29976, #5384, #45998, #10087, #41016, #17179, #26046, #42057 ),
 .UNSPECIFIED., .F., .F.,
 ( 4, 2, 2, 2, 2, 2, 2, 2, 4 ),
 ( 0.000000000000000000, 0.06249952351881701840, 0.1249990470376340368, 0.1874985705564510552, 0.2499980940752680736, 0.3124976175940852308, 0.3749971411129023324, 0.4374966646317194896, 0.4999961881505365913 ),
 .UNSPECIFIED. ) ;
#30683 = B_SPLINE_CURVE_WITH_KNOTS ( 'NONE', 3,
 ( #45162, #34385, #22330, #14228, #49629, #41746, #30200, #37551, #9533, #2425 ),
 .UNSPECIFIED., .F., .F.,
 ( 4, 1, 1, 1, 1, 1, 1, 4 ),
 ( 0.5000009373669883628, 0.5765256927868320780, 0.6557446238503832348, 0.7349635549139298396, 0.8141824859776393142, 0.8934014170411903599, 0.9726203481048998345, 1.000000000000000000 ),
 .UNSPECIFIED. ) ;
#30684 = CARTESIAN_POINT ( 'NONE',  ( 16.13393739769620083, -15.61618894467929941, -21.14999999999999858 ) ) ;
#30685 = EDGE_CURVE ( 'NONE', #16602, #2647, #46829, .T. ) ;
#30686 = CARTESIAN_POINT ( 'NONE',  ( 41.86539284521009563, -44.96648031818330082, -5.828818289935889574 ) ) ;
#30687 = DIRECTION ( 'NONE',  ( 0.000000000000000000, -1.000000000000000000, 0.000000000000000000 ) ) ;
#30688 = CARTESIAN_POINT ( 'NONE',  ( 18.10323547118819931, -7.609655000036609884, -59.08443656163060353 ) ) ;
#30689 = EDGE_CURVE ( 'NONE', #3281, #44314, #35604, .T. ) ;
#30690 = ORIENTED_EDGE ( 'NONE', *, *, #2523, .F. ) ;
#30691 = CARTESIAN_POINT ( 'NONE',  ( 20.28858101704520323, -22.28087760341009727, -32.14999999999999858 ) ) ;
#30692 = CARTESIAN_POINT ( 'NONE',  ( 56.46547357425270519, -50.77622842041579787, -74.28536251387168932 ) ) ;
#30694 = CARTESIAN_POINT ( 'NONE',  ( 41.86875520594507094, -39.75028450918884459, -76.96502288003935632 ) ) ;
#30693 = CARTESIAN_POINT ( 'NONE',  ( -2.018330718851010008, 19.83360531021549988, -7.106613257804940353 ) ) ;
#30695 = LINE ( 'NONE', #7380, #11306 ) ;
#30696 = CARTESIAN_POINT ( 'NONE',  ( 51.13393739769620083, 19.38381105532069881, 16.21999999999999886 ) ) ;
#30697 = VERTEX_POINT ( 'NONE', #3570 ) ;
#30698 =( BOUNDED_CURVE ( )  B_SPLINE_CURVE ( 3, ( #43805, #35930, #19694, #7905 ),
 .UNSPECIFIED., .F., .T. ) 
 B_SPLINE_CURVE_WITH_KNOTS ( ( 4, 4 ),
 ( 4.712388980384689674, 5.070260775219133542 ),
 .UNSPECIFIED. ) 
 CURVE ( )  GEOMETRIC_REPRESENTATION_ITEM ( )  RATIONAL_B_SPLINE_CURVE ( ( 1.000000000000000000, 0.9893557610490356646, 0.9893557610490356646, 1.000000000000000000 ) ) 
 REPRESENTATION_ITEM ( '' )  );
#30699 = CARTESIAN_POINT ( 'NONE',  ( -3.978056048070269579, -47.86712544008820203, -4.331835806862760485 ) ) ;
#30700 = CARTESIAN_POINT ( 'NONE',  ( 47.62947969218000566, 23.30723700853820191, -55.11574735166309580 ) ) ;
#30701 = CYLINDRICAL_SURFACE ( 'NONE', #48796, 0.4999999999999364397 ) ;
#30702 = CARTESIAN_POINT ( 'NONE',  ( 63.34508830662979761, 1.264689361399209844, -62.28332989495390137 ) ) ;
#30703 = CARTESIAN_POINT ( 'NONE',  ( 20.59972290337550049, 10.43523626583286656, -34.89146800830130246 ) ) ;
#30704 = CARTESIAN_POINT ( 'NONE',  ( 12.12757547496249977, 33.95539785654250409, -16.69244762553350014 ) ) ;
#30705 = CARTESIAN_POINT ( 'NONE',  ( 51.73306672719670019, 17.77684044143289910, -77.03096706391420412 ) ) ;
#30706 = CARTESIAN_POINT ( 'NONE',  ( 52.82975622904280755, 18.42854261028849905, -48.48625935290110078 ) ) ;
#30707 = CARTESIAN_POINT ( 'NONE',  ( 61.75019796695539753, -46.11618894467930119, -46.37203261889099792 ) ) ;
#30708 = CARTESIAN_POINT ( 'NONE',  ( 54.36797223100090548, -49.00084403992370596, -48.99483916641750625 ) ) ;
#30709 = CARTESIAN_POINT ( 'NONE',  ( 54.41698384653929566, 16.87217916612360114, -26.66137050635050088 ) ) ;
#30710 = CARTESIAN_POINT ( 'NONE',  ( 50.26586832373690328, 21.96242454341640027, -54.04500157025010054 ) ) ;
#30711 = CARTESIAN_POINT ( 'NONE',  ( 11.27223721714355698, -9.290040501825846064, -37.08399908769415987 ) ) ;
#30712 = CARTESIAN_POINT ( 'NONE',  ( 52.63952980978569940, 18.56936772728549911, -48.69585515676859444 ) ) ;
#30713 = CARTESIAN_POINT ( 'NONE',  ( 20.11805472015788609, -22.52872049315324432, -75.84102053616285843 ) ) ;
#30714 = CARTESIAN_POINT ( 'NONE',  ( 71.28186865452410359, 1.191644800533210091, -60.65994692684869705 ) ) ;
#30715 = CARTESIAN_POINT ( 'NONE',  ( 10.77242972425730017, 32.05451349809659689, -45.20492820379810439 ) ) ;
#30716 = CARTESIAN_POINT ( 'NONE',  ( 72.62688124152660407, 1.412342135319809788, -62.12493822889140205 ) ) ;
#30717 = AXIS2_PLACEMENT_3D ( 'NONE', #26375, #6489, #27419 ) ;
#30718 = LINE ( 'NONE', #18673, #47716 ) ;
#30719 = CARTESIAN_POINT ( 'NONE',  ( 9.366980835600751121, -15.61636285886159925, -47.84717978380999881 ) ) ;
#30720 = EDGE_LOOP ( 'NONE', ( #24158, #37412, #2030, #16328 ) ) ;
#30721 = ORIENTED_EDGE ( 'NONE', *, *, #6981, .T. ) ;
#30722 = DIRECTION ( 'NONE',  ( 0.6934629132905126836, 0.5038302981000500891, 0.5150380749100492705 ) ) ;
#30723 = CARTESIAN_POINT ( 'NONE',  ( 49.38368952090034725, -2.298263431363495535, -15.71712813759418026 ) ) ;
#30724 = ORIENTED_EDGE ( 'NONE', *, *, #45974, .F. ) ;
#30725 = CARTESIAN_POINT ( 'NONE',  ( 11.14030921647079886, -63.71572269098970054, -44.01013735364150392 ) ) ;
#30726 = CARTESIAN_POINT ( 'NONE',  ( 57.36258065022549602, -45.13425998825839969, -25.53108703577100158 ) ) ;
#30727 = CARTESIAN_POINT ( 'NONE',  ( 8.043767453946731649, -21.49404146760402767, -5.966499999999999915 ) ) ;
#30728 = CARTESIAN_POINT ( 'NONE',  ( 63.49151163952229382, 1.387131204727280132, -68.68796153961081075 ) ) ;
#30729 = ORIENTED_EDGE ( 'NONE', *, *, #14854, .T. ) ;
#30730 = DIRECTION ( 'NONE',  ( -1.000000000000000000, 0.000000000000000000, 0.000000000000000000 ) ) ;
#30731 = CARTESIAN_POINT ( 'NONE',  ( 43.00066473404336165, 6.545556978096114698, -75.31636325171257340 ) ) ;
#30732 = CARTESIAN_POINT ( 'NONE',  ( 11.44079479683260026, 33.77516212222609937, -23.47454584385869936 ) ) ;
#30733 = VERTEX_POINT ( 'NONE', #47591 ) ;
#30734 = CARTESIAN_POINT ( 'NONE',  ( 8.112799223618010203, -17.52513170135909704, -36.71796074224590001 ) ) ;
#30735 = EDGE_CURVE ( 'NONE', #18008, #36317, #6983, .T. ) ;
#30736 = DIRECTION ( 'NONE',  ( 0.000000000000000000, 0.000000000000000000, -1.000000000000000000 ) ) ;
#30737 = DIRECTION ( 'NONE',  ( 0.7071067811865457964, 0.7071067811865492381, 0.000000000000000000 ) ) ;
#30738 = CARTESIAN_POINT ( 'NONE',  ( 22.89776929422545493, -15.84020125202738605, -50.46335449847054377 ) ) ;
#30739 = ADVANCED_FACE ( 'NONE', ( #3048 ), #19019, .F. ) ;
#30740 = CARTESIAN_POINT ( 'NONE',  ( 64.78100246958599939, -29.69834437706749952, -16.45672703461520214 ) ) ;
#30741 = CARTESIAN_POINT ( 'NONE',  ( 63.25402410758490390, 0.9098571636355720083, -62.15909090909049439 ) ) ;
#30742 = CARTESIAN_POINT ( 'NONE',  ( 46.93451352784899910, -54.01342379717689823, -75.73967526752529977 ) ) ;
#30743 = CARTESIAN_POINT ( 'NONE',  ( 52.33571454780909704, 13.13344079467719894, -7.409926258573939606 ) ) ;
#30744 = DIRECTION ( 'NONE',  ( 0.000000000000000000, 0.000000000000000000, -1.000000000000000000 ) ) ;
#30745 = B_SPLINE_SURFACE_WITH_KNOTS ( 'NONE', 3, 3, ( 
 ( #17020, #29308, #44270, #21181, #17277, #44530, #33237, #13104, #45310, #8896, #499, #9419, #20404, #25369, #5484, #12568, #24582, #9153 ),
 ( #36147, #25104, #249, #16233, #48207, #40853, #4693, #28530, #8632, #20663, #36648, #32189, #753, #32971, #16750, #12310, #32702, #28269 ),
 ( #4956, #24325, #48729, #12833, #28790, #44791, #20926, #36922, #1026, #48997, #21692, #10445, #46615, #49510, #30073, #38479, #25879, #38220 ),
 ( #14106, #2315, #41893, #41625, #37440, #50535, #18553, #45829, #33497, #1795, #22470, #2579, #29812, #17778, #30594, #42679, #9663, #37962 ),
 ( #17529, #1541, #10703, #2059, #30336, #34529, #25622, #18037, #37699, #46359, #26144, #49763, #14627, #34259, #46098, #18287, #50282, #26657 ),
 ( #14368, #42154, #26398, #34006, #33748, #21441, #13601, #29564, #45570, #5733, #42418, #13855, #10183, #6510, #9916, #5991, #21951, #50016 ),
 ( #6253, #22210, #27442, #35577, #19331, #19068, #31875, #35830, #23752, #19840, #30847, #51562, #7802, #47388, #15663, #27950, #3870, #31616 ),
 ( #51814, #14882, #11484, #26929, #11995, #22984, #3103, #47634, #11222, #35042, #42935, #11742, #27700, #39768, #43698, #15920, #39006, #23491 ),
 ( #2842, #47892, #34788, #51051, #15148, #31107, #39254, #22726, #27185, #35311, #6775, #43192, #7287, #23238, #18808, #50794, #3357, #51312 ),
 ( #15407, #31360, #43445, #7547, #3615, #19587, #24005, #9090, #40025, #694, #12501, #48403, #20599, #4115, #24262, #20092, #12769, #36083 ) ),
 .UNSPECIFIED., .F., .F., .F.,
 ( 4, 1, 1, 1, 1, 1, 1, 4 ),
 ( 4, 2, 2, 2, 2, 2, 2, 2, 4 ),
 ( 0.000000000000000000, 0.1428571428571430157, 0.2857142857142860315, 0.4285714285714289917, 0.5714285714285709528, 0.7142857142857139685, 0.8571428571428569843, 1.000004205110210043 ),
 ( -4.205110215000000084E-06, 0.4467108845949059881, 0.9572376098462269667, 1.276316813128300032, 1.435856414769340006, 1.633224234453040102, 1.949012745946970160, 2.454274364337259762, 2.552637831366810328 ),
 .UNSPECIFIED. ) ;
#30746 = CARTESIAN_POINT ( 'NONE',  ( 65.46029542295769943, -29.76883965895079953, -16.55376543218019947 ) ) ;
#30747 = CARTESIAN_POINT ( 'NONE',  ( 13.47464181256609983, -7.811647465521459388, -36.90313586381709854 ) ) ;
#30748 = EDGE_CURVE ( 'NONE', #39800, #29825, #33130, .T. ) ;
#30749 = ORIENTED_EDGE ( 'NONE', *, *, #40241, .T. ) ;
#30750 = CARTESIAN_POINT ( 'NONE',  ( 54.57977433850850701, -48.05032713420980173, -26.70386303289920349 ) ) ;
#30751 = CARTESIAN_POINT ( 'NONE',  ( -3.898789279713819944, -49.42317546875409562, -6.816182948762260274 ) ) ;
#30752 = CARTESIAN_POINT ( 'NONE',  ( 75.27130359675959426, 4.589503367956900171, -12.40984670276689883 ) ) ;
#30753 = AXIS2_PLACEMENT_3D ( 'NONE', #12216, #11710, #11970 ) ;
#30754 = CARTESIAN_POINT ( 'NONE',  ( 75.29154419428947165, 13.40016185298322782, -14.05786387858811182 ) ) ;
#30755 = CARTESIAN_POINT ( 'NONE',  ( 74.23393739769618094, -0.5161889446793590519, -65.65000000000000568 ) ) ;
#30756 = DIRECTION ( 'NONE',  ( -1.000000000000000000, 0.000000000000000000, 0.000000000000000000 ) ) ;
#30757 = CARTESIAN_POINT ( 'NONE',  ( 16.13393739769620083, -15.61618894467929941, -6.721843382729280059 ) ) ;
#30758 = CARTESIAN_POINT ( 'NONE',  ( 82.37380189745128689, -45.11495191480410227, -46.56083452486799956 ) ) ;
#30759 = DIRECTION ( 'NONE',  ( -1.000000000000000000, 0.000000000000000000, 0.000000000000000000 ) ) ;
#30760 = CARTESIAN_POINT ( 'NONE',  ( 40.40277276999439948, 13.62463458412210038, -4.354462746277430796 ) ) ;
#30761 = CARTESIAN_POINT ( 'NONE',  ( 51.13393739769620083, 19.38381105532069881, 16.85000000000000142 ) ) ;
#30762 = CARTESIAN_POINT ( 'NONE',  ( -0.1295185695942999982, 0.6472670226113349523, -84.65000000000000568 ) ) ;
#30763 = DIRECTION ( 'NONE',  ( 0.5215975411497816294, -0.8522221556268643194, 0.04066205264374356254 ) ) ;
#30764 = CYLINDRICAL_SURFACE ( 'NONE', #20862, 1.000000000000001110 ) ;
#30765 = CARTESIAN_POINT ( 'NONE',  ( 17.73673790147540075, -51.97808261890140358, -75.79330468503940210 ) ) ;
#30766 = CARTESIAN_POINT ( 'NONE',  ( 20.53650276133985031, -41.76263555408612405, -34.79644660940672907 ) ) ;
#30767 = ORIENTED_EDGE ( 'NONE', *, *, #10659, .T. ) ;
#30768 = CARTESIAN_POINT ( 'NONE',  ( 10.10928765634339932, -11.23323448080919995, -56.26754282442009725 ) ) ;
#30769 = CARTESIAN_POINT ( 'NONE',  ( 63.70304491682400538, 1.421976796946359922, -62.00656477358510443 ) ) ;
#30770 = ORIENTED_EDGE ( 'NONE', *, *, #46447, .F. ) ;
#30771 = CARTESIAN_POINT ( 'NONE',  ( -1.839728563314089849, -28.30269090235150031, -54.64999999999999858 ) ) ;
#30772 = DIRECTION ( 'NONE',  ( 0.5835456732599411112, 0.8120803206700689669, 0.000000000000000000 ) ) ;
#30773 = CARTESIAN_POINT ( 'NONE',  ( 73.16133767175020353, 0.8879664753683469414, -68.92499589875220067 ) ) ;
#30774 = CARTESIAN_POINT ( 'NONE',  ( 17.01980771413989757, -8.849199239206612333, -73.99448688925269835 ) ) ;
#30775 = CARTESIAN_POINT ( 'NONE',  ( 10.24083624763009936, -19.10015682395959757, -81.23899999999999011 ) ) ;
#30776 = CARTESIAN_POINT ( 'NONE',  ( 41.75079782317220634, -45.66965496456020190, -6.577253294032040287 ) ) ;
#30777 = ORIENTED_EDGE ( 'NONE', *, *, #3829, .T. ) ;
#30778 = EDGE_LOOP ( 'NONE', ( #11663, #4879 ) ) ;
#30779 = ORIENTED_EDGE ( 'NONE', *, *, #35198, .T. ) ;
#30780 = CARTESIAN_POINT ( 'NONE',  ( 29.13393739769619728, -4.468739684871080087, -35.14999999999999858 ) ) ;
#30781 = CARTESIAN_POINT ( 'NONE',  ( 61.08961532041769971, -45.33614436321569485, -46.92979171198570043 ) ) ;
#30782 = CARTESIAN_POINT ( 'NONE',  ( -5.815486204891447741, -48.02745134462772825, -40.24138896526777387 ) ) ;
#30783 = TOROIDAL_SURFACE ( 'NONE', #40003, 1.499999999717960053, 0.4999999999863239952 ) ;
#30784 = ORIENTED_EDGE ( 'NONE', *, *, #44030, .T. ) ;
#30785 = CARTESIAN_POINT ( 'NONE',  ( 20.86616962407251208, -10.71475060854243644, -80.19705727907313531 ) ) ;
#30786 = ORIENTED_EDGE ( 'NONE', *, *, #6269, .T. ) ;
#30787 = CARTESIAN_POINT ( 'NONE',  ( 68.13393739769620083, -33.11618894467940066, -65.65000000000000568 ) ) ;
#30788 = EDGE_CURVE ( 'NONE', #16420, #6443, #25558, .T. ) ;
#30789 = APPLICATION_CONTEXT ( 'automotive_design' ) ;
#30790 = DIRECTION ( 'NONE',  ( 0.000000000000000000, -1.000000000000000000, 0.000000000000000000 ) ) ;
#30791 = VERTEX_POINT ( 'NONE', #41008 ) ;
#30792 = CARTESIAN_POINT ( 'NONE',  ( 61.55415490858696614, -29.38851365205942656, -15.99574535869865599 ) ) ;
#30793 = CARTESIAN_POINT ( 'NONE',  ( 52.36416846730020325, -50.95050588212149734, -76.17671309931749590 ) ) ;
#30794 = CARTESIAN_POINT ( 'NONE',  ( 60.73370194276889578, 14.32741777250609871, -47.36977307575320140 ) ) ;
#30795 = CARTESIAN_POINT ( 'NONE',  ( 50.95939078474921047, -48.61618894467930119, -76.37902184192927280 ) ) ;
#30796 = CARTESIAN_POINT ( 'NONE',  ( 41.85352072865990181, -43.83138081351579984, -4.272019245294999656 ) ) ;
#30797 = DIRECTION ( 'NONE',  ( 0.000000000000000000, 0.000000000000000000, -1.000000000000000000 ) ) ;
#30798 = CARTESIAN_POINT ( 'NONE',  ( -10.42111060954870005, 11.57999969675590002, -6.138047689998500367 ) ) ;
#30799 = CARTESIAN_POINT ( 'NONE',  ( 64.30690765430760791, 1.170657617701480024, -70.22888111369030639 ) ) ;
#30800 = CARTESIAN_POINT ( 'NONE',  ( 11.59299064767398590, -21.01270279974525934, -39.56984226053648257 ) ) ;
#30801 = DIRECTION ( 'NONE',  ( -0.2260571801428030714, 0.000000000000000000, 0.9741140340359972782 ) ) ;
#30802 = CARTESIAN_POINT ( 'NONE',  ( 13.58021417256130015, -23.03678500379669813, -51.89300772538110351 ) ) ;
#30803 = ADVANCED_FACE ( 'NONE', ( #20294 ), #9649, .T. ) ;
#30804 = EDGE_LOOP ( 'NONE', ( #48716, #36199, #19856, #30080, #39380, #40518 ) ) ;
#30805 = DIRECTION ( 'NONE',  ( 0.000000000000000000, 0.000000000000000000, -1.000000000000000000 ) ) ;
#30806 = CARTESIAN_POINT ( 'NONE',  ( 57.48053633206980351, 19.28116340013579944, -53.28847060521069778 ) ) ;
#30807 = EDGE_CURVE ( 'NONE', #17993, #46283, #10855, .T. ) ;
#30808 = CARTESIAN_POINT ( 'NONE',  ( 71.38118348160060123, 1.400446703426730055, -70.22110957219430816 ) ) ;
#30809 = CARTESIAN_POINT ( 'NONE',  ( 46.12656867617091905, -40.10072528304355899, -56.34446073384248166 ) ) ;
#30810 = CARTESIAN_POINT ( 'NONE',  ( 15.94238461914910054, 19.75473507481530078, -20.23090583108210083 ) ) ;
#30811 = CARTESIAN_POINT ( 'NONE',  ( 20.69643343333880381, -10.53272061581830066, -32.14999999999999858 ) ) ;
#30812 = CARTESIAN_POINT ( 'NONE',  ( 8.223013028489239318, -15.61598591435789984, -40.50766849176299189 ) ) ;
#30813 = DIRECTION ( 'NONE',  ( 0.000000000000000000, 0.000000000000000000, 1.000000000000000000 ) ) ;
#30814 = CARTESIAN_POINT ( 'NONE',  ( 48.04058133588620194, -54.36387450899209739, -55.20769835483399390 ) ) ;
#30815 = CARTESIAN_POINT ( 'NONE',  ( 19.44826417394619966, -21.62186115282320031, -81.18618737929101314 ) ) ;
#30816 = AXIS2_PLACEMENT_3D ( 'NONE', #4281, #36244, #24428 ) ;
#30817 = CARTESIAN_POINT ( 'NONE',  ( -3.978056047869968914, -47.86712544021135329, -4.331835810920249052 ) ) ;
#30818 = CARTESIAN_POINT ( 'NONE',  ( 47.90025853917680365, 23.12498366852580034, -54.74357571739309947 ) ) ;
#30819 = ORIENTED_EDGE ( 'NONE', *, *, #917, .T. ) ;
#30820 = CARTESIAN_POINT ( 'NONE',  ( 9.885447592686571028, -18.88711149514460175, -75.69367482554670801 ) ) ;
#30821 = ORIENTED_EDGE ( 'NONE', *, *, #12089, .F. ) ;
#30822 = CARTESIAN_POINT ( 'NONE',  ( 71.52074786344320501, 0.8966068345641440285, -70.60278586552529134 ) ) ;
#30823 = DIRECTION ( 'NONE',  ( 0.000000000000000000, 0.000000000000000000, -1.000000000000000000 ) ) ;
#30824 = CARTESIAN_POINT ( 'NONE',  ( 58.27624582431690214, -46.80735200045160127, -47.55852830428500511 ) ) ;
#30825 = CARTESIAN_POINT ( 'NONE',  ( 16.13393739769620083, -15.61618894467929941, 9.349999999999999645 ) ) ;
#30827 = CARTESIAN_POINT ( 'NONE',  ( 44.13393739769620083, -33.11618894467930829, -54.27132075603720551 ) ) ;
#30826 = FACE_OUTER_BOUND ( 'NONE', #45499, .T. ) ;
#30828 = CARTESIAN_POINT ( 'NONE',  ( 8.643744238043529649, 17.52287609088129727, -35.14999999999999858 ) ) ;
#30829 = CARTESIAN_POINT ( 'NONE',  ( 23.04647245864238769, -19.60029819911440541, -41.67433410030931640 ) ) ;
#30830 = DIRECTION ( 'NONE',  ( 0.000000000000000000, 0.000000000000000000, -1.000000000000000000 ) ) ;
#30831 = ORIENTED_EDGE ( 'NONE', *, *, #25529, .T. ) ;
#30832 = CARTESIAN_POINT ( 'NONE',  ( 18.13393739769620083, -32.62399965035220362, -35.14999999999999858 ) ) ;
#30833 = ORIENTED_EDGE ( 'NONE', *, *, #25572, .F. ) ;
#30834 = EDGE_LOOP ( 'NONE', ( #6729, #13321, #48705, #10370, #16368, #10156 ) ) ;
#30835 = CARTESIAN_POINT ( 'NONE',  ( 12.36320305068320025, -64.54682834576858852, -15.76422791927960176 ) ) ;
#30836 = CARTESIAN_POINT ( 'NONE',  ( 12.14973823253568419, -8.703704093358281213, -39.12565883727726401 ) ) ;
#30837 = DIRECTION ( 'NONE',  ( -0.3487035033511789450, 0.9372330909387559528, 0.000000000000000000 ) ) ;
#30838 = CARTESIAN_POINT ( 'NONE',  ( 12.40793752380340109, -65.45934900383400645, -47.57600753193199949 ) ) ;
#30839 = EDGE_LOOP ( 'NONE', ( #17654, #30915, #19779, #16480, #34422 ) ) ;
#30840 = ORIENTED_EDGE ( 'NONE', *, *, #15949, .T. ) ;
#30841 = CARTESIAN_POINT ( 'NONE',  ( 63.63393739769619373, 21.88381105532059934, 11.84999999999999964 ) ) ;
#30842 = CARTESIAN_POINT ( 'NONE',  ( 82.45630311851421368, -45.09271792554360303, -46.38988467804559690 ) ) ;
#30843 = CARTESIAN_POINT ( 'NONE',  ( 52.70127459758040089, -49.76132437923789809, -48.79000188394560666 ) ) ;
#30844 = EDGE_CURVE ( 'NONE', #34917, #5766, #2731, .T. ) ;
#30845 = DIRECTION ( 'NONE',  ( 0.000000000000000000, 0.000000000000000000, 1.000000000000000000 ) ) ;
#30846 = CARTESIAN_POINT ( 'NONE',  ( 58.94098116141569932, -3.123968702424910315, -15.65000564697079710 ) ) ;
#30847 = CARTESIAN_POINT ( 'NONE',  ( 51.57818415910379883, -49.54080979270530349, -76.64184137469480618 ) ) ;
#30848 = CARTESIAN_POINT ( 'NONE',  ( 57.43655318892930239, -49.91794914532149363, -52.37342405164899617 ) ) ;
#30849 = VERTEX_POINT ( 'NONE', #6661 ) ;
#30850 = CARTESIAN_POINT ( 'NONE',  ( 24.04420212447170613, -15.49892605004181334, -33.78761283496942980 ) ) ;
#30851 = CARTESIAN_POINT ( 'NONE',  ( 9.367479402551163403, -16.16638264608517161, -51.82130573733594758 ) ) ;
#30852 = ORIENTED_EDGE ( 'NONE', *, *, #50302, .F. ) ;
#30853 = CARTESIAN_POINT ( 'NONE',  ( 9.501448989937911094, -14.08578117475173919, -33.52488049317692997 ) ) ;
#30854 = AXIS2_PLACEMENT_3D ( 'NONE', #13494, #14257, #29450 ) ;
#30855 = CARTESIAN_POINT ( 'NONE',  ( 68.13393739769620083, 4.883811055320659733, -65.65000000000000568 ) ) ;
#30856 = AXIS2_PLACEMENT_3D ( 'NONE', #25945, #10251, #38549 ) ;
#30857 = CARTESIAN_POINT ( 'NONE',  ( 21.47828441782199960, -9.869476621963398699, -43.75095171636819913 ) ) ;
#30858 = CARTESIAN_POINT ( 'NONE',  ( 13.50106232664160011, -51.29021222096099564, -22.28116776360520035 ) ) ;
#30859 = AXIS2_PLACEMENT_3D ( 'NONE', #21287, #20252, #48313 ) ;
#30860 = DIRECTION ( 'NONE',  ( 0.000000000000000000, 1.000000000000000000, 0.000000000000000000 ) ) ;
#30861 = CARTESIAN_POINT ( 'NONE',  ( 57.30711608794669587, 13.88381105532070059, -16.97812376854340144 ) ) ;
#30862 = DIRECTION ( 'NONE',  ( 1.000000000000000000, 0.000000000000000000, 0.000000000000000000 ) ) ;
#30863 = CARTESIAN_POINT ( 'NONE',  ( 71.17905174416029013, 1.387412027389909985, -70.29005197907430613 ) ) ;
#30864 = CARTESIAN_POINT ( 'NONE',  ( 13.05928102721579975, -9.268823555959679439, -40.20359370904520091 ) ) ;
#30865 = CARTESIAN_POINT ( 'NONE',  ( 46.60111831227250434, -39.96272243613920239, -54.61658773935999989 ) ) ;
#30866 = ORIENTED_EDGE ( 'NONE', *, *, #3544, .T. ) ;
#30867 = B_SPLINE_CURVE_WITH_KNOTS ( 'NONE', 3,
 ( #24416, #8209, #32530, #16068, #36485, #12666, #5318, #590, #16575, #48557, #5058, #48049, #16325, #12148, #33064, #44885, #24155, #28102 ),
 .UNSPECIFIED., .F., .F.,
 ( 4, 2, 2, 2, 2, 2, 2, 2, 4 ),
 ( 0.000000000000000000, 0.06249986135442708174, 0.1249997227088541635, 0.1874995840632812383, 0.2499994454177083270, 0.3124993067721353879, 0.3749991681265624766, 0.4374990294809895652, 0.4999988908354166539 ),
 .UNSPECIFIED. ) ;
#30868 = CARTESIAN_POINT ( 'NONE',  ( 47.26969180900800183, 22.92145913501139987, -75.47109442055808870 ) ) ;
#30869 = CARTESIAN_POINT ( 'NONE',  ( 64.81979753630260177, 0.8904513541338849869, -60.64834380034769623 ) ) ;
#30870 = EDGE_CURVE ( 'NONE', #47619, #15485, #22460, .T. ) ;
#30871 = CARTESIAN_POINT ( 'NONE',  ( 23.53669455186048864, 17.69319178430572137, -34.79644561402099612 ) ) ;
#30872 = DIRECTION ( 'NONE',  ( 0.000000000000000000, 0.000000000000000000, -1.000000000000000000 ) ) ;
#30873 = DIRECTION ( 'NONE',  ( 4.809214325624639985E-31, -1.000000000000000000, -6.060292087350920604E-16 ) ) ;
#30874 = FACE_OUTER_BOUND ( 'NONE', #10881, .T. ) ;
#30875 = CARTESIAN_POINT ( 'NONE',  ( 82.45926474365251124, 14.04402909200689997, -47.17634237573840039 ) ) ;
#30876 = CARTESIAN_POINT ( 'NONE',  ( -21.18743422985509994, -3.890487093983819644, -53.43809524694220414 ) ) ;
#30878 = CARTESIAN_POINT ( 'NONE',  ( 22.46012367902698514, -20.47783799420304618, -58.00066461748448177 ) ) ;
#30877 = CARTESIAN_POINT ( 'NONE',  ( 68.13393739769620083, 17.38381105532069881, -65.65000000000000568 ) ) ;
#30879 = CARTESIAN_POINT ( 'NONE',  ( 8.222903922732800908, -15.61639209420869889, -32.79233150823699816 ) ) ;
#30880 = DIRECTION ( 'NONE',  ( 0.000000000000000000, -1.000000000000000000, 0.000000000000000000 ) ) ;
#30881 = FACE_OUTER_BOUND ( 'NONE', #50211, .T. ) ;
#30882 = ORIENTED_EDGE ( 'NONE', *, *, #25106, .T. ) ;
#30883 = CARTESIAN_POINT ( 'NONE',  ( 53.33637666853859827, -49.41089065994679430, -48.94981449663340101 ) ) ;
#30884 = ORIENTED_EDGE ( 'NONE', *, *, #47470, .F. ) ;
#30885 = AXIS2_PLACEMENT_3D ( 'NONE', #30996, #39144, #15291 ) ;
#30886 = CARTESIAN_POINT ( 'NONE',  ( 46.39209508087989775, 9.012977385794867402, -54.53647718218035578 ) ) ;
#30887 = CARTESIAN_POINT ( 'NONE',  ( 19.54197556973233318, -9.703305473112902035, -42.11948649911619924 ) ) ;
#30888 = CARTESIAN_POINT ( 'NONE',  ( 13.81950199472360019, 20.03075999611900215, -23.06529971393420198 ) ) ;
#30889 = DIRECTION ( 'NONE',  ( 1.000000000000000000, 0.000000000000000000, 0.000000000000000000 ) ) ;
#30890 = CARTESIAN_POINT ( 'NONE',  ( 15.31286695519810159, -8.611304789671351045, -55.91567931908580391 ) ) ;
#30891 = CIRCLE ( 'NONE', #35959, 0.5000000000000004441 ) ;
#30892 = CARTESIAN_POINT ( 'NONE',  ( 52.96080964268509916, 18.38537766553690034, -48.98458843674050200 ) ) ;
#30893 = CARTESIAN_POINT ( 'NONE',  ( 56.28192814617099771, -45.52819751003289639, -17.93020058329020117 ) ) ;
#30894 = CARTESIAN_POINT ( 'NONE',  ( 68.13393739769620083, -50.61618894467930119, -73.25000000000000000 ) ) ;
#30895 = EDGE_LOOP ( 'NONE', ( #19709, #40460, #37603, #46978, #36260, #38941 ) ) ;
#30896 = CARTESIAN_POINT ( 'NONE',  ( 8.524204963362700838, -13.69818986724079934, -36.36609723691169904 ) ) ;
#30897 = ORIENTED_EDGE ( 'NONE', *, *, #32662, .F. ) ;
#30898 = CARTESIAN_POINT ( 'NONE',  ( 61.13393739769620083, 4.883811055320659733, -84.38499399519520239 ) ) ;
#30899 = CARTESIAN_POINT ( 'NONE',  ( 9.383988014790560328, 32.17454221883009780, -46.50702848791099342 ) ) ;
#30900 = CARTESIAN_POINT ( 'NONE',  ( 73.02919596257699197, 0.9065823421260970072, -62.18054194328749418 ) ) ;
#30901 = CARTESIAN_POINT ( 'NONE',  ( 50.87650205437540052, -52.17794571071839727, -52.56647976602120309 ) ) ;
#30902 = CARTESIAN_POINT ( 'NONE',  ( 53.30280620372429468, 18.18069847459639732, -48.78464136231010428 ) ) ;
#30903 = CARTESIAN_POINT ( 'NONE',  ( 71.33393739769628894, 4.883811055320659733, -61.44999999999999574 ) ) ;
#30904 = CARTESIAN_POINT ( 'NONE',  ( 51.65923706648989366, -52.70673387297149759, -53.94592918870640119 ) ) ;
#30905 = ORIENTED_EDGE ( 'NONE', *, *, #18638, .F. ) ;
#30906 = CARTESIAN_POINT ( 'NONE',  ( 64.64662912975160225, 0.9425424353905850205, -70.53248918539379986 ) ) ;
#30907 = ORIENTED_EDGE ( 'NONE', *, *, #36227, .T. ) ;
#30908 = CARTESIAN_POINT ( 'NONE',  ( 10.14486239315709959, -63.26972435890289148, -45.99310794422409998 ) ) ;
#30909 = EDGE_CURVE ( 'NONE', #20523, #11224, #45716, .T. ) ;
#30910 = CARTESIAN_POINT ( 'NONE',  ( 68.13393739769769297, 18.72622661238300168, -73.39853292320978539 ) ) ;
#30911 = ORIENTED_EDGE ( 'NONE', *, *, #21041, .F. ) ;
#30912 = CARTESIAN_POINT ( 'NONE',  ( 11.38042644497720701, -64.49026688052417455, -44.43662027715303964 ) ) ;
#30913 = FACE_OUTER_BOUND ( 'NONE', #5549, .T. ) ;
#30914 = CARTESIAN_POINT ( 'NONE',  ( 52.71937669323779829, 18.95387029200830042, -77.16972201513189589 ) ) ;
#30915 = ORIENTED_EDGE ( 'NONE', *, *, #30266, .T. ) ;
#30916 = EDGE_CURVE ( 'NONE', #50655, #47312, #50938, .T. ) ;
#30917 = CARTESIAN_POINT ( 'NONE',  ( 68.13393739806289773, -1.666188944679350081, -89.15000000000000568 ) ) ;
#30918 = FACE_OUTER_BOUND ( 'NONE', #38685, .T. ) ;
#30919 = CARTESIAN_POINT ( 'NONE',  ( 83.53665348986312722, -44.61316859376488253, -46.51478504062129105 ) ) ;
#30920 = FACE_BOUND ( 'NONE', #41295, .T. ) ;
#30921 = EDGE_CURVE ( 'NONE', #18539, #23485, #34050, .T. ) ;
#30922 = CARTESIAN_POINT ( 'NONE',  ( 10.28542518435660114, -21.42804105449349805, -62.54333226898589260 ) ) ;
#30923 = CARTESIAN_POINT ( 'NONE',  ( 8.222988179026620159, -15.61639226004780134, -48.50766849176299189 ) ) ;
#30924 = CARTESIAN_POINT ( 'NONE',  ( 46.17549598699994107, -38.17137574164103597, -59.44215122485496039 ) ) ;
#30925 = ORIENTED_EDGE ( 'NONE', *, *, #23312, .F. ) ;
#30926 = ORIENTED_EDGE ( 'NONE', *, *, #14274, .F. ) ;
#30927 = AXIS2_PLACEMENT_3D ( 'NONE', #23757, #10708, #50798 ) ;
#30928 = DIRECTION ( 'NONE',  ( 1.000000000000000000, 0.000000000000000000, 0.000000000000000000 ) ) ;
#30929 = CARTESIAN_POINT ( 'NONE',  ( 18.45084779930429875, -8.535326003196420430, -49.83331551772709389 ) ) ;
#30930 = AXIS2_PLACEMENT_3D ( 'NONE', #34936, #51204, #19973 ) ;
#30931 = EDGE_CURVE ( 'NONE', #31554, #18021, #22881, .T. ) ;
#30932 = CARTESIAN_POINT ( 'NONE',  ( 46.59919755282350451, 13.88381105532070059, -7.957589888115209398 ) ) ;
#30933 = AXIS2_PLACEMENT_3D ( 'NONE', #293, #49300, #12610 ) ;
#30934 = CARTESIAN_POINT ( 'NONE',  ( 10.85494166744680022, -21.28090959162620166, -32.14999999999999858 ) ) ;
#30935 = CARTESIAN_POINT ( 'NONE',  ( 13.13393739769619906, -63.52234721269329754, -46.39999999999999858 ) ) ;
#30936 = AXIS2_PLACEMENT_3D ( 'NONE', #9841, #33922, #41802 ) ;
#30937 = CARTESIAN_POINT ( 'NONE',  ( 0.03729862092324889855, 14.54995912156149984, -34.73403371893299862 ) ) ;
#30938 = EDGE_CURVE ( 'NONE', #2407, #32428, #27369, .T. ) ;
#30939 = CYLINDRICAL_SURFACE ( 'NONE', #49121, 2.000000000000000888 ) ;
#30940 = CARTESIAN_POINT ( 'NONE',  ( 22.64063804623240017, -20.68033422096370089, -59.71818801013959899 ) ) ;
#30941 = CARTESIAN_POINT ( 'NONE',  ( 21.90854117136780133, -20.69689202967290242, -32.14999999999999858 ) ) ;
#30942 = CARTESIAN_POINT ( 'NONE',  ( 55.82040737148000176, -50.78110051580220130, -75.19538818979980022 ) ) ;
#30944 = DIRECTION ( 'NONE',  ( -0.9987374001630935361, 0.000000000000000000, -0.05023550054955997629 ) ) ;
#30943 = CARTESIAN_POINT ( 'NONE',  ( -2.275804916070590433, 19.87795878944950090, -7.555165436777629751 ) ) ;
#30945 = DIRECTION ( 'NONE',  ( 0.000000000000000000, 0.000000000000000000, 1.000000000000000000 ) ) ;
#30946 = LINE ( 'NONE', #14210, #3865 ) ;
#30947 = VERTEX_POINT ( 'NONE', #11115 ) ;
#30948 = DIRECTION ( 'NONE',  ( 1.000000000000000000, 2.460964292799963328E-14, 0.000000000000000000 ) ) ;
#30949 = CARTESIAN_POINT ( 'NONE',  ( 47.72868234502399787, 23.24232774156940096, -54.87766230676579937 ) ) ;
#30950 = ADVANCED_FACE ( 'NONE', ( #50431 ), #22366, .F. ) ;
#30951 = DIRECTION ( 'NONE',  ( -1.000000000000000000, 0.000000000000000000, 0.000000000000000000 ) ) ;
#30952 = DIRECTION ( 'NONE',  ( 0.000000000000000000, 1.000000000000000000, 0.000000000000000000 ) ) ;
#30953 = CARTESIAN_POINT ( 'NONE',  ( 61.05708818547999783, 14.47205664048929918, -47.78546709072629994 ) ) ;
#30954 = CARTESIAN_POINT ( 'NONE',  ( 11.84787507268790030, 34.05753326919850110, -17.04454487390190209 ) ) ;
#30955 = CARTESIAN_POINT ( 'NONE',  ( 51.96022074122749501, 18.76462827808190070, -76.69846447276000845 ) ) ;
#30956 = CARTESIAN_POINT ( 'NONE',  ( 53.43246109071290562, 18.11429855641319975, -48.81566079190549345 ) ) ;
#30957 = FACE_OUTER_BOUND ( 'NONE', #32316, .T. ) ;
#30958 = DIRECTION ( 'NONE',  ( 0.000000000000000000, 1.000000000000000000, 0.000000000000000000 ) ) ;
#30959 = CARTESIAN_POINT ( 'NONE',  ( 54.84972377084940121, 16.62358603453460049, -26.66243130723649912 ) ) ;
#30960 = CARTESIAN_POINT ( 'NONE',  ( 13.00414154252432120, 18.14234304701931322, -34.70142521051216278 ) ) ;
#30961 = CIRCLE ( 'NONE', #26776, 0.5000000000000004441 ) ;
#30962 = LINE ( 'NONE', #40389, #16133 ) ;
#30963 = VECTOR ( 'NONE', #49416, 1000.000000000000000 ) ;
#30964 = CARTESIAN_POINT ( 'NONE',  ( 53.02879948416539690, 18.37809327181799901, -49.09530617495999394 ) ) ;
#30965 = CARTESIAN_POINT ( 'NONE',  ( 62.27952691711369937, -30.53997204947359734, -16.33238526922729861 ) ) ;
#30966 = CARTESIAN_POINT ( 'NONE',  ( 71.26289196806200721, 1.269319268680890067, -60.73450645366870049 ) ) ;
#30967 = CARTESIAN_POINT ( 'NONE',  ( 11.13393739769619906, 32.22978334998650496, -43.92380911455280312 ) ) ;
#30968 = CARTESIAN_POINT ( 'NONE',  ( 72.65319675752509454, 1.258806274519030044, -61.81501369061300721 ) ) ;
#30969 = VECTOR ( 'NONE', #3735, 1000.000000000000000 ) ;
#30970 = AXIS2_PLACEMENT_3D ( 'NONE', #24180, #16090, #11656 ) ;
#30971 = AXIS2_PLACEMENT_3D ( 'NONE', #28399, #24454, #4827 ) ;
#30972 = CARTESIAN_POINT ( 'NONE',  ( 51.13861002788090104, -34.97236549711250575, -76.48487255855283706 ) ) ;
#30973 = DIRECTION ( 'NONE',  ( 0.3863301728269200042, -0.9223605572462009183, 0.000000000000000000 ) ) ;
#30974 = ORIENTED_EDGE ( 'NONE', *, *, #31501, .T. ) ;
#30975 = ORIENTED_EDGE ( 'NONE', *, *, #44228, .F. ) ;
#30976 = B_SPLINE_CURVE_WITH_KNOTS ( 'NONE', 3,
 ( #23215, #18787, #46854, #10942, #3078, #36836, #24761, #8809, #36308, #28185, #24496, #35811, #23981, #8286, #40771, #20319, #15897, #36061, #4872, #12477, #11976, #48381, #43681, #40514, #23731, #51794, #4093, #3849, #44187, #11716, #27680, #20577, #7781, #48123, #32104, #12222, #673, #39747, #27931, #19823, #48647, #418, #168, #40005, #43933, #24234, #40259, #20839, #4351, #28445, #31854, #47873, #8030, #16662, #20067, #16405, #941, #16937, #44704, #32362, #47615, #44447, #8553, #4603, #16145, #36570, #32619, #12747, #28702, #1459, #33414, #33926, #28967, #38141, #5147, #45491, #41290, #13781, #49432, #14034, #10106, #9589, #32881, #45751, #49943, #5400, #29224, #42073, #2241, #21101, #13529, #9339, #29993, #49687, #21357, #33672, #25543, #48915, #13269, #13012, #1720, #46015, #29486, #26066, #9845, #6175, #21877, #37360, #29735, #37887, #22134, #17958, #41547, #44966, #17449, #25798, #5663, #21610, #41806, #37614, #1201, #17704, #9069, #25017, #17193, #41031, #5912, #1979, #37104, #45231, #33150, #49177, #25286, #51239, #50710, #18988, #38925, #23162, #42600, #31283, #27113, #38674, #14809, #50459, #50200, #2759, #7466, #39179, #10629, #14292, #42337, #6436, #22654, #11404, #26328, #23419, #34182, #2498, #43116, #15065, #27366, #35232, #47316, #22395, #11143, #19250 ),
 .UNSPECIFIED., .F., .F.,
 ( 4, 2, 2, 2, 2, 1, 1, 2, 2, 2, 2, 1, 1, 1, 2, 2, 2, 2, 1, 1, 1, 2, 2, 2, 2, 1, 1, 1, 2, 2, 2, 2, 1, 1, 1, 2, 2, 2, 2, 1, 1, 2, 2, 2, 2, 1, 1, 2, 2, 2, 2, 1, 1, 2, 2, 2, 2, 1, 1, 2, 2, 2, 2, 1, 1, 2, 2, 2, 2, 1, 1, 2, 2, 2, 2, 1, 1, 1, 2, 2, 2, 2, 1, 1, 1, 2, 2, 2, 2, 1, 1, 1, 2, 2, 2, 2, 1, 1, 1, 2, 2, 4 ),
 ( 0.000000000000000000, 0.007812499999983147161, 0.01562499999996629432, 0.03124999999993430255, 0.04687499999990230731, 0.05468749999988631316, 0.05859374999987772281, 0.06054687499987279620, 0.06249999999986786958, 0.09374999999980140886, 0.1093749999997681993, 0.1171874999997514766, 0.1210937499997431221, 0.1230468749997389588, 0.1240234374997369882, 0.1249999999997350175, 0.1562499999996768141, 0.1718749999996477262, 0.1796874999996338484, 0.1835937499996276034, 0.1855468749996250499, 0.1865234374996244116, 0.1874999999996237732, 0.2187499999995946853, 0.2343749999995808353, 0.2421874999995740352, 0.2460937499995706490, 0.2480468749995677347, 0.2490234374995661526, 0.2499999999995645705, 0.2812499999995325406, 0.2968749999995165534, 0.3046874999995086153, 0.3085937499995046185, 0.3105468749995026201, 0.3115234374995022315, 0.3124999999995018429, 0.3437499999994832467, 0.3593749999994740318, 0.3671874999994684807, 0.3710937499994668154, 0.3730468749994660937, 0.3749999999994653721, 0.4062499999994700350, 0.4218749999994716449, 0.4296874999994724775, 0.4335937499994735878, 0.4355468749994740874, 0.4374999999994745870, 0.4687499999994834132, 0.4843749999994878541, 0.4921874999994891864, 0.4960937499994897415, 0.4980468749994909627, 0.4999999999994921840, 0.5312499999995180522, 0.5468749999995308197, 0.5546874999995378142, 0.5585937499995413669, 0.5605468749995424771, 0.5624999999995435873, 0.5937499999995519140, 0.6093749999995561328, 0.6171874999995581312, 0.6210937499995600186, 0.6230468749995621280, 0.6249999999995642375, 0.6562499999995939914, 0.6718749999996094235, 0.6796874999996179723, 0.6835937499996220801, 0.6855468749996240785, 0.6874999999996260769, 0.7187499999996537214, 0.7343749999996674882, 0.7421874999996742606, 0.7460937499996777023, 0.7480468749996793676, 0.7490234374996802558, 0.7499999999996811439, 0.7812499999997200018, 0.7968749999997398747, 0.8046874999997497557, 0.8085937499997547517, 0.8105468749997569722, 0.8115234374997581934, 0.8124999999997594147, 0.8437499999997956079, 0.8593749999998133715, 0.8671874999998223643, 0.8710937499998268052, 0.8730468749998290257, 0.8740234374998301359, 0.8749999999998312461, 0.9062499999998698819, 0.9218749999998896438, 0.9296874999998994138, 0.9335937499999042988, 0.9355468749999069633, 0.9365234374999084066, 0.9374999999999098499, 1.000000000000000000 ),
 .UNSPECIFIED. ) ;
#30977 = CARTESIAN_POINT ( 'NONE',  ( 22.90131613704217628, -15.82328094948992359, -36.85691428242716938 ) ) ;
#30978 = CARTESIAN_POINT ( 'NONE',  ( 68.13393739845098196, -29.66618894551239904, -65.65000000119469803 ) ) ;
#30979 = EDGE_LOOP ( 'NONE', ( #39567, #42614, #48255, #9 ) ) ;
#30980 = CARTESIAN_POINT ( 'NONE',  ( 11.13393758244130005, -63.50662458344459793, -43.95118814396819573 ) ) ;
#30981 = CARTESIAN_POINT ( 'NONE',  ( 56.99918881514469859, -45.18030430956060428, -25.37149625033120159 ) ) ;
#30982 = CARTESIAN_POINT ( 'NONE',  ( 16.02066548673491653, -23.52649381719373878, -78.01222798080634391 ) ) ;
#30983 = EDGE_CURVE ( 'NONE', #43431, #47622, #46260, .T. ) ;
#30984 = CYLINDRICAL_SURFACE ( 'NONE', #31774, 3.000000000000000444 ) ;
#30985 = VERTEX_POINT ( 'NONE', #12659 ) ;
#30986 = CARTESIAN_POINT ( 'NONE',  ( 11.29751794088404360, 33.95857977818198492, -22.86704619065415756 ) ) ;
#30987 = CARTESIAN_POINT ( 'NONE',  ( 43.48293223442611577, 6.614494798211716819, -72.90498134187569690 ) ) ;
#30988 = CARTESIAN_POINT ( 'NONE',  ( 42.75216321632269967, -44.98233172091430276, -6.093641062779489914 ) ) ;
#30989 = EDGE_CURVE ( 'NONE', #41820, #8182, #3746, .T. ) ;
#30990 = EDGE_LOOP ( 'NONE', ( #22533, #964, #19299, #5967 ) ) ;
#30991 = CARTESIAN_POINT ( 'NONE',  ( 17.66316605052760025, -7.514079356226750050, -37.35171219075489546 ) ) ;
#30992 = CARTESIAN_POINT ( 'NONE',  ( 51.68174538021649767, 1.214832132191203673, -18.13120047747256436 ) ) ;
#30993 = CARTESIAN_POINT ( 'NONE',  ( 8.714124674500926204, -18.45117587401020032, -50.67606243729918702 ) ) ;
#30994 = AXIS2_PLACEMENT_3D ( 'NONE', #977, #43969, #28224 ) ;
#30995 = CARTESIAN_POINT ( 'NONE',  ( 60.79941944348659888, -29.22537550237669990, -15.89275653899559870 ) ) ;
#30996 = CARTESIAN_POINT ( 'NONE',  ( 16.13393739769620083, 30.88381105532059934, 11.84999999999999964 ) ) ;
#30997 = CARTESIAN_POINT ( 'NONE',  ( 47.19472346965950038, -54.65936592792999704, -74.80901628187270092 ) ) ;
#30998 = CARTESIAN_POINT ( 'NONE',  ( 55.69411755635510275, 14.72515888537330042, -17.00763503960670064 ) ) ;
#30999 = CARTESIAN_POINT ( 'NONE',  ( 15.05440318628110141, 21.88381105532300097, -76.14999999999999147 ) ) ;
#31000 =( BOUNDED_CURVE ( )  B_SPLINE_CURVE ( 3, ( #14530, #50950, #22892, #47040 ),
 .UNSPECIFIED., .F., .F. ) 
 B_SPLINE_CURVE_WITH_KNOTS ( ( 4, 4 ),
 ( 3.802771094680959862, 3.909080582966734774 ),
 .UNSPECIFIED. ) 
 CURVE ( )  GEOMETRIC_REPRESENTATION_ITEM ( )  RATIONAL_B_SPLINE_CURVE ( ( 1.000000000000000000, 0.9990584127885050458, 0.9990584127885050458, 1.000000000000000000 ) ) 
 REPRESENTATION_ITEM ( '' )  );
#31001 = CIRCLE ( 'NONE', #11768, 5.500000000000005329 ) ;
#31002 = CARTESIAN_POINT ( 'NONE',  ( 61.74535513545370691, 13.88381108448669998, -28.01209385561339715 ) ) ;
#31003 = CIRCLE ( 'NONE', #15992, 0.9999999999999964473 ) ;
#31004 = CARTESIAN_POINT ( 'NONE',  ( 8.877163880441720778, -12.62854938784190040, -80.41182290828409407 ) ) ;
#31005 = B_SPLINE_SURFACE_WITH_KNOTS ( 'NONE', 3, 3, ( 
 ( #33127, #49155, #29201, #45211, #33652, #37588 ),
 ( #9320, #1701, #17936, #21337, #37341, #45469 ),
 ( #9569, #25778, #17683, #49670, #41785, #5892 ),
 ( #45990, #26829, #11120, #51466, #26561, #51211 ),
 ( #10606, #27344, #19224, #38648, #46774, #47537 ),
 ( #2994, #50687, #23141, #6932, #23389, #19482 ),
 ( #2736, #11634, #35474, #42315, #22633, #18964 ),
 ( #47036, #43348, #15305, #15565, #31259, #43093 ),
 ( #22371, #15039, #47291, #7442, #11381, #2467 ),
 ( #18456, #39415, #34944, #42837, #22886, #31519 ),
 ( #39156, #42575, #38377, #6668, #3515, #18709 ),
 ( #27089, #6413, #34425, #3251, #50436, #7185 ),
 ( #35210, #14525, #34685, #30495, #14783, #30752 ),
 ( #46517, #10860, #38904, #50945, #31009, #40174 ),
 ( #8468, #44109, #8725, #4788, #12665, #39925 ),
 ( #20756, #27596, #7950, #23649, #43603, #39665 ) ),
 .UNSPECIFIED., .F., .F., .F.,
 ( 4, 2, 2, 2, 2, 2, 2, 4 ),
 ( 4, 1, 1, 4 ),
 ( 9.575042469628741060, 13.03139574839190118, 27.92441946083980042, 37.23255928111969837, 41.88662919125970063, 49.33314104748369999, 61.24756001744199807, 64.89007609261069831 ),
 ( -0.001356146170799000074, 0.3333333333333329818, 0.6666666666666670737, 1.001373499198290107 ),
 .UNSPECIFIED. ) ;
#31006 = VERTEX_POINT ( 'NONE', #23894 ) ;
#31007 = DIRECTION ( 'NONE',  ( -0.3618033988749886909, -0.2628655560595661855, 0.8944271909999162995 ) ) ;
#31008 = CARTESIAN_POINT ( 'NONE',  ( 8.625847590987680391, -62.42720030092139893, -14.82880704068799993 ) ) ;
#31009 = CARTESIAN_POINT ( 'NONE',  ( 75.63587938996879245, 9.758298940360759843, -13.13773444762449927 ) ) ;
#31010 = CARTESIAN_POINT ( 'NONE',  ( 75.42809886163706778, 12.76391134240307679, -13.58404645785000220 ) ) ;
#31011 = CARTESIAN_POINT ( 'NONE',  ( 17.49475137708000005, -51.11618894467930119, -15.67743210564179890 ) ) ;
#31012 = LINE ( 'NONE', #11124, #2152 ) ;
#31013 = CARTESIAN_POINT ( 'NONE',  ( 47.21773113835070035, 23.54756601831279639, -54.61692783540039642 ) ) ;
#31014 = EDGE_CURVE ( 'NONE', #3841, #39608, #6079, .T. ) ;
#31015 = CARTESIAN_POINT ( 'NONE',  ( 82.57809707948020161, -45.19656880909330710, -47.00698240636869940 ) ) ;
#31016 = CARTESIAN_POINT ( 'NONE',  ( 57.36818733098329659, -50.13385377957740019, -52.61777321114799832 ) ) ;
#31017 = CARTESIAN_POINT ( 'NONE',  ( 42.93197233849409855, 11.32569894967160096, -3.307825584507050110 ) ) ;
#31018 = CARTESIAN_POINT ( 'NONE',  ( 47.58822566456690595, -54.46711296473307584, -74.72768729673299504 ) ) ;
#31019 = CARTESIAN_POINT ( 'NONE',  ( 68.57574012094990223, -45.11618894467940066, -13.49754435276109987 ) ) ;
#31020 = CARTESIAN_POINT ( 'NONE',  ( 58.65392622551220114, -46.60947465638219711, -47.57606315241160644 ) ) ;
#31021 = CARTESIAN_POINT ( 'NONE',  ( 56.55522360613520760, 14.97957722649010037, -26.26695323647559732 ) ) ;
#31022 = EDGE_CURVE ( 'NONE', #22850, #40057, #3568, .T. ) ;
#31023 = CARTESIAN_POINT ( 'NONE',  ( 67.02526494145590163, -1.318240963702770108, -17.24421836522840223 ) ) ;
#31024 = CARTESIAN_POINT ( 'NONE',  ( 17.87259706178020124, -51.26000396899109290, -74.91994212300129163 ) ) ;
#31025 = CARTESIAN_POINT ( 'NONE',  ( 58.83289924021099893, -43.75437917904619667, -8.825342791311319601 ) ) ;
#31026 = EDGE_CURVE ( 'NONE', #26336, #37382, #34480, .T. ) ;
#31027 = CARTESIAN_POINT ( 'NONE',  ( 19.23095358872740235, -8.840114487382349395, -60.70380296398279540 ) ) ;
#31028 = CARTESIAN_POINT ( 'NONE',  ( 63.78947450026019084, 1.274155933524790063, -61.60356854227319445 ) ) ;
#31029 = ORIENTED_EDGE ( 'NONE', *, *, #23856, .F. ) ;
#31030 = CARTESIAN_POINT ( 'NONE',  ( 53.63393739769619373, -53.11618894467930119, 17.35000000000000142 ) ) ;
#31031 = CARTESIAN_POINT ( 'NONE',  ( 61.30872397726910350, -45.59477435387500321, -47.67209317366800292 ) ) ;
#31032 = CARTESIAN_POINT ( 'NONE',  ( 73.15215840802929392, 0.9242073871622918935, -68.93904330669420233 ) ) ;
#31033 = CARTESIAN_POINT ( 'NONE',  ( 15.24822436422556216, -8.849178651065907175, -73.91115355493535333 ) ) ;
#31034 = CARTESIAN_POINT ( 'NONE',  ( 9.205734167420709824, -3.616188944679339823, -32.14999999999999858 ) ) ;
#31035 = CARTESIAN_POINT ( 'NONE',  ( 45.32091058997599475, -45.57449214110749836, -8.659579893190318955 ) ) ;
#31036 = ORIENTED_EDGE ( 'NONE', *, *, #5224, .T. ) ;
#31037 = CARTESIAN_POINT ( 'NONE',  ( 17.95470215398700375, 20.84016670874339638, -75.79682998878489286 ) ) ;
#31038 = ORIENTED_EDGE ( 'NONE', *, *, #44423, .T. ) ;
#31039 = ORIENTED_EDGE ( 'NONE', *, *, #41038, .T. ) ;
#31040 = DIRECTION ( 'NONE',  ( 0.9441882088883221114, 0.3294064756440929775, 0.000000000000000000 ) ) ;
#31041 = CARTESIAN_POINT ( 'NONE',  ( -31.36606260230380272, 21.88381105532059934, 16.35000000000000142 ) ) ;
#31042 = AXIS2_PLACEMENT_3D ( 'NONE', #30159, #47209, #6331 ) ;
#31043 = CARTESIAN_POINT ( 'NONE',  ( 16.13393739769620083, -15.61618894467929941, -11.54999999999999893 ) ) ;
#31044 = VECTOR ( 'NONE', #40209, 1000.000000000000000 ) ;
#31045 = ORIENTED_EDGE ( 'NONE', *, *, #43594, .F. ) ;
#31046 = EDGE_CURVE ( 'NONE', #2118, #27635, #41199, .T. ) ;
#31047 = DIRECTION ( 'NONE',  ( 0.000000000000000000, 0.000000000000000000, -1.000000000000000000 ) ) ;
#31048 = VERTEX_POINT ( 'NONE', #28613 ) ;
#31049 = CARTESIAN_POINT ( 'NONE',  ( 12.86517331568640010, -49.11618894467930829, -34.64999999999999858 ) ) ;
#31050 = B_SPLINE_CURVE_WITH_KNOTS ( 'NONE', 3,
 ( #16050, #27837, #31752, #35961, #572, #7935, #47773, #8708, #51448, #39648, #32006, #43835, #16558, #16304, #39908, #321, #4003, #32258 ),
 .UNSPECIFIED., .F., .F.,
 ( 4, 2, 2, 2, 2, 2, 2, 2, 4 ),
 ( 0.4999985970897953269, 0.5624987724535709388, 0.6249989478173465507, 0.6874991231811220516, 0.7499992985448976635, 0.8124994739086732753, 0.8749996492724487762, 0.9374998246362243881, 1.000000000000000000 ),
 .UNSPECIFIED. ) ;
#31051 = CARTESIAN_POINT ( 'NONE',  ( 57.24929578595760660, -50.61618894467930119, -74.14999999999999147 ) ) ;
#31052 = VERTEX_POINT ( 'NONE', #44357 ) ;
#31053 = DIRECTION ( 'NONE',  ( 0.1961161351381830731, 0.000000000000000000, 0.9805806756909203337 ) ) ;
#31054 = CARTESIAN_POINT ( 'NONE',  ( 52.71259601604019451, -51.43286903184419856, -75.79898490202970152 ) ) ;
#31055 = CARTESIAN_POINT ( 'NONE',  ( 60.49619678835889403, 14.44108935951489947, -47.41857351171270096 ) ) ;
#31056 = CARTESIAN_POINT ( 'NONE',  ( 16.13393739769620083, -15.61618894467929941, -11.11999999999999922 ) ) ;
#31057 = DIRECTION ( 'NONE',  ( 0.000000000000000000, -1.000000000000000000, 0.000000000000000000 ) ) ;
#31058 = CARTESIAN_POINT ( 'NONE',  ( -7.616907281497659277, 14.17406059737050050, -5.566654447284809848 ) ) ;
#31059 = CARTESIAN_POINT ( 'NONE',  ( 64.27705669950368872, 1.080042774363660030, -70.23909358936700187 ) ) ;
#31060 = DIRECTION ( 'NONE',  ( 0.000000000000000000, 0.000000000000000000, 1.000000000000000000 ) ) ;
#31061 = CARTESIAN_POINT ( 'NONE',  ( 23.11702576777929607, -19.19714202993379715, -57.43833289983449930 ) ) ;
#31062 = EDGE_LOOP ( 'NONE', ( #33420, #8514, #19556, #10255, #7352, #46271, #16870, #12494 ) ) ;
#31063 = FACE_OUTER_BOUND ( 'NONE', #23614, .T. ) ;
#31064 = B_SPLINE_CURVE_WITH_KNOTS ( 'NONE', 3,
 ( #13000, #21598, #33403, #1448, #25532, #18204, #45218, #44954, #33661, #34170, #5132, #45738, #38130, #49676, #49420, #13765, #13516, #29473 ),
 .UNSPECIFIED., .F., .F.,
 ( 4, 2, 2, 2, 2, 2, 2, 2, 4 ),
 ( 0.000000000000000000, 0.06250000039148076447, 0.1250000007829615289, 0.1875000011744422934, 0.2500000015659230579, 0.3125000019574037391, 0.3750000023488843648, 0.4375000027403650460, 0.5000000031318456717 ),
 .UNSPECIFIED. ) ;
#31065 = CARTESIAN_POINT ( 'NONE',  ( 57.43631978869650112, 18.92123149693339812, -52.64527532753600525 ) ) ;
#31066 = CARTESIAN_POINT ( 'NONE',  ( 71.80939745721281042, 1.439519383694590093, -70.03165268182070236 ) ) ;
#31067 = CARTESIAN_POINT ( 'NONE',  ( 45.15893990696358173, -40.04164385324116182, -61.04083920648312755 ) ) ;
#31068 = CARTESIAN_POINT ( 'NONE',  ( 14.01533392343269924, 19.26065124468200196, -21.05253849812200073 ) ) ;
#31069 = AXIS2_PLACEMENT_3D ( 'NONE', #25471, #21029, #37030 ) ;
#31070 = CARTESIAN_POINT ( 'NONE',  ( 63.26785353957599511, 1.102139304147789822, -69.09899266709390986 ) ) ;
#31071 = CARTESIAN_POINT ( 'NONE',  ( 48.02285049171399578, -54.32307516229949584, -54.84930373619759791 ) ) ;
#31072 = DIRECTION ( 'NONE',  ( -1.000000000000000000, 0.000000000000000000, 0.000000000000000000 ) ) ;
#31073 = ADVANCED_FACE ( 'NONE', ( #29588 ), #32018, .T. ) ;
#31074 = CARTESIAN_POINT ( 'NONE',  ( 56.39270784037419304, 19.29512405589720103, -52.86271187285759510 ) ) ;
#31075 = CARTESIAN_POINT ( 'NONE',  ( 47.64143405403320486, 23.30250925608009993, -55.14905519569659731 ) ) ;
#31076 = EDGE_CURVE ( 'NONE', #28912, #11278, #46332, .T. ) ;
#31077 = ORIENTED_EDGE ( 'NONE', *, *, #12652, .T. ) ;
#31078 = CARTESIAN_POINT ( 'NONE',  ( 20.76651019224579997, -21.45108085822009869, -35.35374502362449789 ) ) ;
#31079 = ORIENTED_EDGE ( 'NONE', *, *, #44488, .F. ) ;
#31080 = CARTESIAN_POINT ( 'NONE',  ( 71.46564822584178955, 0.9966178393190270324, -70.63122704464430512 ) ) ;
#31081 = CARTESIAN_POINT ( 'NONE',  ( 60.52694424712060339, -45.62814803647550121, -47.19145984235160540 ) ) ;
#31082 = DIRECTION ( 'NONE',  ( 1.000000000000000000, 0.000000000000000000, 0.000000000000000000 ) ) ;
#31083 = CARTESIAN_POINT ( 'NONE',  ( 50.03007040746459921, 17.38381105532069881, -76.14999999999999147 ) ) ;
#31085 = CARTESIAN_POINT ( 'NONE',  ( 61.75019796695539753, -45.11618894467940066, -46.37203261889099792 ) ) ;
#31084 = FACE_OUTER_BOUND ( 'NONE', #48955, .T. ) ;
#31086 = FACE_BOUND ( 'NONE', #40529, .T. ) ;
#31087 = CARTESIAN_POINT ( 'NONE',  ( 17.16954876375649874, -23.52717981931520086, -41.96600113731807369 ) ) ;
#31088 = FACE_OUTER_BOUND ( 'NONE', #50455, .T. ) ;
#31089 = EDGE_LOOP ( 'NONE', ( #3857, #15068, #25941, #25500, #5160 ) ) ;
#31090 = FACE_OUTER_BOUND ( 'NONE', #18281, .T. ) ;
#31091 = ORIENTED_EDGE ( 'NONE', *, *, #47568, .T. ) ;
#31092 = ORIENTED_EDGE ( 'NONE', *, *, #21330, .T. ) ;
#31093 = CARTESIAN_POINT ( 'NONE',  ( 0.2609591194317604779, -26.58175058825759152, -34.64999999999999147 ) ) ;
#31094 = DIRECTION ( 'NONE',  ( 0.9858858899415445798, 2.580012592456886595E-12, -0.1674186728360041176 ) ) ;
#31095 = CARTESIAN_POINT ( 'NONE',  ( 12.91917450909959975, 34.27891870249889905, -47.58062843006289455 ) ) ;
#31096 = CARTESIAN_POINT ( 'NONE',  ( 10.32255761268189964, -64.75990130589950411, -46.96739154628469493 ) ) ;
#31097 = AXIS2_PLACEMENT_3D ( 'NONE', #18058, #42438, #6273 ) ;
#31098 = VERTEX_POINT ( 'NONE', #4515 ) ;
#31099 = VERTEX_POINT ( 'NONE', #40422 ) ;
#31100 = EDGE_CURVE ( 'NONE', #5359, #2490, #2783, .T. ) ;
#31101 = CARTESIAN_POINT ( 'NONE',  ( 19.13393739769600188, 18.38381105532069881, -35.14999999999999858 ) ) ;
#31102 = DIRECTION ( 'NONE',  ( 1.000000000000000000, 0.000000000000000000, 0.000000000000000000 ) ) ;
#31103 = CARTESIAN_POINT ( 'NONE',  ( 23.83903735962793746, -17.68686596444559100, -69.59100467832332981 ) ) ;
#31104 = DIRECTION ( 'NONE',  ( 0.000000000000000000, 0.000000000000000000, -1.000000000000000000 ) ) ;
#31105 = ADVANCED_FACE ( 'NONE', ( #35726 ), #4264, .T. ) ;
#31106 = CARTESIAN_POINT ( 'NONE',  ( 64.31467946070409880, -0.4499903462937720477, -16.60140817515059908 ) ) ;
#31107 = CARTESIAN_POINT ( 'NONE',  ( 51.73429016900899313, -49.15904133096110229, -76.96796945980311477 ) ) ;
#31108 = CARTESIAN_POINT ( 'NONE',  ( 19.31296351478360052, 18.65448050664020130, -82.14319696191608955 ) ) ;
#31109 = AXIS2_PLACEMENT_3D ( 'NONE', #27678, #31338, #11462 ) ;
#31110 = ORIENTED_EDGE ( 'NONE', *, *, #24642, .F. ) ;
#31111 = CARTESIAN_POINT ( 'NONE',  ( 63.23867883281540969, 0.9065823421260940096, -69.11945805671248877 ) ) ;
#31113 = DIRECTION ( 'NONE',  ( 0.000000000000000000, -1.000000000000000000, 0.000000000000000000 ) ) ;
#31112 = AXIS2_PLACEMENT_3D ( 'NONE', #42658, #50264, #21672 ) ;
#31114 = CARTESIAN_POINT ( 'NONE',  ( 0.3209249304026170480, -15.61618894467929941, -35.14999999999999858 ) ) ;
#31115 = CARTESIAN_POINT ( 'NONE',  ( 59.53476406250169362, -46.29126728519970158, -47.84522406268589378 ) ) ;
#31116 = CARTESIAN_POINT ( 'NONE',  ( 8.706976243475381239, -13.08103695608429895, -43.11720026785919657 ) ) ;
#31117 = CARTESIAN_POINT ( 'NONE',  ( 12.44378448573739959, -49.98269638858799624, -21.13285771745299968 ) ) ;
#31118 = CARTESIAN_POINT ( 'NONE',  ( 54.32114520510300082, 19.38381105532069881, -76.86722889149370985 ) ) ;
#31119 = CARTESIAN_POINT ( 'NONE',  ( 16.13393739769620083, -15.61618894467929941, -14.68999999999999950 ) ) ;
#31120 = CARTESIAN_POINT ( 'NONE',  ( 56.88018964337059913, 13.94865836461010034, -17.08460512071569681 ) ) ;
#31121 = CARTESIAN_POINT ( 'NONE',  ( 61.02921381188160410, -45.52723101486190416, -47.53466998951989808 ) ) ;
#31122 = CARTESIAN_POINT ( 'NONE',  ( 56.77563393664169666, -50.64689510413649742, -53.45922468511930248 ) ) ;
#31123 = CARTESIAN_POINT ( 'NONE',  ( 9.575305561104880070, -13.02256067399330064, -47.96704895327989959 ) ) ;
#31124 = CARTESIAN_POINT ( 'NONE',  ( 20.29254231923757956, -10.20481729065597598, -44.16112523059096873 ) ) ;
#31125 = ORIENTED_EDGE ( 'NONE', *, *, #39261, .F. ) ;
#31126 = CARTESIAN_POINT ( 'NONE',  ( 13.42256853332840016, -51.72201361531850239, -74.35192203308750436 ) ) ;
#31127 = CARTESIAN_POINT ( 'NONE',  ( 64.92925538503580185, 1.097085799869280009, -60.62778596399619602 ) ) ;
#31128 = CARTESIAN_POINT ( 'NONE',  ( 9.807850478269243055, -10.75441043811473918, -50.71600121525216309 ) ) ;
#31129 = CARTESIAN_POINT ( 'NONE',  ( 11.67620015026735203, -64.89165383396532150, -23.88711004025349283 ) ) ;
#31130 = CARTESIAN_POINT ( 'NONE',  ( 70.56223753246619879, 13.88381105532070059, -14.05824725777380024 ) ) ;
#31131 = CARTESIAN_POINT ( 'NONE',  ( 0.08375394646315241498, 19.63944928676770019, -34.70982966457259522 ) ) ;
#31132 = CARTESIAN_POINT ( 'NONE',  ( 82.39375047534959151, 13.90419211000809874, -46.71925512375379697 ) ) ;
#31133 = CARTESIAN_POINT ( 'NONE',  ( 13.00753648416289998, -8.313058068840117443, -64.87884994055072241 ) ) ;
#31135 = DIRECTION ( 'NONE',  ( 0.000000000000000000, -1.000000000000000000, 0.000000000000000000 ) ) ;
#31134 = CARTESIAN_POINT ( 'NONE',  ( 53.23465404654513122, 19.19659352034578959, -77.19488661914444094 ) ) ;
#31136 = EDGE_CURVE ( 'NONE', #43673, #29694, #19418, .T. ) ;
#31137 = DIRECTION ( 'NONE',  ( 0.000000000000000000, 0.000000000000000000, -1.000000000000000000 ) ) ;
#31138 = CARTESIAN_POINT ( 'NONE',  ( 49.47908289717140207, 22.45249353912830159, -54.66541287124849902 ) ) ;
#31139 = EDGE_LOOP ( 'NONE', ( #12180, #32232, #6578, #30897, #11673, #23695 ) ) ;
#31140 = CIRCLE ( 'NONE', #25266, 22.00000000000000355 ) ;
#31141 =( BOUNDED_CURVE ( )  B_SPLINE_CURVE ( 3, ( #40006, #28186, #28446, #28968 ),
 .UNSPECIFIED., .F., .T. ) 
 B_SPLINE_CURVE_WITH_KNOTS ( ( 4, 4 ),
 ( 1.570796326794886344, 2.356194490192476731 ),
 .UNSPECIFIED. ) 
 CURVE ( )  GEOMETRIC_REPRESENTATION_ITEM ( )  RATIONAL_B_SPLINE_CURVE ( ( 1.000000000000000000, 0.9492530216741729143, 0.9492530216741729143, 1.000000000000000000 ) ) 
 REPRESENTATION_ITEM ( '' )  );
#31142 = CARTESIAN_POINT ( 'NONE',  ( 53.10876379251020296, -49.52367567955289474, -48.93018545852340395 ) ) ;
#31143 = CIRCLE ( 'NONE', #36207, 39.00000000000000000 ) ;
#31144 = VERTEX_POINT ( 'NONE', #2338 ) ;
#31145 = CARTESIAN_POINT ( 'NONE',  ( 46.75983893905041100, 8.015321561625365021, -57.03879444339121818 ) ) ;
#31146 = CARTESIAN_POINT ( 'NONE',  ( 13.05928102721579975, -9.268823555959679439, -40.20359370904520091 ) ) ;
#31147 = CARTESIAN_POINT ( 'NONE',  ( 13.91186867058490151, 19.84412712960480007, -22.10133442523809677 ) ) ;
#31148 = CARTESIAN_POINT ( 'NONE',  ( 47.07753517504149698, -39.26143421117000543, -34.91082242604309727 ) ) ;
#31149 = CARTESIAN_POINT ( 'NONE',  ( 22.86441391394799894, -17.72408945485720366, -56.54943076759479936 ) ) ;
#31150 = CARTESIAN_POINT ( 'NONE',  ( 52.76221410082400354, 18.49020305563599820, -48.84748657229020097 ) ) ;
#31151 = CARTESIAN_POINT ( 'NONE',  ( 55.80275820535209874, -45.58445552780170118, -16.47843131335860178 ) ) ;
#31152 = CARTESIAN_POINT ( 'NONE',  ( 8.784728771152179760, 31.88305279685639704, -46.67204636145419983 ) ) ;
#31153 = VERTEX_POINT ( 'NONE', #6800 ) ;
#31154 = CARTESIAN_POINT ( 'NONE',  ( 15.06271142038569977, -23.39045548577020028, -33.83109144287589487 ) ) ;
#31155 = ORIENTED_EDGE ( 'NONE', *, *, #3182, .F. ) ;
#31156 = CARTESIAN_POINT ( 'NONE',  ( 11.71337184211249927, -65.28004931318540116, -17.10636605765209950 ) ) ;
#31157 = CARTESIAN_POINT ( 'NONE',  ( 11.14532849681570070, 33.83291464669790116, -47.04966230858290288 ) ) ;
#31158 = CARTESIAN_POINT ( 'NONE',  ( 73.10713808934470137, 0.9971903505820729485, -62.30620812933800323 ) ) ;
#31159 = CARTESIAN_POINT ( 'NONE',  ( 12.14969309051077317, -22.52864826167251522, -40.45900981262661134 ) ) ;
#31160 = CARTESIAN_POINT ( 'NONE',  ( 52.56949981068906652, -49.85724369911663700, -48.49331493222930334 ) ) ;
#31161 = CARTESIAN_POINT ( 'NONE',  ( 82.45630311851421368, -45.09271792554360303, -46.38988467804559690 ) ) ;
#31162 = CARTESIAN_POINT ( 'NONE',  ( 51.75362667781039505, -52.76185628017049822, -54.27263750760450023 ) ) ;
#31163 = ORIENTED_EDGE ( 'NONE', *, *, #20567, .T. ) ;
#31164 = CARTESIAN_POINT ( 'NONE',  ( 64.80710063092610085, 1.263823323415690147, -70.46116989902610328 ) ) ;
#31165 = CARTESIAN_POINT ( 'NONE',  ( 9.732699106784480136, -63.17170994995979783, -46.29943774989700245 ) ) ;
#31166 = CARTESIAN_POINT ( 'NONE',  ( 70.83393739769690001, 16.88381105531530579, -74.20000000000047180 ) ) ;
#31167 = ORIENTED_EDGE ( 'NONE', *, *, #37132, .T. ) ;
#31168 = ADVANCED_FACE ( 'NONE', ( #14907 ), #16014, .F. ) ;
#31169 = CARTESIAN_POINT ( 'NONE',  ( 23.91899059252033766, -17.05099851077971707, -43.85032385076039674 ) ) ;
#31170 = CARTESIAN_POINT ( 'NONE',  ( 57.19702054503510169, 19.38356614133159894, -53.75054411148590106 ) ) ;
#31171 = CARTESIAN_POINT ( 'NONE',  ( 12.13393739769649926, 24.18330853958550364, -23.15000000000000213 ) ) ;
#31172 = VERTEX_POINT ( 'NONE', #2864 ) ;
#31173 = CARTESIAN_POINT ( 'NONE',  ( 24.04493738681399151, -16.65173670305258113, -35.54933226178233241 ) ) ;
#31174 = CARTESIAN_POINT ( 'NONE',  ( 18.26295693003078213, -22.08338128206962736, -32.85173728777652258 ) ) ;
#31175 = CARTESIAN_POINT ( 'NONE',  ( 8.223569788570660677, -15.61625877447020017, -68.79233150823709764 ) ) ;
#31176 = CARTESIAN_POINT ( 'NONE',  ( 8.542109907880320208, -12.39953300709269968, -64.91990020089438929 ) ) ;
#31177 = CARTESIAN_POINT ( 'NONE',  ( 1.633937397696199056, -15.61618894467930119, -7.349999999999999645 ) ) ;
#31178 = CARTESIAN_POINT ( 'NONE',  ( 46.39112542121452520, -38.19271976108705502, -58.36405639519246336 ) ) ;
#31179 = ORIENTED_EDGE ( 'NONE', *, *, #35968, .T. ) ;
#31180 = ORIENTED_EDGE ( 'NONE', *, *, #51871, .T. ) ;
#31181 = CARTESIAN_POINT ( 'NONE',  ( 43.27084646103560317, -43.87227363443550132, -5.051381114840269859 ) ) ;
#31182 = CARTESIAN_POINT ( 'NONE',  ( 21.87051971591800026, -10.86242021751020026, -56.01239214068929329 ) ) ;
#31183 = AXIS2_PLACEMENT_3D ( 'NONE', #10914, #22679, #42361 ) ;
#31184 = CARTESIAN_POINT ( 'NONE',  ( 50.93004313118130000, -50.92639752731179925, -76.14999999999999147 ) ) ;
#31185 = CARTESIAN_POINT ( 'NONE',  ( 44.13393739769620083, -33.11618894467940066, -54.27132075603720551 ) ) ;
#31186 = CARTESIAN_POINT ( 'NONE',  ( 47.24352027743620397, 23.52783393649020027, -74.19756735715161255 ) ) ;
#31187 = DIRECTION ( 'NONE',  ( 1.000000000000000000, 0.000000000000000000, 0.000000000000000000 ) ) ;
#31188 = CARTESIAN_POINT ( 'NONE',  ( 0.1542402430813090142, -50.99248106341759978, -19.14999999999999858 ) ) ;
#31189 = CARTESIAN_POINT ( 'NONE',  ( 11.66836325772959881, 33.74040207072849995, -16.48189043737649939 ) ) ;
#31190 = CARTESIAN_POINT ( 'NONE',  ( 8.020540499375330867, -17.08435497047219798, -58.45068511312169335 ) ) ;
#31191 = CARTESIAN_POINT ( 'NONE',  ( 52.58769281011270635, -49.83788694981130618, -27.98708932276760208 ) ) ;
#31192 = AXIS2_PLACEMENT_3D ( 'NONE', #5126, #29717, #25523 ) ;
#31193 = CARTESIAN_POINT ( 'NONE',  ( 57.21119120591109208, -50.61618800962469322, -74.41418816113228729 ) ) ;
#31195 = CARTESIAN_POINT ( 'NONE',  ( 9.367243689500000414, -15.61633989587210003, -59.45282021618999835 ) ) ;
#31194 = CARTESIAN_POINT ( 'NONE',  ( -7.152478658582400506, 15.01426846172460117, -6.869100105340580242 ) ) ;
#31196 = EDGE_CURVE ( 'NONE', #19168, #14168, #18829, .T. ) ;
#31197 = DIRECTION ( 'NONE',  ( -1.000000000000000000, 0.000000000000000000, 0.000000000000000000 ) ) ;
#31198 = DIRECTION ( 'NONE',  ( 1.000000000000000000, 0.000000000000000000, 0.000000000000000000 ) ) ;
#31199 = EDGE_CURVE ( 'NONE', #9596, #9489, #28783, .T. ) ;
#31200 = ORIENTED_EDGE ( 'NONE', *, *, #16258, .F. ) ;
#31201 = CARTESIAN_POINT ( 'NONE',  ( 14.43858045676712720, 21.38896804172114230, -76.01806011802842988 ) ) ;
#31202 = EDGE_CURVE ( 'NONE', #47320, #12485, #27463, .T. ) ;
#31203 = CARTESIAN_POINT ( 'NONE',  ( 47.53404130184800636, 23.35181273068509711, -55.01564180042830543 ) ) ;
#31204 = CARTESIAN_POINT ( 'NONE',  ( 61.41267152474549817, -45.16781038087659539, -27.92979456378700220 ) ) ;
#31205 = FACE_OUTER_BOUND ( 'NONE', #29228, .T. ) ;
#31206 = CARTESIAN_POINT ( 'NONE',  ( 61.37892440507240366, 14.09575071485549991, -47.24517396406390191 ) ) ;
#31207 = CARTESIAN_POINT ( 'NONE',  ( 13.09659873358270055, -8.813155235764829953, -73.59899483681280685 ) ) ;
#31208 = B_SPLINE_CURVE_WITH_KNOTS ( 'NONE', 3,
 ( #39278, #11245, #27208, #19861, #43219, #35602, #10990, #50817, #26954, #31641, #39029, #15434, #23778, #39790, #14908, #35068, #15173, #51587 ),
 .UNSPECIFIED., .F., .F.,
 ( 4, 2, 2, 2, 2, 2, 2, 2, 4 ),
 ( 0.000000000000000000, 0.06250008666983568328, 0.1250001733396713666, 0.1875002600095070637, 0.2500003466793427331, 0.3125004333491783193, 0.3750005200190139054, 0.4375006066888494360, 0.5000006933586850222 ),
 .UNSPECIFIED. ) ;
#31209 = ADVANCED_FACE ( 'NONE', ( #43217 ), #49701, .F. ) ;
#31210 = CARTESIAN_POINT ( 'NONE',  ( 51.30775049128980214, 17.38380848247659571, -76.60305691058019306 ) ) ;
#31211 = CARTESIAN_POINT ( 'NONE',  ( 53.40534283797200032, 18.12842647251899919, -48.82229431740969972 ) ) ;
#31212 = FACE_OUTER_BOUND ( 'NONE', #3149, .T. ) ;
#31213 = CARTESIAN_POINT ( 'NONE',  ( 40.75465142538513419, -33.99486860111964859, -82.06602514716892927 ) ) ;
#31214 = CARTESIAN_POINT ( 'NONE',  ( 55.35735860040240652, 16.14714136825730151, -26.51181232951169875 ) ) ;
#31215 = CARTESIAN_POINT ( 'NONE',  ( 50.52790554252050015, 22.07298246124570085, -54.91101322106079863 ) ) ;
#31216 = AXIS2_PLACEMENT_3D ( 'NONE', #35480, #31526, #43860 ) ;
#31217 = CARTESIAN_POINT ( 'NONE',  ( 16.17501676180923553, -23.52709765870719849, -62.00601847604462336 ) ) ;
#31218 = CARTESIAN_POINT ( 'NONE',  ( 10.49497832658790131, -63.36864664907449196, -45.62743361653370044 ) ) ;
#31219 = CARTESIAN_POINT ( 'NONE',  ( 42.62644315548480023, 11.62703185229469938, -3.197525305353840608 ) ) ;
#31220 = CARTESIAN_POINT ( 'NONE',  ( 59.05823500560009620, -28.84314769625699881, -15.68946708767219711 ) ) ;
#31221 = CARTESIAN_POINT ( 'NONE',  ( 71.08986881540380409, 1.373356196620449943, -60.86873524938349789 ) ) ;
#31222 = CARTESIAN_POINT ( 'NONE',  ( 11.13393739769619906, 32.09516374018799922, -43.74800381802249660 ) ) ;
#31223 = VECTOR ( 'NONE', #46095, 1000.000000000000000 ) ;
#31224 = CARTESIAN_POINT ( 'NONE',  ( 72.53531777184440443, 1.426105412860890098, -61.95447814822819765 ) ) ;
#31225 = DIRECTION ( 'NONE',  ( -1.000000000000000000, 0.000000000000000000, 0.000000000000000000 ) ) ;
#31226 = DIRECTION ( 'NONE',  ( 0.2313469967918511672, -0.8455706941739528082, 0.4811327968758425389 ) ) ;
#31227 = ORIENTED_EDGE ( 'NONE', *, *, #3724, .F. ) ;
#31228 = ORIENTED_EDGE ( 'NONE', *, *, #35597, .F. ) ;
#31229 = CARTESIAN_POINT ( 'NONE',  ( 56.73072851102580216, 19.11736299019269936, -52.75329813363410381 ) ) ;
#31230 = CARTESIAN_POINT ( 'NONE',  ( 49.58944174246663295, -29.23728716619012857, -15.75935478527375189 ) ) ;
#31231 = EDGE_LOOP ( 'NONE', ( #11928, #47483, #33938, #43006 ) ) ;
#31232 = EDGE_CURVE ( 'NONE', #25171, #31048, #8690, .T. ) ;
#31233 = CARTESIAN_POINT ( 'NONE',  ( 56.07552736419609829, -45.72903556735669639, -25.51839513193560194 ) ) ;
#31234 = CARTESIAN_POINT ( 'NONE',  ( 15.68102735321344099, -23.51607019824295008, -78.02589618440929087 ) ) ;
#31235 = VERTEX_POINT ( 'NONE', #3381 ) ;
#31236 = CARTESIAN_POINT ( 'NONE',  ( -0.03447620312152044342, -8.421650097910747590, -34.79644660940672196 ) ) ;
#31237 = CARTESIAN_POINT ( 'NONE',  ( 42.95888890335680799, 6.539414064201790389, -75.52524143611269380 ) ) ;
#31238 = CARTESIAN_POINT ( 'NONE',  ( 12.64456732695109942, 34.26332736361320030, -22.97177317294229937 ) ) ;
#31239 = ORIENTED_EDGE ( 'NONE', *, *, #51114, .T. ) ;
#31240 = CARTESIAN_POINT ( 'NONE',  ( 46.03121482517249774, -45.11618894467940066, -7.582874669927740285 ) ) ;
#31241 = AXIS2_PLACEMENT_3D ( 'NONE', #3301, #140, #11174 ) ;
#31242 = CARTESIAN_POINT ( 'NONE',  ( 57.50723796702470025, -47.11618894467930119, -31.98003398042899903 ) ) ;
#31243 = DIRECTION ( 'NONE',  ( 0.000000000000000000, 1.000000000000000000, 0.000000000000000000 ) ) ;
#31244 = CARTESIAN_POINT ( 'NONE',  ( 59.46287080461119956, -28.41472307337230063, -15.69699063629330027 ) ) ;
#31245 = CARTESIAN_POINT ( 'NONE',  ( 72.33393739769618946, 10.88381105532070059, -62.44999999999999574 ) ) ;
#31246 = CARTESIAN_POINT ( 'NONE',  ( 46.41240425002109760, -53.01349718276490108, -76.14999999999999147 ) ) ;
#31247 = CARTESIAN_POINT ( 'NONE',  ( 21.55806612471909744, -9.944718664031841016, -75.75539986607049059 ) ) ;
#31248 = CARTESIAN_POINT ( 'NONE',  ( 9.366941535224629689, -16.50201745891097005, -37.41115343530533011 ) ) ;
#31249 = ADVANCED_FACE ( 'NONE', ( #51334 ), #20113, .T. ) ;
#31250 = CARTESIAN_POINT ( 'NONE',  ( 45.01575386057460548, 14.77919493983159960, -8.915118302820459917 ) ) ;
#31251 = CARTESIAN_POINT ( 'NONE',  ( -21.36606260230379917, 21.88381105532059934, 11.84999999999999964 ) ) ;
#31252 = AXIS2_PLACEMENT_3D ( 'NONE', #202, #32396, #31631 ) ;
#31253 = CARTESIAN_POINT ( 'NONE',  ( 84.39650841167420481, -43.49490765828570460, -47.35795223498069362 ) ) ;
#31254 = DIRECTION ( 'NONE',  ( 0.6339889056055360017, 0.000000000000000000, -0.7733421413379041320 ) ) ;
#31255 = CARTESIAN_POINT ( 'NONE',  ( 16.36649570679220034, -23.46046469067789886, -79.77807145977510572 ) ) ;
#31256 = ORIENTED_EDGE ( 'NONE', *, *, #1875, .T. ) ;
#31257 = CARTESIAN_POINT ( 'NONE',  ( 54.79698325214220489, -47.90516110802800398, -26.67907444486039736 ) ) ;
#31258 = CARTESIAN_POINT ( 'NONE',  ( -5.802364285079610440, -47.44218980195390145, -6.163383152730290249 ) ) ;
#31259 = CARTESIAN_POINT ( 'NONE',  ( 75.26680305930699433, -14.04978866029259876, -11.37374796283529932 ) ) ;
#31260 = DIRECTION ( 'NONE',  ( 0.000000000000000000, -0.7071067811865162644, -0.7071067811865786590 ) ) ;
#31261 = CARTESIAN_POINT ( 'NONE',  ( 12.89658887244659979, -50.00140126166379417, -21.06837794357040039 ) ) ;
#31262 = CARTESIAN_POINT ( 'NONE',  ( 13.87894895853409416, -55.55385804827719909, -76.14999999999999147 ) ) ;
#31263 = CARTESIAN_POINT ( 'NONE',  ( 47.21691115651439929, 23.54821565252409954, -54.61897267083390517 ) ) ;
#31264 = CARTESIAN_POINT ( 'NONE',  ( 82.26799080613189119, -45.14410041576280008, -46.71841345350929942 ) ) ;
#31265 = CARTESIAN_POINT ( 'NONE',  ( 57.27338646566600033, -50.61204626796450157, -53.75880438950069617 ) ) ;
#31266 = CARTESIAN_POINT ( 'NONE',  ( 42.25512407695530470, 12.46306899543039926, -4.476913604614050080 ) ) ;
#31267 = EDGE_CURVE ( 'NONE', #51550, #37751, #47917, .T. ) ;
#31268 = CARTESIAN_POINT ( 'NONE',  ( 68.13393739769620083, 1.883811055320669947, -60.94999999999999574 ) ) ;
#31269 = CARTESIAN_POINT ( 'NONE',  ( 64.36068579096159681, 0.9644290104359670712, -60.98409269229870233 ) ) ;
#31270 = CARTESIAN_POINT ( 'NONE',  ( 56.23228709081130461, -47.87823924875339543, -47.98841366488070292 ) ) ;
#31271 = DIRECTION ( 'NONE',  ( 0.8529225269813149879, 0.5196435251606980055, -0.04993765839895900061 ) ) ;
#31272 = AXIS2_PLACEMENT_3D ( 'NONE', #47635, #28661, #11743 ) ;
#31273 = CARTESIAN_POINT ( 'NONE',  ( 66.66723128061150305, -1.312581826788029815, -17.00552257602960182 ) ) ;
#31274 = CARTESIAN_POINT ( 'NONE',  ( 17.88460903198290097, -51.65751396603660339, -75.51495726157199329 ) ) ;
#31275 = CARTESIAN_POINT ( 'NONE',  ( 44.81421300434149657, -45.11618894467940066, -7.294680430930359449 ) ) ;
#31276 = CARTESIAN_POINT ( 'NONE',  ( 14.12092483504799922, -22.78936639689409915, -61.65443013674619976 ) ) ;
#31277 = CARTESIAN_POINT ( 'NONE',  ( 20.99566316520265730, -9.290061801217850856, -41.21600092569405405 ) ) ;
#31278 = CARTESIAN_POINT ( 'NONE',  ( 63.27838127973599569, 0.9150552061906049861, -62.12504221718990038 ) ) ;
#31279 = ORIENTED_EDGE ( 'NONE', *, *, #8251, .T. ) ;
#31280 = CARTESIAN_POINT ( 'NONE',  ( 8.792634198315560923, 31.92357537073090157, -46.67064936031920297 ) ) ;
#31281 = CARTESIAN_POINT ( 'NONE',  ( 17.18180055072906498, -22.35999544095330194, -34.90393729465625938 ) ) ;
#31282 = CARTESIAN_POINT ( 'NONE',  ( 72.78816252330430814, 1.385888765344509999, -68.65207957385619864 ) ) ;
#31283 = CARTESIAN_POINT ( 'NONE',  ( 45.40902987668481217, 8.825533465273407430, -59.82804123183892386 ) ) ;
#31284 = CARTESIAN_POINT ( 'NONE',  ( 11.24014119269209999, -9.776142739560269135, -81.23899999999999011 ) ) ;
#31285 = CARTESIAN_POINT ( 'NONE',  ( 40.72222851082409534, -45.28361251854680347, -5.660115265888800096 ) ) ;
#31286 = ORIENTED_EDGE ( 'NONE', *, *, #49415, .F. ) ;
#31287 = CARTESIAN_POINT ( 'NONE',  ( 17.77507174714839877, 21.09308431968760189, -75.96462645239850531 ) ) ;
#31288 = ORIENTED_EDGE ( 'NONE', *, *, #80, .T. ) ;
#31289 = CIRCLE ( 'NONE', #36338, 2.000000000000004441 ) ;
#31290 = ORIENTED_EDGE ( 'NONE', *, *, #31576, .F. ) ;
#31291 = EDGE_CURVE ( 'NONE', #48131, #26643, #43723, .T. ) ;
#31292 = CARTESIAN_POINT ( 'NONE',  ( 57.38548500607309677, -45.11618894467940066, -16.91114573195289950 ) ) ;
#31293 = CARTESIAN_POINT ( 'NONE',  ( 23.55096566107879852, -15.91424779115909871, -81.23899999999999011 ) ) ;
#31294 = AXIS2_PLACEMENT_3D ( 'NONE', #28955, #39994, #27921 ) ;
#31295 = CARTESIAN_POINT ( 'NONE',  ( 23.04647602230480885, -11.63208635115726253, -73.62566485141034889 ) ) ;
#31296 = ORIENTED_EDGE ( 'NONE', *, *, #6734, .F. ) ;
#31297 = DIRECTION ( 'NONE',  ( 0.4872913772396111898, 0.8732394366197182567, 0.000000000000000000 ) ) ;
#31298 = EDGE_LOOP ( 'NONE', ( #3873, #17261, #42760, #3609, #29684, #40018 ) ) ;
#31299 = CARTESIAN_POINT ( 'NONE',  ( 24.04516176800591865, -15.61618872104648226, -63.79232972929064971 ) ) ;
#31300 = CARTESIAN_POINT ( 'NONE',  ( 46.63393739769619373, -15.61618894467929941, -35.14999999999999858 ) ) ;
#31302 = VERTEX_POINT ( 'NONE', #39537 ) ;
#31301 =( BOUNDED_CURVE ( )  B_SPLINE_CURVE ( 2, ( #22651, #46277, #30771 ),
 .UNSPECIFIED., .F., .T. ) 
 B_SPLINE_CURVE_WITH_KNOTS ( ( 3, 3 ),
 ( 0.1321855491485360024, 2.139356573196280031 ),
 .UNSPECIFIED. ) 
 CURVE ( )  GEOMETRIC_REPRESENTATION_ITEM ( )  RATIONAL_B_SPLINE_CURVE ( ( 1.001093714210500085, 1.008874108803850200, 1.000760730680210209 ) ) 
 REPRESENTATION_ITEM ( '' )  );
#31303 = CARTESIAN_POINT ( 'NONE',  ( 45.14832757675640096, 2.060512883921409966, -35.14999999999999858 ) ) ;
#31304 = CARTESIAN_POINT ( 'NONE',  ( 51.81953057646069993, -51.23881869680439394, -76.05779032467960121 ) ) ;
#31305 = CARTESIAN_POINT ( 'NONE',  ( 61.23361899263159813, 14.35831534285940059, -47.66404968818600452 ) ) ;
#31306 = EDGE_CURVE ( 'NONE', #1545, #29700, #25612, .T. ) ;
#31307 = EDGE_CURVE ( 'NONE', #16677, #28918, #12806, .T. ) ;
#31308 = CARTESIAN_POINT ( 'NONE',  ( 13.13393739769600010, 18.38381105532060289, -35.14999999999999858 ) ) ;
#31309 = AXIS2_PLACEMENT_3D ( 'NONE', #46955, #38041, #22546 ) ;
#31310 = CARTESIAN_POINT ( 'NONE',  ( 12.26481034824478478, 34.23527980536555759, -22.60721090778044484 ) ) ;
#31311 = EDGE_CURVE ( 'NONE', #37505, #38543, #622, .T. ) ;
#31312 = CARTESIAN_POINT ( 'NONE',  ( -9.426225745850960180, 12.53465503246489909, -5.815077069593810322 ) ) ;
#31313 = CARTESIAN_POINT ( 'NONE',  ( 47.18058889863803529, 23.56890040466754499, -74.36261479959277665 ) ) ;
#31314 = CARTESIAN_POINT ( 'NONE',  ( 34.13393739769599478, 18.23736444591407135, -34.79644660940672907 ) ) ;
#31315 = AXIS2_PLACEMENT_3D ( 'NONE', #48693, #29015, #37150 ) ;
#31316 = CARTESIAN_POINT ( 'NONE',  ( 8.518398427704360287, -17.51100143664740116, -52.20988344963559769 ) ) ;
#31317 = ORIENTED_EDGE ( 'NONE', *, *, #5899, .F. ) ;
#31318 =( NAMED_UNIT ( * ) SI_UNIT ( $, .STERADIAN. ) SOLID_ANGLE_UNIT ( ) );
#31319 = COLOUR_RGB ( '', 0.09019608, 0.27058824, 0.51372549) ;
#31320 = DIRECTION ( 'NONE',  ( 1.000000000000000000, 0.000000000000000000, 0.000000000000000000 ) ) ;
#31321 = CARTESIAN_POINT ( 'NONE',  ( 71.40386387224138787, 1.392490173687920052, -70.25015106115239405 ) ) ;
#31322 = CARTESIAN_POINT ( 'NONE',  ( 44.88531378893124213, -40.02229542238428905, -62.36962640805702307 ) ) ;
#31323 = CARTESIAN_POINT ( 'NONE',  ( 15.33884134720609893, 19.72557400333539945, -21.05298682722020231 ) ) ;
#31324 = EDGE_CURVE ( 'NONE', #47971, #9060, #51586, .T. ) ;
#31325 = CARTESIAN_POINT ( 'NONE',  ( 12.22498195829099998, 18.79317371135340053, -21.14999999988710400 ) ) ;
#31326 = ADVANCED_FACE ( 'NONE', ( #15685 ), #51842, .T. ) ;
#31327 = CARTESIAN_POINT ( 'NONE',  ( -0.8554694999317272730, 0.5322876908067696311, 4.943674098299870145 ) ) ;
#31328 = CARTESIAN_POINT ( 'NONE',  ( 48.66886125943680952, -54.03308671629140036, -54.81979436189590160 ) ) ;
#31329 = DIRECTION ( 'NONE',  ( 0.000000000000000000, 0.000000000000000000, -1.000000000000000000 ) ) ;
#31330 = CARTESIAN_POINT ( 'NONE',  ( 63.92076813643380007, 1.033004454759739899, -69.92211063522330505 ) ) ;
#31331 = CARTESIAN_POINT ( 'NONE',  ( 20.99559669166361431, -9.290008747073166262, -71.50065479947573976 ) ) ;
#31332 = ORIENTED_EDGE ( 'NONE', *, *, #51496, .T. ) ;
#31333 = CARTESIAN_POINT ( 'NONE',  ( 21.77309873898569847, -20.48512569386770110, -33.29405281597039590 ) ) ;
#31334 = EDGE_LOOP ( 'NONE', ( #23646, #1020, #6013, #35943 ) ) ;
#31335 = CARTESIAN_POINT ( 'NONE',  ( 17.98856614016580480, 21.26098553207546971, -75.92929758216462233 ) ) ;
#31336 = CARTESIAN_POINT ( 'NONE',  ( 60.83600080046799974, -45.51118010285600235, -47.34051533470169915 ) ) ;
#31337 = CARTESIAN_POINT ( 'NONE',  ( 48.64767879017822594, -53.93625458155253938, -54.52761353198754080 ) ) ;
#31338 = DIRECTION ( 'NONE',  ( -0.8660254037844387076, 0.4999999999999998890, 1.942890293094024439E-16 ) ) ;
#31340 = CARTESIAN_POINT ( 'NONE',  ( 14.63393739769630031, 0.9255523191757060175, -34.64999999999999858 ) ) ;
#31339 = CARTESIAN_POINT ( 'NONE',  ( 83.05638573198190500, 14.23020891227059970, -47.55746740334460299 ) ) ;
#31341 = CARTESIAN_POINT ( 'NONE',  ( 68.13393739769618662, -30.66618894467940137, -100.2061629005786898 ) ) ;
#31342 = DIRECTION ( 'NONE',  ( 0.000000000000000000, 0.000000000000000000, -1.000000000000000000 ) ) ;
#31343 = VERTEX_POINT ( 'NONE', #39028 ) ;
#31344 = CYLINDRICAL_SURFACE ( 'NONE', #31478, 2.000000000000001776 ) ;
#31345 = AXIS2_PLACEMENT_3D ( 'NONE', #6720, #33949, #42358 ) ;
#31346 = EDGE_LOOP ( 'NONE', ( #9392, #42077, #23787, #24250 ) ) ;
#31347 = ORIENTED_EDGE ( 'NONE', *, *, #45860, .T. ) ;
#31348 = CYLINDRICAL_SURFACE ( 'NONE', #36164, 6.766999999999998572 ) ;
#31349 = CARTESIAN_POINT ( 'NONE',  ( 29.13393739769619728, -4.468739684871080087, -35.14999999999999858 ) ) ;
#31350 = CARTESIAN_POINT ( 'NONE',  ( 24.04527493495583457, -15.61618894149694192, -73.79233149842438877 ) ) ;
#31351 = CARTESIAN_POINT ( 'NONE',  ( 9.056254019423489510, -63.50214810053400782, -46.63926694421989794 ) ) ;
#31352 = EDGE_LOOP ( 'NONE', ( #25506, #47454, #44407, #31673, #40509 ) ) ;
#31353 = VERTEX_POINT ( 'NONE', #47658 ) ;
#31354 = CARTESIAN_POINT ( 'NONE',  ( 9.366403394718119557, -15.61612932825470068, -61.45282021618999124 ) ) ;
#31355 = DIRECTION ( 'NONE',  ( 0.000000000000000000, -1.000000000000000000, 0.000000000000000000 ) ) ;
#31356 = CARTESIAN_POINT ( 'NONE',  ( 56.31131641729229642, -50.56001720853080172, -52.86807145390460505 ) ) ;
#31357 = AXIS2_PLACEMENT_3D ( 'NONE', #47151, #27719, #47408 ) ;
#31358 = CARTESIAN_POINT ( 'NONE',  ( 68.13393739769620083, 1.383811055320669947, -65.65000000000000568 ) ) ;
#31359 = CARTESIAN_POINT ( 'NONE',  ( 59.10309117834729875, -3.122143041457199786, -15.65534436044210054 ) ) ;
#31360 = CARTESIAN_POINT ( 'NONE',  ( 51.67588099511449684, -48.69063913976710012, -77.01364301606309937 ) ) ;
#31361 = CARTESIAN_POINT ( 'NONE',  ( 13.96299814188780175, -52.23919279717198094, -75.65449996341371275 ) ) ;
#31362 = ORIENTED_EDGE ( 'NONE', *, *, #46395, .T. ) ;
#31363 = CARTESIAN_POINT ( 'NONE',  ( -7.894031745507627207, -33.07353038881739593, 7.944363289481099599 ) ) ;
#31364 = FACE_OUTER_BOUND ( 'NONE', #32562, .T. ) ;
#31365 = DIRECTION ( 'NONE',  ( 1.000000000000000000, 0.000000000000000000, 0.000000000000000000 ) ) ;
#31366 = CARTESIAN_POINT ( 'NONE',  ( 16.13393739769620083, -15.61618894467929941, -35.14999999999999858 ) ) ;
#31367 = AXIS2_PLACEMENT_3D ( 'NONE', #49808, #10234, #18336 ) ;
#31368 = CARTESIAN_POINT ( 'NONE',  ( 12.88457861957980199, -8.472771336652998642, -57.37660785931070251 ) ) ;
#31369 = EDGE_CURVE ( 'NONE', #32627, #31681, #6304, .T. ) ;
#31370 = CARTESIAN_POINT ( 'NONE',  ( 13.33362440043809904, -50.59907500154410087, -21.35584257635559879 ) ) ;
#31371 = CARTESIAN_POINT ( 'NONE',  ( 57.14246561268299729, 19.38381105532069881, -74.67211522426370607 ) ) ;
#31372 = DIRECTION ( 'NONE',  ( 0.000000000000000000, -1.000000000000000000, 0.000000000000000000 ) ) ;
#31373 = ADVANCED_FACE ( 'NONE', ( #25328, #4650 ), #16984, .T. ) ;
#31374 = CARTESIAN_POINT ( 'NONE',  ( 56.58040397675829780, 14.03809001566030012, -16.97035855063799659 ) ) ;
#31375 = CARTESIAN_POINT ( 'NONE',  ( 60.96921016464919774, -45.39643253083639962, -46.92502502242910367 ) ) ;
#31376 = CARTESIAN_POINT ( 'NONE',  ( 56.74347696462359636, -50.41867359881469923, -52.86071028780529701 ) ) ;
#31377 = CARTESIAN_POINT ( 'NONE',  ( 10.43067722519890062, -11.46704655386430005, -56.04737992176909955 ) ) ;
#31378 = DIRECTION ( 'NONE',  ( 0.8660254037844381525, 0.5000000000000007772, 0.000000000000000000 ) ) ;
#31379 = ORIENTED_EDGE ( 'NONE', *, *, #7219, .F. ) ;
#31380 = CONICAL_SURFACE ( 'NONE', #25548, 1.980489356881870222, 0.4636476090008052053 ) ;
#31381 = CARTESIAN_POINT ( 'NONE',  ( 16.13393739769620083, -15.61618894467929941, -82.15000000000000568 ) ) ;
#31382 = CARTESIAN_POINT ( 'NONE',  ( 64.93084822843239579, 1.265664290790580182, -60.77244468760530083 ) ) ;
#31383 = CARTESIAN_POINT ( 'NONE',  ( 23.04647402534414979, -11.63208260442388564, -51.34099938571964827 ) ) ;
#31384 = CARTESIAN_POINT ( 'NONE',  ( 17.85630073056284672, 20.07361857726406384, -75.01676221294343350 ) ) ;
#31385 = CARTESIAN_POINT ( 'NONE',  ( 56.12351168987260763, 13.88381105532070059, -10.09719779148739960 ) ) ;
#31386 = CARTESIAN_POINT ( 'NONE',  ( 9.367202679915338948, -15.61634672871210050, -75.45282021618999124 ) ) ;
#31387 = EDGE_CURVE ( 'NONE', #17917, #14173, #463, .T. ) ;
#31388 = CARTESIAN_POINT ( 'NONE',  ( 11.01613591017130034, 33.93391017002509358, -18.04558894928910107 ) ) ;
#31389 = CARTESIAN_POINT ( 'NONE',  ( 61.75019796695539753, 14.88381105532069881, -46.37203261889099792 ) ) ;
#31391 = CARTESIAN_POINT ( 'NONE',  ( 47.13180046211940066, -38.11666126782029806, -54.64277967633139355 ) ) ;
#31390 = CARTESIAN_POINT ( 'NONE',  ( 53.57529076486616049, 19.31354156546077405, -77.11805887586452002 ) ) ;
#31392 = AXIS2_PLACEMENT_3D ( 'NONE', #47788, #2991, #27342 ) ;
#31393 = EDGE_CURVE ( 'NONE', #3425, #29321, #17941, .T. ) ;
#31394 = CARTESIAN_POINT ( 'NONE',  ( 14.74660166870041955, -52.24942673173599417, -75.96019247805895702 ) ) ;
#31395 = CARTESIAN_POINT ( 'NONE',  ( 49.21269661613270330, 22.37820248916990096, -54.26152208607290106 ) ) ;
#31396 = ORIENTED_EDGE ( 'NONE', *, *, #51417, .T. ) ;
#31397 = CARTESIAN_POINT ( 'NONE',  ( 52.68346768350169640, -49.76694581559849695, -48.72606083504529551 ) ) ;
#31398 = ORIENTED_EDGE ( 'NONE', *, *, #46935, .T. ) ;
#31399 = CARTESIAN_POINT ( 'NONE',  ( 41.69094003941798832, 7.483996613871343406, -82.16073232984879837 ) ) ;
#31400 = CARTESIAN_POINT ( 'NONE',  ( 22.72481314779377470, -17.38742374030793769, -74.53615356034734418 ) ) ;
#31401 = CYLINDRICAL_SURFACE ( 'NONE', #4461, 5.499999999999998224 ) ;
#31402 = DIRECTION ( 'NONE',  ( 0.000000000000000000, 1.000000000000000000, 0.000000000000000000 ) ) ;
#31403 = CARTESIAN_POINT ( 'NONE',  ( 9.086494889888442117, -15.89207442050179964, -55.44036573270419410 ) ) ;
#31404 = CARTESIAN_POINT ( 'NONE',  ( 68.13393739769618662, -25.01418894467940035, -65.65000000000000568 ) ) ;
#31405 = CARTESIAN_POINT ( 'NONE',  ( 55.13249787720189943, -46.09229425796829815, -16.25834332036090046 ) ) ;
#31406 = DIRECTION ( 'NONE',  ( 0.6668512999106339656, 0.3436531272335545117, -0.6612199875609449107 ) ) ;
#31407 = VERTEX_POINT ( 'NONE', #13062 ) ;
#31408 = CARTESIAN_POINT ( 'NONE',  ( 19.32439272560200294, -22.78610825969399656, -43.65423889476469554 ) ) ;
#31409 = ORIENTED_EDGE ( 'NONE', *, *, #44902, .F. ) ;
#31410 = CARTESIAN_POINT ( 'NONE',  ( 11.78860069758130003, -65.42274227350759475, -17.85348597566460072 ) ) ;
#31411 = CARTESIAN_POINT ( 'NONE',  ( 11.71414166034919901, 34.09778695716270391, -47.42034454235100327 ) ) ;
#31412 = CARTESIAN_POINT ( 'NONE',  ( 72.92278648876258274, 1.264689361399219836, -62.28332989495380190 ) ) ;
#31413 = DIRECTION ( 'NONE',  ( 0.000000000000000000, 1.000000000000000000, 0.000000000000000000 ) ) ;
#31414 = DIRECTION ( 'NONE',  ( 0.000000000000000000, -6.470469973722704271E-12, -1.000000000000000000 ) ) ;
#31415 = DIRECTION ( 'NONE',  ( -0.8660254037844379305, 0.5000000000000011102, 0.000000000000000000 ) ) ;
#31416 = ORIENTED_EDGE ( 'NONE', *, *, #20618, .T. ) ;
#31417 = CARTESIAN_POINT ( 'NONE',  ( 57.24929578595760660, 19.38381105532069881, -74.14999999999999147 ) ) ;
#31418 = AXIS2_PLACEMENT_3D ( 'NONE', #29020, #25066, #720 ) ;
#31419 = CARTESIAN_POINT ( 'NONE',  ( 11.10530294771309912, -63.11543068638779630, -44.25053028539870326 ) ) ;
#31420 = CARTESIAN_POINT ( 'NONE',  ( 70.83393739769690001, 16.88381105531960458, -68.79999999999942872 ) ) ;
#31421 = EDGE_LOOP ( 'NONE', ( #12091, #13398 ) ) ;
#31422 = CARTESIAN_POINT ( 'NONE',  ( 22.14842110270483744, -20.87114761213502589, -44.02058836580484780 ) ) ;
#31423 = CARTESIAN_POINT ( 'NONE',  ( 56.62412426277949606, 19.48324289140059662, -53.71767670195740152 ) ) ;
#31424 = CARTESIAN_POINT ( 'NONE',  ( 20.13393739769620083, -28.89524513604070322, -62.14999999999999858 ) ) ;
#31425 = ORIENTED_EDGE ( 'NONE', *, *, #23825, .T. ) ;
#31426 = CARTESIAN_POINT ( 'NONE',  ( 18.20462292297444762, -23.32128735048156543, -35.92433339525297953 ) ) ;
#31427 = CARTESIAN_POINT ( 'NONE',  ( 0.5406133260286609676, 12.32747302715160131, -21.14999999999999858 ) ) ;
#31428 = CARTESIAN_POINT ( 'NONE',  ( 13.10862549112176012, -21.71576177937856400, -33.09924202300560125 ) ) ;
#31429 = CARTESIAN_POINT ( 'NONE',  ( 57.26283657379369885, -50.61618895537380070, -53.75815476539319349 ) ) ;
#31430 = CARTESIAN_POINT ( 'NONE',  ( 11.87640767932309949, -8.555299428973780707, -77.11961558469180034 ) ) ;
#31431 = EDGE_CURVE ( 'NONE', #50288, #14340, #46442, .T. ) ;
#31432 = CARTESIAN_POINT ( 'NONE',  ( -11.36606260230380094, -15.61618894467929941, -54.64999999999999858 ) ) ;
#31433 = DIRECTION ( 'NONE',  ( 0.000000000000000000, 0.000000000000000000, -1.000000000000000000 ) ) ;
#31434 = DIRECTION ( 'NONE',  ( 0.000000000000000000, 0.000000000000000000, 1.000000000000000000 ) ) ;
#31435 = ORIENTED_EDGE ( 'NONE', *, *, #36828, .F. ) ;
#31436 = VERTEX_POINT ( 'NONE', #36612 ) ;
#31437 = CARTESIAN_POINT ( 'NONE',  ( -22.75376598977980080, -12.76162732185420268, -54.69834592236689019 ) ) ;
#31438 = CARTESIAN_POINT ( 'NONE',  ( 23.33558369893389894, -13.70752858803779972, -50.15019124198150280 ) ) ;
#31439 = CARTESIAN_POINT ( 'NONE',  ( 16.13393739769620083, -15.61618894467929941, -16.68902128623620129 ) ) ;
#31440 = DIRECTION ( 'NONE',  ( -0.4412403921323043154, 0.5329539830277481016, -0.7219882051154223879 ) ) ;
#31441 = AXIS2_PLACEMENT_3D ( 'NONE', #32610, #20309, #44957 ) ;
#31442 = CARTESIAN_POINT ( 'NONE',  ( 46.73672019546049938, 22.47805634369839822, -75.96172454647880556 ) ) ;
#31443 = CARTESIAN_POINT ( 'NONE',  ( 9.366937397696199596, -15.61618894467949836, -28.45282021618999835 ) ) ;
#31444 = CARTESIAN_POINT ( 'NONE',  ( 9.895693118437268510, 22.37718731335050038, -34.65000333313919612 ) ) ;
#31445 =( BOUNDED_SURFACE ( )  B_SPLINE_SURFACE ( 2, 2, ( 
 ( #11488, #27703, #39771 ),
 ( #7290, #39257, #36085 ),
 ( #192, #43701, #3360 ) ),
 .UNSPECIFIED., .F., .F., .T. ) 
 B_SPLINE_SURFACE_WITH_KNOTS ( ( 3, 3 ),
 ( 3, 3 ),
 ( 3.075382746042809996E-13, 1.570796326795540043 ),
 ( -1.570796326795069975, 2.603505476660149968E-13 ),
 .UNSPECIFIED. ) 
 GEOMETRIC_REPRESENTATION_ITEM ( )  RATIONAL_B_SPLINE_SURFACE ( (
 ( 1.000000000000000000, 0.7071067811863940289, 1.000000000000000000),
 ( 0.7071067811864010233, 0.4999999999997879474, 0.7071067811864010233),
 ( 1.000000000000000000, 0.7071067811863940289, 1.000000000000000000) ) ) 
 REPRESENTATION_ITEM ( '' )  SURFACE ( )  );
#31446 = CARTESIAN_POINT ( 'NONE',  ( 41.80336364839079266, -44.88664980482889888, -5.672379628686790021 ) ) ;
#31447 = CARTESIAN_POINT ( 'NONE',  ( 12.04070883443819895, 33.58235188910439462, -16.10368401051540133 ) ) ;
#31448 = VECTOR ( 'NONE', #24032, 1000.000000000000000 ) ;
#31449 = CARTESIAN_POINT ( 'NONE',  ( 12.89829992594130026, -23.19994598590569979, -74.13603346371840530 ) ) ;
#31450 = ADVANCED_FACE ( 'NONE', ( #32932 ), #24542, .T. ) ;
#31451 = CARTESIAN_POINT ( 'NONE',  ( 54.34775236769140605, -47.86158002624129892, -25.94360105443890063 ) ) ;
#31452 = AXIS2_PLACEMENT_3D ( 'NONE', #9897, #18015, #25853 ) ;
#31453 = CARTESIAN_POINT ( 'NONE',  ( 56.90586760780780651, -50.64480473018880247, -74.36144200333770016 ) ) ;
#31455 = CARTESIAN_POINT ( 'NONE',  ( 12.72585954689345655, -9.703326353824166972, -59.78612966474727841 ) ) ;
#31454 = CARTESIAN_POINT ( 'NONE',  ( 0.06538248623146999949, 21.54194279676389812, -7.555612708363120156 ) ) ;
#31457 = ADVANCED_FACE ( 'NONE', ( #48959 ), #2050, .T. ) ;
#31456 = CARTESIAN_POINT ( 'NONE',  ( 63.02016742692980245, 0.9209567800143640959, -68.78847615610249022 ) ) ;
#31458 = FACE_OUTER_BOUND ( 'NONE', #11980, .T. ) ;
#31459 = ORIENTED_EDGE ( 'NONE', *, *, #27834, .T. ) ;
#31460 = CARTESIAN_POINT ( 'NONE',  ( 53.18570859912749427, -49.47442707985450028, -48.81732526230189961 ) ) ;
#31461 = CARTESIAN_POINT ( 'NONE',  ( 47.55693705089040435, 23.33414435787860342, -54.87298417455060218 ) ) ;
#31462 = CARTESIAN_POINT ( 'NONE',  ( 61.26565493546950592, -45.23349057862129996, -27.96003281282710162 ) ) ;
#31463 = CARTESIAN_POINT ( 'NONE',  ( 8.673554481405242100, -18.33517393658237182, -66.68099849312459071 ) ) ;
#31464 = CARTESIAN_POINT ( 'NONE',  ( 61.58449942664206844, -45.28981909799563255, -47.18862349895694308 ) ) ;
#31465 = CARTESIAN_POINT ( 'NONE',  ( 23.58421856477589884, -15.61827139591260050, -74.23274628532179520 ) ) ;
#31466 = CARTESIAN_POINT ( 'NONE',  ( 51.08267997340979605, 17.48509555023420248, -76.44192736852110670 ) ) ;
#31467 = CARTESIAN_POINT ( 'NONE',  ( 52.81743982411089888, 18.43499551991449792, -48.47378032971769812 ) ) ;
#31468 = CARTESIAN_POINT ( 'NONE',  ( 24.04493739326861146, -16.65173287428400428, -69.83400117973924637 ) ) ;
#31469 = CARTESIAN_POINT ( 'NONE',  ( 53.11114670112049652, -49.51349214730240078, -48.80212167156650338 ) ) ;
#31470 = CARTESIAN_POINT ( 'NONE',  ( 50.27626388677308000, 5.227946323752799884, -76.15207597994086086 ) ) ;
#31471 = CARTESIAN_POINT ( 'NONE',  ( 24.04795836731096159, -15.76465008236952947, -61.51362244070021035 ) ) ;
#31472 = CARTESIAN_POINT ( 'NONE',  ( 53.88536905793235121, -48.73596811206648738, -27.04541679508261254 ) ) ;
#31473 = DIRECTION ( 'NONE',  ( 0.000000000000000000, 0.000000000000000000, -1.000000000000000000 ) ) ;
#31474 = CARTESIAN_POINT ( 'NONE',  ( 59.50660854669460065, -29.52284063487349997, -15.84052005884069914 ) ) ;
#31475 = CARTESIAN_POINT ( 'NONE',  ( 71.06936022730370439, 1.374300485541529948, -60.86138005882520474 ) ) ;
#31476 = DIRECTION ( 'NONE',  ( -0.4316160343590924597, 0.9020574254913767964, 0.000000000000000000 ) ) ;
#31477 = CARTESIAN_POINT ( 'NONE',  ( 72.67981544229699864, 0.9952277120690129486, -61.73279890693489591 ) ) ;
#31478 = AXIS2_PLACEMENT_3D ( 'NONE', #11469, #23987, #27423 ) ;
#31479 = CARTESIAN_POINT ( 'NONE',  ( 51.29176893202588872, -34.69240276036310888, -76.59668289401075469 ) ) ;
#31480 = CARTESIAN_POINT ( 'NONE',  ( 43.91474985151640453, 12.31375205243809923, -5.093415854581109237 ) ) ;
#31481 = ORIENTED_EDGE ( 'NONE', *, *, #42309, .T. ) ;
#31482 = ORIENTED_EDGE ( 'NONE', *, *, #50483, .F. ) ;
#31483 = CARTESIAN_POINT ( 'NONE',  ( 40.64814283787870153, 13.41987867678509971, -4.018323132419280519 ) ) ;
#31484 = CARTESIAN_POINT ( 'NONE',  ( 17.01980479381098377, -22.38317906675219504, -58.91115339620073144 ) ) ;
#31485 = ORIENTED_EDGE ( 'NONE', *, *, #41272, .T. ) ;
#31486 = CARTESIAN_POINT ( 'NONE',  ( 55.85894235177089939, -45.98179482937800344, -25.33296393815039949 ) ) ;
#31487 = PRODUCT_DEFINITION ( 'UNKNOWN', '', #49473, #39983 ) ;
#31488 = FACE_BOUND ( 'NONE', #26149, .T. ) ;
#31489 = EDGE_LOOP ( 'NONE', ( #42617, #16297, #43988, #23810 ) ) ;
#31490 = CARTESIAN_POINT ( 'NONE',  ( 20.09351995423807580, -21.16054109508102954, -80.75524004131028732 ) ) ;
#31491 = CARTESIAN_POINT ( 'NONE',  ( 44.75655348390716881, 6.781133406353570869, -66.53686104485265673 ) ) ;
#31492 = AXIS2_PLACEMENT_3D ( 'NONE', #2354, #18595, #38789 ) ;
#31493 = DIRECTION ( 'NONE',  ( 0.000000000000000000, 0.000000000000000000, 1.000000000000000000 ) ) ;
#31494 = CARTESIAN_POINT ( 'NONE',  ( 22.28114148176659981, -21.11115046850839860, -34.02451708608289493 ) ) ;
#31495 = AXIS2_PLACEMENT_3D ( 'NONE', #51141, #34880, #34615 ) ;
#31496 = EDGE_CURVE ( 'NONE', #8898, #19834, #16707, .T. ) ;
#31497 = DIRECTION ( 'NONE',  ( -1.000000000000000000, 0.000000000000000000, 0.000000000000000000 ) ) ;
#31498 = DIRECTION ( 'NONE',  ( 0.000000000000000000, -1.000000000000000000, 0.000000000000000000 ) ) ;
#31499 = B_SPLINE_CURVE_WITH_KNOTS ( 'NONE', 3,
 ( #31386, #7830, #16196, #48170, #212, #19611, #32153, #31901, #12272, #43978, #43469, #35855, #40050, #36110, #4141, #11769, #20117, #23520 ),
 .UNSPECIFIED., .F., .F.,
 ( 4, 2, 2, 2, 2, 2, 2, 2, 4 ),
 ( 0.000000000000000000, 0.06250000040710312899, 0.1250000008142062580, 0.1875000012213093870, 0.2500000016284125159, 0.3125000020355155339, 0.3750000024426185519, 0.4375000028497215698, 0.5000000032568245878 ),
 .UNSPECIFIED. ) ;
#31500 = CARTESIAN_POINT ( 'NONE',  ( 10.63047440947285160, -19.59698183909219082, -51.25339573762192202 ) ) ;
#31501 = EDGE_CURVE ( 'NONE', #17172, #45555, #44750, .T. ) ;
#31502 = CARTESIAN_POINT ( 'NONE',  ( 59.32541119420320541, -28.11267854137589595, -15.67734865989629789 ) ) ;
#31503 = EDGE_CURVE ( 'NONE', #9786, #36317, #21866, .T. ) ;
#31504 = CARTESIAN_POINT ( 'NONE',  ( 21.54529180190751703, -11.45756348979150907, -64.24448863903798213 ) ) ;
#31505 = CARTESIAN_POINT ( 'NONE',  ( 46.65019242837639979, -53.38344801646140070, -76.07596939981860373 ) ) ;
#31506 = CARTESIAN_POINT ( 'NONE',  ( 19.56389830141130304, -22.67466723610790424, -70.36851255374439518 ) ) ;
#31507 = CARTESIAN_POINT ( 'NONE',  ( 22.04685232790915350, -19.02417400735164321, -36.61948459849637771 ) ) ;
#31508 = CARTESIAN_POINT ( 'NONE',  ( 41.75078909917250058, 14.43727496473849925, -6.577246330791240325 ) ) ;
#31509 = ADVANCED_FACE ( 'NONE', ( #32150 ), #13310, .F. ) ;
#31510 = CARTESIAN_POINT ( 'NONE',  ( 15.05440318628110141, 21.88381105532300097, -76.14999999999999147 ) ) ;
#31511 = CARTESIAN_POINT ( 'NONE',  ( 83.25229294592290330, -45.14839585538909716, -47.26064541804080221 ) ) ;
#31512 = CIRCLE ( 'NONE', #29830, 1.999999999999998668 ) ;
#31513 = EDGE_CURVE ( 'NONE', #34513, #1610, #19376, .T. ) ;
#31514 = CARTESIAN_POINT ( 'NONE',  ( 65.41765814209475138, -30.18662511381366187, -16.56748189521639247 ) ) ;
#31515 = CARTESIAN_POINT ( 'NONE',  ( 21.62555272082460078, -21.76638258811500037, -45.77565614294260143 ) ) ;
#31516 = ORIENTED_EDGE ( 'NONE', *, *, #5353, .F. ) ;
#31517 = CARTESIAN_POINT ( 'NONE',  ( 53.00356549828499908, -49.51115989585530741, -27.69254757381720111 ) ) ;
#31518 = CARTESIAN_POINT ( 'NONE',  ( 16.22100018021849976, -51.07051512547269567, -20.14984494908150126 ) ) ;
#31519 = CARTESIAN_POINT ( 'NONE',  ( 75.07324054225550469, -8.405693818634281556, -11.43558758117930019 ) ) ;
#31521 = EDGE_CURVE ( 'NONE', #47619, #12694, #19629, .T. ) ;
#31520 = LINE ( 'NONE', #32531, #14583 ) ;
#31522 = CARTESIAN_POINT ( 'NONE',  ( 68.13393739769618662, -31.81618894467930403, -65.65000000000000568 ) ) ;
#31523 = ORIENTED_EDGE ( 'NONE', *, *, #40329, .T. ) ;
#31524 = FACE_OUTER_BOUND ( 'NONE', #45184, .T. ) ;
#31525 = DIRECTION ( 'NONE',  ( 0.000000000000000000, 0.000000000000000000, 1.000000000000000000 ) ) ;
#31526 = DIRECTION ( 'NONE',  ( -0.2260571801428161165, -2.775557561562891043E-17, 0.9741140340359943917 ) ) ;
#31527 = CARTESIAN_POINT ( 'NONE',  ( 82.31238480745950881, -45.35763125051939681, -47.32928030304829292 ) ) ;
#31528 = CARTESIAN_POINT ( 'NONE',  ( 57.35780229286250176, -50.16949399769480067, -52.65865520802150002 ) ) ;
#31529 = CARTESIAN_POINT ( 'NONE',  ( 41.49029383318099917, 13.34306788730399873, -5.136314537161009497 ) ) ;
#31530 = CARTESIAN_POINT ( 'NONE',  ( 47.63732207932127238, -54.52964753594648784, -74.36335264234261899 ) ) ;
#31531 = CARTESIAN_POINT ( 'NONE',  ( 64.59570122278479687, 0.9170823515331258946, -60.80394275157760831 ) ) ;
#31532 = CARTESIAN_POINT ( 'NONE',  ( 54.20043578388980166, -48.94278307704079367, -48.51842787370119936 ) ) ;
#31533 = CARTESIAN_POINT ( 'NONE',  ( -0.1135338934745361295, -20.70530579567934026, -34.86513988225942740 ) ) ;
#31534 = CARTESIAN_POINT ( 'NONE',  ( 68.16055449185739690, -0.9007378807446890789, -18.00106518090050045 ) ) ;
#31535 = CARTESIAN_POINT ( 'NONE',  ( 18.12345004666019932, -52.06054985064280061, -75.71157996061791096 ) ) ;
#31536 = CARTESIAN_POINT ( 'NONE',  ( 51.54415332628170177, -52.59067900109340599, -53.64346124582210251 ) ) ;
#31537 = CARTESIAN_POINT ( 'NONE',  ( 9.618178158523400967, -12.00349246206750031, -60.22848937760100085 ) ) ;
#31538 = DIRECTION ( 'NONE',  ( -1.000000000000000000, 0.000000000000000000, 0.000000000000000000 ) ) ;
#31539 = CARTESIAN_POINT ( 'NONE',  ( 56.51051770571049815, -45.90816165454779707, -45.01386504879189943 ) ) ;
#31540 = ORIENTED_EDGE ( 'NONE', *, *, #48306, .T. ) ;
#31541 = CARTESIAN_POINT ( 'NONE',  ( 22.16915665782680023, -54.07211264381400184, -34.88336916441289759 ) ) ;
#31542 = CARTESIAN_POINT ( 'NONE',  ( 22.90093207708843792, -15.62495752410452887, -34.45323087790774963 ) ) ;
#31543 = CARTESIAN_POINT ( 'NONE',  ( 73.12314370215899828, 1.096110717717199812, -68.90857121967530929 ) ) ;
#31544 = DIRECTION ( 'NONE',  ( 0.000000000000000000, 1.000000000000000000, 0.000000000000000000 ) ) ;
#31545 = ADVANCED_FACE ( 'NONE', ( #28494, #8596 ), #25838, .T. ) ;
#31546 = CARTESIAN_POINT ( 'NONE',  ( 12.09138161462960070, -9.064420227699880428, -81.23899999999999011 ) ) ;
#31547 = VERTEX_POINT ( 'NONE', #34220 ) ;
#31548 = CARTESIAN_POINT ( 'NONE',  ( 17.69970719370899914, 21.04130707244170040, -75.96082109999758814 ) ) ;
#31549 = VERTEX_POINT ( 'NONE', #9881 ) ;
#31550 = VERTEX_POINT ( 'NONE', #22171 ) ;
#31551 = CARTESIAN_POINT ( 'NONE',  ( 23.57620331537150093, -14.43797626381360111, -81.23899999999999011 ) ) ;
#31552 = CARTESIAN_POINT ( 'NONE',  ( 68.13393739769618662, -30.66618894467940137, -65.65000000000000568 ) ) ;
#31553 = CARTESIAN_POINT ( 'NONE',  ( 61.58777976395109732, 14.02680365743669988, -47.11785714435669803 ) ) ;
#31554 = VERTEX_POINT ( 'NONE', #1505 ) ;
#31555 = CARTESIAN_POINT ( 'NONE',  ( 63.88393739769619373, 4.883811055320659733, -61.34712802272770915 ) ) ;
#31556 = ORIENTED_EDGE ( 'NONE', *, *, #19502, .F. ) ;
#31557 = DIRECTION ( 'NONE',  ( -0.2720339695306771000, 0.4031695913578095536, 0.8737572889686010535 ) ) ;
#31558 = EDGE_CURVE ( 'NONE', #50249, #16294, #6710, .T. ) ;
#31559 = DIRECTION ( 'NONE',  ( 0.000000000000000000, 0.000000000000000000, 1.000000000000000000 ) ) ;
#31560 = ORIENTED_EDGE ( 'NONE', *, *, #44461, .T. ) ;
#31561 = EDGE_CURVE ( 'NONE', #434, #46863, #5026, .T. ) ;
#31562 = CARTESIAN_POINT ( 'NONE',  ( 59.34499803081109803, -28.11618894467929763, -15.68015151901639825 ) ) ;
#31563 = CARTESIAN_POINT ( 'NONE',  ( 52.20740540343859237, -51.40483972235690402, -75.93239679552310406 ) ) ;
#31564 = CARTESIAN_POINT ( 'NONE',  ( 61.19258921585740296, 14.32575781460780107, -47.61960278887369924 ) ) ;
#31565 = AXIS2_PLACEMENT_3D ( 'NONE', #5410, #25809, #13538 ) ;
#31566 = ADVANCED_FACE ( 'NONE', ( #46057 ), #21652, .T. ) ;
#31567 = CARTESIAN_POINT ( 'NONE',  ( 17.56839097463578980, -8.943911882717593187, -40.02052517762369632 ) ) ;
#31568 = CARTESIAN_POINT ( 'NONE',  ( 42.93197233849409855, -42.55807683903029925, -3.187564294433600232 ) ) ;
#31569 = CARTESIAN_POINT ( 'NONE',  ( -3.954343448002319850, 17.15822905836070333, -5.572179413950920868 ) ) ;
#31570 = FACE_OUTER_BOUND ( 'NONE', #35305, .T. ) ;
#31571 = CARTESIAN_POINT ( 'NONE',  ( 26.13393739769619728, -15.61618894467929941, 17.35000000000000142 ) ) ;
#31572 = CARTESIAN_POINT ( 'NONE',  ( 16.42129855753530165, -23.45864849172179945, -63.77584738492399197 ) ) ;
#31573 = ORIENTED_EDGE ( 'NONE', *, *, #29431, .F. ) ;
#31574 = CARTESIAN_POINT ( 'NONE',  ( 23.53669455186071602, -48.92556967366427756, -34.79644561402096770 ) ) ;
#31576 = EDGE_CURVE ( 'NONE', #2407, #42744, #20075, .T. ) ;
#31575 = CARTESIAN_POINT ( 'NONE',  ( 71.81740743633011448, 1.051325075267619980, -70.37790726184800860 ) ) ;
#31577 = CARTESIAN_POINT ( 'NONE',  ( 42.50259719104650458, -39.81721345468353235, -73.90402679261637786 ) ) ;
#31578 = CARTESIAN_POINT ( 'NONE',  ( 15.54393737248530094, 19.58453728325200061, -20.39348321914659934 ) ) ;
#31579 = CYLINDRICAL_SURFACE ( 'NONE', #46515, 1.999999999999970246 ) ;
#31580 = CARTESIAN_POINT ( 'NONE',  ( 63.23627918741579634, 0.9395704634982890990, -69.11607016250880520 ) ) ;
#31581 = CARTESIAN_POINT ( 'NONE',  ( 48.66936276473360579, -53.96730371771859325, -54.61968686218679636 ) ) ;
#31582 = LINE ( 'NONE', #27152, #49079 ) ;
#31583 = CARTESIAN_POINT ( 'NONE',  ( 6.633937397696199945, -15.61618894467929941, -18.35000000000000142 ) ) ;
#31584 = CARTESIAN_POINT ( 'NONE',  ( 73.06894106338339157, -30.31618894467939995, -62.06450996101596473 ) ) ;
#31585 = CARTESIAN_POINT ( 'NONE',  ( 47.67338561975220301, 23.28889910737600033, -55.14318275608980002 ) ) ;
#31586 = EDGE_LOOP ( 'NONE', ( #40220, #29998, #12151, #17589 ) ) ;
#31587 = CARTESIAN_POINT ( 'NONE',  ( 22.16258581960079965, -19.27651095769689604, -79.02086993021860906 ) ) ;
#31588 = CARTESIAN_POINT ( 'NONE',  ( 64.86401092314891059, 1.392490173688039956, -61.04984893884839892 ) ) ;
#31589 = ORIENTED_EDGE ( 'NONE', *, *, #31656, .T. ) ;
#31590 = CARTESIAN_POINT ( 'NONE',  ( 71.54045699608269615, 0.8986939045430379913, -70.58925035374331003 ) ) ;
#31591 = CARTESIAN_POINT ( 'NONE',  ( 60.28833275760250388, -45.75485330741069845, -47.30217035591910246 ) ) ;
#31592 = CARTESIAN_POINT ( 'NONE',  ( 48.29537619369078527, -54.13523159705017207, -54.65524445810790866 ) ) ;
#31593 = AXIS2_PLACEMENT_3D ( 'NONE', #39075, #30149, #34600 ) ;
#31594 = CARTESIAN_POINT ( 'NONE',  ( 82.62219371776291155, 13.83471874997871964, -46.37145547400888290 ) ) ;
#31596 = CARTESIAN_POINT ( 'NONE',  ( 14.39116781407899914, 1.145880372108919909, -34.70985242058469566 ) ) ;
#31595 = DIRECTION ( 'NONE',  ( -1.180619220495489865E-10, 8.141548257237140630E-09, 1.000000000000000000 ) ) ;
#31597 = EDGE_CURVE ( 'NONE', #9855, #13869, #28738, .T. ) ;
#31598 = CARTESIAN_POINT ( 'NONE',  ( 30.37740194055309928, 4.394033142310519224, -84.60975078156931772 ) ) ;
#31599 = DIRECTION ( 'NONE',  ( 0.000000000000000000, 0.000000000000000000, -1.000000000000000000 ) ) ;
#31600 = ORIENTED_EDGE ( 'NONE', *, *, #36042, .T. ) ;
#31601 = DIRECTION ( 'NONE',  ( 1.000000000000000000, 0.000000000000000000, 0.000000000000000000 ) ) ;
#31602 = EDGE_CURVE ( 'NONE', #20523, #49499, #10407, .T. ) ;
#31603 = ORIENTED_EDGE ( 'NONE', *, *, #5517, .F. ) ;
#31604 = AXIS2_PLACEMENT_3D ( 'NONE', #25737, #38078, #49877 ) ;
#31605 = EDGE_LOOP ( 'NONE', ( #16819, #9222, #32247, #24309, #32943 ) ) ;
#31606 = CARTESIAN_POINT ( 'NONE',  ( 16.13393739769620083, -15.61618894467929941, -2.149999999999999911 ) ) ;
#31607 = CARTESIAN_POINT ( 'NONE',  ( 8.222412332301150428, -15.61630761206940043, -38.79233150823699816 ) ) ;
#31608 = CARTESIAN_POINT ( 'NONE',  ( 22.90070908176307896, -14.58601874559523992, -62.79870702742260136 ) ) ;
#31609 = CARTESIAN_POINT ( 'NONE',  ( 8.835310923510441228, -63.39783216344699213, -46.67672964034989747 ) ) ;
#31610 = ORIENTED_EDGE ( 'NONE', *, *, #40619, .F. ) ;
#31611 = CARTESIAN_POINT ( 'NONE',  ( 28.63393739769619728, -4.678675331415849570, -34.64999999999999858 ) ) ;
#31612 = CARTESIAN_POINT ( 'NONE',  ( -18.86687343253337090, 1.668172178233732206, -51.44400016804027587 ) ) ;
#31613 = CARTESIAN_POINT ( 'NONE',  ( 56.51188083447159727, -50.74428706468020067, -53.61551639950389614 ) ) ;
#31614 = CARTESIAN_POINT ( 'NONE',  ( 10.40721350023446057, -11.95274919063715835, -45.63409041280543477 ) ) ;
#31615 = CARTESIAN_POINT ( 'NONE',  ( 58.98154412302919525, -3.123513370137979805, -15.65041568119880289 ) ) ;
#31616 = CARTESIAN_POINT ( 'NONE',  ( 51.99246080072099829, -50.02585771624480060, -76.70334503327950415 ) ) ;
#31617 = CARTESIAN_POINT ( 'NONE',  ( 13.88455093916192951, -52.17615671833033275, -75.56421372420085447 ) ) ;
#31618 = EDGE_CURVE ( 'NONE', #34264, #309, #18402, .T. ) ;
#31619 = EDGE_LOOP ( 'NONE', ( #3087, #36843 ) ) ;
#31620 = DIRECTION ( 'NONE',  ( 1.000000000000000000, 0.000000000000000000, 0.000000000000000000 ) ) ;
#31621 = CARTESIAN_POINT ( 'NONE',  ( 16.13393739769599833, 14.38381105532070059, -35.14999999999999858 ) ) ;
#31622 = CARTESIAN_POINT ( 'NONE',  ( 16.13393739769629676, -15.61618894467929941, -20.75000000000000000 ) ) ;
#31623 = CARTESIAN_POINT ( 'NONE',  ( -3.366062602303800055, -15.61618894467929763, -14.68999999999999950 ) ) ;
#31624 = EDGE_CURVE ( 'NONE', #42867, #39634, #49475, .T. ) ;
#31625 = CARTESIAN_POINT ( 'NONE',  ( 12.12491682425339867, -22.36263257323610176, -54.68316420314769033 ) ) ;
#31626 = CARTESIAN_POINT ( 'NONE',  ( 13.58580407945710000, -50.38962722024810148, -21.11665590476469845 ) ) ;
#31627 = CARTESIAN_POINT ( 'NONE',  ( 55.77509494401380152, 19.38954758360430120, -76.00676941660189812 ) ) ;
#31628 = CARTESIAN_POINT ( 'NONE',  ( 62.09157612670949788, 4.883811055320659733, -65.34607522167520699 ) ) ;
#31629 = CARTESIAN_POINT ( 'NONE',  ( 10.61752692138360032, -64.82564047392860118, -18.17418372802830007 ) ) ;
#31630 = CARTESIAN_POINT ( 'NONE',  ( 60.92599963243960559, -45.60351086516099883, -47.62103043570899530 ) ) ;
#31631 = DIRECTION ( 'NONE',  ( 0.000000000000000000, 0.000000000000000000, 1.000000000000000000 ) ) ;
#31632 = CIRCLE ( 'NONE', #9067, 21.50000000000000000 ) ;
#31633 = CARTESIAN_POINT ( 'NONE',  ( 23.18476211127489961, -15.44757686670599917, -56.83956923240509695 ) ) ;
#31634 = CARTESIAN_POINT ( 'NONE',  ( 49.72648160330989953, 22.41435850158119791, -55.11972614036179863 ) ) ;
#31635 = VERTEX_POINT ( 'NONE', #25584 ) ;
#31636 = CARTESIAN_POINT ( 'NONE',  ( 47.41053033963120100, 23.00881195654629607, -75.29848680172570141 ) ) ;
#31637 = CARTESIAN_POINT ( 'NONE',  ( 64.82950905750189463, 0.9955677559369568996, -60.65081522799539471 ) ) ;
#31638 = CARTESIAN_POINT ( 'NONE',  ( 41.74231633223259763, -45.72926218777020324, -6.615723881723910793 ) ) ;
#31639 = CARTESIAN_POINT ( 'NONE',  ( 16.13393739769620083, -15.61618894467929941, -32.14999999999999858 ) ) ;
#31640 = CARTESIAN_POINT ( 'NONE',  ( 14.27688375769564999, -50.38989777066024800, -20.83437850749841047 ) ) ;
#31641 = CARTESIAN_POINT ( 'NONE',  ( 17.16954621662006630, -7.705197706395741086, -47.04933590956818534 ) ) ;
#31642 = CARTESIAN_POINT ( 'NONE',  ( 10.63085818559157048, -64.83909131530428738, -18.12438161376036660 ) ) ;
#31643 = CARTESIAN_POINT ( 'NONE',  ( 11.89948726635009812, 34.20418277686660247, -18.06739951299479685 ) ) ;
#31644 = DIRECTION ( 'NONE',  ( 0.6933752452815366007, -0.7071067811865471286, -0.1386750490563077864 ) ) ;
#31646 = CARTESIAN_POINT ( 'NONE',  ( 9.807859542861747215, -20.47797908015472501, -58.58399811593378814 ) ) ;
#31645 = CARTESIAN_POINT ( 'NONE',  ( 40.57649240635721810, 4.883811055320659733, -83.97002642401369599 ) ) ;
#31647 = FACE_OUTER_BOUND ( 'NONE', #42342, .T. ) ;
#31648 = CARTESIAN_POINT ( 'NONE',  ( 49.00556831830410687, 22.49847617784580223, -54.36652964084350259 ) ) ;
#31649 = VERTEX_POINT ( 'NONE', #22429 ) ;
#31650 = CARTESIAN_POINT ( 'NONE',  ( 53.24077194809640190, -49.47968887696829654, -49.04425631192140145 ) ) ;
#31651 = ORIENTED_EDGE ( 'NONE', *, *, #2309, .T. ) ;
#31652 = CARTESIAN_POINT ( 'NONE',  ( 43.90669715076391810, 6.478564597039538242, -70.75373661325032515 ) ) ;
#31653 = CARTESIAN_POINT ( 'NONE',  ( 14.28038400710292777, -23.61618894467940066, -34.79644660940672907 ) ) ;
#31654 = DIRECTION ( 'NONE',  ( -1.000000000000000000, 0.000000000000000000, 0.000000000000000000 ) ) ;
#31655 = CARTESIAN_POINT ( 'NONE',  ( 84.22671941158239406, 12.55804992541220066, -46.99905560746370270 ) ) ;
#31656 = EDGE_CURVE ( 'NONE', #45923, #51745, #40143, .T. ) ;
#31657 = CARTESIAN_POINT ( 'NONE',  ( 10.85209793954360080, -20.29002362670730264, -53.22223566292269226 ) ) ;
#31658 = CARTESIAN_POINT ( 'NONE',  ( 52.64726118030579727, 18.56190800186159962, -48.69235233590459444 ) ) ;
#31659 = CARTESIAN_POINT ( 'NONE',  ( 56.48065915063589415, -45.38274434046520156, -17.55965706255600267 ) ) ;
#31660 = EDGE_CURVE ( 'NONE', #41906, #43383, #13566, .T. ) ;
#31661 = ORIENTED_EDGE ( 'NONE', *, *, #18197, .F. ) ;
#31662 = CARTESIAN_POINT ( 'NONE',  ( 17.95501807827959695, -7.982682978349759928, -42.86204958412849919 ) ) ;
#31663 = ORIENTED_EDGE ( 'NONE', *, *, #453, .F. ) ;
#31664 = EDGE_CURVE ( 'NONE', #14121, #27414, #10902, .T. ) ;
#31665 = CARTESIAN_POINT ( 'NONE',  ( 11.96242383438930013, -65.43598681641390158, -17.67418089159339800 ) ) ;
#31666 = CARTESIAN_POINT ( 'NONE',  ( 10.84460789103059852, 32.90608426506580031, -45.64388948703140159 ) ) ;
#31667 = CARTESIAN_POINT ( 'NONE',  ( 72.84798422376138660, 1.369544300367010026, -62.51645495968789845 ) ) ;
#31668 = CARTESIAN_POINT ( 'NONE',  ( 14.06313816487032753, -23.32125786362827569, -40.37567779348978547 ) ) ;
#31669 = CARTESIAN_POINT ( 'NONE',  ( 8.792634198315560923, 31.92357537073090157, -46.67064936031920297 ) ) ;
#31670 = CARTESIAN_POINT ( 'NONE',  ( 13.79233564179163629, -22.26896734107802445, -67.45490599494564776 ) ) ;
#31671 = AXIS2_PLACEMENT_3D ( 'NONE', #36595, #13290, #697 ) ;
#31672 = AXIS2_PLACEMENT_3D ( 'NONE', #45888, #9975, #25937 ) ;
#31673 = ORIENTED_EDGE ( 'NONE', *, *, #27565, .F. ) ;
#31674 = CARTESIAN_POINT ( 'NONE',  ( 64.95360084570988590, 1.395196698723379924, -70.24366017557039754 ) ) ;
#31675 = CARTESIAN_POINT ( 'NONE',  ( 11.10570106179580030, -63.43849378863360045, -44.25865445854999791 ) ) ;
#31676 = CARTESIAN_POINT ( 'NONE',  ( 70.83393739769690001, 16.88381105531749782, -71.50000000000000000 ) ) ;
#31677 = ORIENTED_EDGE ( 'NONE', *, *, #4399, .T. ) ;
#31678 = CARTESIAN_POINT ( 'NONE',  ( 67.09900444977570544, -33.06551488220966917, -20.08988936614202103 ) ) ;
#31679 = CARTESIAN_POINT ( 'NONE',  ( 56.53399784873889899, 19.21501630139210093, -52.81205167924800037 ) ) ;
#31680 = CARTESIAN_POINT ( 'NONE',  ( 31.69621505786460247, -15.61618894467929763, -6.649999999999999467 ) ) ;
#31681 = VERTEX_POINT ( 'NONE', #45533 ) ;
#31682 = CARTESIAN_POINT ( 'NONE',  ( 45.68512934788849833, -33.42474020775232191, -54.50653973161868038 ) ) ;
#31683 = DIRECTION ( 'NONE',  ( 1.000000000000000000, 1.964275807512750486E-11, -1.224636774179748846E-16 ) ) ;
#31684 = CARTESIAN_POINT ( 'NONE',  ( 57.35856957771729725, -50.13596282240779800, -52.61941485477820635 ) ) ;
#31685 = FACE_OUTER_BOUND ( 'NONE', #45327, .T. ) ;
#31686 = ADVANCED_FACE ( 'NONE', ( #41590 ), #21913, .T. ) ;
#31687 = CARTESIAN_POINT ( 'NONE',  ( 23.80679600161530374, -12.59791776729979951, -69.67303606471159583 ) ) ;
#31688 = CARTESIAN_POINT ( 'NONE',  ( 16.13393739769620083, -15.61618894467929941, -34.64999999999999858 ) ) ;
#31689 = CARTESIAN_POINT ( 'NONE',  ( 46.02470361814555844, -38.15599428330931886, -60.19611770114092053 ) ) ;
#31690 = VERTEX_POINT ( 'NONE', #26622 ) ;
#31691 = VERTEX_POINT ( 'NONE', #9629 ) ;
#31692 = CARTESIAN_POINT ( 'NONE',  ( 21.61858969539150266, -20.65853789913799687, -66.46929104108710362 ) ) ;
#31693 = CARTESIAN_POINT ( 'NONE',  ( 19.94107633810069657, -40.34105917676275510, -34.79644660940672907 ) ) ;
#31694 = FACE_OUTER_BOUND ( 'NONE', #33006, .T. ) ;
#31695 = CARTESIAN_POINT ( 'NONE',  ( 47.04916798185949744, 22.99805076571630025, -75.51723258725729693 ) ) ;
#31696 = FACE_OUTER_BOUND ( 'NONE', #18073, .T. ) ;
#31697 = CARTESIAN_POINT ( 'NONE',  ( 63.34104417888273986, 21.88381105532059934, 17.05710678118654755 ) ) ;
#31698 = AXIS2_PLACEMENT_3D ( 'NONE', #36540, #28412, #45197 ) ;
#31699 = AXIS2_PLACEMENT_3D ( 'NONE', #13129, #45075, #9184 ) ;
#31701 = CIRCLE ( 'NONE', #9146, 2.999999999999999112 ) ;
#31700 = CARTESIAN_POINT ( 'NONE',  ( 17.63700976455559655, -7.509186158879920470, -69.06602187564659801 ) ) ;
#31702 = CARTESIAN_POINT ( 'NONE',  ( 22.96155967568899925, -13.55454926668129900, -32.14999999999999858 ) ) ;
#31703 = CARTESIAN_POINT ( 'NONE',  ( 56.57655762862680149, -50.65586698240579722, -74.96720691208240339 ) ) ;
#31705 = CARTESIAN_POINT ( 'NONE',  ( 20.29254050540992438, -10.20481584277917619, -60.16112895304275554 ) ) ;
#31704 = CARTESIAN_POINT ( 'NONE',  ( -4.807165379747050160, 16.23227173892630049, -5.209035753736800167 ) ) ;
#31706 = AXIS2_PLACEMENT_3D ( 'NONE', #30707, #46729, #10813 ) ;
#31707 = CARTESIAN_POINT ( 'NONE',  ( 63.01386660552499563, 0.9960089569207349891, -68.76188247756290650 ) ) ;
#31708 = CARTESIAN_POINT ( 'NONE',  ( 61.39380661293360220, 13.96359161412859962, -46.71089551414399921 ) ) ;
#31709 = CYLINDRICAL_SURFACE ( 'NONE', #28084, 3.000000000000000444 ) ;
#31710 = EDGE_LOOP ( 'NONE', ( #46364, #37174, #13811 ) ) ;
#31711 = CARTESIAN_POINT ( 'NONE',  ( 53.36905185836059928, -49.37836840941449168, -48.78905575734700051 ) ) ;
#31712 = CARTESIAN_POINT ( 'NONE',  ( 61.30987170295029642, -45.21799793180310445, -28.05306858404509995 ) ) ;
#31713 = DIRECTION ( 'NONE',  ( 1.000000000000000000, 0.000000000000000000, 0.000000000000000000 ) ) ;
#31714 = CARTESIAN_POINT ( 'NONE',  ( 56.53685690055910129, 14.99694011007190220, -26.26932896201929779 ) ) ;
#31715 = CARTESIAN_POINT ( 'NONE',  ( 10.21705801865680030, -11.08880203620289961, -73.44055697468560595 ) ) ;
#31716 = CARTESIAN_POINT ( 'NONE',  ( 51.50420584715260475, 18.17752645460259942, -76.63112831200879782 ) ) ;
#31717 = CARTESIAN_POINT ( 'NONE',  ( 52.78519658503790168, 18.45700756790349928, -48.68757693859610214 ) ) ;
#31718 = DIRECTION ( 'NONE',  ( 1.000000000000000000, 0.000000000000000000, 0.000000000000000000 ) ) ;
#31719 = CARTESIAN_POINT ( 'NONE',  ( 53.20760851556250515, -49.46295310004039436, -48.79936141347000245 ) ) ;
#31720 = ADVANCED_FACE ( 'NONE', ( #30034 ), #48167, .T. ) ;
#31721 = VERTEX_POINT ( 'NONE', #42639 ) ;
#31722 = CARTESIAN_POINT ( 'NONE',  ( 13.05521822061467319, 18.23736444591386174, -34.79644660940673617 ) ) ;
#31723 = CARTESIAN_POINT ( 'NONE',  ( 47.60135642093380426, -54.55175135494879868, -55.04890805189040037 ) ) ;
#31724 = FACE_BOUND ( 'NONE', #5349, .T. ) ;
#31725 = CARTESIAN_POINT ( 'NONE',  ( 17.90521499757843316, -22.20705366312095208, -70.86948871188650401 ) ) ;
#31726 = CARTESIAN_POINT ( 'NONE',  ( 65.07885343532089450, -32.17484660787989981, -17.72663174665169805 ) ) ;
#31727 = CARTESIAN_POINT ( 'NONE',  ( 71.50269221454749413, 1.097545367735389910, -60.73071135393699649 ) ) ;
#31728 = CARTESIAN_POINT ( 'NONE',  ( -4.615472129303443971, -42.73836944035205931, -38.77992132782590318 ) ) ;
#31729 = CARTESIAN_POINT ( 'NONE',  ( 72.80373209685389213, 0.9973858971044751165, -61.88154445005670112 ) ) ;
#31730 = FACE_BOUND ( 'NONE', #20636, .T. ) ;
#31731 = FACE_OUTER_BOUND ( 'NONE', #17206, .T. ) ;
#31732 = ORIENTED_EDGE ( 'NONE', *, *, #2844, .T. ) ;
#31733 = ORIENTED_EDGE ( 'NONE', *, *, #39016, .F. ) ;
#31734 = CARTESIAN_POINT ( 'NONE',  ( 24.04493737731856839, -14.58063703369262321, -55.75066751970105372 ) ) ;
#31735 = CARTESIAN_POINT ( 'NONE',  ( 19.54197066778965208, -21.52907534521731137, -58.78615336081859510 ) ) ;
#31736 = VERTEX_POINT ( 'NONE', #15626 ) ;
#31737 = DIRECTION ( 'NONE',  ( 0.000000000000000000, 0.000000000000000000, 1.000000000000000000 ) ) ;
#31738 = CARTESIAN_POINT ( 'NONE',  ( 21.71994269503706221, -21.21801661426634666, -77.75811212484384782 ) ) ;
#31739 = CARTESIAN_POINT ( 'NONE',  ( 29.13393739769619728, -26.76363820448759867, -35.14999999999999858 ) ) ;
#31740 = AXIS2_PLACEMENT_3D ( 'NONE', #11452, #7255, #27409 ) ;
#31741 = ADVANCED_FACE ( 'NONE', ( #19545 ), #7766, .F. ) ;
#31742 = TOROIDAL_SURFACE ( 'NONE', #13372, 18.00000000000000000, 2.000000000000000000 ) ;
#31743 = ORIENTED_EDGE ( 'NONE', *, *, #8555, .F. ) ;
#31744 = CARTESIAN_POINT ( 'NONE',  ( 11.40398156086318160, 34.03074001837894969, -22.75443495787784798 ) ) ;
#31745 = AXIS2_PLACEMENT_3D ( 'NONE', #14969, #6863, #7632 ) ;
#31746 = CARTESIAN_POINT ( 'NONE',  ( 44.33589047729159915, 6.728771102257818271, -68.64023485869353181 ) ) ;
#31747 = FACE_OUTER_BOUND ( 'NONE', #32762, .T. ) ;
#31748 = AXIS2_PLACEMENT_3D ( 'NONE', #40382, #24628, #33015 ) ;
#31749 = AXIS2_PLACEMENT_3D ( 'NONE', #13084, #49744, #36632 ) ;
#31750 = ADVANCED_FACE ( 'NONE', ( #51011 ), #18881, .T. ) ;
#31751 = CARTESIAN_POINT ( 'NONE',  ( 9.653580312505349426, -20.71400142694579927, -42.58016164095380418 ) ) ;
#31752 = CARTESIAN_POINT ( 'NONE',  ( 23.83903569875588246, -17.68687415037926769, -67.59099925309431001 ) ) ;
#31753 = AXIS2_PLACEMENT_3D ( 'NONE', #21353, #8549, #668 ) ;
#31754 = CARTESIAN_POINT ( 'NONE',  ( 24.02301761236539690, -16.22472933103653503, -49.81682925502759929 ) ) ;
#31755 = ADVANCED_FACE ( 'NONE', ( #22612 ), #2720, .T. ) ;
#31756 = SHAPE_REPRESENTATION_RELATIONSHIP ( 'NONE' , 'NONE' ,  #4374, #33546 ) ;
#31757 = CARTESIAN_POINT ( 'NONE',  ( 64.07783773375270187, -29.99138570131350434, -16.37128087021990197 ) ) ;
#31758 =( BOUNDED_CURVE ( )  B_SPLINE_CURVE ( 3, ( #30612, #37721, #46379, #1816 ),
 .UNSPECIFIED., .F., .T. ) 
 B_SPLINE_CURVE_WITH_KNOTS ( ( 4, 4 ),
 ( 2.356194490192327962, 3.141592653589778905 ),
 .UNSPECIFIED. ) 
 CURVE ( )  GEOMETRIC_REPRESENTATION_ITEM ( )  RATIONAL_B_SPLINE_CURVE ( ( 1.000000000000000000, 0.9492530216741907889, 0.9492530216741907889, 1.000000000000000000 ) ) 
 REPRESENTATION_ITEM ( '' )  );
#31759 = DIRECTION ( 'NONE',  ( 0.000000000000000000, 0.000000000000000000, -1.000000000000000000 ) ) ;
#31760 = CARTESIAN_POINT ( 'NONE',  ( 21.55489477686560207, -21.29069056903449919, -72.26976689927120390 ) ) ;
#31761 = CARTESIAN_POINT ( 'NONE',  ( 14.36270743733633104, -22.20706670009677097, -37.03615240734319514 ) ) ;
#31762 = CARTESIAN_POINT ( 'NONE',  ( 45.28528579602679116, 14.15028987964289975, -8.309926139390320543 ) ) ;
#31763 = CARTESIAN_POINT ( 'NONE',  ( 14.90280646933509878, 21.76199957607230218, -76.14999999999999147 ) ) ;
#31764 = CARTESIAN_POINT ( 'NONE',  ( 83.62075525755088279, -44.78170833223440184, -47.10035895585609467 ) ) ;
#31765 = CARTESIAN_POINT ( 'NONE',  ( 64.28413441608979895, 1.451794159057709921, -69.91814348332408713 ) ) ;
#31766 = CARTESIAN_POINT ( 'NONE',  ( 23.50805523095529992, -11.92767882673400059, -47.36003476421500125 ) ) ;
#31767 = ORIENTED_EDGE ( 'NONE', *, *, #4771, .T. ) ;
#31768 = CARTESIAN_POINT ( 'NONE',  ( 53.59175609322679890, -48.99677226645609096, -27.20769021208899829 ) ) ;
#31769 = CARTESIAN_POINT ( 'NONE',  ( 11.13902037554059987, -63.56347337547460796, -14.91063010085480123 ) ) ;
#31770 = CARTESIAN_POINT ( 'NONE',  ( 21.26855178092368703, -21.65669804013363375, -39.78344367522398528 ) ) ;
#31771 = CARTESIAN_POINT ( 'NONE',  ( 22.89855964779329867, -15.80993874071388561, -56.46193748095264198 ) ) ;
#31772 =( REPRESENTATION_RELATIONSHIP ('NONE','NONE', #29764, #4683 ) REPRESENTATION_RELATIONSHIP_WITH_TRANSFORMATION ( #23569 )SHAPE_REPRESENTATION_RELATIONSHIP( ) );
#31773 = FACE_OUTER_BOUND ( 'NONE', #40405, .T. ) ;
#31774 = AXIS2_PLACEMENT_3D ( 'NONE', #26800, #42812, #7 ) ;
#31775 = ORIENTED_EDGE ( 'NONE', *, *, #25820, .T. ) ;
#31776 = CIRCLE ( 'NONE', #5034, 0.5000000000000000000 ) ;
#31777 = CYLINDRICAL_SURFACE ( 'NONE', #38147, 0.4999999999999983347 ) ;
#31778 = CIRCLE ( 'NONE', #43526, 2.700000000000230216 ) ;
#31779 = CARTESIAN_POINT ( 'NONE',  ( 47.18324198357279897, 23.57489020266570279, -54.61058319554400242 ) ) ;
#31781 = CIRCLE ( 'NONE', #9234, 0.5000000000000028866 ) ;
#31780 = DIRECTION ( 'NONE',  ( 0.7071067811865461294, -0.7071067811865490160, 0.000000000000000000 ) ) ;
#31782 = CARTESIAN_POINT ( 'NONE',  ( 63.06393505168800573, 0.8850831926798630178, -62.44126551166660022 ) ) ;
#31783 = CARTESIAN_POINT ( 'NONE',  ( 57.47779638733530305, -50.55916219015709601, -53.44452029295939610 ) ) ;
#31784 = CARTESIAN_POINT ( 'NONE',  ( 43.31938993097590185, 11.95891240614390050, -4.740111887263790180 ) ) ;
#31785 = DIRECTION ( 'NONE',  ( 0.000000000000000000, 1.000000000000000000, 0.000000000000000000 ) ) ;
#31786 = CARTESIAN_POINT ( 'NONE',  ( 63.27838127973589621, 0.9150552061906049861, -62.12504221718980091 ) ) ;
#31787 = DIRECTION ( 'NONE',  ( -2.565320000000000120E-13, 1.000000000000000000, -8.628712999999999808E-13 ) ) ;
#31788 = CARTESIAN_POINT ( 'NONE',  ( -0.1863042805355769327, -20.57828601760577669, -34.92844344776042220 ) ) ;
#31789 = EDGE_CURVE ( 'NONE', #47534, #47610, #32355, .T. ) ;
#31790 = CARTESIAN_POINT ( 'NONE',  ( 105.5832649133809724, -15.41618894467840484, -65.65000000000004832 ) ) ;
#31791 = CARTESIAN_POINT ( 'NONE',  ( 20.30127474080349970, -42.11618894467939356, -34.64999999999999858 ) ) ;
#31792 = CARTESIAN_POINT ( 'NONE',  ( 10.03556564381850080, -19.89597355255950362, -63.87256020652749555 ) ) ;
#31793 = LINE ( 'NONE', #14343, #48853 ) ;
#31794 = CARTESIAN_POINT ( 'NONE',  ( 63.30304092011348871, 0.9208623934744509798, -62.09132346512829770 ) ) ;
#31795 = EDGE_LOOP ( 'NONE', ( #29687, #9011, #21574, #14269, #25012 ) ) ;
#31796 = CARTESIAN_POINT ( 'NONE',  ( 72.72056432233058842, 1.396834109478129804, -62.44999999999999574 ) ) ;
#31797 = CARTESIAN_POINT ( 'NONE',  ( 20.91567610440962000, -20.47173450993272681, -34.70503499978224227 ) ) ;
#31798 = CARTESIAN_POINT ( 'NONE',  ( 73.13559359734860266, 0.8904513541338849869, -68.96413986139360475 ) ) ;
#31799 = DIRECTION ( 'NONE',  ( 1.000000000000000000, 0.000000000000000000, 0.000000000000000000 ) ) ;
#31800 = CARTESIAN_POINT ( 'NONE',  ( 9.588579560587598749, -12.15087335004630020, -81.23899999999999011 ) ) ;
#31801 = EDGE_LOOP ( 'NONE', ( #46957, #42592, #6608, #10045, #50706 ) ) ;
#31802 = CARTESIAN_POINT ( 'NONE',  ( 17.21347160910339724, 21.88381105532300097, -76.14999999999999147 ) ) ;
#31803 = EDGE_LOOP ( 'NONE', ( #33068, #26632 ) ) ;
#31804 = VERTEX_POINT ( 'NONE', #51194 ) ;
#31805 = CARTESIAN_POINT ( 'NONE',  ( 56.82261506997360101, -46.00315760091039152, -26.24626569297650036 ) ) ;
#31806 = CARTESIAN_POINT ( 'NONE',  ( 22.54657568291069936, -11.21650286210249980, -81.23899999999999011 ) ) ;
#31807 = DIRECTION ( 'NONE',  ( -0.3863301728269311619, 0.9223605572461961444, 1.110223024625156171E-16 ) ) ;
#31808 = DIRECTION ( 'NONE',  ( 0.000000000000000000, 0.000000000000000000, 1.000000000000000000 ) ) ;
#31809 = ORIENTED_EDGE ( 'NONE', *, *, #26051, .F. ) ;
#31810 = CARTESIAN_POINT ( 'NONE',  ( 61.31807987960689843, -45.64188066342459393, -47.72348187499480332 ) ) ;
#31811 = VERTEX_POINT ( 'NONE', #3497 ) ;
#31812 = CARTESIAN_POINT ( 'NONE',  ( 11.26605718498006681, -64.23738894431306790, -24.07455686696101438 ) ) ;
#31813 = EDGE_CURVE ( 'NONE', #31549, #47622, #42505, .T. ) ;
#31814 = CARTESIAN_POINT ( 'NONE',  ( 59.43561021697854585, -45.50358387466955179, -26.70526119467472981 ) ) ;
#31815 = VERTEX_POINT ( 'NONE', #23883 ) ;
#31816 = AXIS2_PLACEMENT_3D ( 'NONE', #34912, #64, #31226 ) ;
#31817 = EDGE_LOOP ( 'NONE', ( #26138, #51642, #22203, #21170 ) ) ;
#31818 = CARTESIAN_POINT ( 'NONE',  ( 10.57891470305085235, -21.28119600275288192, -50.25446074854212952 ) ) ;
#31819 = FACE_OUTER_BOUND ( 'NONE', #17904, .T. ) ;
#31820 = VECTOR ( 'NONE', #41174, 1000.000000000000000 ) ;
#31821 = CARTESIAN_POINT ( 'NONE',  ( 61.07324514817819505, 14.25386249272230010, -47.46813279917520134 ) ) ;
#31822 = AXIS2_PLACEMENT_3D ( 'NONE', #50605, #7107, #22799 ) ;
#31823 = DIRECTION ( 'NONE',  ( 0.000000000000000000, 0.000000000000000000, -1.000000000000000000 ) ) ;
#31824 = FACE_OUTER_BOUND ( 'NONE', #32900, .T. ) ;
#31825 = CARTESIAN_POINT ( 'NONE',  ( -7.968494235580870111, 13.83148165310410072, -5.506078144787959872 ) ) ;
#31826 = CARTESIAN_POINT ( 'NONE',  ( 17.92370450339619836, 20.88381105532299742, -74.14999999999999147 ) ) ;
#31827 = CARTESIAN_POINT ( 'NONE',  ( 58.53215119733189908, 14.40509552366270007, -26.46582177025860005 ) ) ;
#31828 = CARTESIAN_POINT ( 'NONE',  ( 11.39303770747540057, -21.87003722477430046, -65.99397745470540144 ) ) ;
#31829 = ORIENTED_EDGE ( 'NONE', *, *, #39955, .T. ) ;
#31830 = DIRECTION ( 'NONE',  ( 0.000000000000000000, 0.000000000000000000, 1.000000000000000000 ) ) ;
#31831 = CARTESIAN_POINT ( 'NONE',  ( 41.03169806305130152, 14.25711695494940123, -6.001447860943059709 ) ) ;
#31832 = CARTESIAN_POINT ( 'NONE',  ( -5.066062602303800233, -15.61618894467930119, -12.65000000000000036 ) ) ;
#31833 = CARTESIAN_POINT ( 'NONE',  ( 72.39774331670469110, 1.277124412296150036, -69.78360917201301561 ) ) ;
#31834 = CARTESIAN_POINT ( 'NONE',  ( 44.26457877669638918, -39.97584597393014150, -65.37864771724724733 ) ) ;
#31835 = CARTESIAN_POINT ( 'NONE',  ( 46.35275103504449845, -52.90993241930539881, -76.14999999999999147 ) ) ;
#31836 = CARTESIAN_POINT ( 'NONE',  ( 8.222950370390678998, -16.35708134086146615, -32.47786278411599170 ) ) ;
#31837 = CARTESIAN_POINT ( 'NONE',  ( 63.23690831390890565, 1.005545696829380109, -69.10544663728329340 ) ) ;
#31838 = CARTESIAN_POINT ( 'NONE',  ( 48.62042966150410450, -53.96634867048729234, -54.57170596908269999 ) ) ;
#31839 = CARTESIAN_POINT ( 'NONE',  ( 51.87293486654318286, -32.75009382961766136, -18.77186997386058209 ) ) ;
#31840 = ADVANCED_FACE ( 'NONE', ( #4004 ), #19209, .T. ) ;
#31841 = CARTESIAN_POINT ( 'NONE',  ( 64.57410506046470289, 0.9210617359723460851, -70.48005104816749622 ) ) ;
#31842 = CARTESIAN_POINT ( 'NONE',  ( 8.428818494671439510, -13.54557800259576439, -70.87566006981948874 ) ) ;
#31843 = ORIENTED_EDGE ( 'NONE', *, *, #2588, .F. ) ;
#31844 = CIRCLE ( 'NONE', #8428, 1.999999999999998224 ) ;
#31845 = CARTESIAN_POINT ( 'NONE',  ( 23.40719984908270135, -14.00177027172209954, -38.99781585255099259 ) ) ;
#31846 = EDGE_CURVE ( 'NONE', #31144, #17783, #45636, .T. ) ;
#31847 = CARTESIAN_POINT ( 'NONE',  ( 19.54190535476944390, -21.52911439740251964, -76.78616460542943400 ) ) ;
#31848 = ORIENTED_EDGE ( 'NONE', *, *, #921, .F. ) ;
#31849 = CARTESIAN_POINT ( 'NONE',  ( 18.22265159334490292, 21.07288667571724616, -75.74021525124661025 ) ) ;
#31850 = AXIS2_PLACEMENT_3D ( 'NONE', #48701, #13319, #49732 ) ;
#31851 = CARTESIAN_POINT ( 'NONE',  ( 60.78493093637079880, -45.56573178202909702, -47.44768458244219289 ) ) ;
#31852 = CARTESIAN_POINT ( 'NONE',  ( 37.11786083938510217, -15.61618894467929941, 6.789625226207629538 ) ) ;
#31853 = CARTESIAN_POINT ( 'NONE',  ( 7.492845759203720313, 29.94784237631284896, -20.13893727953968948 ) ) ;
#31855 = CARTESIAN_POINT ( 'NONE',  ( 44.65669779474150403, -33.16208384341911852, -44.90189889201600693 ) ) ;
#31854 = CARTESIAN_POINT ( 'NONE',  ( 42.40667996754965685, 8.575301686933304524, -74.36634363102189127 ) ) ;
#31856 = AXIS2_PLACEMENT_3D ( 'NONE', #31622, #47899, #699 ) ;
#31857 = B_SPLINE_CURVE_WITH_KNOTS ( 'NONE', 3,
 ( #17627, #29145, #5321, #33597, #592, #45146, #13449, #45665, #41465, #16577, #5582, #12668, #25719, #49093, #21021, #37020 ),
 .UNSPECIFIED., .F., .F.,
 ( 4, 2, 2, 2, 2, 2, 2, 4 ),
 ( 0.000000000000000000, 2.070511893743590015, 3.936888812047690145, 5.103374385987740069, 5.832427869700280709, 7.290534837125340673, 9.623505985005449404, 11.66485573940060050 ),
 .UNSPECIFIED. ) ;
#31858 = EDGE_CURVE ( 'NONE', #28603, #34738, #35600, .T. ) ;
#31859 = CARTESIAN_POINT ( 'NONE',  ( 71.27262092911109903, 0.8838110553206740549, -70.76364393196210756 ) ) ;
#31860 = CARTESIAN_POINT ( 'NONE',  ( -5.316689532470439516, -0.1743001472114563133, -59.64999999999999147 ) ) ;
#31861 = EDGE_LOOP ( 'NONE', ( #8292, #28962, #39445, #9281, #42085 ) ) ;
#31862 = LINE ( 'NONE', #35814, #40695 ) ;
#31863 = ORIENTED_EDGE ( 'NONE', *, *, #3906, .T. ) ;
#31864 = VERTEX_POINT ( 'NONE', #7170 ) ;
#31865 = CARTESIAN_POINT ( 'NONE',  ( 16.13393739769620083, -15.61618894467919816, -82.14319696191608955 ) ) ;
#31866 = CARTESIAN_POINT ( 'NONE',  ( 15.09842697026319414, -7.705184469708584949, -79.25066590858526183 ) ) ;
#31867 = CARTESIAN_POINT ( 'NONE',  ( 76.39112045134315565, -16.55782844447705315, -12.75825074068906240 ) ) ;
#31868 = ORIENTED_EDGE ( 'NONE', *, *, #43962, .F. ) ;
#31869 = EDGE_LOOP ( 'NONE', ( #36438, #49513 ) ) ;
#31870 = DIRECTION ( 'NONE',  ( -0.3502816565540429750, 0.000000000000000000, 0.9366444154970205993 ) ) ;
#31871 = CARTESIAN_POINT ( 'NONE',  ( 56.64799623678120355, -45.30988597762969761, -25.29367807365969867 ) ) ;
#31872 = CARTESIAN_POINT ( 'NONE',  ( 56.32100277383929665, -50.57626126597089922, -52.90110794044780107 ) ) ;
#31873 = CARTESIAN_POINT ( 'NONE',  ( 60.18087665363530192, -1.847621400935020031, -15.84374030865019733 ) ) ;
#31874 = EDGE_CURVE ( 'NONE', #49378, #46311, #49013, .T. ) ;
#31875 = CARTESIAN_POINT ( 'NONE',  ( 51.46000099094769809, -49.32027946797799700, -76.62475863447160407 ) ) ;
#31876 = B_SPLINE_SURFACE_WITH_KNOTS ( 'NONE', 3, 3, ( 
 ( #33464, #8864, #32940, #17243, #9887, #25336, #993, #9120, #25844, #36620, #41088, #20632 ),
 ( #29024, #16992, #5200, #37158, #1256, #33206, #49225, #41339, #17496, #13571, #25590, #41595 ),
 ( #14078, #15114, #11190, #2544, #18005, #18778, #33970, #14853, #50503, #41856, #2026, #18257 ),
 ( #31074, #19036, #3065, #30562, #22436, #34753, #30039, #34226, #18525, #35011, #14593, #10152 ) ),
 .UNSPECIFIED., .F., .F., .F.,
 ( 4, 4 ),
 ( 4, 1, 1, 1, 1, 1, 1, 1, 1, 4 ),
 ( -0.1293119798323739966, 3.989325000000000270E-14 ),
 ( 0.000000000000000000, 0.1111111111111110078, 0.2222222222222219878, 0.3333333333333329818, 0.4444444444444439757, 0.5555555555555560243, 0.6666666666666670737, 0.7777777777777779011, 0.8888888888888889506, 1.000000000000000000 ),
 .UNSPECIFIED. ) ;
#31877 = ORIENTED_EDGE ( 'NONE', *, *, #35492, .T. ) ;
#31878 = DIRECTION ( 'NONE',  ( 0.000000000000000000, 1.000000000000000000, 0.000000000000000000 ) ) ;
#31879 = CARTESIAN_POINT ( 'NONE',  ( 53.07826439650979466, -50.35436285572949089, -77.22375575988948526 ) ) ;
#31880 = CARTESIAN_POINT ( 'NONE',  ( 14.43936601292799438, -9.036495058040628692, -33.87268009392107615 ) ) ;
#31881 = CARTESIAN_POINT ( 'NONE',  ( 52.56521993351449851, -49.86179673305689874, -28.15000000000000213 ) ) ;
#31882 = CARTESIAN_POINT ( 'NONE',  ( 13.78323292975819925, -8.128803813941159362, -53.41566130612969943 ) ) ;
#31883 = CARTESIAN_POINT ( 'NONE',  ( 12.76120696353130057, -49.98606220861660177, -21.08963177777529907 ) ) ;
#31884 = CARTESIAN_POINT ( 'NONE',  ( 52.13393739769618662, -0.5161889446793590519, -65.65000000000000568 ) ) ;
#31885 = CARTESIAN_POINT ( 'NONE',  ( 68.13393739769649926, -48.11618894467630270, -70.54999999999999716 ) ) ;
#31886 = CARTESIAN_POINT ( 'NONE',  ( 60.85051643030340074, -45.45861950383179817, -47.01183782209979967 ) ) ;
#31887 = CONICAL_SURFACE ( 'NONE', #6829, 1.154999999999999361, 0.08090409915523018303 ) ;
#31888 = CARTESIAN_POINT ( 'NONE',  ( 17.01978215929854699, -22.38318229988689367, -38.91115524470608023 ) ) ;
#31889 = VECTOR ( 'NONE', #3744, 1000.000000000000000 ) ;
#31890 = EDGE_CURVE ( 'NONE', #1136, #43399, #2488, .T. ) ;
#31891 = CARTESIAN_POINT ( 'NONE',  ( 9.193808866418558878, -16.87204528351649913, -57.79019640516870027 ) ) ;
#31892 = CARTESIAN_POINT ( 'NONE',  ( 9.543029255252220011, -13.84506841537463373, -43.53614410085236841 ) ) ;
#31893 = CIRCLE ( 'NONE', #8463, 1.999999999999998224 ) ;
#31894 = ORIENTED_EDGE ( 'NONE', *, *, #45631, .F. ) ;
#31895 = CARTESIAN_POINT ( 'NONE',  ( 13.60550091177310073, -51.43165038652990262, -74.14992922886710858 ) ) ;
#31896 = CARTESIAN_POINT ( 'NONE',  ( 47.30522570423300266, -54.71767344092400265, -54.76519543323880157 ) ) ;
#31897 = FILL_AREA_STYLE_COLOUR ( '', #23213 ) ;
#31898 = CARTESIAN_POINT ( 'NONE',  ( 17.01972112733642462, -8.849186874510190037, -37.99448857803940882 ) ) ;
#31899 = DIRECTION ( 'NONE',  ( 0.000000000000000000, 0.000000000000000000, -1.000000000000000000 ) ) ;
#31900 = CARTESIAN_POINT ( 'NONE',  ( 61.35257968416159713, 13.88381105532070059, -11.49663005730239895 ) ) ;
#31901 = CARTESIAN_POINT ( 'NONE',  ( 14.36259954236786918, -9.025339123761108695, -75.86946488318916693 ) ) ;
#31902 = CARTESIAN_POINT ( 'NONE',  ( 11.41950678101309968, 34.12481452477189947, -18.15863199430730290 ) ) ;
#31903 = CARTESIAN_POINT ( 'NONE',  ( 18.86653953160487163, -8.170294702091634775, -65.11960522023254327 ) ) ;
#31905 = CARTESIAN_POINT ( 'NONE',  ( -8.077363885194191795, -45.04970852165219952, -5.734713034113010366 ) ) ;
#31904 = DIRECTION ( 'NONE',  ( 0.000000000000000000, 0.000000000000000000, 1.000000000000000000 ) ) ;
#31906 = CARTESIAN_POINT ( 'NONE',  ( -8.936452451236569061, -44.38145624430249825, -6.564714805037400680 ) ) ;
#31907 = CARTESIAN_POINT ( 'NONE',  ( 49.59785998471309654, 22.46914640684560283, -55.11090114299469889 ) ) ;
#31908 = ORIENTED_EDGE ( 'NONE', *, *, #41330, .F. ) ;
#31909 = CARTESIAN_POINT ( 'NONE',  ( 53.05390111010630250, -49.57533313438899825, -49.03220058437089790 ) ) ;
#31910 = EDGE_LOOP ( 'NONE', ( #36128, #8560, #24036, #11734, #48404 ) ) ;
#31911 = CARTESIAN_POINT ( 'NONE',  ( 47.33846070720256449, 6.770505468649851366, -53.56164933099653780 ) ) ;
#31912 = CARTESIAN_POINT ( 'NONE',  ( 10.72266925234624679, -19.77492588197056378, -75.24448688531667528 ) ) ;
#31913 = DIRECTION ( 'NONE',  ( 0.000000000000000000, 0.000000000000000000, 1.000000000000000000 ) ) ;
#31914 = CARTESIAN_POINT ( 'NONE',  ( 83.73251846585449698, 13.29777256131780128, -46.86010343433790126 ) ) ;
#31915 = CARTESIAN_POINT ( 'NONE',  ( 9.158617068706689679, -14.57337304308830106, -57.50005794035820372 ) ) ;
#31917 = EDGE_CURVE ( 'NONE', #28850, #35503, #17999, .T. ) ;
#31916 = CARTESIAN_POINT ( 'NONE',  ( -0.4410626023037880206, -27.49517073325580085, -35.14999999999999858 ) ) ;
#31918 = CARTESIAN_POINT ( 'NONE',  ( 55.95983537943720165, -45.42096113467239604, -16.30775385143880030 ) ) ;
#31919 = CARTESIAN_POINT ( 'NONE',  ( 53.08725068471199648, 18.06569830069809868, -26.91751262120149590 ) ) ;
#31920 = ORIENTED_EDGE ( 'NONE', *, *, #16653, .T. ) ;
#31921 = CARTESIAN_POINT ( 'NONE',  ( 11.87411739806599797, -9.025234404255449761, -44.60486606752819938 ) ) ;
#31922 = EDGE_LOOP ( 'NONE', ( #10884, #21168, #23296, #36747, #28193 ) ) ;
#31923 = CARTESIAN_POINT ( 'NONE',  ( 11.92291171973240083, -65.34405718864840651, -17.18421396917739941 ) ) ;
#31924 = CARTESIAN_POINT ( 'NONE',  ( 10.89794792890609898, 33.54155821960309680, -46.64989010007410286 ) ) ;
#31925 = CARTESIAN_POINT ( 'NONE',  ( 73.08617409304301304, 0.9989215084294049696, -62.27490163988890259 ) ) ;
#31926 = CIRCLE ( 'NONE', #149, 0.5000000000000000000 ) ;
#31927 = LINE ( 'NONE', #27234, #18492 ) ;
#31928 = DIRECTION ( 'NONE',  ( 0.000000000000000000, 1.000000000000000000, 0.000000000000000000 ) ) ;
#31929 = CARTESIAN_POINT ( 'NONE',  ( 51.37210604755092191, 3.311019760866724226, -76.66704681122699583 ) ) ;
#31930 = CIRCLE ( 'NONE', #16889, 6.049999999999999822 ) ;
#31931 = VERTEX_POINT ( 'NONE', #24398 ) ;
#31932 = CARTESIAN_POINT ( 'NONE',  ( 11.13393739769620616, 24.07008072128959597, -44.08754088842374586 ) ) ;
#31933 = CARTESIAN_POINT ( 'NONE',  ( 11.13393739769619906, -63.11543068638779630, -43.74348518090240390 ) ) ;
#31934 = CARTESIAN_POINT ( 'NONE',  ( 68.13393739769706769, 17.98087126524919555, -68.79648330188412331 ) ) ;
#31935 = ORIENTED_EDGE ( 'NONE', *, *, #34467, .F. ) ;
#31936 = CARTESIAN_POINT ( 'NONE',  ( 11.58381202359622364, -22.16518687231168627, -44.48577634035566319 ) ) ;
#31937 = CARTESIAN_POINT ( 'NONE',  ( 56.62432785583700223, 19.48323104976229914, -53.83726655423080132 ) ) ;
#31938 = CARTESIAN_POINT ( 'NONE',  ( 65.46029542295769943, -29.76883965895079953, -16.55376543218019947 ) ) ;
#31939 = CARTESIAN_POINT ( 'NONE',  ( 24.04493721399152051, -15.53462765768975196, -49.50438507894359930 ) ) ;
#31940 = ORIENTED_EDGE ( 'NONE', *, *, #20306, .F. ) ;
#31941 = CARTESIAN_POINT ( 'NONE',  ( 19.22157560178293423, -49.74868907930050455, -82.73668660645817852 ) ) ;
#31942 = CARTESIAN_POINT ( 'NONE',  ( 11.27237311615841087, -9.289937688271868055, -56.79933486857391500 ) ) ;
#31943 = CARTESIAN_POINT ( 'NONE',  ( 24.04487853986463008, -15.61618860033810030, -61.79233400586811342 ) ) ;
#31944 = CARTESIAN_POINT ( 'NONE',  ( 8.205515328865471858, -13.35281898941070011, -68.88084675407539237 ) ) ;
#31945 = CARTESIAN_POINT ( 'NONE',  ( 22.13393739769589885, 22.91950879131610108, -35.14999999999999858 ) ) ;
#31946 = CARTESIAN_POINT ( 'NONE',  ( 46.61351573269507043, -38.21450491841939368, -57.25208055290525522 ) ) ;
#31947 = VERTEX_POINT ( 'NONE', #21003 ) ;
#31948 = CARTESIAN_POINT ( 'NONE',  ( 11.53167905867499954, -21.47502090899229898, -66.94460462746880580 ) ) ;
#31949 = CARTESIAN_POINT ( 'NONE',  ( 52.95053218911250781, -49.64355395051840247, -49.05140896314050281 ) ) ;
#31950 = EDGE_CURVE ( 'NONE', #26981, #19127, #44999, .T. ) ;
#31951 = CARTESIAN_POINT ( 'NONE',  ( 38.67452568954060155, 4.883811055320659733, -84.65000000000000568 ) ) ;
#31952 = CARTESIAN_POINT ( 'NONE',  ( 10.21244040264410025, -20.49383822526380072, -32.14999999999999858 ) ) ;
#31953 = EDGE_CURVE ( 'NONE', #14876, #4764, #23307, .T. ) ;
#31954 = CARTESIAN_POINT ( 'NONE',  ( 46.91913817000130393, 22.75192970925369806, -75.76197391125640479 ) ) ;
#31955 = CARTESIAN_POINT ( 'NONE',  ( 71.03155062328740144, 1.383928098097870096, -60.96256459357869772 ) ) ;
#31956 = ADVANCED_FACE ( 'NONE', ( #2916 ), #27257, .T. ) ;
#31957 = CARTESIAN_POINT ( 'NONE',  ( 0.1246572822142906628, 19.61312073211624707, -34.68957853602456964 ) ) ;
#31958 = AXIS2_PLACEMENT_3D ( 'NONE', #31865, #3341, #19057 ) ;
#31959 = VECTOR ( 'NONE', #36573, 1000.000000000000000 ) ;
#31960 = CARTESIAN_POINT ( 'NONE',  ( 12.01222358505770060, 33.78335047254940093, -16.39655052252450318 ) ) ;
#31961 = CARTESIAN_POINT ( 'NONE',  ( 24.37792036543810070, -15.47666999773330154, -73.50228201520930327 ) ) ;
#31962 = B_SPLINE_CURVE_WITH_KNOTS ( 'NONE', 3,
 ( #6715, #37638, #18233, #49708, #34727, #29754 ),
 .UNSPECIFIED., .F., .F.,
 ( 4, 2, 4 ),
 ( -0.3033244957681310305, -0.3025616577353109626, -0.2608998691367954148 ),
 .UNSPECIFIED. ) ;
#31963 = CARTESIAN_POINT ( 'NONE',  ( 56.83675909612700394, -50.64711008564240302, -74.57384771777940102 ) ) ;
#31965 = CARTESIAN_POINT ( 'NONE',  ( 17.01966651355726867, -8.849179074080744556, -59.99445920821477785 ) ) ;
#31964 = DIRECTION ( 'NONE',  ( 0.5835456732599411112, 0.8120803206700689669, 0.000000000000000000 ) ) ;
#31966 = CARTESIAN_POINT ( 'NONE',  ( 63.08453170404659716, 0.9940423591679348192, -68.87653036433009390 ) ) ;
#31967 = B_SPLINE_CURVE_WITH_KNOTS ( 'NONE', 3,
 ( #43297, #18656, #18910, #18394 ),
 .UNSPECIFIED., .F., .F.,
 ( 4, 4 ),
 ( 0.4993904256265703223, 1.000000000000000000 ),
 .UNSPECIFIED. ) ;
#31968 = CARTESIAN_POINT ( 'NONE',  ( 61.46917948669830167, 13.93954126835109975, -46.68479815709330438 ) ) ;
#31969 = CARTESIAN_POINT ( 'NONE',  ( 22.37218167695459670, 22.37718731335059985, -34.65000333313919612 ) ) ;
#31970 = FACE_OUTER_BOUND ( 'NONE', #18810, .T. ) ;
#31971 = ORIENTED_EDGE ( 'NONE', *, *, #1888, .T. ) ;
#31972 = CARTESIAN_POINT ( 'NONE',  ( 53.30581663188380048, -49.41149911629590008, -48.80307694725580347 ) ) ;
#31973 = CARTESIAN_POINT ( 'NONE',  ( 60.31615391617089728, -45.30095148067049848, -26.93200975326800162 ) ) ;
#31974 = CARTESIAN_POINT ( 'NONE',  ( 22.90077909847273219, -15.61618896438501203, -58.84717277627543552 ) ) ;
#31975 = CARTESIAN_POINT ( 'NONE',  ( 57.36674151108839936, 14.38237697927210057, -26.19522064574950093 ) ) ;
#31976 = CARTESIAN_POINT ( 'NONE',  ( 18.95302484735409720, -8.719853703674310452, -71.85617835341321324 ) ) ;
#31977 = CARTESIAN_POINT ( 'NONE',  ( 50.83757486290169680, 17.38380788181660108, -76.31330845207050118 ) ) ;
#31979 = EDGE_CURVE ( 'NONE', #28709, #26641, #33067, .T. ) ;
#31978 = CARTESIAN_POINT ( 'NONE',  ( 52.98906683290070418, 18.34770546868389829, -48.84983105046850227 ) ) ;
#31980 = CARTESIAN_POINT ( 'NONE',  ( 71.25019707560579718, 0.8838110553206759423, -70.77727272727280194 ) ) ;
#31981 = DIRECTION ( 'NONE',  ( 0.2946419978043516297, 0.8205364433225794674, 0.4898020399195900931 ) ) ;
#31982 = ORIENTED_EDGE ( 'NONE', *, *, #6927, .T. ) ;
#31983 = DIRECTION ( 'NONE',  ( -0.7071067811865441310, 0.000000000000000000, 0.7071067811865510144 ) ) ;
#31984 = CARTESIAN_POINT ( 'NONE',  ( 47.63102691442649927, -54.53857517529880283, -55.07721006389790119 ) ) ;
#31985 = FACE_BOUND ( 'NONE', #15541, .T. ) ;
#31986 = CARTESIAN_POINT ( 'NONE',  ( 12.72599073039820539, -21.52912574338567353, -71.11948792801658215 ) ) ;
#31987 = CARTESIAN_POINT ( 'NONE',  ( 62.21566394024790725, -30.80684386566390032, -16.45443897629299812 ) ) ;
#31988 = CARTESIAN_POINT ( 'NONE',  ( 71.52819866244169589, 1.000225705806889964, -60.71075825745960231 ) ) ;
#31989 = DIRECTION ( 'NONE',  ( -1.000000000000000000, 0.000000000000000000, 0.000000000000000000 ) ) ;
#31990 = CARTESIAN_POINT ( 'NONE',  ( 72.26623590265971586, 1.348264851907009731, -61.45091980464700043 ) ) ;
#31991 = CARTESIAN_POINT ( 'NONE',  ( 9.367366684597708826, -15.61630833865650025, -41.84717978380999170 ) ) ;
#31992 = CARTESIAN_POINT ( 'NONE',  ( 59.94131200797997394, -45.42892869204277417, -26.87338874175082992 ) ) ;
#31993 = EDGE_LOOP ( 'NONE', ( #34215, #33426, #50596, #12638, #10168 ) ) ;
#31994 = ORIENTED_EDGE ( 'NONE', *, *, #28600, .T. ) ;
#31995 = CARTESIAN_POINT ( 'NONE',  ( 71.33393739769809372, 11.38368607098449914, -61.45000000000081286 ) ) ;
#31996 = CARTESIAN_POINT ( 'NONE',  ( 12.72603599818342701, -21.52915135001642710, -59.11948678850429673 ) ) ;
#31997 = ORIENTED_EDGE ( 'NONE', *, *, #31979, .F. ) ;
#31998 = CARTESIAN_POINT ( 'NONE',  ( 18.20456379148673065, -7.911073824624160089, -59.09096439960827496 ) ) ;
#31999 = CARTESIAN_POINT ( 'NONE',  ( 12.96504724582215395, -9.608149964835362766, -49.79827915037039077 ) ) ;
#32000 = EDGE_LOOP ( 'NONE', ( #40150, #35771, #48654 ) ) ;
#32001 = AXIS2_PLACEMENT_3D ( 'NONE', #19905, #36657, #44276 ) ;
#32002 = CARTESIAN_POINT ( 'NONE',  ( 11.39201708760626630, 34.02281520799220971, -22.76707769548407256 ) ) ;
#32003 = CARTESIAN_POINT ( 'NONE',  ( 17.73647699123739940, 1.019008445897469972, -34.65800258959620095 ) ) ;
#32004 = CARTESIAN_POINT ( 'NONE',  ( 11.27234134993635983, -9.289961720576606297, -34.79933427684135694 ) ) ;
#32005 = CARTESIAN_POINT ( 'NONE',  ( 14.34289366216970052, -23.66447338258069877, -40.36203157117240181 ) ) ;
#32006 = CARTESIAN_POINT ( 'NONE',  ( 14.06326646941806935, -23.32129108267079687, -68.09100065600449625 ) ) ;
#32007 = CARTESIAN_POINT ( 'NONE',  ( 10.69832412674970001, 33.66039914567009816, -17.91220997198119846 ) ) ;
#32008 = CARTESIAN_POINT ( 'NONE',  ( 61.68013916707700162, -30.03519813877060329, -16.11687714886729950 ) ) ;
#32009 = CARTESIAN_POINT ( 'NONE',  ( 20.99565480752007574, -21.94232275358465856, -42.08399776718106722 ) ) ;
#32010 = CARTESIAN_POINT ( 'NONE',  ( 12.47311850084049922, -22.55771338299259909, -80.66697359201489803 ) ) ;
#32011 = CARTESIAN_POINT ( 'NONE',  ( 40.88927357473509971, 13.86719357938189923, -5.596100048965730878 ) ) ;
#32012 = EDGE_CURVE ( 'NONE', #14545, #4756, #42758, .T. ) ;
#32013 = AXIS2_PLACEMENT_3D ( 'NONE', #21590, #38122, #34159 ) ;
#32014 = CARTESIAN_POINT ( 'NONE',  ( 14.78004722010049932, 21.61970083732919790, -76.12726769927830617 ) ) ;
#32015 = EDGE_CURVE ( 'NONE', #51296, #42080, #6628, .T. ) ;
#32016 = CARTESIAN_POINT ( 'NONE',  ( 8.404314066867630828, -17.56895299481232797, -60.71374772562547406 ) ) ;
#32017 = CARTESIAN_POINT ( 'NONE',  ( 84.42999065749789622, -43.29956543148999515, -47.39892822416609874 ) ) ;
#32018 = PLANE ( 'NONE',  #25268 ) ;
#32019 = CARTESIAN_POINT ( 'NONE',  ( 22.35346372623429900, -10.20322183249439973, -39.27970379572579418 ) ) ;
#32020 = ORIENTED_EDGE ( 'NONE', *, *, #48464, .T. ) ;
#32021 = CARTESIAN_POINT ( 'NONE',  ( 53.43229558763829345, -49.00751707029830584, -27.03092591272499945 ) ) ;
#32022 = CARTESIAN_POINT ( 'NONE',  ( 13.86889551668869913, -50.63824991484180060, -21.27403962367300139 ) ) ;
#32023 = CARTESIAN_POINT ( 'NONE',  ( 22.01208305704984625, -20.93590873092134430, -39.74177713259125966 ) ) ;
#32024 = DIRECTION ( 'NONE',  ( 0.000000000000000000, -1.000000000000000000, 0.000000000000000000 ) ) ;
#32025 = CARTESIAN_POINT ( 'NONE',  ( 22.89142722538155184, -16.00359191757463151, -56.47104994342021911 ) ) ;
#32026 = CARTESIAN_POINT ( 'NONE',  ( 82.02429831058030629, 10.00628846694210061, -45.87976092105969883 ) ) ;
#32027 = CIRCLE ( 'NONE', #5323, 0.4999999999999986677 ) ;
#32028 = ORIENTED_EDGE ( 'NONE', *, *, #44738, .T. ) ;
#32029 = DIRECTION ( 'NONE',  ( 0.5516667872527449834, 0.8340645993220396903, 2.775557561562889194E-17 ) ) ;
#32030 = VECTOR ( 'NONE', #41321, 1000.000000000000000 ) ;
#32031 = CARTESIAN_POINT ( 'NONE',  ( 16.13393739769620083, -15.61618894467929941, -32.14999999999999858 ) ) ;
#32032 = CARTESIAN_POINT ( 'NONE',  ( 24.04462281140675728, -15.61619016268715399, -39.50767146438039390 ) ) ;
#32033 = CARTESIAN_POINT ( 'NONE',  ( 63.14388432454488509, 1.191644800533210091, -62.50206874317210293 ) ) ;
#32034 = CARTESIAN_POINT ( 'NONE',  ( 57.46993325851799739, -50.61178216551700615, -53.76538998729250096 ) ) ;
#32035 = CARTESIAN_POINT ( 'NONE',  ( 41.57868469450720283, 13.12802241111150003, -4.871763367457619509 ) ) ;
#32037 = EDGE_CURVE ( 'NONE', #25645, #4148, #14959, .T. ) ;
#32036 = CARTESIAN_POINT ( 'NONE',  ( 17.90525277672623616, -22.20704298856055203, -64.86948817688498536 ) ) ;
#32038 = CARTESIAN_POINT ( 'NONE',  ( 16.13393739769620083, -15.61618894467929941, -7.139181489322110608 ) ) ;
#32039 = CARTESIAN_POINT ( 'NONE',  ( 54.21899510283260071, -48.93305932984999629, -48.60061331225900005 ) ) ;
#32040 = CARTESIAN_POINT ( 'NONE',  ( 8.222913253182543514, -14.58081823353785289, -74.83400703225677830 ) ) ;
#32041 = CARTESIAN_POINT ( 'NONE',  ( 31.58225770014178835, -2.032350560840699760, -65.65000000000000568 ) ) ;
#32042 = CARTESIAN_POINT ( 'NONE',  ( 17.34547572264069970, -52.74444847917729362, -76.12391999848780699 ) ) ;
#32043 = ADVANCED_FACE ( 'NONE', ( #39585, #35121 ), #3690, .T. ) ;
#32044 = CARTESIAN_POINT ( 'NONE',  ( 9.807815828836600858, -10.75445489836692836, -77.00066418793667822 ) ) ;
#32045 = CARTESIAN_POINT ( 'NONE',  ( -18.86606260230360022, -50.61618894467959962, 14.21249999999999858 ) ) ;
#32046 = VERTEX_POINT ( 'NONE', #35652 ) ;
#32047 = CARTESIAN_POINT ( 'NONE',  ( 16.13393739769620083, -15.61618894467929941, -54.64999999999999858 ) ) ;
#32048 = DIRECTION ( 'NONE',  ( 1.224647048234162108E-16, 1.000000000000000000, -1.205421602240320019E-11 ) ) ;
#32049 = DIRECTION ( 'NONE',  ( -0.3487035033511758919, -0.9372330909387569520, 0.000000000000000000 ) ) ;
#32050 = CARTESIAN_POINT ( 'NONE',  ( 11.98399099476960039, -9.143003290065829347, -81.23899999999999011 ) ) ;
#32051 = ORIENTED_EDGE ( 'NONE', *, *, #41171, .T. ) ;
#32052 = CARTESIAN_POINT ( 'NONE',  ( 17.64668853360479872, 20.66382337739360153, -75.74020909530109691 ) ) ;
#32053 = VERTEX_POINT ( 'NONE', #51639 ) ;
#32054 = ORIENTED_EDGE ( 'NONE', *, *, #19462, .F. ) ;
#32055 = CIRCLE ( 'NONE', #35450, 6.999999999999999112 ) ;
#32056 = VERTEX_POINT ( 'NONE', #46956 ) ;
#32057 = CARTESIAN_POINT ( 'NONE',  ( 57.39016325515699180, -45.80620285074159881, -26.27722981911719913 ) ) ;
#32058 = CARTESIAN_POINT ( 'NONE',  ( 19.11635189901000231, -21.76136781846319934, -81.23899999999999011 ) ) ;
#32059 =( BOUNDED_CURVE ( )  B_SPLINE_CURVE ( 3, ( #14740, #18919, #30960, #31722 ),
 .UNSPECIFIED., .F., .T. ) 
 B_SPLINE_CURVE_WITH_KNOTS ( ( 4, 4 ),
 ( 1.570796326794896558, 2.356194490192338620 ),
 .UNSPECIFIED. ) 
 CURVE ( )  GEOMETRIC_REPRESENTATION_ITEM ( )  RATIONAL_B_SPLINE_CURVE ( ( 1.000000000000000000, 0.9492530216741918991, 0.9492530216741918991, 1.000000000000000000 ) ) 
 REPRESENTATION_ITEM ( '' )  );
#32060 = FACE_OUTER_BOUND ( 'NONE', #11711, .T. ) ;
#32061 = CARTESIAN_POINT ( 'NONE',  ( 75.47966807050509885, 12.14072485751589880, -13.40512917118210012 ) ) ;
#32062 = CARTESIAN_POINT ( 'NONE',  ( 12.26481002496320016, -65.46765766720608326, -22.60721059743012873 ) ) ;
#32063 = ORIENTED_EDGE ( 'NONE', *, *, #17043, .F. ) ;
#32064 = FACE_OUTER_BOUND ( 'NONE', #36594, .T. ) ;
#32065 = VECTOR ( 'NONE', #46596, 1000.000000000000000 ) ;
#32066 = CARTESIAN_POINT ( 'NONE',  ( 58.98993200268654391, -45.56937796336901414, -26.56610208028315867 ) ) ;
#32067 = ORIENTED_EDGE ( 'NONE', *, *, #43960, .F. ) ;
#32068 = TOROIDAL_SURFACE ( 'NONE', #50506, 34.55616290057869833, 2.000000000000000000 ) ;
#32069 = ORIENTED_EDGE ( 'NONE', *, *, #845, .T. ) ;
#32070 = DIRECTION ( 'NONE',  ( 2.020486089517491233E-31, -1.000000000000000000, 2.054487543405499690E-16 ) ) ;
#32072 = DIRECTION ( 'NONE',  ( 0.000000000000000000, 0.000000000000000000, -1.000000000000000000 ) ) ;
#32071 = CIRCLE ( 'NONE', #27896, 6.099999999999994316 ) ;
#32073 = CARTESIAN_POINT ( 'NONE',  ( 60.66741122180980028, 14.45296748104540008, -47.62419456964220643 ) ) ;
#32074 = CARTESIAN_POINT ( 'NONE',  ( 22.72397170760201845, -14.02689616002885309, -40.37749311795220564 ) ) ;
#32075 = EDGE_CURVE ( 'NONE', #46034, #32635, #51806, .T. ) ;
#32076 = CARTESIAN_POINT ( 'NONE',  ( -21.36606260230379917, 21.88381105532059934, 17.35000000000000142 ) ) ;
#32077 = CARTESIAN_POINT ( 'NONE',  ( -7.635283139872090175, 14.03913662587130062, -5.082544383023049228 ) ) ;
#32078 = CARTESIAN_POINT ( 'NONE',  ( 47.10256183579443245, 23.39255389708953459, -75.00952367219578321 ) ) ;
#32079 = CARTESIAN_POINT ( 'NONE',  ( 57.82240384458129512, 14.50996769876100068, -26.33560015361079820 ) ) ;
#32080 = CARTESIAN_POINT ( 'NONE',  ( 13.10477641622549960, -22.85572842806620031, -57.91364648621609490 ) ) ;
#32081 = EDGE_LOOP ( 'NONE', ( #13772, #42996, #27126, #4343 ) ) ;
#32082 = CARTESIAN_POINT ( 'NONE',  ( 55.16626882053050451, 17.34692063200439804, -48.76159087390789892 ) ) ;
#32083 = AXIS2_PLACEMENT_3D ( 'NONE', #3424, #19395, #35376 ) ;
#32084 = CARTESIAN_POINT ( 'NONE',  ( 40.76017233408010298, 14.12870932884110076, -5.740519046195230679 ) ) ;
#32085 = CARTESIAN_POINT ( 'NONE',  ( 11.57631367792649968, 33.55102097998219790, -44.87215126223550499 ) ) ;
#32086 = CARTESIAN_POINT ( 'NONE',  ( 72.55472656186499592, 1.019773975906300034, -69.70721229073478753 ) ) ;
#32087 = CARTESIAN_POINT ( 'NONE',  ( 43.64633900757768714, -39.92480820678616027, -68.37225813791066287 ) ) ;
#32088 =( NAMED_UNIT ( * ) PLANE_ANGLE_UNIT ( ) SI_UNIT ( $, .RADIAN. ) );
#32089 = CARTESIAN_POINT ( 'NONE',  ( 46.84224516425109641, 22.80152155003670345, -75.76637104849140769 ) ) ;
#32090 = CARTESIAN_POINT ( 'NONE',  ( 48.87228429941779950, -54.00865885737479744, -55.18590764587609954 ) ) ;
#32091 = CARTESIAN_POINT ( 'NONE',  ( -7.625877374285919608, 14.22289747138790084, -5.682500641286110543 ) ) ;
#32092 = CARTESIAN_POINT ( 'NONE',  ( -18.86606260230390220, 19.38381105532060289, 10.84999999999999964 ) ) ;
#32093 = PLANE ( 'NONE',  #22097 ) ;
#32094 = EDGE_CURVE ( 'NONE', #11209, #4421, #6994, .T. ) ;
#32095 = CARTESIAN_POINT ( 'NONE',  ( 15.09844560108056477, -23.52719567249974020, -54.33399961690664526 ) ) ;
#32096 = VERTEX_POINT ( 'NONE', #19910 ) ;
#32097 = CARTESIAN_POINT ( 'NONE',  ( 10.09604082153919968, -19.98116939500580358, -31.86811205682530002 ) ) ;
#32098 = CARTESIAN_POINT ( 'NONE',  ( 64.80088823274370213, 1.308647200627810259, -60.89791552425909771 ) ) ;
#32099 = VERTEX_POINT ( 'NONE', #21191 ) ;
#32100 = DIRECTION ( 'NONE',  ( 0.000000000000000000, 0.000000000000000000, -1.000000000000000000 ) ) ;
#32101 = CARTESIAN_POINT ( 'NONE',  ( 60.45022673394080215, -45.68032972807930037, -47.34936493783050793 ) ) ;
#32102 = DIRECTION ( 'NONE',  ( 0.000000000000000000, 0.000000000000000000, -1.000000000000000000 ) ) ;
#32103 = DIRECTION ( 'NONE',  ( 0.000000000000000000, -1.000000000000000000, 0.000000000000000000 ) ) ;
#32105 = DIRECTION ( 'NONE',  ( 0.3918900564939547526, 0.9200120562368543364, 0.000000000000000000 ) ) ;
#32104 = CARTESIAN_POINT ( 'NONE',  ( 41.85500005128616152, 8.516429740364495515, -77.03127993483552416 ) ) ;
#32106 = CARTESIAN_POINT ( 'NONE',  ( 58.91398403652545568, 14.34820724552367288, -26.53092679127404452 ) ) ;
#32107 = LINE ( 'NONE', #45234, #6909 ) ;
#32108 = ORIENTED_EDGE ( 'NONE', *, *, #35472, .F. ) ;
#32109 = CARTESIAN_POINT ( 'NONE',  ( 83.07525583555450055, -45.50440358686140030, -47.60489434516649965 ) ) ;
#32110 = ORIENTED_EDGE ( 'NONE', *, *, #16127, .F. ) ;
#32111 = ORIENTED_EDGE ( 'NONE', *, *, #23765, .F. ) ;
#32112 = ORIENTED_EDGE ( 'NONE', *, *, #32482, .T. ) ;
#32113 = DIRECTION ( 'NONE',  ( -0.9990957361526744407, 0.000000000000000000, -0.04251717301921301845 ) ) ;
#32114 = CARTESIAN_POINT ( 'NONE',  ( 53.23907584153930372, -49.52980310945599740, -49.17816088826820220 ) ) ;
#32115 = CARTESIAN_POINT ( 'NONE',  ( 23.13393739769620083, -28.89524513604070322, -39.64999999999999858 ) ) ;
#32116 = CARTESIAN_POINT ( 'NONE',  ( 76.39589878011133806, -18.67680352252259013, -12.77887956925968993 ) ) ;
#32117 = CARTESIAN_POINT ( 'NONE',  ( 53.02870100497279537, -51.95943102007580450, -53.35088539576909739 ) ) ;
#32118 = ORIENTED_EDGE ( 'NONE', *, *, #39349, .F. ) ;
#32119 = EDGE_LOOP ( 'NONE', ( #40736, #23677, #45295, #41382 ) ) ;
#32120 = CARTESIAN_POINT ( 'NONE',  ( -0.1695375756935748601, 14.25975516931139708, -34.91378044826135607 ) ) ;
#32121 = CARTESIAN_POINT ( 'NONE',  ( -20.18262829310297590, -1.399661344290894061, -52.57430347528295300 ) ) ;
#32122 = CARTESIAN_POINT ( 'NONE',  ( 56.44840739252509820, -50.75241255283049924, -53.50789655320240001 ) ) ;
#32123 = AXIS2_PLACEMENT_3D ( 'NONE', #38886, #14508, #6396 ) ;
#32124 = CARTESIAN_POINT ( 'NONE',  ( 16.13393739769620083, -15.61618894467929941, -8.050000000000000711 ) ) ;
#32125 = CARTESIAN_POINT ( 'NONE',  ( 51.13393739769659874, -45.11618894467899565, 14.21249999999999858 ) ) ;
#32126 = CARTESIAN_POINT ( 'NONE',  ( 16.13393739769620083, -15.61618894467929941, -32.14999999999999858 ) ) ;
#32127 = VERTEX_POINT ( 'NONE', #37199 ) ;
#32128 = CARTESIAN_POINT ( 'NONE',  ( 63.15096886846589541, 0.8925687589132609290, -68.99219224778180148 ) ) ;
#32129 = CARTESIAN_POINT ( 'NONE',  ( 52.84793105771459665, -50.35222278663569284, -76.98160984018271336 ) ) ;
#32130 = DIRECTION ( 'NONE',  ( -0.6934629132905126836, -0.5038302981000498670, 0.5150380749100492705 ) ) ;
#32131 = CARTESIAN_POINT ( 'NONE',  ( 4.133937397696232807, -12.40079863550581862, -22.14999999999998792 ) ) ;
#32132 = CARTESIAN_POINT ( 'NONE',  ( 20.35952799517920297, -9.003237130697479884, -57.69348358356519668 ) ) ;
#32133 = CARTESIAN_POINT ( 'NONE',  ( 12.69305026481350041, -50.32355431075080077, -21.19712586183110048 ) ) ;
#32134 = ADVANCED_FACE ( 'NONE', ( #25118 ), #24857, .F. ) ;
#32135 = TOROIDAL_SURFACE ( 'NONE', #27959, 34.55616290057869833, 2.000000000000000000 ) ;
#32136 = CARTESIAN_POINT ( 'NONE',  ( 18.68046040379451611, -51.42830650673013082, -15.73013301310943035 ) ) ;
#32137 = CARTESIAN_POINT ( 'NONE',  ( 55.55363803660430477, 13.88381105532070059, -14.32024155674050014 ) ) ;
#32139 = ADVANCED_FACE ( 'NONE', ( #17288 ), #44279, .F. ) ;
#32138 = CARTESIAN_POINT ( 'NONE',  ( 61.12445724983340511, -45.77187651496940646, -47.85281658922149717 ) ) ;
#32140 = EDGE_CURVE ( 'NONE', #5719, #21125, #50988, .T. ) ;
#32141 = CARTESIAN_POINT ( 'NONE',  ( 11.97535763329322300, -21.02757826297640875, -39.16115446231404462 ) ) ;
#32142 = CARTESIAN_POINT ( 'NONE',  ( 11.96950732185199939, -9.924082013335240759, -54.14612557624219846 ) ) ;
#32143 = CARTESIAN_POINT ( 'NONE',  ( 17.52097594613490728, -52.86909450412152722, -76.12392058102736314 ) ) ;
#32144 = ADVANCED_FACE ( 'NONE', ( #13114 ), #48476, .T. ) ;
#32145 = EDGE_LOOP ( 'NONE', ( #27120, #37898, #34719, #33918 ) ) ;
#32146 = DIRECTION ( 'NONE',  ( 0.000000000000000000, 0.000000000000000000, 1.000000000000000000 ) ) ;
#32147 = CARTESIAN_POINT ( 'NONE',  ( 47.34065738921189848, -54.69081672572639974, -54.67801390606140188 ) ) ;
#32148 = FILL_AREA_STYLE ('',( #31897 ) ) ;
#32149 = CARTESIAN_POINT ( 'NONE',  ( 11.97528171298242761, -10.20485706339848697, -37.74448779564736611 ) ) ;
#32150 = FACE_OUTER_BOUND ( 'NONE', #51266, .T. ) ;
#32151 = CARTESIAN_POINT ( 'NONE',  ( 60.83133137330749918, -45.46867109277970087, -47.01992810568810199 ) ) ;
#32152 = EDGE_CURVE ( 'NONE', #22659, #23707, #4446, .T. ) ;
#32153 = CARTESIAN_POINT ( 'NONE',  ( 12.72585555203040641, -9.703328613768398725, -75.78613368438831799 ) ) ;
#32154 = CARTESIAN_POINT ( 'NONE',  ( 10.72852875961880059, 33.70931783810110005, -18.17421237878960127 ) ) ;
#32155 = CIRCLE ( 'NONE', #39753, 40.00000000000000711 ) ;
#32157 = CARTESIAN_POINT ( 'NONE',  ( 8.222944410885272504, -16.65178775934220212, -52.75066473391525790 ) ) ;
#32156 = CARTESIAN_POINT ( 'NONE',  ( 47.38034238265840514, 22.97049270074940708, -75.36289877198294107 ) ) ;
#32158 = CARTESIAN_POINT ( 'NONE',  ( 10.61752692138360032, -64.82564047392860118, -18.17418372802830007 ) ) ;
#32159 = EDGE_CURVE ( 'NONE', #27673, #34513, #33248, .T. ) ;
#32160 = CARTESIAN_POINT ( 'NONE',  ( 48.59256985241970028, 22.83699819754599858, -54.83953650029820182 ) ) ;
#32161 = ORIENTED_EDGE ( 'NONE', *, *, #20482, .T. ) ;
#32162 = CARTESIAN_POINT ( 'NONE',  ( 53.11153479641689756, -49.53865774820230428, -49.01452490533140605 ) ) ;
#32163 = ORIENTED_EDGE ( 'NONE', *, *, #16093, .T. ) ;
#32164 = CARTESIAN_POINT ( 'NONE',  ( 64.90705159044762240, -17.44293478064540892, -18.18360580342293531 ) ) ;
#32165 = CARTESIAN_POINT ( 'NONE',  ( 14.18536260820837214, -41.66761415519157197, -34.89146800830128825 ) ) ;
#32166 = DIRECTION ( 'NONE',  ( -1.000000000000000000, 0.000000000000000000, 0.000000000000000000 ) ) ;
#32167 = CARTESIAN_POINT ( 'NONE',  ( 84.44784216359251161, 11.88381105532070059, -47.47585302082339354 ) ) ;
#32168 = CARTESIAN_POINT ( 'NONE',  ( 9.639954762936479682, -12.86468967408800168, -65.58038890884739658 ) ) ;
#32169 = CARTESIAN_POINT ( 'NONE',  ( 52.61151938036640274, 18.58685067986549910, -48.60683035550010089 ) ) ;
#32170 = CARTESIAN_POINT ( 'NONE',  ( 55.46022005097690055, -45.45871768700150284, -15.74543532541669855 ) ) ;
#32171 = CARTESIAN_POINT ( 'NONE',  ( 68.13393739769618662, -2.032350560841069687, -102.2016796975542690 ) ) ;
#32172 = ORIENTED_EDGE ( 'NONE', *, *, #21396, .T. ) ;
#32173 = AXIS2_PLACEMENT_3D ( 'NONE', #39482, #19548, #36556 ) ;
#32174 = CARTESIAN_POINT ( 'NONE',  ( 13.15543360202459944, -22.87671670251840084, -41.91142241136510194 ) ) ;
#32175 = ORIENTED_EDGE ( 'NONE', *, *, #6889, .F. ) ;
#32176 = CARTESIAN_POINT ( 'NONE',  ( 11.86319498458860089, -65.39781150395960196, -17.45437997871620084 ) ) ;
#32177 = CARTESIAN_POINT ( 'NONE',  ( 10.30800062017689989, 32.11819526227149879, -45.84700176684360429 ) ) ;
#32178 = CARTESIAN_POINT ( 'NONE',  ( 18.52830607121394380, 20.08717197157803369, -15.71177323601433429 ) ) ;
#32179 = CARTESIAN_POINT ( 'NONE',  ( 47.68700795962210037, -54.63828844795879291, -55.28492161652850001 ) ) ;
#32180 = CARTESIAN_POINT ( 'NONE',  ( 8.802044555037090490, 31.97380483823370056, -46.67015369154350424 ) ) ;
#32181 = FACE_OUTER_BOUND ( 'NONE', #15470, .T. ) ;
#32182 = ADVANCED_FACE ( 'NONE', ( #17031 ), #19314, .T. ) ;
#32183 = VERTEX_POINT ( 'NONE', #41067 ) ;
#32184 = CARTESIAN_POINT ( 'NONE',  ( 10.47385200046668707, 23.98129158042145548, -45.62050397739949403 ) ) ;
#32185 = CARTESIAN_POINT ( 'NONE',  ( 11.10561945692110086, -63.36846315954289111, -44.25483350269709604 ) ) ;
#32186 = DIRECTION ( 'NONE',  ( -1.000000000000000000, 0.000000000000000000, 0.000000000000000000 ) ) ;
#32187 = ORIENTED_EDGE ( 'NONE', *, *, #40329, .F. ) ;
#32188 = DIRECTION ( 'NONE',  ( -0.5516667872527389882, -0.8340645993220436871, 8.326672684688667890E-17 ) ) ;
#32189 = CARTESIAN_POINT ( 'NONE',  ( 50.55910954965799675, -50.23966005774419585, -76.14999999999999147 ) ) ;
#32190 = CARTESIAN_POINT ( 'NONE',  ( 22.90085274204890808, -15.61618877333890332, -76.84718755697707593 ) ) ;
#32191 = EDGE_LOOP ( 'NONE', ( #47956, #50509, #45543, #36794 ) ) ;
#32192 = CARTESIAN_POINT ( 'NONE',  ( 14.06324711021505180, -23.32128607067484083, -36.09100056568438930 ) ) ;
#32193 = CARTESIAN_POINT ( 'NONE',  ( 18.11900864776890074, -32.59522544870679894, -35.02873218748179340 ) ) ;
#32194 = CARTESIAN_POINT ( 'NONE',  ( 22.90066830340121840, -15.61618925674170022, -38.84718272210749035 ) ) ;
#32195 = CARTESIAN_POINT ( 'NONE',  ( 56.50924534995709791, 14.67579805743599941, -45.01296638903539815 ) ) ;
#32196 = CARTESIAN_POINT ( 'NONE',  ( 9.582977133340488507, -20.62294834280969980, -74.58460979065590379 ) ) ;
#32197 = VECTOR ( 'NONE', #16971, 1000.000000000000000 ) ;
#32198 = CARTESIAN_POINT ( 'NONE',  ( 83.89200044194980421, 19.24776070067099099, -53.20292136905285929 ) ) ;
#32199 = CARTESIAN_POINT ( 'NONE',  ( 55.41789900912189637, 19.74853478895110115, -75.07114006131348560 ) ) ;
#32200 = VERTEX_POINT ( 'NONE', #51828 ) ;
#32201 = ADVANCED_FACE ( 'NONE', ( #16177 ), #7101, .T. ) ;
#32202 = CARTESIAN_POINT ( 'NONE',  ( 14.88739902878229948, -22.96144836147129809, -66.78616676534149121 ) ) ;
#32203 = CARTESIAN_POINT ( 'NONE',  ( 53.16292395753290378, -49.55788399721789972, -49.15366685756480081 ) ) ;
#32204 = CARTESIAN_POINT ( 'NONE',  ( 16.13393739769620083, -15.61618894467929941, -18.10000000000000142 ) ) ;
#32205 = CARTESIAN_POINT ( 'NONE',  ( 12.29949449227315661, 34.10758153282596794, -23.61819227765068163 ) ) ;
#32206 = EDGE_CURVE ( 'NONE', #39152, #35815, #47903, .T. ) ;
#32207 = CARTESIAN_POINT ( 'NONE',  ( 47.19475760687539889, 23.42706180971210017, -74.80880246430230329 ) ) ;
#32208 = CIRCLE ( 'NONE', #38120, 1.999999999999998224 ) ;
#32209 = CARTESIAN_POINT ( 'NONE',  ( 71.13601697155240799, 1.385888765344509999, -60.99577487439199786 ) ) ;
#32210 = DIRECTION ( 'NONE',  ( -1.000000000000000000, 0.000000000000000000, 0.000000000000000000 ) ) ;
#32211 = DIRECTION ( 'NONE',  ( -1.000000000000000000, 0.000000000000000000, 0.000000000000000000 ) ) ;
#32212 = CARTESIAN_POINT ( 'NONE',  ( 8.244279884465401054, -18.01118895116649909, -78.41385574115369650 ) ) ;
#32213 = CARTESIAN_POINT ( 'NONE',  ( 55.02244667203229511, -50.61618557942939844, -76.57012733959869877 ) ) ;
#32215 = CARTESIAN_POINT ( 'NONE',  ( 40.78962545348711188, -39.66124797165849714, -82.01204344300963101 ) ) ;
#32214 = DIRECTION ( 'NONE',  ( 0.000000000000000000, -1.000000000000000000, 0.000000000000000000 ) ) ;
#32216 = CARTESIAN_POINT ( 'NONE',  ( 63.05799534064709633, 1.101170701158060039, -68.76387392617688477 ) ) ;
#32217 = CARTESIAN_POINT ( 'NONE',  ( 61.43987658220769532, 13.93615501258799938, -46.53628776920029964 ) ) ;
#32218 = EDGE_CURVE ( 'NONE', #2647, #4309, #36337, .T. ) ;
#32219 = CYLINDRICAL_SURFACE ( 'NONE', #12199, 50.00000000000000000 ) ;
#32220 = ORIENTED_EDGE ( 'NONE', *, *, #20093, .T. ) ;
#32221 = CARTESIAN_POINT ( 'NONE',  ( 53.00383630090699683, -49.56971507260659848, -48.79311475622040462 ) ) ;
#32222 = CARTESIAN_POINT ( 'NONE',  ( 61.30973436904390184, -45.21801592863619845, -28.15097513424300146 ) ) ;
#32223 = TOROIDAL_SURFACE ( 'NONE', #14717, 2.500000000000000000, 0.5000000000000000000 ) ;
#32224 = CARTESIAN_POINT ( 'NONE',  ( -6.774824244623153469, -32.26037854176222197, 6.072546842075589701 ) ) ;
#32225 = CARTESIAN_POINT ( 'NONE',  ( 56.52597820759500280, 14.74085777827989929, -26.17543599240089947 ) ) ;
#32226 = CARTESIAN_POINT ( 'NONE',  ( 8.863596654104609840, -13.98866346440020081, -79.30275787339340354 ) ) ;
#32227 = CARTESIAN_POINT ( 'NONE',  ( 50.32395455581429644, 18.50520907444330021, -76.14999999999999147 ) ) ;
#32228 = CARTESIAN_POINT ( 'NONE',  ( 52.77840648010259628, 18.46069720204630116, -48.67385165654339829 ) ) ;
#32229 = CARTESIAN_POINT ( 'NONE',  ( 71.33861941035669929, 1.097085799869280009, -70.67221403600389351 ) ) ;
#32230 = CARTESIAN_POINT ( 'NONE',  ( 42.78018059632900361, -42.70905810753740184, -3.187564294433600232 ) ) ;
#32231 = CIRCLE ( 'NONE', #51505, 10.00000000000000711 ) ;
#32232 = ORIENTED_EDGE ( 'NONE', *, *, #33759, .T. ) ;
#32233 = CARTESIAN_POINT ( 'NONE',  ( 62.63393739769619373, -63.11618894467939356, 11.84999999999999964 ) ) ;
#32234 = CARTESIAN_POINT ( 'NONE',  ( 47.50536557026320139, -54.59832931019789726, -54.95512628287880119 ) ) ;
#32235 = FACE_BOUND ( 'NONE', #40344, .T. ) ;
#32236 = CARTESIAN_POINT ( 'NONE',  ( 22.52288591994712164, -13.38583005777697466, -80.34591106198659816 ) ) ;
#32237 = CARTESIAN_POINT ( 'NONE',  ( 61.25350246668320153, 14.35920381295040116, -47.66861028105059717 ) ) ;
#32238 = CARTESIAN_POINT ( 'NONE',  ( 71.45588032111159293, 0.8910129994591549085, -60.65352295474710331 ) ) ;
#32239 = DIRECTION ( 'NONE',  ( 0.000000000000000000, -1.000000000000000000, 0.000000000000000000 ) ) ;
#32240 = CARTESIAN_POINT ( 'NONE',  ( 71.40255948545589604, 1.402336724396250123, -61.08651255177160522 ) ) ;
#32241 = EDGE_CURVE ( 'NONE', #24197, #8577, #18779, .T. ) ;
#32242 = CARTESIAN_POINT ( 'NONE',  ( 23.79191518862026555, -17.66738158803666536, -71.59098575566194711 ) ) ;
#32243 = AXIS2_PLACEMENT_3D ( 'NONE', #12987, #44678, #9043 ) ;
#32244 = CARTESIAN_POINT ( 'NONE',  ( 65.16374186055298878, 1.338092079250050137, -70.53694914618849054 ) ) ;
#32245 = EDGE_LOOP ( 'NONE', ( #42247, #25281, #41026, #1924 ) ) ;
#32246 = ADVANCED_FACE ( 'NONE', ( #24529 ), #44217, .T. ) ;
#32247 = ORIENTED_EDGE ( 'NONE', *, *, #34873, .T. ) ;
#32248 = CARTESIAN_POINT ( 'NONE',  ( 14.29753604904800035, -51.11618894467939356, -22.54695280101919863 ) ) ;
#32249 = CARTESIAN_POINT ( 'NONE',  ( 0.08551642312349798380, -45.86262496382770593, -34.70586877331279396 ) ) ;
#32250 = ORIENTED_EDGE ( 'NONE', *, *, #38749, .F. ) ;
#32251 = CARTESIAN_POINT ( 'NONE',  ( 12.71291094188550019, -65.48164260791450886, -47.17969016435449703 ) ) ;
#32252 = CARTESIAN_POINT ( 'NONE',  ( 16.13393739769620083, -15.61618894467929941, 4.349999999999999645 ) ) ;
#32253 = ORIENTED_EDGE ( 'NONE', *, *, #6666, .F. ) ;
#32254 = DIRECTION ( 'NONE',  ( 0.000000000000000000, 0.000000000000000000, 1.000000000000000000 ) ) ;
#32255 = CARTESIAN_POINT ( 'NONE',  ( 41.98072431426170681, 6.388270017410889068, -80.41599570558052790 ) ) ;
#32256 = CARTESIAN_POINT ( 'NONE',  ( 18.20468374244083520, -7.911107725230738907, -35.09100006191968646 ) ) ;
#32257 = CARTESIAN_POINT ( 'NONE',  ( 7.897539103648019143, -15.99627209049759813, -38.77765294989999489 ) ) ;
#32258 = CARTESIAN_POINT ( 'NONE',  ( 8.223600577592289795, -15.61621812327629932, -68.50766849176299900 ) ) ;
#32259 = CARTESIAN_POINT ( 'NONE',  ( 42.98612411504951325, -37.77564690010735404, -75.38906579693129117 ) ) ;
#32260 =( LENGTH_UNIT ( ) NAMED_UNIT ( * ) SI_UNIT ( .MILLI., .METRE. ) );
#32261 = ORIENTED_EDGE ( 'NONE', *, *, #12918, .F. ) ;
#32262 = ADVANCED_FACE ( 'NONE', ( #26346 ), #11377, .T. ) ;
#32263 = CARTESIAN_POINT ( 'NONE',  ( 9.807855002554534352, -20.47797325407011115, -42.58399805498525126 ) ) ;
#32264 = CARTESIAN_POINT ( 'NONE',  ( 22.77098726966259790, -19.80382795992320055, -80.19166000563299690 ) ) ;
#32265 = AXIS2_PLACEMENT_3D ( 'NONE', #41795, #5651, #41277 ) ;
#32266 = CARTESIAN_POINT ( 'NONE',  ( 43.99501267352869860, 14.58011966584659902, -8.084181983217140655 ) ) ;
#32267 = EDGE_CURVE ( 'NONE', #37443, #34841, #48893, .T. ) ;
#32268 = AXIS2_PLACEMENT_3D ( 'NONE', #30105, #42447, #2607 ) ;
#32269 = CARTESIAN_POINT ( 'NONE',  ( 14.64464131216699805, 20.99223335001410007, -75.94942944171690158 ) ) ;
#32270 = CARTESIAN_POINT ( 'NONE',  ( 19.81837380836439166, -22.69532670800266416, -60.13927688927024207 ) ) ;
#32271 = CARTESIAN_POINT ( 'NONE',  ( 82.78852321480370335, -45.02051732207199564, -46.36931865296660504 ) ) ;
#32272 = DIRECTION ( 'NONE',  ( 0.000000000000000000, 0.000000000000000000, -1.000000000000000000 ) ) ;
#32273 = CARTESIAN_POINT ( 'NONE',  ( 23.89559567647939886, -18.39816332852450032, -45.61721828081520158 ) ) ;
#32274 = ORIENTED_EDGE ( 'NONE', *, *, #46040, .T. ) ;
#32275 = CARTESIAN_POINT ( 'NONE',  ( 52.77900411135830439, -49.68605478194980662, -28.02809848489370026 ) ) ;
#32276 = CARTESIAN_POINT ( 'NONE',  ( 15.00521638035020189, -50.63531778240700021, -20.65446309923529711 ) ) ;
#32277 = CARTESIAN_POINT ( 'NONE',  ( 15.25515948764014595, -23.51599653976285609, -40.04283046677572599 ) ) ;
#32278 = LINE ( 'NONE', #28619, #10680 ) ;
#32279 = CARTESIAN_POINT ( 'NONE',  ( 74.28246655494581319, 0.9838110553206419473, -70.11716791742273358 ) ) ;
#32280 = DIRECTION ( 'NONE',  ( 1.147431558122957675E-27, 2.220771714818679968E-11, -1.000000000000000000 ) ) ;
#32281 = ORIENTED_EDGE ( 'NONE', *, *, #39129, .F. ) ;
#32282 = FACE_OUTER_BOUND ( 'NONE', #35299, .T. ) ;
#32283 = CARTESIAN_POINT ( 'NONE',  ( 47.40969209871759915, 23.41413369233859854, -54.72755864828499739 ) ) ;
#32284 = VECTOR ( 'NONE', #39500, 1000.000000000000000 ) ;
#32285 = CARTESIAN_POINT ( 'NONE',  ( 11.97539703212459550, -21.02760807041932267, -49.16115413242771837 ) ) ;
#32286 = CARTESIAN_POINT ( 'NONE',  ( 63.13228119804391270, 0.8904513541338849869, -62.33586013860640662 ) ) ;
#32287 = DIRECTION ( 'NONE',  ( 0.000000000000000000, 1.000000000000000000, 0.000000000000000000 ) ) ;
#32288 = CARTESIAN_POINT ( 'NONE',  ( 42.42176422072400044, 12.97522254370229966, -5.045468646584310157 ) ) ;
#32289 = CARTESIAN_POINT ( 'NONE',  ( 57.50723795381379944, -45.11618894467940066, -25.33268388717609909 ) ) ;
#32290 = CARTESIAN_POINT ( 'NONE',  ( 24.04493739769619864, -15.61618894467929941, -32.14999999999999858 ) ) ;
#32291 = DIRECTION ( 'NONE',  ( 0.000000000000000000, 1.000000000000000000, 0.000000000000000000 ) ) ;
#32292 = CARTESIAN_POINT ( 'NONE',  ( 57.50472949952089863, -47.23595428949509767, -47.96958150051639791 ) ) ;
#32293 = AXIS2_PLACEMENT_3D ( 'NONE', #18207, #46270, #50190 ) ;
#32294 = CARTESIAN_POINT ( 'NONE',  ( 67.04038824939736685, -50.70395984888064334, -74.34354914830332461 ) ) ;
#32295 = CARTESIAN_POINT ( 'NONE',  ( 64.65764093855679562, 1.007912009470880221, -60.76768544528139415 ) ) ;
#32296 = FACE_OUTER_BOUND ( 'NONE', #20327, .T. ) ;
#32297 = CARTESIAN_POINT ( 'NONE',  ( 8.223124147305879816, -15.61599092713959891, -72.50766849176299900 ) ) ;
#32298 = CARTESIAN_POINT ( 'NONE',  ( 58.73736653739000246, -47.92991618810659560, -50.00877492792809420 ) ) ;
#32299 = ORIENTED_EDGE ( 'NONE', *, *, #39411, .T. ) ;
#32300 = CARTESIAN_POINT ( 'NONE',  ( 14.28038400710293487, -41.76263555408612405, -34.79644660940672907 ) ) ;
#32301 = CARTESIAN_POINT ( 'NONE',  ( 9.726666662871059188, 31.88305279702909800, -46.30264950036470140 ) ) ;
#32302 = CARTESIAN_POINT ( 'NONE',  ( 22.90087708341497574, -15.64706466928298845, -34.45427045631887353 ) ) ;
#32303 = AXIS2_PLACEMENT_3D ( 'NONE', #50183, #33204, #45019 ) ;
#32304 = CARTESIAN_POINT ( 'NONE',  ( 9.510021278886100049, -12.32986133896500114, -81.23899999999999011 ) ) ;
#32305 = VERTEX_POINT ( 'NONE', #5308 ) ;
#32306 = CARTESIAN_POINT ( 'NONE',  ( 18.11374027727429947, 20.61624280354930150, -75.59143512441710300 ) ) ;
#32307 = AXIS2_PLACEMENT_3D ( 'NONE', #29305, #17274, #7927 ) ;
#32308 = EDGE_LOOP ( 'NONE', ( #26722, #29748, #50889, #28929 ) ) ;
#32309 = EDGE_CURVE ( 'NONE', #29219, #17717, #28623, .T. ) ;
#32310 = ORIENTED_EDGE ( 'NONE', *, *, #2011, .T. ) ;
#32311 = EDGE_LOOP ( 'NONE', ( #28562, #25538, #48331, #36925 ) ) ;
#32312 = FACE_OUTER_BOUND ( 'NONE', #38149, .T. ) ;
#32313 = CARTESIAN_POINT ( 'NONE',  ( -8.719958794165998839, 10.48190171173589924, -1.467676683391609949 ) ) ;
#32314 = EDGE_CURVE ( 'NONE', #5472, #44209, #43794, .T. ) ;
#32315 = CARTESIAN_POINT ( 'NONE',  ( 16.13393739769620083, -15.61618894467929941, -35.14999999999999858 ) ) ;
#32316 = EDGE_LOOP ( 'NONE', ( #26392, #42954, #36636, #19323 ) ) ;
#32317 = LINE ( 'NONE', #24971, #41051 ) ;
#32318 = CARTESIAN_POINT ( 'NONE',  ( 4.133937397696209715, -8.687985714403829718, -47.64999999999999858 ) ) ;
#32319 = EDGE_LOOP ( 'NONE', ( #44785, #30514, #32299, #12143, #38680, #41562 ) ) ;
#32320 = FACE_OUTER_BOUND ( 'NONE', #17201, .T. ) ;
#32321 = VECTOR ( 'NONE', #38381, 1000.000000000000000 ) ;
#32322 = CARTESIAN_POINT ( 'NONE',  ( 14.13393739769619906, -45.61618894467940066, -35.14999999999999858 ) ) ;
#32323 = ORIENTED_EDGE ( 'NONE', *, *, #31953, .F. ) ;
#32324 = ORIENTED_EDGE ( 'NONE', *, *, #18444, .T. ) ;
#32325 = CARTESIAN_POINT ( 'NONE',  ( 61.75019796695539753, -45.11618894467940066, -46.37203261889099792 ) ) ;
#32326 = CARTESIAN_POINT ( 'NONE',  ( 11.88236613209306825, -65.43512710276252164, -17.91369326119161087 ) ) ;
#32327 = CARTESIAN_POINT ( 'NONE',  ( 60.74922417162630239, 14.42261168151119932, -47.61677699820549492 ) ) ;
#32328 = VECTOR ( 'NONE', #7571, 1000.000000000000114 ) ;
#32329 = EDGE_CURVE ( 'NONE', #6692, #42086, #13185, .T. ) ;
#32330 = CARTESIAN_POINT ( 'NONE',  ( 52.07929282054270459, 14.36745883135820101, -13.46056141404780071 ) ) ;
#32331 = DIRECTION ( 'NONE',  ( -0.8696770943981948498, -0.4936210606113898836, 1.887379141852609535E-15 ) ) ;
#32332 = CARTESIAN_POINT ( 'NONE',  ( -2.623662902638759675, 17.43154064381609913, -4.386168478789810088 ) ) ;
#32333 = CARTESIAN_POINT ( 'NONE',  ( 9.367861075313296482, -16.44284879759471352, -55.80828792171165276 ) ) ;
#32334 = AXIS2_PLACEMENT_3D ( 'NONE', #15449, #23275, #31402 ) ;
#32335 = CARTESIAN_POINT ( 'NONE',  ( 60.16078383215049996, 14.16442556805120034, -26.96501188446990227 ) ) ;
#32336 = CARTESIAN_POINT ( 'NONE',  ( 19.85177579122500191, -8.705007724165220395, -66.94460462746880580 ) ) ;
#32337 = ORIENTED_EDGE ( 'NONE', *, *, #10007, .F. ) ;
#32338 = AXIS2_PLACEMENT_3D ( 'NONE', #29397, #14453, #6339 ) ;
#32339 = CARTESIAN_POINT ( 'NONE',  ( 59.66729930240479263, 14.84616221926219914, -47.40987971772899812 ) ) ;
#32340 = CARTESIAN_POINT ( 'NONE',  ( 15.69653675527930226, -8.576924789068980814, -76.32742627405558267 ) ) ;
#32341 = CARTESIAN_POINT ( 'NONE',  ( 11.96163130544649889, 33.91328095727600811, -45.68067242497239278 ) ) ;
#32342 = CARTESIAN_POINT ( 'NONE',  ( 72.14060588395169304, 1.458412159422780130, -69.79309345819311261 ) ) ;
#32343 = CARTESIAN_POINT ( 'NONE',  ( 43.85372935305733932, -39.94273075073680701, -67.36733013287428662 ) ) ;
#32344 = CARTESIAN_POINT ( 'NONE',  ( 9.221428961875151487, -19.60034550577672974, -36.62566438469894337 ) ) ;
#32345 = CARTESIAN_POINT ( 'NONE',  ( 12.52587677871439986, 18.86565027817080065, -21.14436856220130423 ) ) ;
#32346 = CARTESIAN_POINT ( 'NONE',  ( 46.64446819860030757, 22.34959245454500021, -76.02856699519020367 ) ) ;
#32347 = VECTOR ( 'NONE', #47532, 1000.000000000000000 ) ;
#32348 = CARTESIAN_POINT ( 'NONE',  ( 48.55442280000429633, -54.08752141328759677, -54.84940790413600098 ) ) ;
#32349 = DIRECTION ( 'NONE',  ( 0.04251717301921600217, 0.000000000000000000, -0.9990957361526742186 ) ) ;
#32350 = DIRECTION ( 'NONE',  ( 0.000000000000000000, 0.000000000000000000, -1.000000000000000000 ) ) ;
#32351 = CARTESIAN_POINT ( 'NONE',  ( 8.222937397696199469, -15.61618894467929941, -32.14999999999999858 ) ) ;
#32352 = FACE_OUTER_BOUND ( 'NONE', #39668, .T. ) ;
#32353 = ORIENTED_EDGE ( 'NONE', *, *, #46055, .F. ) ;
#32354 = CARTESIAN_POINT ( 'NONE',  ( 15.54540117339269933, -23.04318830182370093, -43.59251385424099823 ) ) ;
#32355 =( BOUNDED_CURVE ( )  B_SPLINE_CURVE ( 2, ( #10847, #25759, #41769 ),
 .UNSPECIFIED., .F., .T. ) 
 B_SPLINE_CURVE_WITH_KNOTS ( ( 3, 3 ),
 ( 2.168627590050199672, 3.232274745523179948 ),
 .UNSPECIFIED. ) 
 CURVE ( )  GEOMETRIC_REPRESENTATION_ITEM ( )  RATIONAL_B_SPLINE_CURVE ( ( 1.425426480542939967, 1.425426480542949959, 1.323085463760209857 ) ) 
 REPRESENTATION_ITEM ( '' )  );
#32356 = CARTESIAN_POINT ( 'NONE',  ( 16.13393739769620083, -15.61618894467929941, -10.21818181818179916 ) ) ;
#32357 = ORIENTED_EDGE ( 'NONE', *, *, #48211, .T. ) ;
#32358 = CARTESIAN_POINT ( 'NONE',  ( 71.35346284499661351, 1.390806392144110060, -70.26251807531768634 ) ) ;
#32359 = CARTESIAN_POINT ( 'NONE',  ( 60.70483243996059741, -45.55211676233259510, -47.28445363277229774 ) ) ;
#32360 = FACE_OUTER_BOUND ( 'NONE', #24969, .T. ) ;
#32361 = CARTESIAN_POINT ( 'NONE',  ( 50.20000624151330015, 18.43678156217400144, -76.14999999999999147 ) ) ;
#32363 = CARTESIAN_POINT ( 'NONE',  ( 0.3209249304026170480, -23.01378514180129997, -34.64999999999999858 ) ) ;
#32362 = CARTESIAN_POINT ( 'NONE',  ( 42.65610030855648205, 8.600309723121037919, -73.16201499959163357 ) ) ;
#32364 = CARTESIAN_POINT ( 'NONE',  ( 30.46076380116034343, 4.402158596034774440, -84.61108498746632733 ) ) ;
#32365 = CARTESIAN_POINT ( 'NONE',  ( 8.222938998452162807, -16.65174813775593776, -52.46600170312751743 ) ) ;
#32366 = ORIENTED_EDGE ( 'NONE', *, *, #13250, .T. ) ;
#32367 = CARTESIAN_POINT ( 'NONE',  ( 83.70743316420070812, -44.91498932721609805, -47.36488538498209522 ) ) ;
#32368 = EDGE_CURVE ( 'NONE', #35847, #4500, #35454, .T. ) ;
#32369 = ORIENTED_EDGE ( 'NONE', *, *, #43141, .T. ) ;
#32370 = ORIENTED_EDGE ( 'NONE', *, *, #36012, .F. ) ;
#32371 = CARTESIAN_POINT ( 'NONE',  ( 61.48309262502669981, -45.36446491065829889, -47.33735133955730134 ) ) ;
#32372 = CARTESIAN_POINT ( 'NONE',  ( 55.91596999402320023, 14.67228162054319895, -25.32543311652580087 ) ) ;
#32373 = CARTESIAN_POINT ( 'NONE',  ( 76.39209740234862522, -14.56176142460520317, -12.76245032130310264 ) ) ;
#32374 = CARTESIAN_POINT ( 'NONE',  ( 52.70023876989939993, -52.26368731436640047, -53.73525348785970124 ) ) ;
#32375 = STYLED_ITEM ( 'NONE', ( #17047 ), #43885 ) ;
#32376 = EDGE_LOOP ( 'NONE', ( #34781, #472, #22001, #47378, #26224 ) ) ;
#32377 = EDGE_LOOP ( 'NONE', ( #50921, #44805, #47834, #3776 ) ) ;
#32378 = CARTESIAN_POINT ( 'NONE',  ( 48.42313109053679909, 22.83113193936399909, -54.61340708730690352 ) ) ;
#32379 = CARTESIAN_POINT ( 'NONE',  ( 12.96511943382801313, -9.565397813277416006, -32.19390020089446125 ) ) ;
#32380 = CARTESIAN_POINT ( 'NONE',  ( 56.42219321547700162, -50.76386628334259399, -53.51233868223550161 ) ) ;
#32381 = DIRECTION ( 'NONE',  ( -1.000000000000000000, 0.000000000000000000, 0.000000000000000000 ) ) ;
#32382 = CARTESIAN_POINT ( 'NONE',  ( 65.05449253170610291, 1.020160266966620100, -17.84100813038880062 ) ) ;
#32383 = VERTEX_POINT ( 'NONE', #45397 ) ;
#32384 = CARTESIAN_POINT ( 'NONE',  ( 8.784728771177219286, 31.88305279678909443, -46.67204636144870022 ) ) ;
#32385 = CARTESIAN_POINT ( 'NONE',  ( 52.43830835031209858, -49.98684424990290154, -77.15472072683439819 ) ) ;
#32386 = CARTESIAN_POINT ( 'NONE',  ( 64.72741779930989026, 0.8986939045430250017, -70.58925035374339529 ) ) ;
#32387 = CARTESIAN_POINT ( 'NONE',  ( -11.80944000494499768, -34.05870648691990255, -45.03554556751409166 ) ) ;
#32388 = CARTESIAN_POINT ( 'NONE',  ( 23.62296424492599911, -17.96165786859479852, -56.10910496229280398 ) ) ;
#32389 = EDGE_CURVE ( 'NONE', #11278, #10625, #20013, .T. ) ;
#32390 = CARTESIAN_POINT ( 'NONE',  ( 84.44784216359251161, 11.88381105532070059, -47.47585302082339354 ) ) ;
#32391 = ADVANCED_FACE ( 'NONE', ( #19413 ), #48684, .T. ) ;
#32392 = CARTESIAN_POINT ( 'NONE',  ( 42.69362901904169405, -43.61869170235599569, -4.694965688641879353 ) ) ;
#32393 = CARTESIAN_POINT ( 'NONE',  ( 16.13393739769620083, -15.61618894467929941, -12.65000000000000036 ) ) ;
#32394 = CARTESIAN_POINT ( 'NONE',  ( 65.43042069957887463, -49.21324915460321137, -75.95351669811965678 ) ) ;
#32395 = CARTESIAN_POINT ( 'NONE',  ( 16.13393739769620083, -15.61618894467929941, 2.750000000000000000 ) ) ;
#32396 = DIRECTION ( 'NONE',  ( -1.000000000000000000, -0.000000000000000000, -0.000000000000000000 ) ) ;
#32397 = CARTESIAN_POINT ( 'NONE',  ( 11.91260932085759983, -21.26622862968550010, -49.55142757455229940 ) ) ;
#32398 = CARTESIAN_POINT ( 'NONE',  ( 17.93046645737056011, -52.54004929531408408, -75.96019247805895702 ) ) ;
#32399 = ORIENTED_EDGE ( 'NONE', *, *, #50279, .F. ) ;
#32400 = CARTESIAN_POINT ( 'NONE',  ( 14.33365608540959890, -52.10138505899109873, -75.81674732426940011 ) ) ;
#32401 = CARTESIAN_POINT ( 'NONE',  ( 47.25178503846339595, -54.75397576815099399, -54.62830328906390065 ) ) ;
#32402 = CARTESIAN_POINT ( 'NONE',  ( 22.04684738446895764, -12.20819461931851357, -38.28615615749678369 ) ) ;
#32403 = DIRECTION ( 'NONE',  ( 0.000000000000000000, 1.000000000000000000, 0.000000000000000000 ) ) ;
#32404 = CARTESIAN_POINT ( 'NONE',  ( 24.04493739677426234, -15.61429984773749169, -55.50759605722655010 ) ) ;
#32405 = CIRCLE ( 'NONE', #642, 5.499999999999998224 ) ;
#32406 = DIRECTION ( 'NONE',  ( 0.3535533905932799481, 0.6123724356957926940, 0.7071067811865460184 ) ) ;
#32407 = B_SPLINE_CURVE_WITH_KNOTS ( 'NONE', 3,
 ( #11085, #15002, #27052, #48012, #11600, #15776, #43056, #30972, #4237, #31479, #35940, #12111, #3216, #27559, #15269, #16035, #19707, #7405, #36195, #27818 ),
 .UNSPECIFIED., .F., .F.,
 ( 4, 2, 1, 1, 1, 2, 2, 2, 1, 1, 1, 2, 4 ),
 ( 0.5244055620448262456, 0.5318367251378740557, 0.5392678882309219768, 0.5541302144170151545, 0.5838548667892086153, 0.6433041715336005328, 0.7622027810223866995, 0.7696339441154360639, 0.7770651072084853173, 0.7919274333945859334, 0.8216520857667848343, 0.8811013905111874100, 1.000000000000000000 ),
 .UNSPECIFIED. ) ;
#32408 = FACE_OUTER_BOUND ( 'NONE', #32119, .T. ) ;
#32410 = CARTESIAN_POINT ( 'NONE',  ( 8.223360643215830379, -15.61635149015999957, -74.50766849176298479 ) ) ;
#32409 = DIRECTION ( 'NONE',  ( 0.000000000000000000, 0.000000000000000000, -1.000000000000000000 ) ) ;
#32411 = VECTOR ( 'NONE', #22579, 1000.000000000000000 ) ;
#32412 = FACE_OUTER_BOUND ( 'NONE', #39321, .T. ) ;
#32413 = CARTESIAN_POINT ( 'NONE',  ( 48.52740815778420114, 22.81021699678759873, -54.66898914902790096 ) ) ;
#32414 = ORIENTED_EDGE ( 'NONE', *, *, #21078, .T. ) ;
#32415 = CARTESIAN_POINT ( 'NONE',  ( 52.77947507452280007, -49.70653929005730021, -48.82716071996740226 ) ) ;
#32416 = ORIENTED_EDGE ( 'NONE', *, *, #34508, .T. ) ;
#32417 = DIRECTION ( 'NONE',  ( -1.000000000000000000, 0.000000000000000000, 0.000000000000000000 ) ) ;
#32418 = DIRECTION ( 'NONE',  ( -1.000000000000000000, -0.000000000000000000, -0.000000000000000000 ) ) ;
#32419 = LINE ( 'NONE', #7588, #39647 ) ;
#32421 = CARTESIAN_POINT ( 'NONE',  ( 53.90944104900800227, 17.28048702971980077, -26.72631102452049845 ) ) ;
#32420 = CARTESIAN_POINT ( 'NONE',  ( 84.25787305080559975, 12.62791954601209987, -47.19072229952409714 ) ) ;
#32422 = CARTESIAN_POINT ( 'NONE',  ( 20.70280240204410305, -20.98908679115569953, -62.72850739055710534 ) ) ;
#32423 = CARTESIAN_POINT ( 'NONE',  ( 52.59913543871140007, 18.59668918921780190, -48.56922736988880018 ) ) ;
#32424 = CARTESIAN_POINT ( 'NONE',  ( 57.04817660294939685, -45.12828403733969651, -16.72517180066030207 ) ) ;
#32425 = CARTESIAN_POINT ( 'NONE',  ( 12.06284766121009966, -63.44323389162830296, -22.25048313876769868 ) ) ;
#32426 = EDGE_LOOP ( 'NONE', ( #30461, #26999, #42254, #7092 ) ) ;
#32427 = EDGE_CURVE ( 'NONE', #16602, #24198, #43021, .T. ) ;
#32428 = VERTEX_POINT ( 'NONE', #19915 ) ;
#32429 = CARTESIAN_POINT ( 'NONE',  ( 12.00051660606130177, -65.12476112613200030, -16.59289575486429769 ) ) ;
#32430 = CARTESIAN_POINT ( 'NONE',  ( 11.91762376145129743, 34.07103531667779350, -47.17701748307580090 ) ) ;
#32431 = CARTESIAN_POINT ( 'NONE',  ( 39.13393739769620083, -15.61618894467929941, -15.65000000000000036 ) ) ;
#32432 = CARTESIAN_POINT ( 'NONE',  ( 47.28894142370269549, -54.73349313190560395, -54.78420696420580072 ) ) ;
#32433 = CARTESIAN_POINT ( 'NONE',  ( 11.18482555203581441, -65.08283002702597742, -22.98856200317182896 ) ) ;
#32434 = CYLINDRICAL_SURFACE ( 'NONE', #25913, 1.000000000000003775 ) ;
#32435 = ORIENTED_EDGE ( 'NONE', *, *, #10588, .F. ) ;
#32436 = CARTESIAN_POINT ( 'NONE',  ( 0.5716597375277996385, -15.61618894467929941, -8.050000000000000711 ) ) ;
#32437 = CARTESIAN_POINT ( 'NONE',  ( 11.13393739769619906, -63.16199138576410377, -43.91250325741290084 ) ) ;
#32438 = CARTESIAN_POINT ( 'NONE',  ( 47.99879017111000223, 23.44647020611570198, -55.58088518830679448 ) ) ;
#32439 = LINE ( 'NONE', #4692, #48459 ) ;
#32440 = CARTESIAN_POINT ( 'NONE',  ( 63.49151163952229382, 1.387131204727290124, -62.61203846038919352 ) ) ;
#32441 = CARTESIAN_POINT ( 'NONE',  ( 22.90112932213407149, -15.61618880384378905, -64.45281843961751633 ) ) ;
#32442 = VERTEX_POINT ( 'NONE', #51137 ) ;
#32443 = CARTESIAN_POINT ( 'NONE',  ( 10.13393739769589885, 22.91950879131600161, -35.14999999999999858 ) ) ;
#32444 = DIRECTION ( 'NONE',  ( -0.2260571801428161165, 1.249000902703300368E-16, 0.9741140340359943917 ) ) ;
#32445 = AXIS2_PLACEMENT_3D ( 'NONE', #27189, #20095, #31620 ) ;
#32446 = CARTESIAN_POINT ( 'NONE',  ( 53.79693027462740673, 21.85383143305579878, -55.67392376200250226 ) ) ;
#32447 = CARTESIAN_POINT ( 'NONE',  ( 15.75961300321349690, -23.85285096904510027, -70.30678751322059838 ) ) ;
#32448 = CARTESIAN_POINT ( 'NONE',  ( 22.90066830340121840, -15.61618925674170022, -38.84718272210749035 ) ) ;
#32449 = CARTESIAN_POINT ( 'NONE',  ( 53.70843326355630154, 20.08253603804340059, -75.56345715548110320 ) ) ;
#32450 = ADVANCED_FACE ( 'NONE', ( #14966 ), #20172, .T. ) ;
#32451 = CARTESIAN_POINT ( 'NONE',  ( 47.09661774331770090, -53.91811590987600056, -75.74144252524291687 ) ) ;
#32452 = ORIENTED_EDGE ( 'NONE', *, *, #7096, .T. ) ;
#32453 = CARTESIAN_POINT ( 'NONE',  ( 12.24237353118370031, -9.263046062766429500, -61.55771731514269618 ) ) ;
#32454 = CARTESIAN_POINT ( 'NONE',  ( 53.27415667070290084, -49.51643490155070282, -49.18599851058429806 ) ) ;
#32455 = FACE_BOUND ( 'NONE', #44268, .T. ) ;
#32456 = CARTESIAN_POINT ( 'NONE',  ( 47.33320835756340017, 23.23980503609559634, -75.00312280669810150 ) ) ;
#32457 = CARTESIAN_POINT ( 'NONE',  ( 19.44419974378226712, -53.43866955709284383, -16.61603860993866633 ) ) ;
#32458 = DIRECTION ( 'NONE',  ( 0.000000000000000000, 0.000000000000000000, -1.000000000000000000 ) ) ;
#32459 = CARTESIAN_POINT ( 'NONE',  ( 12.36320305067610015, 33.31445045643330616, -15.76422791930239953 ) ) ;
#32460 = CARTESIAN_POINT ( 'NONE',  ( 15.63466510375951302, -49.61614664559245114, -83.23984175397698948 ) ) ;
#32461 = CARTESIAN_POINT ( 'NONE',  ( 73.22214118178139586, 1.102581332775300016, -68.74251431096891451 ) ) ;
#32463 = FACE_OUTER_BOUND ( 'NONE', #20344, .T. ) ;
#32462 = CARTESIAN_POINT ( 'NONE',  ( -10.65907218400529999, 10.01002500177520105, -4.264802379178179947 ) ) ;
#32464 = CARTESIAN_POINT ( 'NONE',  ( 63.07934790479939835, 0.9219904752505979628, -68.88295677568349618 ) ) ;
#32465 = CARTESIAN_POINT ( 'NONE',  ( 61.41767410373359581, 13.94937499305689954, -46.63511954085710443 ) ) ;
#32466 = CARTESIAN_POINT ( 'NONE',  ( -18.46117119615139757, -52.29887744895199830, -53.76231701354959824 ) ) ;
#32467 = ORIENTED_EDGE ( 'NONE', *, *, #3416, .F. ) ;
#32468 = CARTESIAN_POINT ( 'NONE',  ( 53.36494266454960211, -49.38052133118390685, -48.76947209987829979 ) ) ;
#32469 = AXIS2_PLACEMENT_3D ( 'NONE', #2582, #49766, #13858 ) ;
#32470 = CARTESIAN_POINT ( 'NONE',  ( 58.02351487609760028, -45.11618911064800841, -25.42861971957569622 ) ) ;
#32471 = CARTESIAN_POINT ( 'NONE',  ( 9.807682861627638360, -20.47775237701530315, -72.58401298376038824 ) ) ;
#32472 = CARTESIAN_POINT ( 'NONE',  ( 13.11803317904709942, 19.67693774826710040, -21.59044394916249843 ) ) ;
#32473 = CARTESIAN_POINT ( 'NONE',  ( 56.68398579694790129, 14.78090256954719983, -26.22808307489359692 ) ) ;
#32474 = CARTESIAN_POINT ( 'NONE',  ( 22.89779876327829911, -12.49259093177239954, -80.09494718402969227 ) ) ;
#32476 = CARTESIAN_POINT ( 'NONE',  ( 51.59928859560229597, 19.10878590974600044, -76.34973321511711220 ) ) ;
#32475 = VECTOR ( 'NONE', #29107, 1000.000000000000114 ) ;
#32477 = CARTESIAN_POINT ( 'NONE',  ( 52.83452149259679942, 18.43073975597890168, -48.76554741659339953 ) ) ;
#32478 = CARTESIAN_POINT ( 'NONE',  ( 71.34390086684349797, 1.188582381068100213, -70.60520998597918663 ) ) ;
#32479 = CARTESIAN_POINT ( 'NONE',  ( 26.13393739769619728, -2.337132753317950229, -39.64999999999999858 ) ) ;
#32480 = CARTESIAN_POINT ( 'NONE',  ( 75.41292065207370854, -44.30578118641259522, -13.67617913553320186 ) ) ;
#32481 = ORIENTED_EDGE ( 'NONE', *, *, #27532, .F. ) ;
#32482 = EDGE_CURVE ( 'NONE', #29117, #6764, #27015, .T. ) ;
#32483 = CIRCLE ( 'NONE', #17525, 5.499999999999998224 ) ;
#32484 = CARTESIAN_POINT ( 'NONE',  ( 16.13393739769620083, -15.61618894467929941, -35.02873218748179340 ) ) ;
#32485 = CARTESIAN_POINT ( 'NONE',  ( 47.60675842126480006, -54.53351696772000423, -54.82215150501349399 ) ) ;
#32486 = CARTESIAN_POINT ( 'NONE',  ( -5.346827492203339638, 15.73560381608349701, -4.480328059553770004 ) ) ;
#32487 = CARTESIAN_POINT ( 'NONE',  ( 40.50275707922880031, 13.54185611314979987, -4.148922232357650230 ) ) ;
#32488 = CARTESIAN_POINT ( 'NONE',  ( 56.82230906587010111, 18.91528989288639906, -52.48692337665460173 ) ) ;
#32490 = ADVANCED_FACE ( 'NONE', ( #7117 ), #22000, .T. ) ;
#32489 = CARTESIAN_POINT ( 'NONE',  ( 71.31202044992319600, 1.326578174762029994, -60.85378544217730479 ) ) ;
#32491 = CARTESIAN_POINT ( 'NONE',  ( 0.1457841021255935343, -15.61618894467929941, -34.68167779225149161 ) ) ;
#32492 = CARTESIAN_POINT ( 'NONE',  ( 71.53423548837180590, 1.309820314133740116, -60.93204159761199890 ) ) ;
#32493 = CARTESIAN_POINT ( 'NONE',  ( 23.94343581735640214, -16.90563803632168316, -71.55974283691564608 ) ) ;
#32494 = B_SPLINE_CURVE_WITH_KNOTS ( 'NONE', 3,
 ( #51718, #43351, #20242, #35212 ),
 .UNSPECIFIED., .F., .F.,
 ( 4, 4 ),
 ( 0.000000000000000000, 1.000000000000000000 ),
 .UNSPECIFIED. ) ;
#32495 = EDGE_CURVE ( 'NONE', #27228, #40081, #29526, .T. ) ;
#32496 = CARTESIAN_POINT ( 'NONE',  ( 65.13423472332449649, 1.371651820402789879, -70.41530492215990478 ) ) ;
#32497 = EDGE_LOOP ( 'NONE', ( #29935, #40692, #50477, #30767 ) ) ;
#32498 = VERTEX_POINT ( 'NONE', #47469 ) ;
#32499 = DIRECTION ( 'NONE',  ( -1.000000000000000000, 0.000000000000000000, 0.000000000000000000 ) ) ;
#32500 = CARTESIAN_POINT ( 'NONE',  ( 58.92073396209919878, -28.11618894467929763, -15.65000000000000036 ) ) ;
#32501 = EDGE_LOOP ( 'NONE', ( #2660, #2307, #9454, #12431, #21506 ) ) ;
#32502 = CARTESIAN_POINT ( 'NONE',  ( 56.42249722292559966, -45.43314942097339326, -25.29439853946469796 ) ) ;
#32503 = CARTESIAN_POINT ( 'NONE',  ( 9.487004236308452576, -14.16812596634764354, -49.52099469407719567 ) ) ;
#32504 = VERTEX_POINT ( 'NONE', #11564 ) ;
#32505 = CARTESIAN_POINT ( 'NONE',  ( -0.1295185695944119919, -31.87964491196989414, 4.943674098299959851 ) ) ;
#32506 = CARTESIAN_POINT ( 'NONE',  ( 15.20323989161956391, -8.855217236353226440, -71.90910339118616434 ) ) ;
#32507 = ADVANCED_FACE ( 'NONE', ( #31694 ), #11823, .T. ) ;
#32508 = CARTESIAN_POINT ( 'NONE',  ( 24.04493605050502936, -15.62153787553132034, -65.50788166513238764 ) ) ;
#32509 = CARTESIAN_POINT ( 'NONE',  ( 16.66011486035179701, -7.387832041036370256, -41.31265874393589144 ) ) ;
#32510 = CARTESIAN_POINT ( 'NONE',  ( 45.34325132301859895, 2.693353616613840096, -34.65000333093299645 ) ) ;
#32511 = CARTESIAN_POINT ( 'NONE',  ( 42.04061362852223027, -37.63029778570905393, -80.11654543539063411 ) ) ;
#32512 = EDGE_CURVE ( 'NONE', #17157, #30658, #44285, .T. ) ;
#32513 = VERTEX_POINT ( 'NONE', #49017 ) ;
#32514 = CARTESIAN_POINT ( 'NONE',  ( 10.73251648177490125, -64.28497866039579378, -23.50916409409489916 ) ) ;
#32515 = CARTESIAN_POINT ( 'NONE',  ( 20.82320479922240253, -9.323532524045690550, -79.71634641925129472 ) ) ;
#32516 = AXIS2_PLACEMENT_3D ( 'NONE', #29508, #42353, #10647 ) ;
#32517 = AXIS2_PLACEMENT_3D ( 'NONE', #24030, #20119, #28499 ) ;
#32518 = CARTESIAN_POINT ( 'NONE',  ( 9.221354224360256424, -11.63216018383065986, -32.67433414864056118 ) ) ;
#32519 = VECTOR ( 'NONE', #21547, 1000.000000000000000 ) ;
#32520 = CARTESIAN_POINT ( 'NONE',  ( 14.00623127734409934, 20.66741474030959935, -75.53710645103448940 ) ) ;
#32521 = CARTESIAN_POINT ( 'NONE',  ( 23.59532682517835056, -18.30036212264693773, -59.90219143874516305 ) ) ;
#32522 = CARTESIAN_POINT ( 'NONE',  ( 84.44784216359251161, -43.11618894467930119, -47.47585302082339354 ) ) ;
#32523 = CARTESIAN_POINT ( 'NONE',  ( 48.42521416700790127, 25.14253336855949783, -74.14999999999999147 ) ) ;
#32524 = EDGE_CURVE ( 'NONE', #37146, #12364, #1305, .T. ) ;
#32525 = CARTESIAN_POINT ( 'NONE',  ( 9.742225364899180562, -20.82471445568270241, -42.29002317614339290 ) ) ;
#32526 = VERTEX_POINT ( 'NONE', #4454 ) ;
#32527 = CARTESIAN_POINT ( 'NONE',  ( 53.50804305007959982, -48.99566724766310699, -27.12258064042100258 ) ) ;
#32528 = CARTESIAN_POINT ( 'NONE',  ( 15.54393737248089913, -50.81691517260839674, -20.39348321914689777 ) ) ;
#32529 = CARTESIAN_POINT ( 'NONE',  ( 50.45285235388368505, -36.16382338628016413, -76.19501922796175108 ) ) ;
#32530 = CARTESIAN_POINT ( 'NONE',  ( 8.428887333864649278, -17.68705018600014256, -64.70899835976443626 ) ) ;
#32531 = CARTESIAN_POINT ( 'NONE',  ( 9.366937397696199596, -15.61618894467949836, -28.45282021618999835 ) ) ;
#32532 = ORIENTED_EDGE ( 'NONE', *, *, #17285, .T. ) ;
#32533 = CARTESIAN_POINT ( 'NONE',  ( -6.562477110335280805, -46.34503278340989141, -5.556459679399529783 ) ) ;
#32534 = CARTESIAN_POINT ( 'NONE',  ( 47.38009481930370015, 23.43661158662580135, -54.80057124748829978 ) ) ;
#32535 = DIRECTION ( 'NONE',  ( 0.000000000000000000, -1.000000000000000000, 0.000000000000000000 ) ) ;
#32536 = CARTESIAN_POINT ( 'NONE',  ( 63.44650199127489998, 1.383928098097870096, -62.75238677440889035 ) ) ;
#32537 = CARTESIAN_POINT ( 'NONE',  ( 54.66073981893745071, 16.79829358645031334, -26.72725689915946745 ) ) ;
#32538 = CARTESIAN_POINT ( 'NONE',  ( 11.35626914493999884, 34.06258128150169995, -17.73521909030590038 ) ) ;
#32539 = PLANE ( 'NONE',  #40824 ) ;
#32540 = CARTESIAN_POINT ( 'NONE',  ( 17.16951678489785138, -7.705193502012818385, -61.33399649469901505 ) ) ;
#32541 = FACE_OUTER_BOUND ( 'NONE', #16670, .T. ) ;
#32542 = CARTESIAN_POINT ( 'NONE',  ( 59.86299467440079525, -46.00059797876070178, -47.55238746115900028 ) ) ;
#32543 = CARTESIAN_POINT ( 'NONE',  ( 24.01953109262902331, -14.96959097810077033, -75.76629004851450588 ) ) ;
#32544 = CARTESIAN_POINT ( 'NONE',  ( 64.81907236522970095, 1.326666718054990035, -60.91913985162000245 ) ) ;
#32545 = CARTESIAN_POINT ( 'NONE',  ( -18.86606260230390220, 19.38381105532060289, 16.85000000000000142 ) ) ;
#32546 = ADVANCED_FACE ( 'NONE', ( #32455, #1043 ), #40874, .T. ) ;
#32547 = DIRECTION ( 'NONE',  ( 0.000000000000000000, 1.000000000000000000, 0.000000000000000000 ) ) ;
#32548 = AXIS2_PLACEMENT_3D ( 'NONE', #43009, #19137, #35116 ) ;
#32549 = CARTESIAN_POINT ( 'NONE',  ( 10.22106108903712851, -12.20813745483522617, -47.61948721594488632 ) ) ;
#32550 = ORIENTED_EDGE ( 'NONE', *, *, #33050, .T. ) ;
#32551 = CARTESIAN_POINT ( 'NONE',  ( 20.13393739009281447, 24.18330851781475488, -20.36976997827363434 ) ) ;
#32552 = CARTESIAN_POINT ( 'NONE',  ( 10.14239080937649895, 31.99922782709920099, -45.99351196094749383 ) ) ;
#32553 = DIRECTION ( 'NONE',  ( -1.000000000000000000, 0.000000000000000000, 0.000000000000000000 ) ) ;
#32554 = VECTOR ( 'NONE', #22808, 1000.000000000000000 ) ;
#32555 = VECTOR ( 'NONE', #14807, 1000.000000000000000 ) ;
#32556 = CONICAL_SURFACE ( 'NONE', #39298, 0.7980000000000000426, 0.7853981633974476129 ) ;
#32557 = CARTESIAN_POINT ( 'NONE',  ( 13.16285594202260079, -8.418783507588880610, -81.23899999999999011 ) ) ;
#32558 = ADVANCED_FACE ( 'NONE', ( #49273 ), #8395, .T. ) ;
#32559 = ORIENTED_EDGE ( 'NONE', *, *, #51762, .F. ) ;
#32560 = CARTESIAN_POINT ( 'NONE',  ( 18.82294826520599784, 20.50885532556510071, -74.53071772762450564 ) ) ;
#32561 = ORIENTED_EDGE ( 'NONE', *, *, #16484, .F. ) ;
#32562 = EDGE_LOOP ( 'NONE', ( #13787, #50593, #19572, #28437 ) ) ;
#32563 = AXIS2_PLACEMENT_3D ( 'NONE', #27303, #11598, #31476 ) ;
#32564 = EDGE_LOOP ( 'NONE', ( #10439, #26659, #22777, #19086, #5720, #4729 ) ) ;
#32565 = CARTESIAN_POINT ( 'NONE',  ( 12.39616473040790012, -65.41581959449560202, -47.19115183429629923 ) ) ;
#32566 = CARTESIAN_POINT ( 'NONE',  ( 57.42036092767180122, -45.80331578673570192, -26.28157325255090271 ) ) ;
#32567 = CARTESIAN_POINT ( 'NONE',  ( 21.46001303057629883, -20.23894261149060014, -81.23899999999999011 ) ) ;
#32568 = CARTESIAN_POINT ( 'NONE',  ( 12.14987812824804614, -8.703624956618371655, -62.84100237377567311 ) ) ;
#32569 = CARTESIAN_POINT ( 'NONE',  ( 61.44894565603249958, 13.98760630883520051, -46.94547993154250065 ) ) ;
#32570 = ORIENTED_EDGE ( 'NONE', *, *, #38437, .T. ) ;
#32571 = ORIENTED_EDGE ( 'NONE', *, *, #40387, .F. ) ;
#32572 = DIRECTION ( 'NONE',  ( 1.000000000000000000, 0.000000000000000000, 0.000000000000000000 ) ) ;
#32573 = ORIENTED_EDGE ( 'NONE', *, *, #20544, .F. ) ;
#32574 = CARTESIAN_POINT ( 'NONE',  ( 11.14568262985824276, -63.77342232876421946, -24.13735806910611004 ) ) ;
#32575 = CARTESIAN_POINT ( 'NONE',  ( 26.13393739769619728, -2.337132753317950229, -84.65000000000000568 ) ) ;
#32576 = CARTESIAN_POINT ( 'NONE',  ( 38.67452568954060155, -33.11618894467940066, -81.65000000000000568 ) ) ;
#32577 = ORIENTED_EDGE ( 'NONE', *, *, #42880, .F. ) ;
#32578 = VERTEX_POINT ( 'NONE', #13366 ) ;
#32579 = CYLINDRICAL_SURFACE ( 'NONE', #11624, 3.000000000000000444 ) ;
#32580 = DIRECTION ( 'NONE',  ( -2.565320000000000120E-13, -1.000000000000000000, 8.628712999999999808E-13 ) ) ;
#32581 = CARTESIAN_POINT ( 'NONE',  ( 61.36407574442390001, 14.34895716591110038, -47.65743212064409562 ) ) ;
#32582 = CARTESIAN_POINT ( 'NONE',  ( 52.33303711461739738, 14.99040022374890135, -14.16117149841140055 ) ) ;
#32583 = CARTESIAN_POINT ( 'NONE',  ( -3.610905026759430037, 19.17089483124840044, -4.296538310234230273 ) ) ;
#32584 = CARTESIAN_POINT ( 'NONE',  ( -6.116815533026069396, 15.22351030921669945, -4.952229201496230360 ) ) ;
#32585 = CONICAL_SURFACE ( 'NONE', #1688, 3.118521338338071214, 0.6364736820000767015 ) ;
#32586 = VECTOR ( 'NONE', #51060, 1000.000000000000000 ) ;
#32587 = CIRCLE ( 'NONE', #50178, 1.500000000000001332 ) ;
#32588 = CARTESIAN_POINT ( 'NONE',  ( 9.366668631897962172, -15.87390888100710029, -63.83506491120805038 ) ) ;
#32589 = CARTESIAN_POINT ( 'NONE',  ( 55.65312842910222457, 14.73492698990839322, -16.92919021100515309 ) ) ;
#32590 = EDGE_CURVE ( 'NONE', #38460, #49655, #24920, .T. ) ;
#32591 = AXIS2_PLACEMENT_3D ( 'NONE', #33086, #21298, #22591 ) ;
#32592 = CARTESIAN_POINT ( 'NONE',  ( 8.681468816368131058, -13.15703050580209954, -58.38896007259789656 ) ) ;
#32593 = B_SPLINE_SURFACE_WITH_KNOTS ( 'NONE', 3, 3, ( 
 ( #1567, #17558, #47160, #51077 ),
 ( #15175, #26956, #26430, #26684 ),
 ( #2867, #3127, #19096, #46905 ),
 ( #50821, #31132, #30106, #22756 ),
 ( #11248, #35071, #10212, #34294 ),
 ( #46387, #27210, #34558, #50561 ),
 ( #14653, #30875, #42448, #30362 ),
 ( #38510, #38777, #18580, #42966 ),
 ( #26173, #19356, #6535, #7061 ),
 ( #39033, #2609, #10991, #43223 ),
 ( #7314, #46647, #42708, #18315 ),
 ( #30623, #23263, #14395, #18833 ),
 ( #46126, #3389, #39281, #22241 ),
 ( #50043, #14136, #22498, #10475 ),
 ( #42183, #38248, #23012, #6283 ) ),
 .UNSPECIFIED., .F., .F., .F.,
 ( 4, 1, 1, 1, 1, 1, 1, 1, 1, 3, 4 ),
 ( 4, 4 ),
 ( 0.000000000000000000, 0.1111111111111110078, 0.2222222222222219878, 0.3333333333333329818, 0.4444444444444439757, 0.5555555555555560243, 0.6666666666666670737, 0.7777777777777779011, 0.8888888888888889506, 1.000000000000000000, 1.010000000000000009 ),
 ( 0.05091673086865800002, 0.2043272503186320255 ),
 .UNSPECIFIED. ) ;
#32594 = ORIENTED_EDGE ( 'NONE', *, *, #45123, .F. ) ;
#32596 = ADVANCED_FACE ( 'NONE', ( #16769 ), #16249, .T. ) ;
#32595 = CARTESIAN_POINT ( 'NONE',  ( 56.59159595385349917, 16.48196327652579996, -48.16094229791880110 ) ) ;
#32598 = AXIS2_PLACEMENT_3D ( 'NONE', #36641, #21175, #4170 ) ;
#32597 = DIRECTION ( 'NONE',  ( 0.000000000000000000, 0.000000000000000000, -1.000000000000000000 ) ) ;
#32599 = CARTESIAN_POINT ( 'NONE',  ( 11.89321892211240161, 34.20364954171930094, -18.17421237891140251 ) ) ;
#32600 = CARTESIAN_POINT ( 'NONE',  ( 72.27589226135678757, 1.457833794292699992, -69.65505222163159260 ) ) ;
#32601 = ADVANCED_FACE ( 'NONE', ( #5504 ), #4976, .F. ) ;
#32602 = CARTESIAN_POINT ( 'NONE',  ( 44.14365615324429371, -39.96620590573778742, -65.96444131013311107 ) ) ;
#32603 =( NAMED_UNIT ( * ) PLANE_ANGLE_UNIT ( ) SI_UNIT ( $, .RADIAN. ) );
#32604 = CARTESIAN_POINT ( 'NONE',  ( -1.143840380081600161, -14.00933513942850794, -35.76111111111113416 ) ) ;
#32605 = CARTESIAN_POINT ( 'NONE',  ( 49.45769129680230236, -53.75852492999699450, -55.06250210633439934 ) ) ;
#32606 = B_SPLINE_CURVE_WITH_KNOTS ( 'NONE', 3,
 ( #5875, #5629, #1426, #14513, #34413, #50424, #49905, #37326, #50160, #18436, #45712, #33640, #46503, #33380, #25507, #1945 ),
 .UNSPECIFIED., .F., .F.,
 ( 4, 2, 2, 2, 2, 2, 2, 4 ),
 ( -1.183080999999999906E-15, 0.07216186899280699341, 0.1546325764131580016, 0.2061767685508779924, 0.2319488646197380433, 0.2731842183299139637, 0.3391607842661950034, 0.4123535371017569839 ),
 .UNSPECIFIED. ) ;
#32607 = CARTESIAN_POINT ( 'NONE',  ( 46.13393739769619373, 2.762490711761015572, -83.77132034355965118 ) ) ;
#32608 = DIRECTION ( 'NONE',  ( -1.000000000000000000, 0.000000000000000000, 0.000000000000000000 ) ) ;
#32609 = CARTESIAN_POINT ( 'NONE',  ( 65.04224801900546993, -32.25487679741158331, -17.84439582078725550 ) ) ;
#32610 = CARTESIAN_POINT ( 'NONE',  ( 0.1339373976962109913, -15.61618894467929941, -34.64999999999999858 ) ) ;
#32611 = ORIENTED_EDGE ( 'NONE', *, *, #42644, .F. ) ;
#32612 = CARTESIAN_POINT ( 'NONE',  ( 23.57992767232060416, -15.86901926038440003, -47.07814682104019255 ) ) ;
#32613 = CARTESIAN_POINT ( 'NONE',  ( 63.97287235346109213, 1.200163167270720033, -61.36285812046030230 ) ) ;
#32614 = ORIENTED_EDGE ( 'NONE', *, *, #5646, .T. ) ;
#32615 = CARTESIAN_POINT ( 'NONE',  ( 47.90111851008797572, -46.16659547561683041, 16.85000000000000142 ) ) ;
#32616 = CARTESIAN_POINT ( 'NONE',  ( 61.08724268487739550, -45.59010680718600383, -47.64259283952999624 ) ) ;
#32617 = DIRECTION ( 'NONE',  ( 0.000000000000000000, 1.000000000000000000, 0.000000000000000000 ) ) ;
#32618 = DIRECTION ( 'NONE',  ( 0.000000000000000000, 0.000000000000000000, -1.000000000000000000 ) ) ;
#32620 = CARTESIAN_POINT ( 'NONE',  ( 0.2609591194317595897, -22.97916386469509575, -34.64999999999999147 ) ) ;
#32619 = CARTESIAN_POINT ( 'NONE',  ( 42.92096165568810306, 8.626172559110205640, -71.88163569493146099 ) ) ;
#32621 = CARTESIAN_POINT ( 'NONE',  ( 53.62552786343490396, -51.33071804962359153, -75.58099297212140755 ) ) ;
#32622 = DIRECTION ( 'NONE',  ( 0.000000000000000000, 0.000000000000000000, -1.000000000000000000 ) ) ;
#32623 = EDGE_CURVE ( 'NONE', #1782, #6044, #39601, .T. ) ;
#32624 = VERTEX_POINT ( 'NONE', #32721 ) ;
#32625 = CARTESIAN_POINT ( 'NONE',  ( 83.94526921706011535, -44.52752621732469862, -47.24461768887499602 ) ) ;
#32626 = ORIENTED_EDGE ( 'NONE', *, *, #31624, .T. ) ;
#32627 = VERTEX_POINT ( 'NONE', #4712 ) ;
#32628 = CARTESIAN_POINT ( 'NONE',  ( 41.13393739769620083, -15.61618894467929941, -84.65000000000000568 ) ) ;
#32629 = AXIS2_PLACEMENT_3D ( 'NONE', #31300, #47074, #27130 ) ;
#32630 = CARTESIAN_POINT ( 'NONE',  ( 11.72609483531606323, -55.37304398355237822, -21.92220830349348049 ) ) ;
#32631 = CIRCLE ( 'NONE', #10074, 1.000000000000000888 ) ;
#32632 = CARTESIAN_POINT ( 'NONE',  ( 76.44668319880682361, -6.578471008536523001, -12.99766820392643574 ) ) ;
#32633 = CARTESIAN_POINT ( 'NONE',  ( 53.73900786348829683, -51.91625817396269582, -53.89034489052589549 ) ) ;
#32634 = VECTOR ( 'NONE', #28705, 1000.000000000000000 ) ;
#32635 = VERTEX_POINT ( 'NONE', #28548 ) ;
#32636 = ORIENTED_EDGE ( 'NONE', *, *, #46381, .T. ) ;
#32637 = AXIS2_PLACEMENT_3D ( 'NONE', #29382, #826, #9491 ) ;
#32638 = AXIS2_PLACEMENT_3D ( 'NONE', #49587, #13930, #5806 ) ;
#32639 = CARTESIAN_POINT ( 'NONE',  ( -0.3803200024020541581, 14.07826830858616063, -35.09718034791147545 ) ) ;
#32640 = DIRECTION ( 'NONE',  ( 1.000000000000000000, 0.000000000000000000, 0.000000000000000000 ) ) ;
#32641 = CARTESIAN_POINT ( 'NONE',  ( 8.806603807574589382, -63.23125877106109982, -46.67034945549170288 ) ) ;
#32642 = CARTESIAN_POINT ( 'NONE',  ( 24.03381966901990552, -15.16329667443855911, -59.77410034332016409 ) ) ;
#32643 = CARTESIAN_POINT ( 'NONE',  ( 64.08038400710292137, 11.23736444591397543, -62.44999999999999574 ) ) ;
#32644 = ORIENTED_EDGE ( 'NONE', *, *, #43080, .F. ) ;
#32645 = CARTESIAN_POINT ( 'NONE',  ( 9.986016378432044149, 30.93468997499846296, -13.71124846808129050 ) ) ;
#32646 = DIRECTION ( 'NONE',  ( 0.2260571801428161165, -2.775557561562891043E-17, -0.9741140340359943917 ) ) ;
#32647 = CARTESIAN_POINT ( 'NONE',  ( 64.81979753630270125, 0.8904513541338869853, -70.65165619965239330 ) ) ;
#32648 = CARTESIAN_POINT ( 'NONE',  ( 60.64009084818329853, 14.33648947266850016, -47.14749194313639435 ) ) ;
#32649 = CARTESIAN_POINT ( 'NONE',  ( 23.45525733055259821, -18.44196707332659813, -62.12974372312790194 ) ) ;
#32650 = PLANE ( 'NONE',  #45589 ) ;
#32651 = CARTESIAN_POINT ( 'NONE',  ( 42.11495618085190529, -44.00662160972859738, -4.742906900993289376 ) ) ;
#32652 = CARTESIAN_POINT ( 'NONE',  ( 27.50893739769620083, -36.61730498645199816, -35.14999999999999858 ) ) ;
#32653 = CARTESIAN_POINT ( 'NONE',  ( 70.83745409581581498, -49.21324915459896943, -75.95351669811965678 ) ) ;
#32654 = CARTESIAN_POINT ( 'NONE',  ( 67.09900448097283743, 1.833136996312119571, -20.08988941315463705 ) ) ;
#32655 = CARTESIAN_POINT ( 'NONE',  ( 64.05763092918830637, 1.195687002465839921, -70.01615807439628725 ) ) ;
#32656 = DIRECTION ( 'NONE',  ( 0.000000000000000000, 1.000000000000000000, 0.000000000000000000 ) ) ;
#32657 = CARTESIAN_POINT ( 'NONE',  ( 65.66434943752820175, 1.163675854572349788, -18.02570572091639889 ) ) ;
#32658 = ORIENTED_EDGE ( 'NONE', *, *, #27723, .F. ) ;
#32660 = EDGE_CURVE ( 'NONE', #26727, #28850, #30382, .T. ) ;
#32659 = CARTESIAN_POINT ( 'NONE',  ( 14.47836920878520139, -52.11833314967490338, -75.86497326479759806 ) ) ;
#32661 = CARTESIAN_POINT ( 'NONE',  ( 47.39033437818570604, -54.65766784492359420, -54.69850838941369631 ) ) ;
#32662 = EDGE_CURVE ( 'NONE', #24695, #42065, #43127, .T. ) ;
#32663 = CARTESIAN_POINT ( 'NONE',  ( 18.20462679473721224, -7.911091633304650372, -37.09100355881665934 ) ) ;
#32664 =( BOUNDED_CURVE ( )  B_SPLINE_CURVE ( 2, ( #47890, #27948, #18806 ),
 .UNSPECIFIED., .F., .T. ) 
 B_SPLINE_CURVE_WITH_KNOTS ( ( 3, 3 ),
 ( 0.2168422315598149963, 3.147551163863049783 ),
 .UNSPECIFIED. ) 
 CURVE ( )  GEOMETRIC_REPRESENTATION_ITEM ( )  RATIONAL_B_SPLINE_CURVE ( ( 1.000597593688320019, 1.004455541115450101, 1.003436844929990190 ) ) 
 REPRESENTATION_ITEM ( '' )  );
#32665 = CARTESIAN_POINT ( 'NONE',  ( 60.86245460095720716, -45.45535556830957802, -47.08538195706119467 ) ) ;
#32666 = CIRCLE ( 'NONE', #6749, 16.60961179679780031 ) ;
#32667 = CARTESIAN_POINT ( 'NONE',  ( 22.16267452853670150, -12.06226307891249938, -32.14999999999999858 ) ) ;
#32669 = AXIS2_PLACEMENT_3D ( 'NONE', #29570, #9669, #21698 ) ;
#32668 = DIRECTION ( 'NONE',  ( 0.000000000000000000, 1.000000000000000000, 0.000000000000000000 ) ) ;
#32670 = CARTESIAN_POINT ( 'NONE',  ( 11.75767683380609796, 34.19214141181279842, -18.01774807205339712 ) ) ;
#32672 = CARTESIAN_POINT ( 'NONE',  ( 23.83903794312202251, -17.68686302044806524, -73.59100117495633242 ) ) ;
#32671 = DIRECTION ( 'NONE',  ( 1.000000000000000000, 0.000000000000000000, 0.000000000000000000 ) ) ;
#32673 = DIRECTION ( 'NONE',  ( 0.000000000000000000, 1.000000000000000000, 0.000000000000000000 ) ) ;
#32674 = DIRECTION ( 'NONE',  ( 0.000000000000000000, -1.000000000000000000, 0.000000000000000000 ) ) ;
#32675 = CARTESIAN_POINT ( 'NONE',  ( 48.38771979903820153, 22.91125108602309979, -54.79794912714500299 ) ) ;
#32676 = ORIENTED_EDGE ( 'NONE', *, *, #20808, .F. ) ;
#32677 = CARTESIAN_POINT ( 'NONE',  ( 23.09258150619950101, -16.76502807425499952, -58.89926144005930553 ) ) ;
#32678 = ORIENTED_EDGE ( 'NONE', *, *, #39970, .T. ) ;
#32679 = DIRECTION ( 'NONE',  ( 0.000000000000000000, -1.000000000000000000, 0.000000000000000000 ) ) ;
#32680 = CARTESIAN_POINT ( 'NONE',  ( 72.13393739769620083, -30.11618894467929763, -20.65000000000000213 ) ) ;
#32681 = DIRECTION ( 'NONE',  ( 0.000000000000000000, 0.000000000000000000, -1.000000000000000000 ) ) ;
#32683 = CARTESIAN_POINT ( 'NONE',  ( 53.64943959690070585, 17.55132301322400323, -26.88176027460789896 ) ) ;
#32682 = CARTESIAN_POINT ( 'NONE',  ( 82.63159810076149370, 13.83598294973969978, -46.43844420537269713 ) ) ;
#32684 = CARTESIAN_POINT ( 'NONE',  ( 9.657775751103418571, -18.40937512247450059, -67.32320539224699019 ) ) ;
#32685 = CARTESIAN_POINT ( 'NONE',  ( 10.86720897088954807, 33.73900725339473894, -17.53558621447852062 ) ) ;
#32686 = CARTESIAN_POINT ( 'NONE',  ( 55.00845962336969563, -45.68083797646840338, -15.68178826579010021 ) ) ;
#32687 = EDGE_CURVE ( 'NONE', #2182, #33090, #4434, .T. ) ;
#32688 = CARTESIAN_POINT ( 'NONE',  ( 15.09849001458553097, -23.52720104044158944, -80.33399924191861885 ) ) ;
#32689 = ORIENTED_EDGE ( 'NONE', *, *, #7096, .F. ) ;
#32690 = ADVANCED_FACE ( 'NONE', ( #51424 ), #43561, .T. ) ;
#32691 = VERTEX_POINT ( 'NONE', #10560 ) ;
#32692 = CARTESIAN_POINT ( 'NONE',  ( 11.70209409419700108, -65.10125953154968670, -16.68277806566640109 ) ) ;
#32693 = CARTESIAN_POINT ( 'NONE',  ( 11.35901696209509915, 33.72246011924219289, -46.58143593047419984 ) ) ;
#32694 = LINE ( 'NONE', #487, #42446 ) ;
#32695 = CARTESIAN_POINT ( 'NONE',  ( 48.12000955664969837, -54.05113525397209884, -53.67196250754390974 ) ) ;
#32696 = CARTESIAN_POINT ( 'NONE',  ( 18.13393739769639978, 6.292713355527299157, -54.64999999999999858 ) ) ;
#32697 = ORIENTED_EDGE ( 'NONE', *, *, #7176, .T. ) ;
#32698 = CARTESIAN_POINT ( 'NONE',  ( 15.09830194314797147, -7.705199573743128028, -74.96596846305294548 ) ) ;
#32699 = CARTESIAN_POINT ( 'NONE',  ( 57.13928881360590140, 14.62761254858610016, -26.25285887909490157 ) ) ;
#32700 = CARTESIAN_POINT ( 'NONE',  ( 18.20461530425851038, -23.32128950267136247, -59.92435972222848051 ) ) ;
#32701 = CARTESIAN_POINT ( 'NONE',  ( 22.90093739769620029, -15.61618894467913243, -28.45282021618999835 ) ) ;
#32702 = CARTESIAN_POINT ( 'NONE',  ( 51.00677944403759767, -50.85929860725079266, -76.14999999999999147 ) ) ;
#32703 = CARTESIAN_POINT ( 'NONE',  ( 22.23620501646714587, -53.91985561452059272, -34.73809820100315449 ) ) ;
#32704 = AXIS2_PLACEMENT_3D ( 'NONE', #10158, #42129, #18012 ) ;
#32705 = EDGE_LOOP ( 'NONE', ( #43522, #2887, #37653, #24784, #34303, #11721 ) ) ;
#32706 = CARTESIAN_POINT ( 'NONE',  ( 55.69968854544299575, -46.18870594509260741, -25.38063974465979911 ) ) ;
#32708 = CYLINDRICAL_SURFACE ( 'NONE', #27571, 6.766999999999998572 ) ;
#32707 = CIRCLE ( 'NONE', #33557, 1.416232040419838523 ) ;
#32709 = ORIENTED_EDGE ( 'NONE', *, *, #5914, .T. ) ;
#32710 = FACE_OUTER_BOUND ( 'NONE', #4055, .T. ) ;
#32711 = CARTESIAN_POINT ( 'NONE',  ( 2.458146360389370511, -25.65221394861527671, -34.79644291222910368 ) ) ;
#32712 = CARTESIAN_POINT ( 'NONE',  ( 23.18808933907469694, -12.17692382128999817, -31.86811205682530002 ) ) ;
#32713 = CARTESIAN_POINT ( 'NONE',  ( 14.21286514218139807, -51.12296065175440418, -22.50824227891619955 ) ) ;
#32714 = CARTESIAN_POINT ( 'NONE',  ( 55.50650517420189800, 19.65167480108070208, -75.18850971831560059 ) ) ;
#32715 = CARTESIAN_POINT ( 'NONE',  ( 47.50309824425850280, -54.59962336152860019, -74.14999999999999147 ) ) ;
#32716 = ORIENTED_EDGE ( 'NONE', *, *, #29719, .T. ) ;
#32717 = CYLINDRICAL_SURFACE ( 'NONE', #1919, 0.4999999999999982236 ) ;
#32718 = CARTESIAN_POINT ( 'NONE',  ( 16.23075547080119918, -8.166536599377129946, -67.73679393810499505 ) ) ;
#32719 = CARTESIAN_POINT ( 'NONE',  ( 52.84318129818419862, -49.69161783228769735, -48.97012305832240031 ) ) ;
#32720 = FACE_OUTER_BOUND ( 'NONE', #22701, .T. ) ;
#32721 = CARTESIAN_POINT ( 'NONE',  ( 24.04475233726670780, -15.61618925176752271, -59.50766149565701113 ) ) ;
#32723 = EDGE_CURVE ( 'NONE', #12924, #25427, #42794, .T. ) ;
#32722 = CARTESIAN_POINT ( 'NONE',  ( 47.43599255124780001, 23.40374485785099878, -74.14999585054489728 ) ) ;
#32724 = DIRECTION ( 'NONE',  ( 0.8933039976646232061, -0.3805134419104956311, 0.2392017731577900652 ) ) ;
#32725 = CARTESIAN_POINT ( 'NONE',  ( 56.53717807884549984, 16.48612042830059821, -47.91220710008310135 ) ) ;
#32726 = DIRECTION ( 'NONE',  ( -1.000000000000000000, 0.000000000000000000, 0.000000000000000000 ) ) ;
#32727 = CARTESIAN_POINT ( 'NONE',  ( 20.28352806221460014, -22.74104818079599966, -79.83979650029888830 ) ) ;
#32728 = DIRECTION ( 'NONE',  ( 0.000000000000000000, -1.000000000000000000, 0.000000000000000000 ) ) ;
#32729 = CARTESIAN_POINT ( 'NONE',  ( 16.13393739769620083, -45.61618894467940066, -49.33749999999999858 ) ) ;
#32730 = CARTESIAN_POINT ( 'NONE',  ( 63.18291598250529262, 1.096305581841150012, -68.96938879548969226 ) ) ;
#32731 = CARTESIAN_POINT ( 'NONE',  ( 61.57009771359940231, 13.89954599885069975, -46.37201592743719658 ) ) ;
#32732 = CARTESIAN_POINT ( 'NONE',  ( 23.83903698041244823, -13.54551011926608162, -79.42433689193339319 ) ) ;
#32733 = CARTESIAN_POINT ( 'NONE',  ( 12.78938691692110119, -63.51980981231629642, -45.78213823142910854 ) ) ;
#32734 = ORIENTED_EDGE ( 'NONE', *, *, #37738, .T. ) ;
#32735 = AXIS2_PLACEMENT_3D ( 'NONE', #51268, #15365, #31320 ) ;
#32736 = CARTESIAN_POINT ( 'NONE',  ( 53.42159007590120012, -49.35880756780849765, -48.88221812793829457 ) ) ;
#32737 = AXIS2_PLACEMENT_3D ( 'NONE', #43813, #20203, #16030 ) ;
#32738 = CARTESIAN_POINT ( 'NONE',  ( 61.31134020973939869, -45.11617949509319203, -27.05924974616770129 ) ) ;
#32739 = DIRECTION ( 'NONE',  ( 0.000000000000000000, 1.000000000000000000, 0.000000000000000000 ) ) ;
#32740 = CARTESIAN_POINT ( 'NONE',  ( 56.83358511926749657, 14.76423303200390080, -26.24603876820060222 ) ) ;
#32741 = CIRCLE ( 'NONE', #25245, 24.00000000000000000 ) ;
#32742 = CARTESIAN_POINT ( 'NONE',  ( 12.57343482522869849, -21.70432331639599965, -39.12126593359850091 ) ) ;
#32743 = CARTESIAN_POINT ( 'NONE',  ( 50.72974176855199602, 18.26067442992610168, -76.22250671056579563 ) ) ;
#32744 = CARTESIAN_POINT ( 'NONE',  ( 53.39267832350149945, 18.14114278012100101, -48.88675587074509821 ) ) ;
#32745 = CARTESIAN_POINT ( 'NONE',  ( 71.36046776202630326, 0.9940423591679348192, -70.69940569364969463 ) ) ;
#32746 = CARTESIAN_POINT ( 'NONE',  ( 83.89200044194980421, -48.61618894467930119, -53.92796738110899923 ) ) ;
#32747 = CARTESIAN_POINT ( 'NONE',  ( 47.26511634744682766, 22.82442341443599432, -75.56574704403116982 ) ) ;
#32748 = ORIENTED_EDGE ( 'NONE', *, *, #2973, .T. ) ;
#32749 = DIRECTION ( 'NONE',  ( 1.000000000000000000, 0.000000000000000000, 0.000000000000000000 ) ) ;
#32750 = CARTESIAN_POINT ( 'NONE',  ( 12.02727910879949924, -21.83246210764250250, -59.75317579121929867 ) ) ;
#32751 = EDGE_CURVE ( 'NONE', #25200, #30141, #17428, .T. ) ;
#32752 = CARTESIAN_POINT ( 'NONE',  ( 72.99182123261159916, 1.264489825601020190, -68.89055226466270199 ) ) ;
#32753 = CARTESIAN_POINT ( 'NONE',  ( 47.60151701969190441, -54.52169367247979892, -54.71364311436219907 ) ) ;
#32754 = DIRECTION ( 'NONE',  ( 0.000000000000000000, -1.000000000000000000, 0.000000000000000000 ) ) ;
#32755 = DIRECTION ( 'NONE',  ( 1.000000000000000000, 2.460964292799963328E-14, 0.000000000000000000 ) ) ;
#32756 = CARTESIAN_POINT ( 'NONE',  ( 58.72865206045799624, 17.58198988844250010, -51.18437690886020164 ) ) ;
#32757 = CARTESIAN_POINT ( 'NONE',  ( 71.25608535201600091, 1.369535599030039963, -60.93144909420819744 ) ) ;
#32758 = CARTESIAN_POINT ( 'NONE',  ( 64.43393739769619799, 10.88381105532070059, -64.04999999999999716 ) ) ;
#32759 = CARTESIAN_POINT ( 'NONE',  ( 71.83998266832981017, 1.442158793902750036, -61.28605443723469648 ) ) ;
#32760 = CARTESIAN_POINT ( 'NONE',  ( 24.04493739903013960, -15.61839112611826330, -71.50776123734669909 ) ) ;
#32761 = CARTESIAN_POINT ( 'NONE',  ( 65.23632417210519918, 1.383928098097870096, -70.33743540642140601 ) ) ;
#32762 = EDGE_LOOP ( 'NONE', ( #18039, #21521, #4422, #31396 ) ) ;
#32763 = ORIENTED_EDGE ( 'NONE', *, *, #36955, .F. ) ;
#32764 = DIRECTION ( 'NONE',  ( -0.4999999999999998890, 0.8660254037844387076, 0.000000000000000000 ) ) ;
#32765 = CARTESIAN_POINT ( 'NONE',  ( 57.77564497937559906, -3.116188944679349593, -20.65000000000000213 ) ) ;
#32766 = ORIENTED_EDGE ( 'NONE', *, *, #18025, .T. ) ;
#32767 = CARTESIAN_POINT ( 'NONE',  ( 11.83663345274839962, -65.04952236550880684, -45.42313153075849641 ) ) ;
#32768 = CARTESIAN_POINT ( 'NONE',  ( 17.01970826270887471, -8.849185036877550203, -69.99448858124149808 ) ) ;
#32769 = CARTESIAN_POINT ( 'NONE',  ( 54.35208312152495580, 19.95646783507805111, -75.41447387695721716 ) ) ;
#32770 = CARTESIAN_POINT ( 'NONE',  ( 53.70323219070949960, 19.53744653144449828, -76.35188078170320125 ) ) ;
#32771 = ORIENTED_EDGE ( 'NONE', *, *, #33887, .F. ) ;
#32772 = CARTESIAN_POINT ( 'NONE',  ( 84.44784216359251161, 11.88381105532070059, -47.47585302082339354 ) ) ;
#32773 = CARTESIAN_POINT ( 'NONE',  ( 20.26294502443843015, -10.18158913507981822, -72.15944758614480747 ) ) ;
#32774 = CARTESIAN_POINT ( 'NONE',  ( 17.16955165497868308, -7.705198479972275472, -35.04933352119421386 ) ) ;
#32775 = CARTESIAN_POINT ( 'NONE',  ( 11.97151152939560070, -22.73355720456560292, -38.46077722564559309 ) ) ;
#32776 = CARTESIAN_POINT ( 'NONE',  ( 22.88119099990498029, -15.08889120109404480, -56.42800610659730864 ) ) ;
#32777 = CARTESIAN_POINT ( 'NONE',  ( 41.82154896394096255, -37.59484916107987118, -81.21190131928830169 ) ) ;
#32778 = VERTEX_POINT ( 'NONE', #7399 ) ;
#32779 = AXIS2_PLACEMENT_3D ( 'NONE', #32313, #12429, #44400 ) ;
#32780 = CARTESIAN_POINT ( 'NONE',  ( 8.223340741289188571, -15.61635616670070092, -42.79233150823699816 ) ) ;
#32781 = CARTESIAN_POINT ( 'NONE',  ( 20.28421976646189862, -9.796066462810269826, -31.92983709734899378 ) ) ;
#32782 = AXIS2_PLACEMENT_3D ( 'NONE', #16940, #25289, #37107 ) ;
#32783 = CARTESIAN_POINT ( 'NONE',  ( 23.83903224035146096, -13.54548743036029990, -33.42433181708312162 ) ) ;
#32784 = EDGE_CURVE ( 'NONE', #15485, #5505, #29942, .T. ) ;
#32785 = CARTESIAN_POINT ( 'NONE',  ( 14.67008335555839871, 21.21781726285519909, -76.03742712147929694 ) ) ;
#32786 = EDGE_CURVE ( 'NONE', #16071, #34347, #16218, .T. ) ;
#32787 = CARTESIAN_POINT ( 'NONE',  ( 24.04474217745232068, -15.67622493691082575, -59.79474066186497794 ) ) ;
#32788 = EDGE_CURVE ( 'NONE', #1009, #32627, #8711, .T. ) ;
#32789 = LINE ( 'NONE', #48814, #28108 ) ;
#32790 = DIRECTION ( 'NONE',  ( -0.7071067811865475727, 0.000000000000000000, -0.7071067811865475727 ) ) ;
#32791 = ADVANCED_FACE ( 'NONE', ( #38861 ), #51169, .F. ) ;
#32792 = CARTESIAN_POINT ( 'NONE',  ( 15.03334340613479903, -7.444811241090149245, -54.96505214632239245 ) ) ;
#32793 = VERTEX_POINT ( 'NONE', #23098 ) ;
#32794 = CARTESIAN_POINT ( 'NONE',  ( 54.07078989395569835, -48.34239437814039775, -26.64548683062099954 ) ) ;
#32795 = CARTESIAN_POINT ( 'NONE',  ( 16.49314696554849746, -51.11618894325009421, -20.88058500138570039 ) ) ;
#32796 = CARTESIAN_POINT ( 'NONE',  ( 50.95939809116894992, -35.29322421015848477, -76.37898009206955408 ) ) ;
#32797 = CARTESIAN_POINT ( 'NONE',  ( 63.43393739769620510, 1.883811055320669947, -68.84999999999999432 ) ) ;
#32798 = DIRECTION ( 'NONE',  ( 2.806155971274087206E-29, 5.103645611290830066E-11, -1.000000000000000000 ) ) ;
#32799 = DIRECTION ( 'NONE',  ( 0.000000000000000000, 0.000000000000000000, -1.000000000000000000 ) ) ;
#32800 = VERTEX_POINT ( 'NONE', #50903 ) ;
#32801 = CARTESIAN_POINT ( 'NONE',  ( -10.86918838363719964, -42.36073152548370047, -6.289582464405770068 ) ) ;
#32802 = CARTESIAN_POINT ( 'NONE',  ( 47.46312990717009228, 23.37191056432249781, -54.66046005970299859 ) ) ;
#32803 = FACE_OUTER_BOUND ( 'NONE', #5161, .T. ) ;
#32804 = CARTESIAN_POINT ( 'NONE',  ( 63.14953303862429124, 0.9272522097098079286, -62.30994913869029972 ) ) ;
#32805 = CARTESIAN_POINT ( 'NONE',  ( 13.39951981361199884, 19.12481834425529925, -21.14252705510070030 ) ) ;
#32806 = CARTESIAN_POINT ( 'NONE',  ( 57.28958346807240787, -50.56274171085619429, -53.44848221258419585 ) ) ;
#32807 = CARTESIAN_POINT ( 'NONE',  ( 10.96947337815019985, 33.83317461693680173, -17.60046538709029917 ) ) ;
#32808 = CYLINDRICAL_SURFACE ( 'NONE', #7696, 14.50000000000000178 ) ;
#32809 = LINE ( 'NONE', #32290, #30065 ) ;
#32810 = CARTESIAN_POINT ( 'NONE',  ( 72.60391569211400054, 1.424120032878380071, -62.14639092277510457 ) ) ;
#32811 = CARTESIAN_POINT ( 'NONE',  ( 56.34619344238320338, -47.91446257689889165, -48.39186534203880541 ) ) ;
#32812 = CARTESIAN_POINT ( 'NONE',  ( 10.53341022709680352, -19.45603223815694349, -67.26142806095880644 ) ) ;
#32813 = CARTESIAN_POINT ( 'NONE',  ( 64.64662912975151698, 0.9425424353906030062, -60.76751081460630388 ) ) ;
#32814 = CARTESIAN_POINT ( 'NONE',  ( 17.36723430360029852, -52.99263752172900155, -76.14999999999999147 ) ) ;
#32815 = EDGE_CURVE ( 'NONE', #26843, #24834, #30962, .T. ) ;
#32816 = CARTESIAN_POINT ( 'NONE',  ( 33.53393739769619231, -15.61618894467929763, -6.649999999999999467 ) ) ;
#32817 = CARTESIAN_POINT ( 'NONE',  ( 19.54195158308641211, -9.703291134712584309, -48.11948821520955732 ) ) ;
#32818 = ORIENTED_EDGE ( 'NONE', *, *, #15458, .F. ) ;
#32819 = DIRECTION ( 'NONE',  ( -1.000000000000000000, 0.000000000000000000, 0.000000000000000000 ) ) ;
#32820 = CARTESIAN_POINT ( 'NONE',  ( 9.296310069140089283, 32.04080841894100473, -46.53012790981569680 ) ) ;
#32821 = VECTOR ( 'NONE', #47395, 1000.000000000000000 ) ;
#32822 = DIRECTION ( 'NONE',  ( 0.000000000000000000, -1.000000000000000000, 0.000000000000000000 ) ) ;
#32823 = CARTESIAN_POINT ( 'NONE',  ( 66.70613048662919198, -29.77145157328190095, -17.03146206158359988 ) ) ;
#32824 = ORIENTED_EDGE ( 'NONE', *, *, #15741, .T. ) ;
#32825 = CARTESIAN_POINT ( 'NONE',  ( 18.59700916488480260, 20.77210737664869811, -75.25165125838280744 ) ) ;
#32826 = ORIENTED_EDGE ( 'NONE', *, *, #28034, .T. ) ;
#32827 = ORIENTED_EDGE ( 'NONE', *, *, #3375, .F. ) ;
#32828 = ORIENTED_EDGE ( 'NONE', *, *, #47790, .T. ) ;
#32829 = CARTESIAN_POINT ( 'NONE',  ( 9.896201805643420002, -63.47691444275439920, -46.22391251453240102 ) ) ;
#32830 = CARTESIAN_POINT ( 'NONE',  ( 57.33492022655319431, -45.81309998369609815, -26.26997405205120018 ) ) ;
#32831 = CARTESIAN_POINT ( 'NONE',  ( 22.70811139964889946, -18.58208211393579745, -81.23899999999999011 ) ) ;
#32832 = CARTESIAN_POINT ( 'NONE',  ( 61.57627151792929965, 13.93414709175500121, -46.78392464288939578 ) ) ;
#32833 = VERTEX_POINT ( 'NONE', #47749 ) ;
#32834 = EDGE_CURVE ( 'NONE', #51359, #34653, #46186, .T. ) ;
#32835 = VERTEX_POINT ( 'NONE', #299 ) ;
#32836 = CARTESIAN_POINT ( 'NONE',  ( 46.63393739769619373, 7.878491304262099426, -34.64999999999999858 ) ) ;
#32837 = VERTEX_POINT ( 'NONE', #28317 ) ;
#32838 = DIRECTION ( 'NONE',  ( 0.000000000000000000, 0.000000000000000000, -1.000000000000000000 ) ) ;
#32839 = CARTESIAN_POINT ( 'NONE',  ( 60.91814615750740103, -46.16813708928359716, -48.29757979411370883 ) ) ;
#32840 = CARTESIAN_POINT ( 'NONE',  ( 10.01860311628955813, -55.14667356096284578, -46.10193818995475112 ) ) ;
#32841 = ORIENTED_EDGE ( 'NONE', *, *, #47809, .F. ) ;
#32842 = ORIENTED_EDGE ( 'NONE', *, *, #25486, .F. ) ;
#32843 = CARTESIAN_POINT ( 'NONE',  ( 51.13393739769620083, 19.38381105532069881, 16.85000000000000142 ) ) ;
#32844 = CARTESIAN_POINT ( 'NONE',  ( 27.13393739769620083, -15.61618894467929941, -20.58999999999999986 ) ) ;
#32845 = CARTESIAN_POINT ( 'NONE',  ( 75.02341226432500321, 13.88381331661629936, -15.00428186426339927 ) ) ;
#32846 = CARTESIAN_POINT ( 'NONE',  ( 50.07777262096480086, 14.74234056921910074, -12.37452011861049961 ) ) ;
#32847 = DIRECTION ( 'NONE',  ( 0.000000000000000000, 0.000000000000000000, -1.000000000000000000 ) ) ;
#32848 = CARTESIAN_POINT ( 'NONE',  ( -6.923399356429929874, 14.58998759983630045, -4.778090145611190387 ) ) ;
#32849 = AXIS2_PLACEMENT_3D ( 'NONE', #4666, #37415, #8348 ) ;
#32850 = VECTOR ( 'NONE', #37308, 999.9999999999998863 ) ;
#32851 = CARTESIAN_POINT ( 'NONE',  ( 12.99575412164399779, -21.93238755621440106, -63.49395944174919748 ) ) ;
#32852 = CARTESIAN_POINT ( 'NONE',  ( 55.54885310752610650, 14.75987100490110393, -16.75765343292357201 ) ) ;
#32853 = B_SPLINE_CURVE_WITH_KNOTS ( 'NONE', 3,
 ( #27464, #27207, #31640, #47659, #30618, #42961, #35853, #46901, #7827, #46642 ),
 .UNSPECIFIED., .F., .F.,
 ( 4, 2, 2, 2, 4 ),
 ( 0.000000000000000000, 0.06066521036188608773, 0.4651142842241269282, 0.7990341870335844199, 1.000000000000000000 ),
 .UNSPECIFIED. ) ;
#32854 = ADVANCED_FACE ( 'NONE', ( #4483 ), #1073, .T. ) ;
#32855 = CARTESIAN_POINT ( 'NONE',  ( 14.45395864162150090, -23.28198437387779762, -71.85617835341309956 ) ) ;
#32856 = EDGE_LOOP ( 'NONE', ( #32577, #19953, #41959, #27387 ) ) ;
#32857 = CARTESIAN_POINT ( 'NONE',  ( 18.11714455905759635, 1.361188710403589797, -35.02127583263639821 ) ) ;
#32858 = CARTESIAN_POINT ( 'NONE',  ( -11.10497851609540021, -41.90811128427360188, -5.474771920946119863 ) ) ;
#32859 = CARTESIAN_POINT ( 'NONE',  ( 12.36078803208969923, 34.13639577542789993, -46.58647024651509838 ) ) ;
#32860 = CARTESIAN_POINT ( 'NONE',  ( 72.12455669199449915, 1.010053820890680187, -70.13159119767701100 ) ) ;
#32861 = CARTESIAN_POINT ( 'NONE',  ( 41.30259114575395785, -39.68594778607436524, -79.69702892170657549 ) ) ;
#32862 = CARTESIAN_POINT ( 'NONE',  ( 18.86789271272390067, -51.78678247029300508, -15.81497036395479761 ) ) ;
#32863 = CARTESIAN_POINT ( 'NONE',  ( 11.03791300131472042, -9.515481636700208412, -64.78606741210316500 ) ) ;
#32864 = CARTESIAN_POINT ( 'NONE',  ( 46.97440157803860217, 23.10210390193510221, -75.47461176419869844 ) ) ;
#32865 = CARTESIAN_POINT ( 'NONE',  ( 49.62716556310680005, -53.64958197259959860, -54.74430167493650146 ) ) ;
#32866 = CYLINDRICAL_SURFACE ( 'NONE', #50711, 22.00000000000000355 ) ;
#32867 = AXIS2_PLACEMENT_3D ( 'NONE', #5644, #10345, #10083 ) ;
#32868 = B_SPLINE_CURVE_WITH_KNOTS ( 'NONE', 3,
 ( #7865, #47959, #22857, #14499, #15984, #18425 ),
 .UNSPECIFIED., .F., .F.,
 ( 4, 2, 4 ),
 ( 0.000000000000000000, 0.2487259972468401914, 0.4974519944936803828 ),
 .UNSPECIFIED. ) ;
#32869 = CARTESIAN_POINT ( 'NONE',  ( 24.04489541832924004, -15.64402584357523374, -33.50878528010039048 ) ) ;
#32870 = CARTESIAN_POINT ( 'NONE',  ( 18.86790574444290058, -51.78681982904430470, -74.14993593045390696 ) ) ;
#32872 = EDGE_CURVE ( 'NONE', #6443, #16420, #46313, .T. ) ;
#32871 = CARTESIAN_POINT ( 'NONE',  ( 18.09661853408499965, -22.39043738500940961, -71.25741468598400274 ) ) ;
#32873 = ORIENTED_EDGE ( 'NONE', *, *, #45865, .F. ) ;
#32874 = CARTESIAN_POINT ( 'NONE',  ( 10.07881066264659964, -11.27543618037340067, -40.26531874956899770 ) ) ;
#32875 = CARTESIAN_POINT ( 'NONE',  ( 64.39929874312750258, 1.394112346784160072, -61.21167439625769902 ) ) ;
#32876 = ORIENTED_EDGE ( 'NONE', *, *, #10245, .T. ) ;
#32877 = DIRECTION ( 'NONE',  ( 0.000000000000000000, 0.000000000000000000, -1.000000000000000000 ) ) ;
#32878 = CARTESIAN_POINT ( 'NONE',  ( 60.39410434858780263, -45.81892262575509989, -47.68307256904559921 ) ) ;
#32879 = CARTESIAN_POINT ( 'NONE',  ( 56.88339341544950400, 19.41749060555369866, -53.85640383776300411 ) ) ;
#32880 = CARTESIAN_POINT ( 'NONE',  ( 65.27736602627911111, 0.8838110553206759423, -60.94999999999999574 ) ) ;
#32882 = CARTESIAN_POINT ( 'NONE',  ( 14.06321080411807678, -23.32127667121109837, -78.37566353430301547 ) ) ;
#32881 = CARTESIAN_POINT ( 'NONE',  ( 43.55216548528601805, 8.684117711060597600, -68.82845419862523784 ) ) ;
#32883 = DIRECTION ( 'NONE',  ( 1.000000000000000000, -1.040313928821094058E-14, -2.593849395860594704E-12 ) ) ;
#32884 = DIRECTION ( 'NONE',  ( 0.000000000000000000, 0.000000000000000000, -1.000000000000000000 ) ) ;
#32885 = ORIENTED_EDGE ( 'NONE', *, *, #46932, .T. ) ;
#32886 = CARTESIAN_POINT ( 'NONE',  ( 83.67079303953970282, -45.04147143931179187, -47.45584445533860674 ) ) ;
#32887 = EDGE_LOOP ( 'NONE', ( #21364, #25755, #18032, #5155, #23542 ) ) ;
#32888 = VERTEX_POINT ( 'NONE', #35935 ) ;
#32889 = AXIS2_PLACEMENT_3D ( 'NONE', #41350, #5467, #21421 ) ;
#32890 = ORIENTED_EDGE ( 'NONE', *, *, #25106, .F. ) ;
#32891 = CARTESIAN_POINT ( 'NONE',  ( 61.57009771103250273, -45.13192389007129890, -46.37194711517049228 ) ) ;
#32892 = CARTESIAN_POINT ( 'NONE',  ( 52.56293433422980144, -49.86422820730079764, -48.47378032971909789 ) ) ;
#32893 = CARTESIAN_POINT ( 'NONE',  ( 52.91668460176483535, -50.26603313699760633, -77.24653538837539202 ) ) ;
#32894 = AXIS2_PLACEMENT_3D ( 'NONE', #50458, #14548, #13779 ) ;
#32895 = CARTESIAN_POINT ( 'NONE',  ( 76.39087184172302614, -15.49781190055006519, -12.75716859379809343 ) ) ;
#32896 = CARTESIAN_POINT ( 'NONE',  ( 54.60804605940690237, -51.56737606348759329, -53.98096760914360459 ) ) ;
#32897 = AXIS2_PLACEMENT_3D ( 'NONE', #33744, #28787, #41365 ) ;
#32898 = ORIENTED_EDGE ( 'NONE', *, *, #27181, .T. ) ;
#32899 = ADVANCED_FACE ( 'NONE', ( #31985, #28842, #28578, #31724, #12886, #32235, #24374, #44578, #24634 ), #44318, .T. ) ;
#32900 = EDGE_LOOP ( 'NONE', ( #30690, #25804, #6124, #16149 ) ) ;
#32901 = CARTESIAN_POINT ( 'NONE',  ( 8.223069265346360623, -15.61598766837350105, -56.50766849176299189 ) ) ;
#32902 = CARTESIAN_POINT ( 'NONE',  ( 56.84933713246299902, 19.42395819629489750, -53.71862199975780072 ) ) ;
#32903 = DIRECTION ( 'NONE',  ( 0.000000000000000000, -1.000000000000000000, 0.000000000000000000 ) ) ;
#32904 = EDGE_CURVE ( 'NONE', #1082, #26468, #14507, .T. ) ;
#32905 = CARTESIAN_POINT ( 'NONE',  ( 22.90135621376786901, -15.43173441932949252, -66.83850953173875098 ) ) ;
#32906 = CARTESIAN_POINT ( 'NONE',  ( 8.793990757808609615, -63.16307462209709911, -46.67050766270720175 ) ) ;
#32907 = CARTESIAN_POINT ( 'NONE',  ( 62.72656151416200743, 0.3176618421485369881, -17.00947622673330173 ) ) ;
#32908 = CARTESIAN_POINT ( 'NONE',  ( 10.72256940289631721, -11.45758012563586092, -53.66115420497921917 ) ) ;
#32909 = EDGE_CURVE ( 'NONE', #3546, #32127, #41838, .T. ) ;
#32910 = ORIENTED_EDGE ( 'NONE', *, *, #49883, .F. ) ;
#32911 = DIRECTION ( 'NONE',  ( 0.7071067811865656694, -0.7071067811865292541, 0.000000000000000000 ) ) ;
#32912 = CARTESIAN_POINT ( 'NONE',  ( 53.83004757226819947, -50.59959810400789593, -77.06233067710800810 ) ) ;
#32913 = CARTESIAN_POINT ( 'NONE',  ( 64.12516823571120028, -29.62180181437879867, -16.36303599707800061 ) ) ;
#32914 = CARTESIAN_POINT ( 'NONE',  ( 60.86304203775009825, 14.21967909778819994, -47.00282332578510847 ) ) ;
#32915 = CARTESIAN_POINT ( 'NONE',  ( 20.01403207936019868, -22.43759736617889899, -64.34787379290919773 ) ) ;
#32916 = LINE ( 'NONE', #48945, #28852 ) ;
#32917 = AXIS2_PLACEMENT_3D ( 'NONE', #44903, #8487, #32547 ) ;
#32918 = CARTESIAN_POINT ( 'NONE',  ( 41.06416708622129619, -44.69533140685900463, -5.123099498004579644 ) ) ;
#32919 = DIRECTION ( 'NONE',  ( 1.000000000000000000, 0.000000000000000000, 0.000000000000000000 ) ) ;
#32920 = CARTESIAN_POINT ( 'NONE',  ( 71.86947670220010309, 0.9561296872641460443, -60.95384405884320245 ) ) ;
#32921 = CARTESIAN_POINT ( 'NONE',  ( 66.85007720623511318, 1.883639210398676989, -20.46329710072452812 ) ) ;
#32922 = EDGE_CURVE ( 'NONE', #7985, #48450, #21178, .T. ) ;
#32923 = CARTESIAN_POINT ( 'NONE',  ( 64.26570060236220172, 1.437402181457050121, -69.93576135023748463 ) ) ;
#32924 = FACE_OUTER_BOUND ( 'NONE', #12493, .T. ) ;
#32925 = CARTESIAN_POINT ( 'NONE',  ( 65.89616026620871025, 0.1838254176425679898, -17.15308774369420064 ) ) ;
#32926 = EDGE_CURVE ( 'NONE', #43692, #39834, #9904, .T. ) ;
#32927 = ORIENTED_EDGE ( 'NONE', *, *, #2063, .F. ) ;
#32928 = CARTESIAN_POINT ( 'NONE',  ( 13.67954409772299940, -51.79024427787750540, -75.14498753492070193 ) ) ;
#32929 = CARTESIAN_POINT ( 'NONE',  ( 47.40680130986410745, -54.64269092349360335, -54.65527420080069732 ) ) ;
#32930 = CARTESIAN_POINT ( 'NONE',  ( 8.892600494392757682, 32.33025239210895307, -46.69114580434834494 ) ) ;
#32931 = VECTOR ( 'NONE', #35995, 1000.000000000000000 ) ;
#32932 = FACE_OUTER_BOUND ( 'NONE', #3809, .T. ) ;
#32933 = CIRCLE ( 'NONE', #8688, 5.251829701412241924 ) ;
#32934 = CARTESIAN_POINT ( 'NONE',  ( 22.89531333654768375, -11.40322039812424748, -55.33051484484766291 ) ) ;
#32935 = CARTESIAN_POINT ( 'NONE',  ( 23.36827203260559926, -17.23220949816419889, -32.14999999999999858 ) ) ;
#32936 = CARTESIAN_POINT ( 'NONE',  ( 57.47203281493852955, 13.89859585196675873, -25.53999618909873348 ) ) ;
#32937 = CARTESIAN_POINT ( 'NONE',  ( 47.67211062985429493, -54.52182009381669303, -55.16489596303849652 ) ) ;
#32939 = CARTESIAN_POINT ( 'NONE',  ( -11.32734370190460105, -41.88171845330919751, -6.430192534648670133 ) ) ;
#32938 = CARTESIAN_POINT ( 'NONE',  ( 14.05648280823140084, 19.92572429986999794, -22.83284003973019693 ) ) ;
#32940 = CARTESIAN_POINT ( 'NONE',  ( 56.30184842130790202, 19.39087536565910241, -52.97276602642149612 ) ) ;
#32941 = DIRECTION ( 'NONE',  ( 1.735698870208309265E-22, -1.000000000000000000, 1.376914871200490071E-11 ) ) ;
#32942 = CARTESIAN_POINT ( 'NONE',  ( 48.40807908919139635, 22.97456863626519663, -55.22863709201329385 ) ) ;
#32943 = ORIENTED_EDGE ( 'NONE', *, *, #41452, .F. ) ;
#32944 = CARTESIAN_POINT ( 'NONE',  ( 10.71149743639709939, -11.10623284283549950, -62.06801868260409094 ) ) ;
#32945 = ORIENTED_EDGE ( 'NONE', *, *, #6270, .F. ) ;
#32946 = CARTESIAN_POINT ( 'NONE',  ( 2.464092196720417238, -5.608468378986529501, -34.77490583097448251 ) ) ;
#32947 = DIRECTION ( 'NONE',  ( 0.8445663830063383504, 0.5331299045725292896, -0.04980089904888002073 ) ) ;
#32948 = CARTESIAN_POINT ( 'NONE',  ( 0.4253373362157371607, -22.38267892379094093, -35.06583844469808042 ) ) ;
#32950 = CARTESIAN_POINT ( 'NONE',  ( 54.23595886153059809, 16.77554233507499859, -26.19545990100650101 ) ) ;
#32949 = CARTESIAN_POINT ( 'NONE',  ( 82.79586663885601183, 13.79056004649610045, -46.43485061813930059 ) ) ;
#32951 = CARTESIAN_POINT ( 'NONE',  ( 12.84739398434249935, -9.375901203816159324, -67.79851897862879184 ) ) ;
#32952 = CYLINDRICAL_SURFACE ( 'NONE', #2807, 2.999999999999999112 ) ;
#32953 = CARTESIAN_POINT ( 'NONE',  ( 72.75396425272869294, 1.390208944942409985, -68.75457626026799574 ) ) ;
#32954 = DIRECTION ( 'NONE',  ( 1.000000000000000000, 0.000000000000000000, 0.000000000000000000 ) ) ;
#32955 = CONICAL_SURFACE ( 'NONE', #18755, 19.50000000000000000, 0.2449786631268651149 ) ;
#32956 = ORIENTED_EDGE ( 'NONE', *, *, #16508, .T. ) ;
#32957 = ORIENTED_EDGE ( 'NONE', *, *, #23825, .F. ) ;
#32958 = CARTESIAN_POINT ( 'NONE',  ( 11.84964338387410088, -64.94214987232159331, -16.34215248990359726 ) ) ;
#32959 = CARTESIAN_POINT ( 'NONE',  ( 11.09465806800830023, 32.35066555307069791, -44.35269109309979996 ) ) ;
#32960 = CARTESIAN_POINT ( 'NONE',  ( 18.15361292478090860, 19.88381105533058246, -15.68107046463052257 ) ) ;
#32961 = CARTESIAN_POINT ( 'NONE',  ( 49.83032669135840109, -52.82339107842129522, -53.07740273290610133 ) ) ;
#32962 = CARTESIAN_POINT ( 'NONE',  ( 0.1375711481831189409, -10.50541980564829814, -34.68474920830804820 ) ) ;
#32963 = VERTEX_POINT ( 'NONE', #37240 ) ;
#32964 = LINE ( 'NONE', #4950, #25950 ) ;
#32965 = CARTESIAN_POINT ( 'NONE',  ( 40.75465142538514840, 2.762490711761011575, -82.06602514716892927 ) ) ;
#32966 = ADVANCED_FACE ( 'NONE', ( #2109 ), #41947, .T. ) ;
#32967 = LINE ( 'NONE', #37184, #42371 ) ;
#32968 = AXIS2_PLACEMENT_3D ( 'NONE', #41464, #9766, #1379 ) ;
#32969 = CARTESIAN_POINT ( 'NONE',  ( 12.14979381587971830, -22.52870523912515566, -60.17435903463200475 ) ) ;
#32970 = DIRECTION ( 'NONE',  ( 1.000000000000000000, 0.000000000000000000, 0.000000000000000000 ) ) ;
#32971 = CARTESIAN_POINT ( 'NONE',  ( 50.75796709625730330, -50.55377401516400226, -76.14999999999999147 ) ) ;
#32972 = EDGE_CURVE ( 'NONE', #35688, #1476, #18646, .T. ) ;
#32973 = CARTESIAN_POINT ( 'NONE',  ( 16.13393739769620083, 31.59091783650714547, 11.14289321881345174 ) ) ;
#32974 = ORIENTED_EDGE ( 'NONE', *, *, #17837, .F. ) ;
#32975 = CARTESIAN_POINT ( 'NONE',  ( 68.13393739806078031, -1.166188945451896330, -42.15000000163579585 ) ) ;
#32976 = FACE_BOUND ( 'NONE', #26421, .T. ) ;
#32977 = ORIENTED_EDGE ( 'NONE', *, *, #13641, .T. ) ;
#32978 = CARTESIAN_POINT ( 'NONE',  ( 12.71214975072897779, -55.46957087202495984, -75.54211829845161219 ) ) ;
#32979 = CARTESIAN_POINT ( 'NONE',  ( 54.47259832750690123, -46.25232753665150653, -15.76422791930239953 ) ) ;
#32980 = CARTESIAN_POINT ( 'NONE',  ( 21.80161389069149891, -10.18809611409700011, -33.76936640235220466 ) ) ;
#32981 = CARTESIAN_POINT ( 'NONE',  ( 13.63913686917599932, -51.36033930440640205, -22.70105461358259902 ) ) ;
#32982 = CARTESIAN_POINT ( 'NONE',  ( 56.40190446271180491, 19.55626960565449934, -74.41752554396340713 ) ) ;
#32983 = CARTESIAN_POINT ( 'NONE',  ( 47.15880624984559688, -54.00277375082009712, -75.65761316843601492 ) ) ;
#32984 = ORIENTED_EDGE ( 'NONE', *, *, #7869, .F. ) ;
#32985 = CARTESIAN_POINT ( 'NONE',  ( 55.59479635141730114, 14.68315623537079873, -16.73302166087749754 ) ) ;
#32986 =( BOUNDED_CURVE ( )  B_SPLINE_CURVE ( 3, ( #31853, #35289, #51024, #20066 ),
 .UNSPECIFIED., .F., .T. ) 
 B_SPLINE_CURVE_WITH_KNOTS ( ( 4, 4 ),
 ( 1.053572925743754274, 1.570796326794900999 ),
 .UNSPECIFIED. ) 
 CURVE ( )  GEOMETRIC_REPRESENTATION_ITEM ( )  RATIONAL_B_SPLINE_CURVE ( ( 1.000000000000000000, 0.9778306343446276916, 0.9778306343446276916, 1.000000000000000000 ) ) 
 REPRESENTATION_ITEM ( '' )  );
#32987 = CARTESIAN_POINT ( 'NONE',  ( 56.94040705048700346, -50.34429464441200253, -52.81451654216659364 ) ) ;
#32988 = CARTESIAN_POINT ( 'NONE',  ( 21.47227334498080253, -20.22538852244909791, -33.07388991331939820 ) ) ;
#32989 = CARTESIAN_POINT ( 'NONE',  ( 0.03808610503981946921, -22.85048806984080372, -34.73334895013599777 ) ) ;
#32990 = EDGE_CURVE ( 'NONE', #14613, #1216, #5564, .T. ) ;
#32991 = AXIS2_PLACEMENT_3D ( 'NONE', #31242, #2451, #10846 ) ;
#32992 = CARTESIAN_POINT ( 'NONE',  ( 46.35275103504439898, 21.67755452994670406, -76.14999999999999147 ) ) ;
#32993 = ADVANCED_FACE ( 'NONE', ( #22005, #34056 ), #33804, .T. ) ;
#32994 = DIRECTION ( 'NONE',  ( 0.000000000000000000, -1.000000000000000000, 0.000000000000000000 ) ) ;
#32995 = B_SPLINE_CURVE_WITH_KNOTS ( 'NONE', 3,
 ( #47590, #23953, #43144, #4069, #23187, #35264, #43654, #51263, #27395, #20037, #7239, #36032, #39203, #7756, #15357, #15869, #16117, #32078, #43396, #19282, #28155, #3821, #31313, #47339, #40233, #44159 ),
 .UNSPECIFIED., .F., .F.,
 ( 4, 2, 2, 2, 2, 2, 2, 2, 2, 2, 2, 2, 4 ),
 ( 0.000000000000000000, 0.03967672352634984967, 0.1774997633214195625, 0.3374995499773481011, 0.4374994166373029070, 0.4999993332997746398, 0.5624992499622464281, 0.6380835170998415684, 0.6985509308099168146, 0.7590183445199933931, 0.8429308035155282930, 0.9771907379083839551, 1.000000000000000000 ),
 .UNSPECIFIED. ) ;
#32996 = CARTESIAN_POINT ( 'NONE',  ( 68.13393739845098196, -29.66618894603428203, -42.15000000287349735 ) ) ;
#32997 = CARTESIAN_POINT ( 'NONE',  ( 65.27736602627911111, 0.8838110553206759423, -70.34999999999999432 ) ) ;
#32998 = CARTESIAN_POINT ( 'NONE',  ( 18.14127191746197809, -49.61613219182720513, -83.14624708861497027 ) ) ;
#32999 = DIRECTION ( 'NONE',  ( 0.000000000000000000, 0.000000000000000000, -1.000000000000000000 ) ) ;
#33000 = CARTESIAN_POINT ( 'NONE',  ( 16.13393739769620083, -15.61618894467929941, -6.928362978644219794 ) ) ;
#33002 = CARTESIAN_POINT ( 'NONE',  ( 42.17665618391549742, -39.84915031662858809, -75.20399989164987176 ) ) ;
#33001 = CARTESIAN_POINT ( 'NONE',  ( -10.89882054044000093, 10.23933580255000031, -4.618747568469349751 ) ) ;
#33003 = CIRCLE ( 'NONE', #10442, 1.999999999999998668 ) ;
#33004 = DIRECTION ( 'NONE',  ( 0.000000000000000000, 0.000000000000000000, -1.000000000000000000 ) ) ;
#33005 = FACE_OUTER_BOUND ( 'NONE', #36076, .T. ) ;
#33006 = EDGE_LOOP ( 'NONE', ( #24382, #13857, #3222, #29179 ) ) ;
#33007 = CARTESIAN_POINT ( 'NONE',  ( 52.84630519521279979, -49.65262790780239754, -48.68178424806700377 ) ) ;
#33008 = DIRECTION ( 'NONE',  ( 0.000000000000000000, 0.000000000000000000, -1.000000000000000000 ) ) ;
#33009 = CARTESIAN_POINT ( 'NONE',  ( 24.04465550003185115, -15.68834717694893932, -65.79523427362767052 ) ) ;
#33010 = CARTESIAN_POINT ( 'NONE',  ( 57.48863382328549676, 14.20681801447659964, -26.08418812544719856 ) ) ;
#33011 = CARTESIAN_POINT ( 'NONE',  ( 18.51000033465340167, -22.25673738164740101, -34.84344365616309602 ) ) ;
#33012 = CARTESIAN_POINT ( 'NONE',  ( 51.16024193372230400, 19.49271328425620098, -76.16561533977029796 ) ) ;
#33013 = CARTESIAN_POINT ( 'NONE',  ( 52.65923532209550473, 18.54112759137870015, -48.49071726774990054 ) ) ;
#33014 = CARTESIAN_POINT ( 'NONE',  ( 71.08986881540380409, 1.373356196620459935, -70.43126475061649217 ) ) ;
#33015 = DIRECTION ( 'NONE',  ( -1.000000000000000000, -1.791661345120054866E-29, -4.486507500526829843E-12 ) ) ;
#33016 = CARTESIAN_POINT ( 'NONE',  ( 69.11293209371449109, -43.39700965238730390, -11.59160171341740053 ) ) ;
#33017 = ORIENTED_EDGE ( 'NONE', *, *, #50037, .T. ) ;
#33018 = CARTESIAN_POINT ( 'NONE',  ( 22.50231163579990223, -19.48277707182389662, -79.24103283286959254 ) ) ;
#33019 = ORIENTED_EDGE ( 'NONE', *, *, #7898, .F. ) ;
#33020 = CARTESIAN_POINT ( 'NONE',  ( 73.07509570698499601, 0.9325382164350239922, -69.05375146239639150 ) ) ;
#33021 = CARTESIAN_POINT ( 'NONE',  ( 47.45236065713989859, -54.62711186455120327, -54.90161485602320113 ) ) ;
#33022 = CARTESIAN_POINT ( 'NONE',  ( 24.03633545123255644, -15.23418074785793763, -49.77695913693929697 ) ) ;
#33023 = CARTESIAN_POINT ( 'NONE',  ( 30.13393739769619728, -38.61618894467930119, -84.65000000000000568 ) ) ;
#33024 = CARTESIAN_POINT ( 'NONE',  ( 56.95284895653189494, 18.93591985592150095, -52.58138290995459840 ) ) ;
#33025 = CARTESIAN_POINT ( 'NONE',  ( 52.94585586128479093, 18.36771476006709847, -48.75076952771310346 ) ) ;
#33026 = CARTESIAN_POINT ( 'NONE',  ( 46.63499162694400724, 7.878850272075009542, -34.64999999999999858 ) ) ;
#33027 = CARTESIAN_POINT ( 'NONE',  ( 71.85972712066590873, 1.428542319231199897, -61.26680764775160526 ) ) ;
#33028 = CARTESIAN_POINT ( 'NONE',  ( 15.13522224570046149, -17.17987958086359512, -34.79644660940672907 ) ) ;
#33029 = CARTESIAN_POINT ( 'NONE',  ( 65.00022493107950083, 0.9952464559119579279, -70.75693755662150863 ) ) ;
#33030 = VERTEX_POINT ( 'NONE', #30129 ) ;
#33031 = ORIENTED_EDGE ( 'NONE', *, *, #2055, .F. ) ;
#33032 = CIRCLE ( 'NONE', #44757, 9.999999999999998224 ) ;
#33033 = CARTESIAN_POINT ( 'NONE',  ( 8.975750908825888885, -63.26599253637061082, -46.63326651989199689 ) ) ;
#33034 = EDGE_CURVE ( 'NONE', #43399, #20583, #10575, .T. ) ;
#33035 = FACE_OUTER_BOUND ( 'NONE', #16606, .T. ) ;
#33036 = ORIENTED_EDGE ( 'NONE', *, *, #42182, .T. ) ;
#33037 = CARTESIAN_POINT ( 'NONE',  ( 22.89189869931721688, -14.41738426556256059, -72.79077680364316905 ) ) ;
#33038 = CARTESIAN_POINT ( 'NONE',  ( 68.38971107317580334, -30.11618894467929763, -18.15384911698640025 ) ) ;
#33039 = CARTESIAN_POINT ( 'NONE',  ( 55.20064104123608928, 19.79077351844777510, -75.15544575098610380 ) ) ;
#33040 = CARTESIAN_POINT ( 'NONE',  ( 53.80070914189850129, 19.45344997228420070, -76.57022543143750681 ) ) ;
#33041 = ORIENTED_EDGE ( 'NONE', *, *, #41812, .T. ) ;
#33042 = CARTESIAN_POINT ( 'NONE',  ( 59.34499803081109803, -3.116188944679349593, -15.68015151901639825 ) ) ;
#33043 = CARTESIAN_POINT ( 'NONE',  ( 42.31744474875747386, 6.441884423166124307, -78.73246318642024733 ) ) ;
#33044 = CARTESIAN_POINT ( 'NONE',  ( 20.11802429440930595, -8.703639022759114496, -43.45903450409944213 ) ) ;
#33045 = B_SPLINE_SURFACE_WITH_KNOTS ( 'NONE', 3, 3, ( 
 ( #21533, #21017, #9253, #41208, #37278, #13446, #37530, #1634, #17624, #33594, #49608, #14722, #30692, #34621 ),
 ( #46714, #27023, #10799, #30429, #26758, #3190, #30175, #2929, #14205, #46195, #46454, #42771, #6871, #50625 ),
 ( #39097, #43030, #22045, #50110, #6603, #26241, #18133, #22820, #18384, #38580, #22564, #45925, #42249, #41990 ),
 ( #6091, #7127, #26498, #38841, #23079, #6348, #18900, #10542, #30942, #2674, #22306, #38314, #34884, #42514 ),
 ( #50884, #46973, #14976, #18647, #11056, #14460, #2400, #10279, #34359, #19163, #35140, #50376, #51145, #15243 ),
 ( #38058, #10015, #34095, #25976, #2153, #7639, #16006, #43789, #47728, #4462, #31703, #31963, #31453, #7890 ),
 ( #4206, #47479, #11833, #24090, #47224, #23326, #35671, #19673, #3705, #51655, #12084, #12331, #7377, #15749 ),
 ( #27279, #8145, #39351, #19423, #27793, #35403, #11571, #28038, #44043, #23836, #20431, #39858, #51399, #47984 ),
 ( #40112, #27533, #11314, #32213, #20178, #3962, #19923, #35916, #24351, #36168, #36419, #48237, #31193, #28291 ),
 ( #276, #44295, #527, #43539, #43288, #3450, #15499, #8403, #40365, #23584, #39602, #49282, #49541, #44557 ) ),
 .UNSPECIFIED., .F., .F., .F.,
 ( 4, 1, 1, 1, 1, 1, 1, 4 ),
 ( 4, 2, 2, 2, 2, 2, 4 ),
 ( -0.0003239663523781590088, 0.1428571428571430157, 0.2857142857142860315, 0.4285714285714289917, 0.5714285714285709528, 0.7142857142857139685, 0.8571428571428569843, 1.000060558257379828 ),
 ( -0.7975921375522809775, -0.7173344096180139795, -0.5738675276944109616, -0.5021340867326099522, -0.3873605811937279597, -0.2037229723315160113, 0.0003085036975347379886 ),
 .UNSPECIFIED. ) ;
#33046 = CARTESIAN_POINT ( 'NONE',  ( 24.00223941041499742, -18.08044207546359772, -55.88894205964189865 ) ) ;
#33047 = DIRECTION ( 'NONE',  ( -2.027310999999999893E-13, 2.567767000000000059E-13, 1.000000000000000000 ) ) ;
#33048 = CARTESIAN_POINT ( 'NONE',  ( 41.61626771661330082, -37.56081407618439982, -82.23834840541459812 ) ) ;
#33049 = EDGE_LOOP ( 'NONE', ( #30884, #1725, #10511, #2503 ) ) ;
#33050 = EDGE_CURVE ( 'NONE', #37879, #28142, #5787, .T. ) ;
#33051 = CARTESIAN_POINT ( 'NONE',  ( 11.01003601656879916, -63.61865847005719843, -24.02609861887260223 ) ) ;
#33052 = CARTESIAN_POINT ( 'NONE',  ( 14.51556075300879911, -22.88857169320650087, -40.80235737647439720 ) ) ;
#33053 = CARTESIAN_POINT ( 'NONE',  ( 41.16398077517839482, 14.31303017726370008, -6.123772754722979883 ) ) ;
#33054 = ADVANCED_FACE ( 'NONE', ( #9971 ), #7337, .T. ) ;
#33055 = ADVANCED_FACE ( 'NONE', ( #11272 ), #50682, .T. ) ;
#33056 = CARTESIAN_POINT ( 'NONE',  ( 14.34756424442590017, 21.20322725566390076, -75.94942944171690158 ) ) ;
#33057 = CARTESIAN_POINT ( 'NONE',  ( -30.36606260230379917, -53.11618894467930119, 11.84999999999999964 ) ) ;
#33058 = CARTESIAN_POINT ( 'NONE',  ( 82.45627759125989087, -45.09272112584100256, -46.38986626917129996 ) ) ;
#33059 = B_SPLINE_CURVE_WITH_KNOTS ( 'NONE', 3,
 ( #1191, #36827, #44436, #4592, #32871, #8798, #8544, #23971, #39995, #663 ),
 .UNSPECIFIED., .F., .F.,
 ( 4, 1, 1, 1, 1, 1, 1, 4 ),
 ( 0.5000020751347326042, 0.5466795889596607338, 0.6258985200233790902, 0.7051174510869482326, 0.7843363821506665889, 0.8635553132142266275, 0.9427742442777956589, 1.000000000000000000 ),
 .UNSPECIFIED. ) ;
#33060 = CARTESIAN_POINT ( 'NONE',  ( 21.28041071868149814, -9.174408673251130963, -53.22223566292279173 ) ) ;
#33061 = ORIENTED_EDGE ( 'NONE', *, *, #46807, .F. ) ;
#33062 = CARTESIAN_POINT ( 'NONE',  ( 54.24920814692630699, -48.27160202174960091, -26.73053837092809815 ) ) ;
#33063 = FACE_OUTER_BOUND ( 'NONE', #13248, .T. ) ;
#33064 = CARTESIAN_POINT ( 'NONE',  ( 23.04647698446151338, -19.60028975017581132, -63.95900002351130809 ) ) ;
#33065 = CARTESIAN_POINT ( 'NONE',  ( 17.37116791007819927, -8.672715762353169211, -52.40330909284259775 ) ) ;
#33066 = CARTESIAN_POINT ( 'NONE',  ( -8.866062602303800944, -15.61618894467929586, 4.450000000000000178 ) ) ;
#33067 = CIRCLE ( 'NONE', #13825, 3.799999999999999378 ) ;
#33068 = ORIENTED_EDGE ( 'NONE', *, *, #31046, .F. ) ;
#33069 = CARTESIAN_POINT ( 'NONE',  ( -8.369583062334038814, -44.67542189550749754, -5.381608453275170234 ) ) ;
#33070 = CARTESIAN_POINT ( 'NONE',  ( 47.24879073443120348, 23.52399838237280250, -54.63316666300269731 ) ) ;
#33071 = DIRECTION ( 'NONE',  ( -1.000000000000000000, 0.000000000000000000, 0.000000000000000000 ) ) ;
#33072 = CARTESIAN_POINT ( 'NONE',  ( 63.33772283987349283, 1.326578174762029994, -62.47191694777300341 ) ) ;
#33073 = CYLINDRICAL_SURFACE ( 'NONE', #40717, 0.4999999999999990008 ) ;
#33074 = CARTESIAN_POINT ( 'NONE',  ( 11.56756857248330128, 34.11390478956230510, -17.53311478114069999 ) ) ;
#33075 = FACE_OUTER_BOUND ( 'NONE', #25031, .T. ) ;
#33076 = CARTESIAN_POINT ( 'NONE',  ( -15.33935108854907625, 24.23791302157028227, 10.84999999999999964 ) ) ;
#33077 = CARTESIAN_POINT ( 'NONE',  ( 72.63889986537131449, 1.416242794301129981, -62.22702189776489945 ) ) ;
#33078 = CARTESIAN_POINT ( 'NONE',  ( 55.61561331844040268, -48.29731251153899763, -48.56918272874399634 ) ) ;
#33079 = B_SPLINE_CURVE_WITH_KNOTS ( 'NONE', 3,
 ( #2924, #50877, #47473, #7122, #30937, #22814 ),
 .UNSPECIFIED., .F., .F.,
 ( 4, 2, 4 ),
 ( 0.03318971727292711893, 0.03563426461091390163, 0.06411833789063960121 ),
 .UNSPECIFIED. ) ;
#33080 = FACE_OUTER_BOUND ( 'NONE', #16941, .T. ) ;
#33081 = CARTESIAN_POINT ( 'NONE',  ( 53.50274481840529717, 20.58623994349600039, -53.37071925176099541 ) ) ;
#33082 = CARTESIAN_POINT ( 'NONE',  ( 12.14985869000924801, -8.703635950884679673, -77.12566379575649478 ) ) ;
#33083 = VERTEX_POINT ( 'NONE', #31832 ) ;
#33084 = DIRECTION ( 'NONE',  ( 0.000000000000000000, 0.000000000000000000, 1.000000000000000000 ) ) ;
#33085 = CARTESIAN_POINT ( 'NONE',  ( 10.14913760601130122, 32.10609558527020369, -45.99399621147029649 ) ) ;
#33086 = CARTESIAN_POINT ( 'NONE',  ( 16.13393739769620083, -15.61618894467929941, -32.14999999999999858 ) ) ;
#33087 = CARTESIAN_POINT ( 'NONE',  ( 66.55656304324030259, -30.20673539474010028, -16.96067054740260005 ) ) ;
#33088 = VERTEX_POINT ( 'NONE', #24477 ) ;
#33089 = CARTESIAN_POINT ( 'NONE',  ( 17.77572303879259863, 20.43782862716600235, -75.53341961486960088 ) ) ;
#33090 = VERTEX_POINT ( 'NONE', #11955 ) ;
#33091 = VERTEX_POINT ( 'NONE', #32599 ) ;
#33092 = CARTESIAN_POINT ( 'NONE',  ( 47.77526208095149940, 23.24550361938759835, -55.21131733320120105 ) ) ;
#33093 = EDGE_CURVE ( 'NONE', #32046, #20864, #12202, .T. ) ;
#33094 = ORIENTED_EDGE ( 'NONE', *, *, #45058, .F. ) ;
#33095 = CARTESIAN_POINT ( 'NONE',  ( 12.11535881846170071, -65.31089811698159053, -46.92786770476139679 ) ) ;
#33096 = CARTESIAN_POINT ( 'NONE',  ( 56.47981878976860060, -46.01152027889720131, -26.17847996949780054 ) ) ;
#33097 = CARTESIAN_POINT ( 'NONE',  ( 20.89839241790010149, -20.73495673888379898, -81.23899999999999011 ) ) ;
#33098 = EDGE_CURVE ( 'NONE', #45437, #814, #4331, .T. ) ;
#33099 = CARTESIAN_POINT ( 'NONE',  ( 61.61685004883869965, 13.90101642484820132, -46.58069093359240043 ) ) ;
#33100 = EDGE_CURVE ( 'NONE', #37257, #22022, #20554, .T. ) ;
#33101 = CARTESIAN_POINT ( 'NONE',  ( 9.366668810525878186, -15.61604052661200015, -35.45282021618999835 ) ) ;
#33102 = ORIENTED_EDGE ( 'NONE', *, *, #2403, .T. ) ;
#33103 = LINE ( 'NONE', #8505, #25131 ) ;
#33104 = CARTESIAN_POINT ( 'NONE',  ( 17.35001377175326098, -22.56339827118826591, -35.29201998310100663 ) ) ;
#33105 = VERTEX_POINT ( 'NONE', #8788 ) ;
#33106 = CARTESIAN_POINT ( 'NONE',  ( 45.64758691443690708, -45.19790785473080064, -8.164367006753829870 ) ) ;
#33107 = AXIS2_PLACEMENT_3D ( 'NONE', #18064, #14134, #10729 ) ;
#33108 = CARTESIAN_POINT ( 'NONE',  ( 16.13393739769620083, -15.61618894467929941, -10.44999999999999929 ) ) ;
#33109 = DIRECTION ( 'NONE',  ( 0.000000000000000000, 0.000000000000000000, -1.000000000000000000 ) ) ;
#33110 = EDGE_LOOP ( 'NONE', ( #25401, #31239 ) ) ;
#33111 = ORIENTED_EDGE ( 'NONE', *, *, #5169, .T. ) ;
#33112 = LINE ( 'NONE', #32325, #49290 ) ;
#33113 = CARTESIAN_POINT ( 'NONE',  ( 46.75888556483590008, -53.81317836377680663, -75.90771320283761270 ) ) ;
#33114 = CARTESIAN_POINT ( 'NONE',  ( 66.62633200496509289, 13.73060551161930043, -11.96361206954319911 ) ) ;
#33115 = CARTESIAN_POINT ( 'NONE',  ( 46.25788900357310496, 14.69397481452669929, -9.684285679222321974 ) ) ;
#33116 = CIRCLE ( 'NONE', #39025, 10.00000000000000888 ) ;
#33117 = EDGE_CURVE ( 'NONE', #22647, #33533, #48811, .T. ) ;
#33118 = DIRECTION ( 'NONE',  ( -0.8224686640529098591, 0.3976080002595605012, -0.4067593573362696113 ) ) ;
#33119 = CARTESIAN_POINT ( 'NONE',  ( -8.908994694087390087, 12.97547407152449850, -5.435440242544679279 ) ) ;
#33120 = CARTESIAN_POINT ( 'NONE',  ( 10.36088797006879858, -19.66766515473189969, -63.65239730387659023 ) ) ;
#33121 = CARTESIAN_POINT ( 'NONE',  ( 59.58068192400040175, 13.98218772109100172, -26.37874264201060015 ) ) ;
#33122 = CARTESIAN_POINT ( 'NONE',  ( 15.40474582320469921, -23.42996062235669896, -75.81712490659418791 ) ) ;
#33123 = ORIENTED_EDGE ( 'NONE', *, *, #352, .F. ) ;
#33124 = CONICAL_SURFACE ( 'NONE', #2180, 0.6299999999999998934, 0.7853981633974476129 ) ;
#33125 = CARTESIAN_POINT ( 'NONE',  ( 53.55347996450739601, 18.14618377272470084, -49.15350056088400521 ) ) ;
#33126 = CARTESIAN_POINT ( 'NONE',  ( 24.04493739769619864, -15.61618894467929941, -32.14999999999999858 ) ) ;
#33127 = CARTESIAN_POINT ( 'NONE',  ( 76.88109178265870014, -43.17103650464989784, -14.86960880489979964 ) ) ;
#33128 = CARTESIAN_POINT ( 'NONE',  ( 72.99216053021440587, 1.027568165751439944, -69.15654010815640618 ) ) ;
#33129 =( BOUNDED_CURVE ( )  B_SPLINE_CURVE ( 3, ( #45070, #28033, #48749, #4978 ),
 .UNSPECIFIED., .F., .T. ) 
 B_SPLINE_CURVE_WITH_KNOTS ( ( 4, 4 ),
 ( 0.003439152616818795267, 0.3469259656636344835 ),
 .UNSPECIFIED. ) 
 CURVE ( )  GEOMETRIC_REPRESENTATION_ITEM ( )  RATIONAL_B_SPLINE_CURVE ( ( 1.000000000000000000, 0.9901922104150019388, 0.9901922104150019388, 1.000000000000000000 ) ) 
 REPRESENTATION_ITEM ( '' )  );
#33130 = B_SPLINE_CURVE_WITH_KNOTS ( 'NONE', 3,
 ( #16377, #48883, #28676, #28938, #40747, #40234, #32589, #4846, #32852, #36806, #20039, #16118, #44422, #24989, #4324, #8524 ),
 .UNSPECIFIED., .F., .F.,
 ( 4, 2, 2, 2, 2, 2, 2, 4 ),
 ( 0.000000000000000000, 0.1775032223223184658, 0.3375025954872091227, 0.4375022037152671017, 0.5000019588578006324, 0.6250014691428724678, 0.7629640249125425600, 1.000000000000000000 ),
 .UNSPECIFIED. ) ;
#33131 = CARTESIAN_POINT ( 'NONE',  ( 8.428848602312072558, -17.68690935890205651, -36.70899794646796721 ) ) ;
#33132 = CIRCLE ( 'NONE', #14763, 1.500000000000001332 ) ;
#33133 = CARTESIAN_POINT ( 'NONE',  ( 82.13853704237929776, -45.11618894467940066, -46.37203261889099792 ) ) ;
#33134 = CARTESIAN_POINT ( 'NONE',  ( 22.04684527241202119, -19.02418722779176363, -78.61948426832272219 ) ) ;
#33135 = CARTESIAN_POINT ( 'NONE',  ( 48.79180034249609577, -53.85388452497259948, -54.46585069627389686 ) ) ;
#33136 = B_SPLINE_CURVE_WITH_KNOTS ( 'NONE', 3,
 ( #17189, #17444, #33146, #49428, #49173, #13524 ),
 .UNSPECIFIED., .F., .F.,
 ( 4, 1, 1, 4 ),
 ( 0.000000000000000000, 0.3333697255252178193, 0.6667202725206615721, 1.000000000000000000 ),
 .UNSPECIFIED. ) ;
#33137 = VECTOR ( 'NONE', #11202, 1000.000000000000000 ) ;
#33138 = CARTESIAN_POINT ( 'NONE',  ( 51.17464648325179155, -31.65168256193422280, -17.11447666815010749 ) ) ;
#33139 = CARTESIAN_POINT ( 'NONE',  ( 59.63596466869476131, -1.505138099722426848, -15.90544011693026683 ) ) ;
#33140 = CARTESIAN_POINT ( 'NONE',  ( 18.12954305947619815, -51.13036009974659635, -74.14993170018701107 ) ) ;
#33141 = CARTESIAN_POINT ( 'NONE',  ( 23.04646962482851791, -19.60030351599067444, -53.95900079672725269 ) ) ;
#33142 = EDGE_LOOP ( 'NONE', ( #37047, #33145, #22080, #34008, #40673, #7408 ) ) ;
#33143 = CARTESIAN_POINT ( 'NONE',  ( 9.593095007195888257, -12.04910678120510070, -44.22626530274989420 ) ) ;
#33144 = CARTESIAN_POINT ( 'NONE',  ( 63.93485720234319558, 1.348264851907009731, -61.51770149503649776 ) ) ;
#33145 = ORIENTED_EDGE ( 'NONE', *, *, #30921, .T. ) ;
#33146 = CARTESIAN_POINT ( 'NONE',  ( 0.006082813051881367540, -51.09064178927788191, -34.98052497386454007 ) ) ;
#33147 = CARTESIAN_POINT ( 'NONE',  ( 60.65080933879319502, -45.73000258907639903, -47.69371751895570100 ) ) ;
#33148 = CARTESIAN_POINT ( 'NONE',  ( 68.13393739769620083, 0.8838110553206759423, -65.65000000000000568 ) ) ;
#33149 = CARTESIAN_POINT ( 'NONE',  ( 50.31596464670999325, 18.73470065217860281, -76.14999999999999147 ) ) ;
#33151 = CARTESIAN_POINT ( 'NONE',  ( 18.13393739769630031, 1.391621760993470014, -35.14999999999999858 ) ) ;
#33150 = CARTESIAN_POINT ( 'NONE',  ( 45.10518118625895312, 8.805447820864591435, -61.30236472867089503 ) ) ;
#33152 = FACE_OUTER_BOUND ( 'NONE', #17513, .T. ) ;
#33153 = CARTESIAN_POINT ( 'NONE',  ( 8.222598545279129922, -15.61602001634830117, -66.50766849176299900 ) ) ;
#33154 = ORIENTED_EDGE ( 'NONE', *, *, #9648, .F. ) ;
#33155 = ORIENTED_EDGE ( 'NONE', *, *, #31660, .F. ) ;
#33156 = ORIENTED_EDGE ( 'NONE', *, *, #22274, .T. ) ;
#33157 = EDGE_CURVE ( 'NONE', #14308, #45450, #12655, .T. ) ;
#33158 = ORIENTED_EDGE ( 'NONE', *, *, #19351, .T. ) ;
#33159 = FACE_OUTER_BOUND ( 'NONE', #37712, .T. ) ;
#33160 = CARTESIAN_POINT ( 'NONE',  ( 50.02331077270184068, -52.39130121342888913, -51.61203677770532749 ) ) ;
#33161 = ADVANCED_FACE ( 'NONE', ( #42052 ), #29972, .T. ) ;
#33162 = FACE_OUTER_BOUND ( 'NONE', #42175, .T. ) ;
#33163 = EDGE_CURVE ( 'NONE', #40265, #7973, #42946, .T. ) ;
#33164 = ORIENTED_EDGE ( 'NONE', *, *, #1490, .T. ) ;
#33165 = EDGE_LOOP ( 'NONE', ( #22455, #17791, #1864, #13217 ) ) ;
#33166 = EDGE_CURVE ( 'NONE', #37946, #25965, #27022, .T. ) ;
#33167 = CARTESIAN_POINT ( 'NONE',  ( 11.54049066802846291, 34.10846995014738781, -22.61126967411468769 ) ) ;
#33168 = VERTEX_POINT ( 'NONE', #14012 ) ;
#33169 = AXIS2_PLACEMENT_3D ( 'NONE', #9835, #42064, #25276 ) ;
#33170 = CARTESIAN_POINT ( 'NONE',  ( 56.45963719500260680, 19.43072222330619780, -53.16982888481129521 ) ) ;
#33171 = CARTESIAN_POINT ( 'NONE',  ( -8.427464958487524527, 14.67799636298092203, -42.48227204479578489 ) ) ;
#33172 = DIRECTION ( 'NONE',  ( 0.5897727341282541502, 0.3900873262218164661, 0.7071067811865459074 ) ) ;
#33173 = CARTESIAN_POINT ( 'NONE',  ( 8.813944282408009201, -63.27296482252339871, -46.67145360045340396 ) ) ;
#33174 = DIRECTION ( 'NONE',  ( -0.1961161351381840723, -2.837236618486510447E-16, -0.9805806756909202226 ) ) ;
#33175 = ORIENTED_EDGE ( 'NONE', *, *, #28869, .T. ) ;
#33176 = CARTESIAN_POINT ( 'NONE',  ( 29.13393739769619728, -36.11618894467930119, -81.65000000000000568 ) ) ;
#33177 = CARTESIAN_POINT ( 'NONE',  ( 51.82414462793709475, -50.18944315258300293, -76.50963453239940293 ) ) ;
#33178 = CARTESIAN_POINT ( 'NONE',  ( 21.60259711254701998, -19.60660697021737775, -46.65346184971561172 ) ) ;
#33179 = CARTESIAN_POINT ( 'NONE',  ( 47.64143405402000297, -54.53488714544439375, -55.14905519569939685 ) ) ;
#33180 = AXIS2_PLACEMENT_3D ( 'NONE', #18144, #45936, #13962 ) ;
#33181 = CARTESIAN_POINT ( 'NONE',  ( 18.62649940869980014, -8.174826017574890358, -65.61537668992708916 ) ) ;
#33182 = AXIS2_PLACEMENT_3D ( 'NONE', #19417, #42766, #6865 ) ;
#33183 = CARTESIAN_POINT ( 'NONE',  ( 8.693390981131532413, 17.62014253445611800, -34.86893418027936775 ) ) ;
#33184 = CARTESIAN_POINT ( 'NONE',  ( 45.24668088971260005, 13.87996455531310147, -7.238505014500240087 ) ) ;
#33185 = EDGE_CURVE ( 'NONE', #23933, #17827, #37920, .T. ) ;
#33186 = CARTESIAN_POINT ( 'NONE',  ( 42.48652067527369525, -44.25687345361960467, -5.094659063150840161 ) ) ;
#33187 = CARTESIAN_POINT ( 'NONE',  ( 70.03247032090770574, -49.95860450174030376, -73.25000000000169109 ) ) ;
#33188 = CARTESIAN_POINT ( 'NONE',  ( 61.24959635998759921, -45.52506596813110207, -47.58791272468889844 ) ) ;
#33189 = CARTESIAN_POINT ( 'NONE',  ( 63.84678457914870364, 1.200162789678009823, -69.81105362774360401 ) ) ;
#33190 = CARTESIAN_POINT ( 'NONE',  ( 18.19606299423181284, -52.32662977634584678, -75.76245441609270870 ) ) ;
#33191 = CARTESIAN_POINT ( 'NONE',  ( 65.04200595171910493, 1.022226219316999973, -17.84399244536480111 ) ) ;
#33192 = AXIS2_PLACEMENT_3D ( 'NONE', #23314, #15740, #35394 ) ;
#33193 = ORIENTED_EDGE ( 'NONE', *, *, #48230, .F. ) ;
#33194 = CARTESIAN_POINT ( 'NONE',  ( 14.52849062202900043, -51.76348103900169662, -75.62474771911489313 ) ) ;
#33195 = CARTESIAN_POINT ( 'NONE',  ( 57.36736290859560938, 18.90165667866860133, -52.61791395480889832 ) ) ;
#33196 = LINE ( 'NONE', #25583, #46542 ) ;
#33197 = CARTESIAN_POINT ( 'NONE',  ( 16.13393739769620083, -15.61618894467929941, -32.14999999999999858 ) ) ;
#33198 = CYLINDRICAL_SURFACE ( 'NONE', #51633, 6.766999999999998572 ) ;
#33199 = VECTOR ( 'NONE', #41211, 999.9999999999998863 ) ;
#33201 = EDGE_CURVE ( 'NONE', #38136, #13016, #17696, .T. ) ;
#33200 = CARTESIAN_POINT ( 'NONE',  ( 22.46384208064960220, -12.53037029265690094, -32.14999999999999858 ) ) ;
#33202 = CARTESIAN_POINT ( 'NONE',  ( 12.06284766121009966, 32.21085600226960111, -22.25048313876769868 ) ) ;
#33203 = CARTESIAN_POINT ( 'NONE',  ( 47.77967683121789833, -54.45042155320719957, -54.88424258904849751 ) ) ;
#33205 = CARTESIAN_POINT ( 'NONE',  ( 14.34417029198830029, 19.88381105532299742, -22.49240188329279988 ) ) ;
#33204 = DIRECTION ( 'NONE',  ( 0.3294064756440921449, -0.9441882088883224444, 0.000000000000000000 ) ) ;
#33206 = CARTESIAN_POINT ( 'NONE',  ( 56.41160328492299669, 19.47925591966880177, -53.28618851948499469 ) ) ;
#33207 = CARTESIAN_POINT ( 'NONE',  ( 33.32492040275669609, -15.61618894397629909, 14.85000000026379396 ) ) ;
#33208 = CARTESIAN_POINT ( 'NONE',  ( 48.65500193615349644, 22.71479567191139992, -54.55862777695219989 ) ) ;
#33209 = ORIENTED_EDGE ( 'NONE', *, *, #46636, .T. ) ;
#33210 = CARTESIAN_POINT ( 'NONE',  ( 23.11112601400289890, -14.58594713474730042, -60.80051578558619241 ) ) ;
#33211 = ORIENTED_EDGE ( 'NONE', *, *, #45734, .T. ) ;
#33212 = CARTESIAN_POINT ( 'NONE',  ( 68.13393739769618662, -29.16618894467940137, -65.65000000000000568 ) ) ;
#33213 = AXIS2_PLACEMENT_3D ( 'NONE', #17516, #33488, #49502 ) ;
#33214 = FACE_OUTER_BOUND ( 'NONE', #19056, .T. ) ;
#33215 = FACE_OUTER_BOUND ( 'NONE', #6428, .T. ) ;
#33217 = CARTESIAN_POINT ( 'NONE',  ( 52.77845664521150582, 18.41768890413229798, -27.63491308911480004 ) ) ;
#33216 = CARTESIAN_POINT ( 'NONE',  ( 82.70745875113269108, 14.23235930836570162, -47.51979026979370246 ) ) ;
#33218 = CARTESIAN_POINT ( 'NONE',  ( 10.78987444403530027, -11.01362989085549948, -63.67913456332050259 ) ) ;
#33219 = FACE_OUTER_BOUND ( 'NONE', #11031, .T. ) ;
#33220 = CARTESIAN_POINT ( 'NONE',  ( 56.07056193865970073, -45.13118964431610181, -15.17735046330640181 ) ) ;
#33221 = CARTESIAN_POINT ( 'NONE',  ( 24.44780054039034667, -9.575813799495710654, -5.690000000000000391 ) ) ;
#33222 = EDGE_LOOP ( 'NONE', ( #49961, #2829, #25689, #47932 ) ) ;
#33223 = ORIENTED_EDGE ( 'NONE', *, *, #37738, .F. ) ;
#33224 = CARTESIAN_POINT ( 'NONE',  ( 12.11414304660010188, -65.16113420147659951, -16.63763903707940273 ) ) ;
#33225 = CARTESIAN_POINT ( 'NONE',  ( 12.37952141923769922, 34.14838032032060511, -46.79454185349629824 ) ) ;
#33226 = CARTESIAN_POINT ( 'NONE',  ( 73.01642658308999501, 0.9425424353906030062, -62.16269173205530763 ) ) ;
#33227 = EDGE_CURVE ( 'NONE', #6636, #27825, #37082, .T. ) ;
#33228 = CARTESIAN_POINT ( 'NONE',  ( 16.13393739769620083, -45.61618894467940066, -49.33749999999999858 ) ) ;
#33229 = CARTESIAN_POINT ( 'NONE',  ( -14.25993951570189999, -0.3776770037709330508, -34.64999999999999858 ) ) ;
#33230 = ORIENTED_EDGE ( 'NONE', *, *, #51754, .T. ) ;
#33231 = ADVANCED_FACE ( 'NONE', ( #30238 ), #6134, .F. ) ;
#33232 = CARTESIAN_POINT ( 'NONE',  ( -13.74979103991289975, -41.20090589574910211, -47.05386678597589878 ) ) ;
#33233 = CARTESIAN_POINT ( 'NONE',  ( 52.88960523627919486, 18.37708893635865692, -27.85916541547489800 ) ) ;
#33234 = DIRECTION ( 'NONE',  ( 0.000000000000000000, 1.000000000000000000, 0.000000000000000000 ) ) ;
#33235 = CARTESIAN_POINT ( 'NONE',  ( 24.04493737759684180, -16.65173755265768563, -59.54933332424322145 ) ) ;
#33236 = PLANE ( 'NONE',  #35883 ) ;
#33237 = CARTESIAN_POINT ( 'NONE',  ( 50.23538084491700317, -49.77012050973760182, -76.14999999999999147 ) ) ;
#33238 = CARTESIAN_POINT ( 'NONE',  ( 20.11806584526820174, -22.52871384128776100, -43.84102563478171533 ) ) ;
#33239 = ORIENTED_EDGE ( 'NONE', *, *, #27392, .F. ) ;
#33240 = B_SPLINE_CURVE_WITH_KNOTS ( 'NONE', 3,
 ( #25902, #17551, #5250, #33523, #14130, #37211, #1311, #33260, #29336, #49535, #3380, #31638, #7567, #19352, #19608, #23516, #18576, #51071, #30616, #15684, #10726, #39274, #50556, #38770, #23006, #39536, #35066, #46640, #50814, #35599, #27205, #26679, #15171, #11505 ),
 .UNSPECIFIED., .F., .F.,
 ( 4, 3, 3, 3, 3, 3, 3, 3, 3, 3, 3, 4 ),
 ( 3.231192999999999801E-12, 0.3998525513778730112, 0.8924049053485588745, 0.9695310320484800126, 1.582190098185180194, 2.108887993389690241, 2.822382364412600264, 3.535876735435510287, 4.252742048685130172, 4.968682683331829608, 5.179452103612369740, 5.526958877413330029 ),
 .UNSPECIFIED. ) ;
#33241 = CARTESIAN_POINT ( 'NONE',  ( 20.29261235332924329, -10.20487319419143368, -68.16115184722131914 ) ) ;
#33242 = DIRECTION ( 'NONE',  ( 0.000000000000000000, 0.000000000000000000, 1.000000000000000000 ) ) ;
#33243 = VERTEX_POINT ( 'NONE', #17427 ) ;
#33244 = CARTESIAN_POINT ( 'NONE',  ( 20.99560421276813571, -9.290014746710346216, -53.50066707012037881 ) ) ;
#33245 = DIRECTION ( 'NONE',  ( 0.000000000000000000, 0.000000000000000000, -1.000000000000000000 ) ) ;
#33246 = CARTESIAN_POINT ( 'NONE',  ( 23.61944552496879979, -12.15932946040240026, -79.65462137872769688 ) ) ;
#33247 = CARTESIAN_POINT ( 'NONE',  ( 13.86591929268250034, -51.23668186105609834, -22.87012482983299932 ) ) ;
#33248 = LINE ( 'NONE', #764, #45581 ) ;
#33249 = CONTEXT_DEPENDENT_SHAPE_REPRESENTATION ( #22750, #29457 ) ;
#33250 = CARTESIAN_POINT ( 'NONE',  ( 47.01491813235679729, -53.96463636605060543, -75.73879140141839628 ) ) ;
#33251 = ORIENTED_EDGE ( 'NONE', *, *, #37996, .F. ) ;
#33252 = CARTESIAN_POINT ( 'NONE',  ( 56.19404819212199698, 14.17124906888450120, -16.68782110614939995 ) ) ;
#33253 = CARTESIAN_POINT ( 'NONE',  ( 57.28774565251580242, -50.57888888196889354, -53.44461253009320245 ) ) ;
#33254 = VECTOR ( 'NONE', #21114, 1000.000000000000000 ) ;
#33255 = CARTESIAN_POINT ( 'NONE',  ( 9.747988662193298737, -18.60988528556680066, -33.70764136182839366 ) ) ;
#33256 = DIRECTION ( 'NONE',  ( -0.8660254037844387076, -0.4999999999999998890, 0.000000000000000000 ) ) ;
#33257 = ORIENTED_EDGE ( 'NONE', *, *, #25699, .T. ) ;
#33258 = CARTESIAN_POINT ( 'NONE',  ( 47.21888195866730342, 22.94886078616289993, -75.46887108633461594 ) ) ;
#33259 = LINE ( 'NONE', #18060, #15868 ) ;
#33260 = CARTESIAN_POINT ( 'NONE',  ( 41.40202236619799692, -45.62702843439980427, -6.330381766430189572 ) ) ;
#33261 = DIRECTION ( 'NONE',  ( 1.000000000000000000, 0.000000000000000000, 0.000000000000000000 ) ) ;
#33262 = EDGE_CURVE ( 'NONE', #34702, #3924, #2217, .T. ) ;
#33263 = CARTESIAN_POINT ( 'NONE',  ( 17.94517161182763942, -49.61615078444357607, -83.16479114451217924 ) ) ;
#33265 = EDGE_CURVE ( 'NONE', #9653, #34462, #3042, .T. ) ;
#33264 = CARTESIAN_POINT ( 'NONE',  ( 60.40020840339374075, 14.46217060654146280, -47.21880793596233872 ) ) ;
#33266 = DIRECTION ( 'NONE',  ( 1.000000000000000000, 0.000000000000000000, 0.000000000000000000 ) ) ;
#33268 = CARTESIAN_POINT ( 'NONE',  ( 16.13393739769620083, -15.61618894467929941, -23.15000000000000213 ) ) ;
#33267 = FACE_OUTER_BOUND ( 'NONE', #34648, .T. ) ;
#33269 = LINE ( 'NONE', #45079, #17631 ) ;
#33270 = CARTESIAN_POINT ( 'NONE',  ( 9.221400882477601257, -11.63208038433509373, -68.67433567719821497 ) ) ;
#33271 = CARTESIAN_POINT ( 'NONE',  ( -26.88697088543599989, -41.87816877422690709, -56.26659592162470602 ) ) ;
#33272 = ADVANCED_FACE ( 'NONE', ( #1180 ), #31005, .T. ) ;
#33273 = VERTEX_POINT ( 'NONE', #24415 ) ;
#33274 = CARTESIAN_POINT ( 'NONE',  ( 52.80018231237879434, -49.68132406852449634, -48.71455220968519484 ) ) ;
#33275 = CARTESIAN_POINT ( 'NONE',  ( 60.57693621588790478, -45.12131271250889597, -26.54673895663080074 ) ) ;
#33276 = CARTESIAN_POINT ( 'NONE',  ( 24.04493739769619864, -15.61618894467929941, -32.14999999999999858 ) ) ;
#33277 = CARTESIAN_POINT ( 'NONE',  ( 13.32586770901309947, 19.62211552346140309, -21.60957827883089877 ) ) ;
#33278 = CARTESIAN_POINT ( 'NONE',  ( 57.06431677564219740, 13.92418399135899953, -25.30300626299959887 ) ) ;
#33279 = CARTESIAN_POINT ( 'NONE',  ( 15.05117764281579973, -22.58542061303949922, -35.00188151829029692 ) ) ;
#33280 = CARTESIAN_POINT ( 'NONE',  ( 51.02428974428540442, 18.84793802927210038, -76.22815759457780871 ) ) ;
#33281 = CARTESIAN_POINT ( 'NONE',  ( 52.67441652328110280, 18.52990734569499764, -48.55744554217059772 ) ) ;
#33282 = CARTESIAN_POINT ( 'NONE',  ( 71.42462519098069151, 0.8888742037077609348, -70.66714310028369539 ) ) ;
#33283 = CARTESIAN_POINT ( 'NONE',  ( 41.72053737372340265, -43.71151935359279861, -3.400228435618770195 ) ) ;
#33284 = CARTESIAN_POINT ( 'NONE',  ( 73.44245504306711325, -45.11618894467940066, -14.54927509218509840 ) ) ;
#33285 = ORIENTED_EDGE ( 'NONE', *, *, #9506, .F. ) ;
#33286 = CARTESIAN_POINT ( 'NONE',  ( 8.692723195675709391, -15.98364715725590024, -70.05163682948979442 ) ) ;
#33287 = B_SPLINE_CURVE_WITH_KNOTS ( 'NONE', 3,
 ( #24008, #36867, #48939, #966 ),
 .UNSPECIFIED., .F., .F.,
 ( 4, 4 ),
 ( 0.4931821390625270030, 20.02578215755499969 ),
 .UNSPECIFIED. ) ;
#33288 = B_SPLINE_CURVE_WITH_KNOTS ( 'NONE', 3,
 ( #7451, #3524, #106, #12938, #24946, #43864, #20251, #32036, #15820, #36756, #20505, #24427, #40441, #28894, #7962, #12407, #48576, #40190 ),
 .UNSPECIFIED., .F., .F.,
 ( 4, 2, 2, 2, 2, 2, 2, 2, 4 ),
 ( 0.5000011091671422436, 0.5625009705212494771, 0.6250008318753568215, 0.6875006932294640549, 0.7500005545835712883, 0.8125004159376785218, 0.8750002772917856442, 0.9375001386458927666, 1.000000000000000000 ),
 .UNSPECIFIED. ) ;
#33289 = CARTESIAN_POINT ( 'NONE',  ( 72.77636315587029969, 1.387131204727280132, -68.68796153961081075 ) ) ;
#33290 = CARTESIAN_POINT ( 'NONE',  ( 47.44513431003649373, -54.62464540978789529, -54.74498770855480245 ) ) ;
#33291 = CARTESIAN_POINT ( 'NONE',  ( 13.69709356640602671, -8.058494653411733211, -49.19314222014786964 ) ) ;
#33292 = CARTESIAN_POINT ( 'NONE',  ( 73.26121012496899709, 0.9212109678634080590, -62.53374032209040223 ) ) ;
#33293 = CARTESIAN_POINT ( 'NONE',  ( 58.15863228698849952, 17.43447541518139943, -50.85867504786170201 ) ) ;
#33294 = CARTESIAN_POINT ( 'NONE',  ( 17.92370450339669929, -51.11618894467930119, -74.14999999999999147 ) ) ;
#33295 = CARTESIAN_POINT ( 'NONE',  ( 46.63393739769619373, 7.878491304262099426, -34.64999999999999858 ) ) ;
#33296 = CARTESIAN_POINT ( 'NONE',  ( 71.99113505772810129, 1.080095028449399974, -61.06117396776439676 ) ) ;
#33297 = VECTOR ( 'NONE', #39960, 1000.000000000000000 ) ;
#33298 = LINE ( 'NONE', #36709, #4234 ) ;
#33299 = EDGE_LOOP ( 'NONE', ( #17710, #35550, #28647, #51245 ) ) ;
#33300 = EDGE_CURVE ( 'NONE', #10111, #24567, #51228, .T. ) ;
#33301 = CARTESIAN_POINT ( 'NONE',  ( 64.97847163984020824, 0.9947083095259759977, -70.74365995857920097 ) ) ;
#33302 = EDGE_LOOP ( 'NONE', ( #24489, #10783, #41553, #38847, #16400, #6825 ) ) ;
#33303 = CARTESIAN_POINT ( 'NONE',  ( 8.813944282408009201, -63.27296482252339871, -46.67145360045340396 ) ) ;
#33304 = AXIS2_PLACEMENT_3D ( 'NONE', #12416, #16086, #7460 ) ;
#33305 = DIRECTION ( 'NONE',  ( 1.000000000000000000, 0.000000000000000000, 0.000000000000000000 ) ) ;
#33306 = VERTEX_POINT ( 'NONE', #23900 ) ;
#33307 = LINE ( 'NONE', #24907, #1583 ) ;
#33308 = CARTESIAN_POINT ( 'NONE',  ( 10.22099953874110412, -12.20824267314787548, -69.61948740543661529 ) ) ;
#33309 = DIRECTION ( 'NONE',  ( -1.000000000000000000, 0.000000000000000000, 0.000000000000000000 ) ) ;
#33310 = CARTESIAN_POINT ( 'NONE',  ( 53.83039865298910343, 19.62284230666540097, -76.11625649682230232 ) ) ;
#33311 = ORIENTED_EDGE ( 'NONE', *, *, #4957, .F. ) ;
#33312 = FACE_OUTER_BOUND ( 'NONE', #20970, .T. ) ;
#33313 = CARTESIAN_POINT ( 'NONE',  ( -14.86606260230379917, -15.61618894467933139, -17.89999999999999858 ) ) ;
#33314 = CARTESIAN_POINT ( 'NONE',  ( 9.910435692222698378, -20.53991556490245785, -66.29463588517631933 ) ) ;
#33315 = CARTESIAN_POINT ( 'NONE',  ( 24.37891534843840091, -15.56088390232210017, -57.79019640516870027 ) ) ;
#33316 = CARTESIAN_POINT ( 'NONE',  ( 12.14477763102834373, -10.07529305404503717, -55.75450440121188933 ) ) ;
#33317 = CARTESIAN_POINT ( 'NONE',  ( 41.95166363962292877, -37.61591301745547611, -80.56130022381232436 ) ) ;
#33318 = ORIENTED_EDGE ( 'NONE', *, *, #37023, .F. ) ;
#33319 = CARTESIAN_POINT ( 'NONE',  ( 56.39270784227079503, -50.52750194671250483, -52.86271187454359932 ) ) ;
#33320 = CARTESIAN_POINT ( 'NONE',  ( 22.72830296970559871, -19.08332558863240180, -42.38673599774679701 ) ) ;
#33321 = CARTESIAN_POINT ( 'NONE',  ( 52.56521993351460509, -49.86179673305679927, -48.47378032971909789 ) ) ;
#33322 = CARTESIAN_POINT ( 'NONE',  ( 42.67456719961179346, 14.69556074203230089, -7.343022369310959974 ) ) ;
#33323 = CARTESIAN_POINT ( 'NONE',  ( 13.74871818702220061, 20.76921105827980085, -75.35480091913980516 ) ) ;
#33324 = DIRECTION ( 'NONE',  ( -0.1999849291395982553, -0.9797989733190325401, 0.000000000000000000 ) ) ;
#33325 = CARTESIAN_POINT ( 'NONE',  ( 83.46510812583990457, -44.70132628866610247, -46.64393865386079341 ) ) ;
#33326 = AXIS2_PLACEMENT_3D ( 'NONE', #16237, #39322, #47706 ) ;
#33327 = CARTESIAN_POINT ( 'NONE',  ( 14.50620669810990115, -7.533292590116819731, -48.94441338548729448 ) ) ;
#33328 = VERTEX_POINT ( 'NONE', #16847 ) ;
#33329 = CARTESIAN_POINT ( 'NONE',  ( 52.77069811684319944, -49.64525113236509668, -27.51082437244179957 ) ) ;
#33330 = EDGE_CURVE ( 'NONE', #19102, #1209, #33654, .T. ) ;
#33331 = CARTESIAN_POINT ( 'NONE',  ( 14.34399776555519956, -51.11618894007569480, -22.49261467888789667 ) ) ;
#33332 = CARTESIAN_POINT ( 'NONE',  ( 13.74532132657402173, -23.19733159729566552, -40.10491864076364976 ) ) ;
#33333 = CARTESIAN_POINT ( 'NONE',  ( 11.76847557413320189, 32.96418959114749470, -15.47533549984080103 ) ) ;
#33334 = CARTESIAN_POINT ( 'NONE',  ( 9.366504787982940172, -15.61629640169840094, -69.84717978381009118 ) ) ;
#33335 = DIRECTION ( 'NONE',  ( 0.000000000000000000, -1.000000000000000000, 0.000000000000000000 ) ) ;
#33336 = VERTEX_POINT ( 'NONE', #22949 ) ;
#33337 = CARTESIAN_POINT ( 'NONE',  ( -11.32734370190460105, -41.88171845330919751, -6.430192534648670133 ) ) ;
#33338 = CARTESIAN_POINT ( 'NONE',  ( 47.48053164517749991, 23.37705619533080181, -54.85557598631709908 ) ) ;
#33339 = CARTESIAN_POINT ( 'NONE',  ( 16.13393739769620083, -15.61618894467929941, -7.049999999999999822 ) ) ;
#33340 = CARTESIAN_POINT ( 'NONE',  ( 63.50007682179899149, 1.388189907116970101, -62.58632377286669879 ) ) ;
#33341 = CARTESIAN_POINT ( 'NONE',  ( 55.58236959119586373, 15.93246778660674323, -26.45502009950325473 ) ) ;
#33342 = CARTESIAN_POINT ( 'NONE',  ( 11.91784406111709949, 34.19847404269119551, -17.65794013793280115 ) ) ;
#33343 = CARTESIAN_POINT ( 'NONE',  ( 10.22104436064596023, -19.02421183790971071, -53.28615311890232675 ) ) ;
#33344 = DIRECTION ( 'NONE',  ( -1.224646799147353207E-16, 1.000000000000000000, 0.000000000000000000 ) ) ;
#33345 = CARTESIAN_POINT ( 'NONE',  ( -11.07640030671909948, 8.018182000708311108, -19.14999999999999858 ) ) ;
#33346 = CARTESIAN_POINT ( 'NONE',  ( 55.20227514146910153, -48.56140865947679686, -48.75929635819750274 ) ) ;
#33347 = DIRECTION ( 'NONE',  ( -0.7071067811865475727, 0.7071067811865475727, 0.000000000000000000 ) ) ;
#33348 = CARTESIAN_POINT ( 'NONE',  ( 53.17432493994039788, 20.66509266784749954, -53.32388713517680401 ) ) ;
#33349 = CARTESIAN_POINT ( 'NONE',  ( 63.46413472570510095, 0.9973839016405651181, -69.41844569992100844 ) ) ;
#33350 = FACE_BOUND ( 'NONE', #40140, .T. ) ;
#33351 = CYLINDRICAL_SURFACE ( 'NONE', #13242, 6.766999999999998572 ) ;
#33352 = VERTEX_POINT ( 'NONE', #51529 ) ;
#33353 = CARTESIAN_POINT ( 'NONE',  ( 16.91199818135557109, 14.75900075713340165, -34.79644660940672907 ) ) ;
#33354 = CARTESIAN_POINT ( 'NONE',  ( 9.289247614019680910, 31.98971538174660267, -46.53005782715530358 ) ) ;
#33355 = CARTESIAN_POINT ( 'NONE',  ( 5.057652393281839132, 1.468834192434126829, -59.64999999999999147 ) ) ;
#33356 = CARTESIAN_POINT ( 'NONE',  ( 66.56327834958220535, -30.21069703426200093, -16.96525396667280106 ) ) ;
#33357 = ADVANCED_FACE ( 'NONE', ( #27916 ), #34747, .T. ) ;
#33358 = CARTESIAN_POINT ( 'NONE',  ( 17.73209452681750165, 20.42331001517590394, -75.51792558472199346 ) ) ;
#33359 = ORIENTED_EDGE ( 'NONE', *, *, #44674, .T. ) ;
#33360 = EDGE_LOOP ( 'NONE', ( #44574, #14754, #18420, #47369, #24060, #41801, #49891, #17067, #33621, #2716, #10721, #38930 ) ) ;
#33361 = CARTESIAN_POINT ( 'NONE',  ( 15.09849879369435399, -23.52720210124172340, -80.04933602518147495 ) ) ;
#33362 = B_SPLINE_CURVE_WITH_KNOTS ( 'NONE', 3,
 ( #4921, #1251, #44496, #45276, #8598, #20892, #32936, #13066, #9386 ),
 .UNSPECIFIED., .F., .F.,
 ( 4, 1, 1, 1, 1, 1, 4 ),
 ( 0.000000000000000000, 0.1666541203251306613, 0.3333161082673998243, 0.4999780962096700421, 0.6666400841519403153, 0.8333020720942094783, 1.000000000000000000 ),
 .UNSPECIFIED. ) ;
#33363 = EDGE_CURVE ( 'NONE', #10625, #5472, #19918, .T. ) ;
#33364 = ORIENTED_EDGE ( 'NONE', *, *, #2540, .T. ) ;
#33365 = CARTESIAN_POINT ( 'NONE',  ( 12.91702256450149910, -65.51268121040151016, -47.68987055332590330 ) ) ;
#33366 = CARTESIAN_POINT ( 'NONE',  ( 56.17575110250020032, -46.09713117230519686, -26.07745160796680040 ) ) ;
#33367 = CARTESIAN_POINT ( 'NONE',  ( 10.22100624670438052, -19.02414668158459321, -45.28616605880424828 ) ) ;
#33368 = CARTESIAN_POINT ( 'NONE',  ( 61.55546069326469905, 13.95115017060379969, -46.85742263993579115 ) ) ;
#33369 = DIRECTION ( 'NONE',  ( 1.000000000000000000, 0.000000000000000000, 0.000000000000000000 ) ) ;
#33370 = ORIENTED_EDGE ( 'NONE', *, *, #8054, .T. ) ;
#33371 = AXIS2_PLACEMENT_3D ( 'NONE', #42564, #37849, #13998 ) ;
#33372 = CARTESIAN_POINT ( 'NONE',  ( 75.17996938839529264, -0.5297985755353621373, -11.94677486813695388 ) ) ;
#33373 = CONICAL_SURFACE ( 'NONE', #14974, 0.7980000000000000426, 0.7853981633974476129 ) ;
#33374 = ORIENTED_EDGE ( 'NONE', *, *, #33749, .F. ) ;
#33375 = CARTESIAN_POINT ( 'NONE',  ( 50.66367948673760679, -45.98186837715630304, -12.79866758418470063 ) ) ;
#33376 = DIRECTION ( 'NONE',  ( 0.000000000000000000, 1.000000000000000000, 0.000000000000000000 ) ) ;
#33377 = AXIS2_PLACEMENT_3D ( 'NONE', #45940, #10294, #37816 ) ;
#33378 = CARTESIAN_POINT ( 'NONE',  ( 68.13393739769810509, 19.38381105532030091, -71.50000000000198952 ) ) ;
#33379 = VERTEX_POINT ( 'NONE', #14849 ) ;
#33380 = CARTESIAN_POINT ( 'NONE',  ( 73.04443511092429731, 0.9036513197889520788, -69.09785636402040154 ) ) ;
#33381 = CARTESIAN_POINT ( 'NONE',  ( 46.91224408115239441, -54.15189901127720162, -75.65958371907380808 ) ) ;
#33382 = CARTESIAN_POINT ( 'NONE',  ( 44.13393739769620083, 4.883811055320659733, -34.64999999999999858 ) ) ;
#33383 = CARTESIAN_POINT ( 'NONE',  ( 50.25339681658829960, 14.35477854232929928, -12.12767580573030024 ) ) ;
#33384 = DIRECTION ( 'NONE',  ( -1.000000000000000000, 0.000000000000000000, 0.000000000000000000 ) ) ;
#33385 = B_SPLINE_CURVE_WITH_KNOTS ( 'NONE', 3,
 ( #48138, #8569, #12495, #51809, #4109, #28465, #36078, #24777, #40530, #12239, #32378, #8301, #3864, #40787, #44203, #44463, #4888, #20087, #36587, #689 ),
 .UNSPECIFIED., .F., .F.,
 ( 4, 2, 2, 2, 2, 2, 2, 2, 2, 4 ),
 ( 0.000000000000000000, 0.03794172797384393753, 0.1301135039818921146, 0.2222852799899402987, 0.3374999999999994116, 0.4374999999999988898, 0.5000000000000018874, 0.6250000000000007772, 0.8250000000000001776, 1.000000000000000000 ),
 .UNSPECIFIED. ) ;
#33386 = DIRECTION ( 'NONE',  ( -0.6023772969742139383, 0.4987169684303948691, -0.6232358923310148402 ) ) ;
#33387 = CARTESIAN_POINT ( 'NONE',  ( 18.14390284338876214, -22.37655861516149614, -55.25519061113300268 ) ) ;
#33388 = CARTESIAN_POINT ( 'NONE',  ( 58.43730894494089512, 13.94609765837119930, -25.90344854066760050 ) ) ;
#33389 = CARTESIAN_POINT ( 'NONE',  ( 8.505345115432438874, -17.45774480160260111, -68.21210752448658354 ) ) ;
#33390 = VERTEX_POINT ( 'NONE', #19806 ) ;
#33391 = CARTESIAN_POINT ( 'NONE',  ( 21.17745084236876707, -10.68612491792656627, -48.60080040178979743 ) ) ;
#33392 = ADVANCED_FACE ( 'NONE', ( #19547 ), #3579, .T. ) ;
#33393 = CARTESIAN_POINT ( 'NONE',  ( 73.13559359734860266, 0.8904513541338869853, -62.33586013860640662 ) ) ;
#33394 = DIRECTION ( 'NONE',  ( 0.8660254037844390407, 0.4999999999999995004, 2.775557561562887037E-17 ) ) ;
#33395 = CARTESIAN_POINT ( 'NONE',  ( 72.65185559415030525, 1.328802495349810098, -69.38895227739480731 ) ) ;
#33396 = AXIS2_PLACEMENT_3D ( 'NONE', #28018, #51120, #35647 ) ;
#33397 = AXIS2_PLACEMENT_3D ( 'NONE', #29962, #29706, #25513 ) ;
#33398 = CARTESIAN_POINT ( 'NONE',  ( 11.41271396217149992, -64.98654470182599141, -16.69425700586020156 ) ) ;
#33399 = CARTESIAN_POINT ( 'NONE',  ( 72.33393739770319542, 11.38381105531869686, -69.85000000000681553 ) ) ;
#33400 = VECTOR ( 'NONE', #10872, 1000.000000000000000 ) ;
#33401 = CARTESIAN_POINT ( 'NONE',  ( 47.46019986771550236, -54.30427659521456718, -75.17791912521337849 ) ) ;
#33402 = CARTESIAN_POINT ( 'NONE',  ( 48.80109316716579571, -53.86560520698500198, -54.49771944612560048 ) ) ;
#33403 = CARTESIAN_POINT ( 'NONE',  ( 8.428792854876448359, -17.68670666238835310, -56.70900359172159000 ) ) ;
#33404 = CARTESIAN_POINT ( 'NONE',  ( 24.03425380569510139, -16.05991031410578884, -33.52552477532261577 ) ) ;
#33405 = CARTESIAN_POINT ( 'NONE',  ( 61.75019796695539753, 14.88381105532069881, -37.26101630944549470 ) ) ;
#33406 = ORIENTED_EDGE ( 'NONE', *, *, #39873, .T. ) ;
#33407 = CARTESIAN_POINT ( 'NONE',  ( 12.86561113652319932, -22.31131685898150252, -47.71189826954910274 ) ) ;
#33408 = CARTESIAN_POINT ( 'NONE',  ( 64.60887562658849959, 1.412342135319750058, -61.15705615616909796 ) ) ;
#33409 = ORIENTED_EDGE ( 'NONE', *, *, #18638, .T. ) ;
#33410 = CARTESIAN_POINT ( 'NONE',  ( 22.90129928757160727, -15.40020387630258725, -34.83702718343101168 ) ) ;
#33411 = CARTESIAN_POINT ( 'NONE',  ( 60.80694905565239594, -45.63379593877770901, -47.60985284215269786 ) ) ;
#33412 = CARTESIAN_POINT ( 'NONE',  ( 16.13393739769620083, -15.61618894467929941, -32.14999999999999858 ) ) ;
#33413 = CARTESIAN_POINT ( 'NONE',  ( 50.36549662992289456, 18.84323467693539911, -76.14999999999999147 ) ) ;
#33415 = CARTESIAN_POINT ( 'NONE',  ( 26.63393739736279997, -15.61618894439989980, -19.08999999982600215 ) ) ;
#33414 = CARTESIAN_POINT ( 'NONE',  ( 43.02593272906347011, 8.636460564420850972, -71.37299277478172144 ) ) ;
#33416 = CARTESIAN_POINT ( 'NONE',  ( 22.90083016047308462, -15.61618874168370752, -60.84718745454353694 ) ) ;
#33417 = CARTESIAN_POINT ( 'NONE',  ( 10.07017945893940869, -54.00735027851921188, -34.80997524098909679 ) ) ;
#33418 = ORIENTED_EDGE ( 'NONE', *, *, #47379, .T. ) ;
#33419 = ORIENTED_EDGE ( 'NONE', *, *, #8769, .F. ) ;
#33420 = ORIENTED_EDGE ( 'NONE', *, *, #41580, .T. ) ;
#33421 = EDGE_CURVE ( 'NONE', #36842, #2213, #27441, .T. ) ;
#33422 = ORIENTED_EDGE ( 'NONE', *, *, #36414, .F. ) ;
#33423 = CARTESIAN_POINT ( 'NONE',  ( 61.49601566777620576, -45.18573077412970207, -46.83864831159979758 ) ) ;
#33424 = CARTESIAN_POINT ( 'NONE',  ( 28.13393739769619728, -22.54439217495490055, -47.64999999999999858 ) ) ;
#33425 = CARTESIAN_POINT ( 'NONE',  ( 54.80487992904060235, -51.26385116109580053, -53.16356012067550552 ) ) ;
#33426 = ORIENTED_EDGE ( 'NONE', *, *, #50559, .T. ) ;
#33427 = EDGE_LOOP ( 'NONE', ( #41987, #2962, #48469, #15705 ) ) ;
#33428 = ORIENTED_EDGE ( 'NONE', *, *, #23269, .T. ) ;
#33429 = DIRECTION ( 'NONE',  ( 0.000000000000000000, 0.000000000000000000, -1.000000000000000000 ) ) ;
#33430 = CARTESIAN_POINT ( 'NONE',  ( -16.54679035245789365, 5.671130177897621749, -49.45205420238420402 ) ) ;
#33431 = CARTESIAN_POINT ( 'NONE',  ( 13.37178884610072060, 18.38381105532060644, -83.05213603420975232 ) ) ;
#33432 = CARTESIAN_POINT ( 'NONE',  ( 55.72786029574290012, -51.09037789658940909, -53.93924188563359934 ) ) ;
#33433 = DIRECTION ( 'NONE',  ( 0.000000000000000000, 0.000000000000000000, 1.000000000000000000 ) ) ;
#33434 = CIRCLE ( 'NONE', #50298, 5.499999999999998224 ) ;
#33435 = AXIS2_PLACEMENT_3D ( 'NONE', #41969, #31683, #23055 ) ;
#33436 = ORIENTED_EDGE ( 'NONE', *, *, #33421, .F. ) ;
#33437 = CYLINDRICAL_SURFACE ( 'NONE', #4053, 0.5000000000000049960 ) ;
#33438 = CARTESIAN_POINT ( 'NONE',  ( 52.10718084980409515, -50.10817224434760675, -76.73077500979640320 ) ) ;
#33439 = CIRCLE ( 'NONE', #2473, 2.499999999999998668 ) ;
#33440 = CARTESIAN_POINT ( 'NONE',  ( 60.70166025825290035, 14.30423153367579836, -47.08674219091739843 ) ) ;
#33441 = VECTOR ( 'NONE', #15766, 1000.000000000000000 ) ;
#33442 = CARTESIAN_POINT ( 'NONE',  ( 23.25678206576879958, -18.91040075118040065, -68.15038248396299991 ) ) ;
#33443 = CARTESIAN_POINT ( 'NONE',  ( 16.13393739769620083, -15.61618894467929941, -2.149999999999999911 ) ) ;
#33444 = CARTESIAN_POINT ( 'NONE',  ( 41.80335235802419902, 13.65426996821039829, -5.672373394308329431 ) ) ;
#33445 = CARTESIAN_POINT ( 'NONE',  ( 43.68128689207919990, -43.54714580617979891, -5.037759820094009910 ) ) ;
#33446 = CARTESIAN_POINT ( 'NONE',  ( 72.61552859537219717, 1.010053820890850051, -61.65938070570059892 ) ) ;
#33447 = CARTESIAN_POINT ( 'NONE',  ( 63.64770250141179986, 1.099199775695780090, -69.62734437806821575 ) ) ;
#33448 = CARTESIAN_POINT ( 'NONE',  ( 13.73527022026379996, 18.97497658877130178, -20.93080062776429884 ) ) ;
#33449 = CARTESIAN_POINT ( 'NONE',  ( 65.70575104159891566, 1.626048249155310099, -18.95023426183129800 ) ) ;
#33450 = ORIENTED_EDGE ( 'NONE', *, *, #8795, .T. ) ;
#33451 = CARTESIAN_POINT ( 'NONE',  ( 13.80796782207779927, -52.11465364279959545, -75.47164421335219231 ) ) ;
#33452 = ADVANCED_FACE ( 'NONE', ( #47858 ), #42755, .T. ) ;
#33453 = CARTESIAN_POINT ( 'NONE',  ( 47.21413493457389876, -54.78279301590860229, -54.62721521096310084 ) ) ;
#33454 = DIRECTION ( 'NONE',  ( 0.8660254037844387076, 0.4999999999999998890, 0.000000000000000000 ) ) ;
#33455 = CARTESIAN_POINT ( 'NONE',  ( 11.20590614225525350, 32.84406522011376239, -44.01467685474590752 ) ) ;
#33456 = EDGE_CURVE ( 'NONE', #49499, #26299, #24528, .T. ) ;
#33457 = CARTESIAN_POINT ( 'NONE',  ( 23.23758385637279744, -14.43887883678110029, -32.14999999999999858 ) ) ;
#33458 = CARTESIAN_POINT ( 'NONE',  ( 54.76549986477987630, -46.18104396004290635, -15.95313387964988472 ) ) ;
#33459 = EDGE_CURVE ( 'NONE', #434, #51110, #32419, .T. ) ;
#33460 = CARTESIAN_POINT ( 'NONE',  ( 64.93393739769619799, 11.23736444591397543, -61.59644660940672622 ) ) ;
#33462 = CARTESIAN_POINT ( 'NONE',  ( 10.11250238224864617, -10.41121846697807030, -44.73474056346155692 ) ) ;
#33461 = CARTESIAN_POINT ( 'NONE',  ( 13.99025901349430079, 19.94838289624579986, -22.90514568906469961 ) ) ;
#33463 = VECTOR ( 'NONE', #22691, 1000.000000000000000 ) ;
#33464 = CARTESIAN_POINT ( 'NONE',  ( 56.27102116988059777, 19.34483839479189982, -52.87264356866189985 ) ) ;
#33465 = APPLICATION_CONTEXT ( 'automotive_design' ) ;
#33466 = CARTESIAN_POINT ( 'NONE',  ( 48.03928511041160476, 23.04428228824039948, -54.71294081448219515 ) ) ;
#33467 = AXIS2_PLACEMENT_3D ( 'NONE', #25751, #29178, #1932 ) ;
#33468 = ORIENTED_EDGE ( 'NONE', *, *, #42227, .F. ) ;
#33469 = CARTESIAN_POINT ( 'NONE',  ( 16.96763219941080081, -8.612796041803930436, -62.38489440685859222 ) ) ;
#33470 = ORIENTED_EDGE ( 'NONE', *, *, #22386, .F. ) ;
#33471 = AXIS2_PLACEMENT_3D ( 'NONE', #8812, #29226, #44969 ) ;
#33472 = CARTESIAN_POINT ( 'NONE',  ( 16.13393739769620083, -15.61618894467929941, 17.35000000000000142 ) ) ;
#33473 = CARTESIAN_POINT ( 'NONE',  ( 22.90093739769620029, -15.61618894467913243, -28.45282021618999835 ) ) ;
#33475 = CARTESIAN_POINT ( 'NONE',  ( 53.08725068471199648, 18.06569830069809868, -26.91751262120149590 ) ) ;
#33474 = CARTESIAN_POINT ( 'NONE',  ( 83.73985275199801492, 13.43641148183490053, -47.11072319708490141 ) ) ;
#33476 = CIRCLE ( 'NONE', #5885, 39.00000000000000711 ) ;
#33477 = CARTESIAN_POINT ( 'NONE',  ( 19.96964979656319983, -21.53479258825970177, -74.76978491222709522 ) ) ;
#33478 = CIRCLE ( 'NONE', #19275, 2.000000000000070166 ) ;
#33479 = CARTESIAN_POINT ( 'NONE',  ( 11.06646955189524029, 33.78253783233923713, -17.18453609578202190 ) ) ;
#33480 = CARTESIAN_POINT ( 'NONE',  ( 64.93393739769619799, 10.88381105532070059, -61.94999999999999574 ) ) ;
#33481 = B_SPLINE_SURFACE_WITH_KNOTS ( 'NONE', 3, 3, ( 
 ( #27438, #43695, #4112, #27182, #3353, #15660, #51559, #35573, #31613, #43951, #44205, #39251 ),
 ( #24002, #7284, #40022, #19327, #51308, #11738, #15402, #43441, #8051, #20089, #47631, #437 ),
 ( #31356, #31872, #36080, #185, #7544, #43189, #12241, #32122, #27697, #19837, #3867, #4369 ),
 ( #16425, #28204, #11218, #19582, #7798, #48140, #8303, #32380, #23488, #23234, #47889, #51811 ) ),
 .UNSPECIFIED., .F., .F., .F.,
 ( 4, 4 ),
 ( 4, 1, 1, 1, 1, 1, 1, 1, 1, 4 ),
 ( -5.132488013533590632, -5.003182328417289604 ),
 ( 0.000000000000000000, 0.1111111111111110078, 0.2222222222222219878, 0.3333333333333329818, 0.4444444444444439757, 0.5555555555555560243, 0.6666666666666670737, 0.7777777777777779011, 0.8888888888888889506, 1.000000000000000000 ),
 .UNSPECIFIED. ) ;
#33482 = CARTESIAN_POINT ( 'NONE',  ( 6.430637565411768897, -15.61618894467929941, -22.14999999999999858 ) ) ;
#33483 = ORIENTED_EDGE ( 'NONE', *, *, #45012, .T. ) ;
#33484 = ADVANCED_FACE ( 'NONE', ( #48442 ), #23710, .F. ) ;
#33485 = ORIENTED_EDGE ( 'NONE', *, *, #50004, .F. ) ;
#33486 = CARTESIAN_POINT ( 'NONE',  ( 11.91426296010549990, -65.11770545154290346, -16.60966417101620252 ) ) ;
#33487 = CARTESIAN_POINT ( 'NONE',  ( 12.64317103172330015, 34.24372746930500000, -47.41952126075570106 ) ) ;
#33488 = DIRECTION ( 'NONE',  ( 0.9223605572461988089, 0.3863301728269249447, 0.000000000000000000 ) ) ;
#33489 = CARTESIAN_POINT ( 'NONE',  ( 12.04090198311089921, 33.96751094227059298, -45.84253678999650106 ) ) ;
#33490 = CARTESIAN_POINT ( 'NONE',  ( 12.89074585038019904, -65.51103569873420440, -47.72398483063609831 ) ) ;
#33491 = ORIENTED_EDGE ( 'NONE', *, *, #5449, .F. ) ;
#33492 = CARTESIAN_POINT ( 'NONE',  ( -1.470455565318980140, -50.51083130937980314, -36.42379920433069884 ) ) ;
#33493 = CARTESIAN_POINT ( 'NONE',  ( 53.50527167498405845, 17.84081837129114234, -27.26089937317538769 ) ) ;
#33494 = CARTESIAN_POINT ( 'NONE',  ( 53.15617301329960043, -49.54407833428120256, -49.11047178172640315 ) ) ;
#33495 = CARTESIAN_POINT ( 'NONE',  ( 48.46496422664660031, 22.55782414888539833, -53.44104536398719318 ) ) ;
#33496 = CARTESIAN_POINT ( 'NONE',  ( 61.57715961643649649, -1.766643160980349903, -16.00619826694699910 ) ) ;
#33497 = CARTESIAN_POINT ( 'NONE',  ( 50.83387910135749621, -49.74010978817180018, -76.22448499253579257 ) ) ;
#33498 = AXIS2_PLACEMENT_3D ( 'NONE', #27716, #3118, #11501 ) ;
#33499 = DIRECTION ( 'NONE',  ( -1.000000000000000000, 0.000000000000000000, 0.000000000000000000 ) ) ;
#33500 = VERTEX_POINT ( 'NONE', #12543 ) ;
#33501 = CARTESIAN_POINT ( 'NONE',  ( 53.00983118628400348, -49.38275580526859443, -27.01103834705430273 ) ) ;
#33502 = CARTESIAN_POINT ( 'NONE',  ( 29.13393739769619728, 1.883811055320659955, -53.85091742636659973 ) ) ;
#33503 = EDGE_LOOP ( 'NONE', ( #35373, #26882, #26129, #17202, #48115, #10934 ) ) ;
#33504 = DIRECTION ( 'NONE',  ( 0.000000000000000000, 0.000000000000000000, -1.000000000000000000 ) ) ;
#33505 = CARTESIAN_POINT ( 'NONE',  ( -8.766062602303849260, -15.61618894467929941, 4.449999999999981526 ) ) ;
#33506 = ADVANCED_FACE ( 'NONE', ( #8350 ), #20642, .F. ) ;
#33507 = CARTESIAN_POINT ( 'NONE',  ( 16.23647018767980299, -23.86072634112229807, -80.28837282723650048 ) ) ;
#33508 = DIRECTION ( 'NONE',  ( 0.000000000000000000, 0.000000000000000000, -1.000000000000000000 ) ) ;
#33509 = CARTESIAN_POINT ( 'NONE',  ( 55.37640121169410179, 19.59244258161170293, -75.41624985117930180 ) ) ;
#33510 = CARTESIAN_POINT ( 'NONE',  ( 46.64206449348299799, -53.27165255397410704, -76.10218428122850298 ) ) ;
#33511 = EDGE_LOOP ( 'NONE', ( #1214, #4939, #33485, #40019 ) ) ;
#33512 = AXIS2_PLACEMENT_3D ( 'NONE', #41770, #29956, #6398 ) ;
#33513 = CARTESIAN_POINT ( 'NONE',  ( 56.13905073043380156, 14.31243755683419927, -17.10657833413849715 ) ) ;
#33514 = AXIS2_PLACEMENT_3D ( 'NONE', #50653, #5857, #10309 ) ;
#33515 = CARTESIAN_POINT ( 'NONE',  ( 56.95883376355960337, -50.25507440355580258, -52.69722347720740174 ) ) ;
#33516 = TOROIDAL_SURFACE ( 'NONE', #10938, 19.56371635397779940, 1.000000000000000000 ) ;
#33517 = CARTESIAN_POINT ( 'NONE',  ( 17.35001377175319703, -22.56339827118789998, -35.29201998310079347 ) ) ;
#33518 = CARTESIAN_POINT ( 'NONE',  ( 22.79012786898881160, -13.80047699738691591, -44.76177760185372279 ) ) ;
#33519 = CIRCLE ( 'NONE', #90, 2.999999999999999112 ) ;
#33520 = ORIENTED_EDGE ( 'NONE', *, *, #30330, .T. ) ;
#33521 = CARTESIAN_POINT ( 'NONE',  ( 46.95813824399459691, 22.72792253046040400, -75.76112237679920725 ) ) ;
#33522 = CARTESIAN_POINT ( 'NONE',  ( 65.09331375576360301, 1.276058558775509999, -60.69120887205459525 ) ) ;
#33523 = CARTESIAN_POINT ( 'NONE',  ( 41.03170894472499697, -45.48949944206719920, -6.001457922227690034 ) ) ;
#33524 = CARTESIAN_POINT ( 'NONE',  ( 53.35699421374690132, -49.92639189236809472, -74.14999999999999147 ) ) ;
#33525 = CARTESIAN_POINT ( 'NONE',  ( 7.936097814644250903, -16.49832144022300184, -80.47354794880769191 ) ) ;
#33526 = ADVANCED_FACE ( 'NONE', ( #27482 ), #43834, .T. ) ;
#33527 = CARTESIAN_POINT ( 'NONE',  ( 68.13393739769630031, -48.11618894467930119, -73.25000000000000000 ) ) ;
#33528 = DIRECTION ( 'NONE',  ( 0.000000000000000000, 0.000000000000000000, -1.000000000000000000 ) ) ;
#33530 = CARTESIAN_POINT ( 'NONE',  ( 42.54468173148520549, -37.68289285273589684, -77.59564625393689141 ) ) ;
#33529 = DIRECTION ( 'NONE',  ( -1.000000000000000000, -1.004313591354993529E-15, 0.000000000000000000 ) ) ;
#33531 = CARTESIAN_POINT ( 'NONE',  ( 61.09392091072469810, 14.09871518747650043, -46.81036500987260496 ) ) ;
#33532 = CARTESIAN_POINT ( 'NONE',  ( -33.78933650424870194, -20.47497671886300097, -57.07866011716559740 ) ) ;
#33533 = VERTEX_POINT ( 'NONE', #12285 ) ;
#33534 = CARTESIAN_POINT ( 'NONE',  ( 52.96856324676929262, -49.58863183502440108, -48.80184355050319311 ) ) ;
#33535 = EDGE_LOOP ( 'NONE', ( #25518, #43807, #20236, #41496, #14932 ) ) ;
#33536 = CARTESIAN_POINT ( 'NONE',  ( 57.90400457952389957, -45.28151604584450496, -25.97936526911970034 ) ) ;
#33537 = CARTESIAN_POINT ( 'NONE',  ( 49.13578581667099598, -53.89835027320579997, -55.25235944000660027 ) ) ;
#33538 = CARTESIAN_POINT ( 'NONE',  ( 13.48899612010369964, 19.59108034571840307, -21.59023847590369982 ) ) ;
#33539 = CARTESIAN_POINT ( 'NONE',  ( 56.70205649827579464, 14.05047582634010084, -25.29386163676009858 ) ) ;
#33540 = CARTESIAN_POINT ( 'NONE',  ( 22.57606680859020187, -18.48699499001489954, -36.58626013956269674 ) ) ;
#33541 = CARTESIAN_POINT ( 'NONE',  ( 28.90964706005109974, -26.65681833330370054, -34.73148477628539865 ) ) ;
#33542 = CARTESIAN_POINT ( 'NONE',  ( 53.03258583333429499, 18.34312913753139895, -48.98438925658670229 ) ) ;
#33543 = CARTESIAN_POINT ( 'NONE',  ( 60.67083030670429622, -45.55276209844719659, -47.13425158708550100 ) ) ;
#33544 = CARTESIAN_POINT ( 'NONE',  ( 47.20214428756302283, 22.74469374127451360, -75.65864031409697077 ) ) ;
#33545 = ORIENTED_EDGE ( 'NONE', *, *, #38966, .F. ) ;
#33546 = ADVANCED_BREP_SHAPE_REPRESENTATION ( '', ( #9246, #20940 ), #40219 ) ;
#33547 = CARTESIAN_POINT ( 'NONE',  ( 8.836677506919789593, -14.11395979259429900, -78.13196779797900149 ) ) ;
#33548 = CARTESIAN_POINT ( 'NONE',  ( 72.97593009921529017, 1.263903724274369811, -62.37965189720969761 ) ) ;
#33549 = CARTESIAN_POINT ( 'NONE',  ( 72.78175560864718818, 1.385702546077159925, -68.77407799673838440 ) ) ;
#33550 = CARTESIAN_POINT ( 'NONE',  ( 47.41106868612380509, -54.65034373980500249, -54.82892287975980139 ) ) ;
#33551 = CARTESIAN_POINT ( 'NONE',  ( 9.239619369984774622, -11.66024772074672633, -48.95806641941920390 ) ) ;
#33552 = CARTESIAN_POINT ( 'NONE',  ( 73.06384957064030061, 1.187237555532410171, -62.39609834743819761 ) ) ;
#33553 = CARTESIAN_POINT ( 'NONE',  ( 11.45636326040439990, -65.36476201173780964, -18.01147071083120110 ) ) ;
#33554 = CARTESIAN_POINT ( 'NONE',  ( 53.20761889774500020, 18.23056977116540267, -48.79936051936330443 ) ) ;
#33555 = CARTESIAN_POINT ( 'NONE',  ( 50.03007040746459921, 17.38381105532069881, -78.14999999999999147 ) ) ;
#33556 = CARTESIAN_POINT ( 'NONE',  ( 13.61287798883271272, -9.318081818693075391, -61.83160618788794949 ) ) ;
#33557 = AXIS2_PLACEMENT_3D ( 'NONE', #41823, #46292, #1737 ) ;
#33558 = AXIS2_PLACEMENT_3D ( 'NONE', #33228, #10436, #50008 ) ;
#33559 = CARTESIAN_POINT ( 'NONE',  ( 9.142468753586408425, -19.44231997591093375, -46.34810776502081353 ) ) ;
#33560 = CARTESIAN_POINT ( 'NONE',  ( 64.94442696602180831, 1.326324093417230232, -70.44093178352311213 ) ) ;
#33561 = ORIENTED_EDGE ( 'NONE', *, *, #3135, .F. ) ;
#33562 = CARTESIAN_POINT ( 'NONE',  ( 8.972284714083951229, -63.24474060077910309, -46.63284625306040709 ) ) ;
#33563 = CARTESIAN_POINT ( 'NONE',  ( 20.63393739769620083, -41.61618894467930119, -54.64999999999999858 ) ) ;
#33564 = ORIENTED_EDGE ( 'NONE', *, *, #24161, .F. ) ;
#33565 = CARTESIAN_POINT ( 'NONE',  ( -23.72016456855327249, -47.08947743092473814, 10.84999999999999964 ) ) ;
#33566 = CARTESIAN_POINT ( 'NONE',  ( 16.13393739769620083, -15.61618894467929941, -16.88999999999999702 ) ) ;
#33567 = CARTESIAN_POINT ( 'NONE',  ( -3.839728563314020349, -6.393788602144800493, -54.64999999999999858 ) ) ;
#33568 = CARTESIAN_POINT ( 'NONE',  ( 51.63598265732919401, 19.13823475874330171, -76.35349669905959047 ) ) ;
#33569 = ORIENTED_EDGE ( 'NONE', *, *, #20132, .T. ) ;
#33570 = DIRECTION ( 'NONE',  ( 1.000000000000000000, 0.000000000000000000, 0.000000000000000000 ) ) ;
#33571 = DIRECTION ( 'NONE',  ( 0.000000000000000000, -1.000000000000000000, 0.000000000000000000 ) ) ;
#33572 = DIRECTION ( 'NONE',  ( 0.000000000000000000, -1.000000000000000000, 0.000000000000000000 ) ) ;
#33573 = EDGE_CURVE ( 'NONE', #43431, #33091, #44482, .T. ) ;
#33574 = CARTESIAN_POINT ( 'NONE',  ( 8.519820190432819018, -12.45265623424450041, -48.91767612604329685 ) ) ;
#33575 = EDGE_CURVE ( 'NONE', #51520, #6375, #41318, .T. ) ;
#33576 = CARTESIAN_POINT ( 'NONE',  ( 16.13393739769620083, -15.61618894467929941, -15.65000000000000036 ) ) ;
#33577 = CARTESIAN_POINT ( 'NONE',  ( 44.54563194250441427, -37.98763156856614387, -67.59149508629086256 ) ) ;
#33578 = ADVANCED_FACE ( 'NONE', ( #20129 ), #31401, .F. ) ;
#33579 = ORIENTED_EDGE ( 'NONE', *, *, #17263, .T. ) ;
#33580 = DIRECTION ( 'NONE',  ( 0.000000000000000000, 1.000000000000000000, 0.000000000000000000 ) ) ;
#33581 = CARTESIAN_POINT ( 'NONE',  ( 20.27276998682100029, -21.81108673272580134, -42.54517385987409739 ) ) ;
#33582 = CARTESIAN_POINT ( 'NONE',  ( 8.428805570490940369, -13.54562505507219505, -32.59100129534225943 ) ) ;
#33583 = B_SPLINE_CURVE_WITH_KNOTS ( 'NONE', 3,
 ( #6162, #46907, #6805, #31390, #47162, #2871, #31134, #34819, #11250, #50823, #26958, #10732, #10477, #14913, #19615, #35339, #38779, #26432 ),
 .UNSPECIFIED., .F., .F.,
 ( 4, 2, 2, 2, 2, 2, 2, 2, 4 ),
 ( 0.000000000000000000, 0.2367787920637725030, 0.3749999997961399045, 0.4999999998369116239, 0.5624999998572962623, 0.6624999998899127052, 0.8224999999420987695, 0.9835460370430810784, 1.000000000000000000 ),
 .UNSPECIFIED. ) ;
#33584 = CARTESIAN_POINT ( 'NONE',  ( 13.76193600395860095, 20.63771170940629673, -75.29799846200430125 ) ) ;
#33585 = CYLINDRICAL_SURFACE ( 'NONE', #32338, 7.910999999999997812 ) ;
#33586 = CARTESIAN_POINT ( 'NONE',  ( 44.89309739530899179, -45.25428046396859827, -7.755542271532889664 ) ) ;
#33587 = VECTOR ( 'NONE', #7400, 1000.000000000000000 ) ;
#33588 = CARTESIAN_POINT ( 'NONE',  ( 24.01463920420174603, -14.90188333430748280, -61.47890500563420346 ) ) ;
#33589 = VECTOR ( 'NONE', #28854, 1000.000000000000000 ) ;
#33590 = CARTESIAN_POINT ( 'NONE',  ( 23.69903331857869944, -18.89521996265120052, -51.63785704165039192 ) ) ;
#33591 = EDGE_CURVE ( 'NONE', #42649, #37266, #7847, .T. ) ;
#33592 = VERTEX_POINT ( 'NONE', #43484 ) ;
#33593 = CARTESIAN_POINT ( 'NONE',  ( 54.46658371067870519, -47.81044456346369742, -26.27512462187450026 ) ) ;
#33594 = CARTESIAN_POINT ( 'NONE',  ( 55.98501704304129589, -50.87010798429000147, -74.79194691214389934 ) ) ;
#33595 = CARTESIAN_POINT ( 'NONE',  ( 5.995642857577959894, 28.70634236700130160, -13.38692505553090051 ) ) ;
#33596 = CARTESIAN_POINT ( 'NONE',  ( 22.23393739769620225, -15.61618894467929941, 14.34999999999999964 ) ) ;
#33597 = CARTESIAN_POINT ( 'NONE',  ( 52.33304160529149840, 14.99038499564479920, -14.16116536265050030 ) ) ;
#33598 = ORIENTED_EDGE ( 'NONE', *, *, #48245, .F. ) ;
#33599 = CARTESIAN_POINT ( 'NONE',  ( -10.88446022757939957, -42.34476442307779820, -6.227089099853370335 ) ) ;
#33600 = CARTESIAN_POINT ( 'NONE',  ( 47.43324995648460174, 23.39942513964739845, -54.73919042832569914 ) ) ;
#33601 = DIRECTION ( 'NONE',  ( 0.000000000000000000, 0.000000000000000000, -1.000000000000000000 ) ) ;
#33602 = CARTESIAN_POINT ( 'NONE',  ( 63.46249669555339779, 1.383767307422969939, -62.59255479634269648 ) ) ;
#33603 = CARTESIAN_POINT ( 'NONE',  ( 60.67373779709330250, 14.31886089341139900, -47.14825094286950247 ) ) ;
#33604 = CARTESIAN_POINT ( 'NONE',  ( 11.93174564592089837, 34.20691397436080194, -17.93019396377509977 ) ) ;
#33605 = CARTESIAN_POINT ( 'NONE',  ( 51.95832322464790565, 18.21933309198920270, -77.09973926587740323 ) ) ;
#33606 = CARTESIAN_POINT ( 'NONE',  ( 53.13663690894949809, 18.26775922387509965, -48.80285956119419666 ) ) ;
#33607 = CARTESIAN_POINT ( 'NONE',  ( 35.31742556088838825, 11.23513843205707019, -54.64999999999999858 ) ) ;
#33608 = DIRECTION ( 'NONE',  ( 0.000000000000000000, 0.000000000000000000, 1.000000000000000000 ) ) ;
#33609 = CARTESIAN_POINT ( 'NONE',  ( 54.27276165828439503, 17.15419499903419975, -26.87182491303840237 ) ) ;
#33610 = CARTESIAN_POINT ( 'NONE',  ( 52.83203762323750396, 21.09151004990239997, -54.28847891111020374 ) ) ;
#33611 = CARTESIAN_POINT ( 'NONE',  ( 63.58222404636121183, 1.087299280848000205, -69.55154624241478700 ) ) ;
#33612 = CARTESIAN_POINT ( 'NONE',  ( 12.04669084400330092, -65.33956968768698914, -17.12210552323070090 ) ) ;
#33613 = CARTESIAN_POINT ( 'NONE',  ( 22.90093737578363786, -14.73039410641558611, -48.41115546478060594 ) ) ;
#33614 = VERTEX_POINT ( 'NONE', #47429 ) ;
#33615 = DIRECTION ( 'NONE',  ( -1.224646936193269808E-16, 1.000000000000000000, 3.054623595244969840E-12 ) ) ;
#33616 = CARTESIAN_POINT ( 'NONE',  ( 10.77143137424659969, 32.00294380475830280, -45.20466975612399807 ) ) ;
#33617 = DIRECTION ( 'NONE',  ( 0.000000000000000000, -0.7071067811865492381, 0.7071067811865457964 ) ) ;
#33618 = CARTESIAN_POINT ( 'NONE',  ( 13.91520078321919840, -8.088981630189278960, -81.23899999999999011 ) ) ;
#33619 = CARTESIAN_POINT ( 'NONE',  ( 12.33744638055669363, 24.20302978297883811, -75.02878472494597872 ) ) ;
#33620 = ORIENTED_EDGE ( 'NONE', *, *, #14592, .T. ) ;
#33621 = ORIENTED_EDGE ( 'NONE', *, *, #6759, .T. ) ;
#33622 = CARTESIAN_POINT ( 'NONE',  ( 14.06336448650593063, -23.32131646376723211, -80.09100261305252388 ) ) ;
#33623 = ORIENTED_EDGE ( 'NONE', *, *, #47243, .T. ) ;
#33624 = CARTESIAN_POINT ( 'NONE',  ( 11.90135363455309836, -65.25553501546980328, -46.97006170066550368 ) ) ;
#33625 = CARTESIAN_POINT ( 'NONE',  ( 57.47999491983949838, -45.29966141242730515, -25.92515611446150103 ) ) ;
#33626 = LINE ( 'NONE', #50144, #44552 ) ;
#33627 = CONICAL_SURFACE ( 'NONE', #51196, 0.6300000000000018918, 0.7853981633974476129 ) ;
#33628 = LINE ( 'NONE', #42028, #4192 ) ;
#33629 = ORIENTED_EDGE ( 'NONE', *, *, #45563, .F. ) ;
#33630 = AXIS2_PLACEMENT_3D ( 'NONE', #48919, #41293, #8557 ) ;
#33631 = CARTESIAN_POINT ( 'NONE',  ( 75.08786029787904681, -6.316746508337682364, -11.49520958555957328 ) ) ;
#33632 = ORIENTED_EDGE ( 'NONE', *, *, #8384, .T. ) ;
#33633 = CARTESIAN_POINT ( 'NONE',  ( 48.66686317495700109, -45.95722105086829856, -11.36446868152489920 ) ) ;
#33634 = EDGE_CURVE ( 'NONE', #26465, #42921, #41278, .T. ) ;
#33635 = CARTESIAN_POINT ( 'NONE',  ( 53.63393739769619373, -53.11618894467930119, 16.35000000000000142 ) ) ;
#33636 = CARTESIAN_POINT ( 'NONE',  ( 14.04279605691050037, 19.71127979334969993, -21.72007173762010268 ) ) ;
#33637 = LINE ( 'NONE', #49654, #23433 ) ;
#33638 = EDGE_CURVE ( 'NONE', #29187, #2702, #29561, .T. ) ;
#33639 = ORIENTED_EDGE ( 'NONE', *, *, #30807, .F. ) ;
#33640 = CARTESIAN_POINT ( 'NONE',  ( 73.08672326322148649, 0.8966068345641430293, -69.03681046574689617 ) ) ;
#33641 = CARTESIAN_POINT ( 'NONE',  ( 46.40452006446609801, -53.01824288504249694, -76.14999999999999147 ) ) ;
#33642 = CARTESIAN_POINT ( 'NONE',  ( 72.75000907364700709, 13.88381105527210124, -14.68250626227150057 ) ) ;
#33643 = CARTESIAN_POINT ( 'NONE',  ( 46.46977925592499759, 13.88381105525470005, -8.151821053502690262 ) ) ;
#33644 = CARTESIAN_POINT ( 'NONE',  ( 14.28038400710302724, 10.53025766472732450, -34.79644660940672907 ) ) ;
#33645 = CARTESIAN_POINT ( 'NONE',  ( 51.84413674030060548, 20.10506014047289725, -76.02231598272810231 ) ) ;
#33646 = CARTESIAN_POINT ( 'NONE',  ( 61.60313986292270272, 13.88613617178600101, -27.62773227502630391 ) ) ;
#33647 = CARTESIAN_POINT ( 'NONE',  ( 13.70687704985900091, -8.153205208187619846, -68.68742111086849889 ) ) ;
#33648 = ADVANCED_FACE ( 'NONE', ( #23534 ), #28246, .F. ) ;
#33649 = ORIENTED_EDGE ( 'NONE', *, *, #51576, .F. ) ;
#33650 = CARTESIAN_POINT ( 'NONE',  ( 68.13393739769620083, 18.13381105532069881, -75.00000000000000000 ) ) ;
#33651 = CARTESIAN_POINT ( 'NONE',  ( 73.24758132965830271, 0.8838110553206740549, -62.51131646858519275 ) ) ;
#33652 = CARTESIAN_POINT ( 'NONE',  ( 75.70738240145129794, -43.41214489997439330, -13.47559953613099992 ) ) ;
#33653 = EDGE_CURVE ( 'NONE', #20243, #25615, #34301, .T. ) ;
#33654 = B_SPLINE_CURVE_WITH_KNOTS ( 'NONE', 3,
 ( #27853, #48819, #43854, #4021, #20239, #20493, #16574, #51715, #16067, #15809, #32023, #31770, #19982, #35976, #95, #48048, #24154, #36229, #32277, #33332, #1635, #8989, #25977, #37016, #41991, #51012, #2803, #30812 ),
 .UNSPECIFIED., .F., .F.,
 ( 4, 2, 2, 2, 2, 2, 2, 2, 2, 2, 2, 2, 2, 4 ),
 ( 0.5000051609194220426, 0.5625045158044944538, 0.6250038706895668650, 0.6875032255746391652, 0.7187529030171753153, 0.7500025804597113543, 0.7812522579022473934, 0.8125019353447835435, 0.8437516127873195826, 0.8750012902298556217, 0.9062509676723917718, 0.9375006451149278108, 0.9687503225574638499, 1.000000000000000000 ),
 .UNSPECIFIED. ) ;
#33655 = CARTESIAN_POINT ( 'NONE',  ( 72.84263360082020711, 1.236214136008370046, -69.21416709495440500 ) ) ;
#33656 = AXIS2_PLACEMENT_3D ( 'NONE', #21724, #20953, #780 ) ;
#33657 = FACE_OUTER_BOUND ( 'NONE', #34608, .T. ) ;
#33658 = DIRECTION ( 'NONE',  ( -1.397030999999999991E-10, 0.000000000000000000, 1.000000000000000000 ) ) ;
#33659 = CARTESIAN_POINT ( 'NONE',  ( 14.06315214856010698, -7.911116337559645828, -59.20904473871448204 ) ) ;
#33660 = CARTESIAN_POINT ( 'NONE',  ( 49.47431290566419904, -53.75415064111020058, -55.14222552823530776 ) ) ;
#33661 = CARTESIAN_POINT ( 'NONE',  ( 15.09828672688668760, -23.52717647678493051, -56.33401646506906246 ) ) ;
#33662 = CARTESIAN_POINT ( 'NONE',  ( -1.143840380081567076, -15.61618894467929941, -35.76111111111109864 ) ) ;
#33663 = CARTESIAN_POINT ( 'NONE',  ( 54.39599759010950208, -51.37714874329260084, -53.12073448206449910 ) ) ;
#33664 = EDGE_LOOP ( 'NONE', ( #10038, #1069, #48601, #12427, #47877, #41752 ) ) ;
#33665 = CARTESIAN_POINT ( 'NONE',  ( 23.17219357687709902, -13.17290339146140177, -58.96098648058299574 ) ) ;
#33666 = CARTESIAN_POINT ( 'NONE',  ( 64.37933009232320103, 1.063298638255609996, -60.97768308011880123 ) ) ;
#33667 = ORIENTED_EDGE ( 'NONE', *, *, #43621, .T. ) ;
#33668 = CARTESIAN_POINT ( 'NONE',  ( 19.38808262899626556, -9.358945304425906997, -34.49983067246480317 ) ) ;
#33669 = CARTESIAN_POINT ( 'NONE',  ( 60.82607126368439765, -45.62681756021819979, -47.60724346531519302 ) ) ;
#33670 = DIRECTION ( 'NONE',  ( -1.000000000000000000, 0.000000000000000000, 0.000000000000000000 ) ) ;
#33671 = CARTESIAN_POINT ( 'NONE',  ( 8.428808952652845576, -17.68676381052137003, -62.42431570012554687 ) ) ;
#33673 = CARTESIAN_POINT ( 'NONE',  ( 22.90060991778284816, -15.13913409275305888, -54.82474789397813453 ) ) ;
#33672 = CARTESIAN_POINT ( 'NONE',  ( 43.96339835255960082, 8.719345853256658785, -66.83668497728366731 ) ) ;
#33674 = DIRECTION ( 'NONE',  ( 0.000000000000000000, 0.000000000000000000, -1.000000000000000000 ) ) ;
#33675 = CYLINDRICAL_SURFACE ( 'NONE', #17734, 2.000000000000000888 ) ;
#33676 = EDGE_LOOP ( 'NONE', ( #10247, #40538, #11103, #9421 ) ) ;
#33677 = ORIENTED_EDGE ( 'NONE', *, *, #32075, .F. ) ;
#33678 = EDGE_LOOP ( 'NONE', ( #40208, #413, #7988, #50603, #43892, #18961 ) ) ;
#33679 = ORIENTED_EDGE ( 'NONE', *, *, #38391, .T. ) ;
#33680 = CARTESIAN_POINT ( 'NONE',  ( -22.84941987848104006, -15.84866128047474376, -54.74989008055889883 ) ) ;
#33681 = CARTESIAN_POINT ( 'NONE',  ( 53.16328977476479878, -49.55862968577820027, -49.15589875833449440 ) ) ;
#33682 = CARTESIAN_POINT ( 'NONE',  ( 49.31207000326343604, -53.03483995837590470, -52.41064504672193891 ) ) ;
#33683 = CARTESIAN_POINT ( 'NONE',  ( 56.54475643210220426, -50.74241129021329755, -53.72841466469270699 ) ) ;
#33684 = ORIENTED_EDGE ( 'NONE', *, *, #7554, .F. ) ;
#33685 = ORIENTED_EDGE ( 'NONE', *, *, #20720, .F. ) ;
#33686 = CARTESIAN_POINT ( 'NONE',  ( 22.84664585888298660, -16.49986012204790953, -72.49448347767508949 ) ) ;
#33687 = EDGE_CURVE ( 'NONE', #25181, #36007, #26231, .T. ) ;
#33688 = DIRECTION ( 'NONE',  ( 0.000000000000000000, 0.000000000000000000, -1.000000000000000000 ) ) ;
#33689 = CARTESIAN_POINT ( 'NONE',  ( 22.90093381512099668, -15.61618921778096336, -54.45281771551935890 ) ) ;
#33690 = AXIS2_PLACEMENT_3D ( 'NONE', #41695, #25947, #22981 ) ;
#33691 = ORIENTED_EDGE ( 'NONE', *, *, #19140, .F. ) ;
#33692 = CARTESIAN_POINT ( 'NONE',  ( 24.03897853505547033, -15.94809715369253844, -49.52101926789728736 ) ) ;
#33694 = CARTESIAN_POINT ( 'NONE',  ( 52.02578741164499831, -50.58705193961559843, -76.37778590614399832 ) ) ;
#33693 = VECTOR ( 'NONE', #29315, 1000.000000000000000 ) ;
#33695 = LINE ( 'NONE', #17219, #48798 ) ;
#33696 = CARTESIAN_POINT ( 'NONE',  ( 13.88388657071990018, -23.13443467540700027, -62.60505730950970360 ) ) ;
#33697 = B_SPLINE_CURVE_WITH_KNOTS ( 'NONE', 3,
 ( #12060, #47196, #27245, #28011, #34856, #30912, #44018, #7099, #35890, #43761, #11283, #50855 ),
 .UNSPECIFIED., .F., .F.,
 ( 4, 2, 2, 2, 2, 4 ),
 ( 0.000000000000000000, 0.06094059512925743827, 0.2755827044638499701, 0.4977784882754372475, 0.7891864372720736043, 1.000000000000000000 ),
 .UNSPECIFIED. ) ;
#33698 = CARTESIAN_POINT ( 'NONE',  ( 2.458146360389407370, -5.580163940743402051, -34.79644291222906105 ) ) ;
#33699 = CARTESIAN_POINT ( 'NONE',  ( 44.42525669626399321, 14.02755080800340082, -7.504247777814939901 ) ) ;
#33700 = CARTESIAN_POINT ( 'NONE',  ( 41.14792718230170010, -44.23795256543909460, -3.958129521531580597 ) ) ;
#33701 = CARTESIAN_POINT ( 'NONE',  ( 68.13393739769841773, -50.61618894467878960, -73.25000000000220268 ) ) ;
#33702 = CARTESIAN_POINT ( 'NONE',  ( -8.870287765918970280, 13.09110620826400151, -5.844096418666690163 ) ) ;
#33703 = CARTESIAN_POINT ( 'NONE',  ( 63.64944581154209402, 1.039768281806159989, -69.63739004519409548 ) ) ;
#33704 = CARTESIAN_POINT ( 'NONE',  ( 11.95218966202808275, -21.29558555530721975, -33.54920349970121407 ) ) ;
#33705 = CARTESIAN_POINT ( 'NONE',  ( 67.52398157331388973, 0.6199779298166340213, -18.22677178226010142 ) ) ;
#33706 = B_SPLINE_SURFACE_WITH_KNOTS ( 'NONE', 3, 3, ( 
 ( #22320, #2416, #46207, #50388, #30705, #46727, #17638, #9777, #2166, #1907, #13712, #33605, #29666, #49619, #25728, #5841, #49871, #22060 ),
 ( #38070, #34111, #50122, #14472, #10292, #30445, #46466, #10554, #26511, #42527, #39110, #19175, #15512, #43043, #35684, #22833, #3465, #11849 ),
 ( #26770, #45, #50897, #51162, #42788, #47741, #3973, #3203, #35154, #19938, #6883, #38854, #16022, #14989, #43803, #51669, #15255, #2943 ),
 ( #31210, #15763, #27292, #27547, #27038, #19436, #47997, #31716, #7139, #7392, #11328, #27806, #7903, #3719, #18914, #30955, #19692, #34897 ),
 ( #23850, #31466, #39616, #46987, #39874, #11072, #23091, #43301, #47237, #23340, #23598, #39363, #35416, #51418, #47490, #11586, #43553, #35928 ),
 ( #31977, #7655, #48250, #12344, #540, #20702, #4735, #5268, #8940, #17316, #29092, #12097, #49035, #16526, #12874, #36693, #32476, #40378 ),
 ( #1063, #793, #28053, #48770, #45091, #32743, #48506, #28310, #24883, #44055, #4218, #36182, #33280, #16274, #28830, #40895, #5005, #13143 ),
 ( #44309, #8418, #12607, #16795, #44835, #21219, #20965, #8161, #9198, #24104, #25150, #28570, #36966, #17059, #44569, #4475, #33012, #41155 ),
 ( #40125, #37231, #1328, #20192, #8670, #289, #32227, #24366, #20444, #36432, #24625, #40636, #50057, #34047, #38005, #14153, #42463, #46403 ),
 ( #1584, #9963, #29606, #21484, #13393, #37483, #45357, #49296, #29351, #45609, #9459, #25408, #41411, #30378, #29855, #30121, #26447, #9708 ) ),
 .UNSPECIFIED., .F., .F., .F.,
 ( 4, 1, 1, 1, 1, 1, 1, 4 ),
 ( 4, 2, 2, 2, 2, 2, 2, 2, 4 ),
 ( -4.205109691999999775E-06, 0.1428571428571430157, 0.2857142857142860315, 0.4285714285714289917, 0.5714285714285709528, 0.7142857142857139685, 0.8571428571428569843, 1.000000000000000000 ),
 ( -2.552637841604540103, -2.105922750108249808, -1.595396022809280057, -1.276316818247430041, -1.116777215966499925, -0.9194146059286070205, -0.6036344298679829912, -0.09838614817098499665, 4.205109683999999746E-06 ),
 .UNSPECIFIED. ) ;
#33707 = ORIENTED_EDGE ( 'NONE', *, *, #37649, .T. ) ;
#33708 = CARTESIAN_POINT ( 'NONE',  ( 14.80174287272940070, -52.40466508994170169, -76.02664804518829555 ) ) ;
#33709 = VECTOR ( 'NONE', #51676, 1000.000000000000000 ) ;
#33710 = CARTESIAN_POINT ( 'NONE',  ( 47.21309542846500307, -54.78361656918900024, -54.62980748658569752 ) ) ;
#33711 = EDGE_CURVE ( 'NONE', #41267, #260, #13830, .T. ) ;
#33712 = PLANE ( 'NONE',  #48159 ) ;
#33713 = CARTESIAN_POINT ( 'NONE',  ( 16.13393739769620083, -15.61618894467929941, 9.349999999999999645 ) ) ;
#33714 = CARTESIAN_POINT ( 'NONE',  ( 47.11354740527600171, -54.64978104499210332, -74.95188530402140259 ) ) ;
#33715 = CARTESIAN_POINT ( 'NONE',  ( 63.18170070234948810, 0.9989215084294049696, -69.02509836011120115 ) ) ;
#33716 = CARTESIAN_POINT ( 'NONE',  ( 8.133937397696209715, -59.33545798990849818, -21.14999999999999858 ) ) ;
#33717 = CARTESIAN_POINT ( 'NONE',  ( 21.57348933224839982, -9.838876617649450651, -45.24807099536945287 ) ) ;
#33718 = CARTESIAN_POINT ( 'NONE',  ( 19.53299567489768407, -55.47150705052180086, -75.56421958049284626 ) ) ;
#33719 = CARTESIAN_POINT ( 'NONE',  ( 48.25578050111359829, 22.93468281862570279, -54.69245131324669984 ) ) ;
#33720 = ORIENTED_EDGE ( 'NONE', *, *, #41521, .F. ) ;
#33721 = TOROIDAL_SURFACE ( 'NONE', #7791, 30.50439988982899564, 1.000000000000000000 ) ;
#33722 = CARTESIAN_POINT ( 'NONE',  ( 9.706778812668741097, -18.52035693179009712, -65.71208951153059274 ) ) ;
#33723 = CIRCLE ( 'NONE', #21156, 20.00000000000000000 ) ;
#33724 = ORIENTED_EDGE ( 'NONE', *, *, #7281, .T. ) ;
#33725 = CARTESIAN_POINT ( 'NONE',  ( 10.85466640530910176, -64.96697012893029921, -17.55961383758990024 ) ) ;
#33726 = CARTESIAN_POINT ( 'NONE',  ( 82.91593256401816348, 14.33042927951009915, -47.63721988092869708 ) ) ;
#33727 = CARTESIAN_POINT ( 'NONE',  ( 19.54196835879244531, -21.52907672520979787, -42.78615316578282801 ) ) ;
#33729 = CARTESIAN_POINT ( 'NONE',  ( 52.82512926767439865, 18.35096675686759937, -27.26906326477469733 ) ) ;
#33728 = CARTESIAN_POINT ( 'NONE',  ( 83.70962855682149950, 13.38540545388440073, -46.98048264170719790 ) ) ;
#33730 = CARTESIAN_POINT ( 'NONE',  ( 17.98361080673300094, -8.810216054891400361, -76.03728780924510033 ) ) ;
#33731 = CARTESIAN_POINT ( 'NONE',  ( 11.22384627824543557, 33.78040140241473921, -16.94931753701081334 ) ) ;
#33732 = CARTESIAN_POINT ( 'NONE',  ( 72.82769086651219936, 1.383811055320669947, -68.52712657046359368 ) ) ;
#33733 = CARTESIAN_POINT ( 'NONE',  ( 9.543023349596007066, -17.38728816782158759, -41.36946782366739939 ) ) ;
#33734 = LINE ( 'NONE', #2566, #36491 ) ;
#33735 = ORIENTED_EDGE ( 'NONE', *, *, #34452, .T. ) ;
#33736 = ORIENTED_EDGE ( 'NONE', *, *, #10875, .T. ) ;
#33737 = CARTESIAN_POINT ( 'NONE',  ( 12.26282170032640195, -64.61533680211610431, -15.83707920938230096 ) ) ;
#33738 = CARTESIAN_POINT ( 'NONE',  ( 12.87771366368730064, 34.27547457673040299, -47.63452228340280215 ) ) ;
#33739 = CARTESIAN_POINT ( 'NONE',  ( 8.222924952385369579, -14.97165744064022519, -38.53361264593338120 ) ) ;
#33740 = CARTESIAN_POINT ( 'NONE',  ( 22.72481197475541848, -17.38742956073991763, -54.53615643352921438 ) ) ;
#33741 = CARTESIAN_POINT ( 'NONE',  ( 12.13162406932769954, -65.41884435375050089, -47.52833373221270108 ) ) ;
#33742 = ORIENTED_EDGE ( 'NONE', *, *, #27971, .T. ) ;
#33743 = CARTESIAN_POINT ( 'NONE',  ( -3.688670878366239858, -49.30016108328199920, -38.41768699663800390 ) ) ;
#33744 = CARTESIAN_POINT ( 'NONE',  ( -0.1295185695942999982, 0.6472670226113349523, 4.943674098299870145 ) ) ;
#33745 = EDGE_CURVE ( 'NONE', #3035, #40977, #34961, .T. ) ;
#33746 = CARTESIAN_POINT ( 'NONE',  ( 52.28488250037529639, 19.00519928096659683, -49.49583856337359578 ) ) ;
#33747 = CARTESIAN_POINT ( 'NONE',  ( 63.46371119967039931, -1.000585159038779981, -16.34221528051200067 ) ) ;
#33748 = CARTESIAN_POINT ( 'NONE',  ( 51.15450547264799752, -49.15030747453590010, -76.44814621741299732 ) ) ;
#33749 = EDGE_CURVE ( 'NONE', #43574, #30462, #39143, .T. ) ;
#33750 = CARTESIAN_POINT ( 'NONE',  ( 59.53688790405669806, -47.75280472282830146, -50.02630812161699936 ) ) ;
#33751 =( BOUNDED_CURVE ( )  B_SPLINE_CURVE ( 3, ( #39456, #3554, #19524, #51504 ),
 .UNSPECIFIED., .F., .T. ) 
 B_SPLINE_CURVE_WITH_KNOTS ( ( 4, 4 ),
 ( 0.05097448463362189847, 0.2043272503186140121 ),
 .UNSPECIFIED. ) 
 CURVE ( )  GEOMETRIC_REPRESENTATION_ITEM ( )  RATIONAL_B_SPLINE_CURVE ( ( 1.000000000000000000, 0.9980412040773742888, 0.9980412040773742888, 1.000000000000000000 ) ) 
 REPRESENTATION_ITEM ( '' )  );
#33752 = ORIENTED_EDGE ( 'NONE', *, *, #36399, .F. ) ;
#33753 = ADVANCED_FACE ( 'NONE', ( #33215 ), #9397, .T. ) ;
#33754 = CARTESIAN_POINT ( 'NONE',  ( 23.04639156216936868, -11.67809813557746956, -33.62763753640791009 ) ) ;
#33755 = CARTESIAN_POINT ( 'NONE',  ( 8.428888394969163755, -17.68705404388839142, -48.70899834144735507 ) ) ;
#33756 = ORIENTED_EDGE ( 'NONE', *, *, #36175, .T. ) ;
#33757 = CARTESIAN_POINT ( 'NONE',  ( 17.16957720519042851, -7.705202128115011817, -57.04933462012610335 ) ) ;
#33758 = PLANE ( 'NONE',  #48753 ) ;
#33759 = EDGE_CURVE ( 'NONE', #24768, #40719, #17504, .T. ) ;
#33760 = CARTESIAN_POINT ( 'NONE',  ( 13.73097534871769909, -8.145411141615490180, -37.41343723127859278 ) ) ;
#33761 = CARTESIAN_POINT ( 'NONE',  ( 68.13393739769708191, 17.98087126524488610, -74.20351669811759621 ) ) ;
#33762 = CARTESIAN_POINT ( 'NONE',  ( 54.42316715427640617, 19.80705547073500128, -75.56251559860999123 ) ) ;
#33763 = CARTESIAN_POINT ( 'NONE',  ( 47.49696547520699852, -54.38722354157379613, -75.00840848463889188 ) ) ;
#33764 = ORIENTED_EDGE ( 'NONE', *, *, #10308, .T. ) ;
#33765 = CARTESIAN_POINT ( 'NONE',  ( 55.88393979655880628, 14.62082033763359945, -17.33319607435739940 ) ) ;
#33766 = CARTESIAN_POINT ( 'NONE',  ( 22.90060573590868032, -14.60176553067577743, -78.79944796840196375 ) ) ;
#33767 = AXIS2_PLACEMENT_3D ( 'NONE', #37885, #2239, #37612 ) ;
#33768 = CARTESIAN_POINT ( 'NONE',  ( 56.87160283908409752, -50.28903218254829710, -52.71743054463500044 ) ) ;
#33769 = CIRCLE ( 'NONE', #49700, 18.00000000000000355 ) ;
#33770 = CARTESIAN_POINT ( 'NONE',  ( 10.94780721248440081, -10.83637588594240064, -36.08420929373698982 ) ) ;
#33771 = DIRECTION ( 'NONE',  ( 0.000000000000000000, 1.000000000000000000, 0.000000000000000000 ) ) ;
#33772 = ORIENTED_EDGE ( 'NONE', *, *, #18678, .T. ) ;
#33773 = CARTESIAN_POINT ( 'NONE',  ( 46.60371894209130517, 22.01667934560690298, -76.11277936203079264 ) ) ;
#33774 = DIRECTION ( 'NONE',  ( 0.000000000000000000, -1.000000000000000000, 0.000000000000000000 ) ) ;
#33775 = EDGE_CURVE ( 'NONE', #24020, #10985, #21207, .T. ) ;
#33776 = CARTESIAN_POINT ( 'NONE',  ( 75.29541660774471268, -36.36885601039063687, -12.50788449865524044 ) ) ;
#33777 = CARTESIAN_POINT ( 'NONE',  ( 8.222962354643469141, -14.58045876702774457, -56.83399816310966912 ) ) ;
#33778 = CARTESIAN_POINT ( 'NONE',  ( 29.07912664786299928, -4.512658877537830016, -34.92075920103120268 ) ) ;
#33779 = CARTESIAN_POINT ( 'NONE',  ( 82.02429831058030629, -41.23866635630079713, -45.87976092105969883 ) ) ;
#33780 = CIRCLE ( 'NONE', #31272, 0.5000000000000004441 ) ;
#33781 = CARTESIAN_POINT ( 'NONE',  ( 0.2392085819250069911, 19.81485081108809965, -34.59935833162420238 ) ) ;
#33783 = CARTESIAN_POINT ( 'NONE',  ( 43.47966092493172852, -39.00974599031439283, -73.04851394742181014 ) ) ;
#33782 = LINE ( 'NONE', #17306, #3169 ) ;
#33784 = DIRECTION ( 'NONE',  ( -0.2846079131720410937, -0.9586440088791334801, 0.000000000000000000 ) ) ;
#33785 = CARTESIAN_POINT ( 'NONE',  ( -33.45614285200539939, -10.80293933298100129, -56.47882598457800185 ) ) ;
#33786 = VERTEX_POINT ( 'NONE', #21666 ) ;
#33787 = CARTESIAN_POINT ( 'NONE',  ( 52.88990466204330687, -49.62977065132299970, -48.74279805905700158 ) ) ;
#33788 = B_SPLINE_CURVE_WITH_KNOTS ( 'NONE', 3,
 ( #20622, #27972, #24284, #40304, #4396, #36883, #7824, #11764, #19859, #28493, #44493, #8595, #3895, #14070, #10142, #26103, #41589, #49979, #33962, #32930, #13309, #42110 ),
 .UNSPECIFIED., .F., .F.,
 ( 4, 2, 2, 2, 2, 2, 2, 2, 2, 2, 4 ),
 ( 0.000000000000000000, 0.04949999999865291322, 0.1774999999951696883, 0.2574999999929937777, 0.3374999999908167014, 0.4374999999880958557, 0.4999999999863959932, 0.6249999999829938258, 0.7432269898313242917, 0.8817545104238473375, 1.000000000000000000 ),
 .UNSPECIFIED. ) ;
#33789 = EDGE_LOOP ( 'NONE', ( #40457, #9840, #47287, #13926 ) ) ;
#33790 = ADVANCED_FACE ( 'NONE', ( #13578 ), #730, .T. ) ;
#33791 = CARTESIAN_POINT ( 'NONE',  ( 41.27131287472999333, 8.477448802151759111, -79.73408454280998114 ) ) ;
#33792 = LINE ( 'NONE', #49801, #20157 ) ;
#33793 = CARTESIAN_POINT ( 'NONE',  ( 57.21713864038489561, 13.97813355815990022, -25.72061388221139921 ) ) ;
#33794 = CARTESIAN_POINT ( 'NONE',  ( 12.18644699963370037, -21.46083420798060004, -45.14190469443359888 ) ) ;
#33795 = CARTESIAN_POINT ( 'NONE',  ( 28.67375133668760157, -26.56866050586220140, -34.65024193067809222 ) ) ;
#33796 = CARTESIAN_POINT ( 'NONE',  ( 52.71274604433429545, 18.50164618420620144, -48.58382401692190200 ) ) ;
#33797 = CARTESIAN_POINT ( 'NONE',  ( 65.01129443250870565, 1.391252479931859964, -61.03617692120100457 ) ) ;
#33798 = CARTESIAN_POINT ( 'NONE',  ( 8.223401571539490362, -15.61634053766229968, -58.50766849176299900 ) ) ;
#33799 = CARTESIAN_POINT ( 'NONE',  ( 52.56521993351449851, 18.62941884369810097, -28.06240138782640159 ) ) ;
#33800 = ORIENTED_EDGE ( 'NONE', *, *, #9163, .F. ) ;
#33801 = CARTESIAN_POINT ( 'NONE',  ( 19.06740212538899826, -22.46465439540060061, -75.43852414181598931 ) ) ;
#33802 = CARTESIAN_POINT ( 'NONE',  ( 72.84798422376138660, 1.369544300367010026, -68.78354504031220529 ) ) ;
#33803 = CARTESIAN_POINT ( 'NONE',  ( 47.42839689129279890, -54.63796168553609789, -54.78693215226149960 ) ) ;
#33804 = PLANE ( 'NONE',  #41251 ) ;
#33805 = CARTESIAN_POINT ( 'NONE',  ( 72.81780655506248934, 1.383161449028140089, -62.62844710992279573 ) ) ;
#33806 = CARTESIAN_POINT ( 'NONE',  ( 11.53916947328389853, -65.37687372592600354, -17.79819407340969661 ) ) ;
#33807 = CARTESIAN_POINT ( 'NONE',  ( 71.50060750274239751, 1.264689361399219836, -60.86115090893359536 ) ) ;
#33808 = CARTESIAN_POINT ( 'NONE',  ( 18.18145487699519691, -23.32761325202299929, -76.20989520122053307 ) ) ;
#33809 = CARTESIAN_POINT ( 'NONE',  ( 71.25019707560579718, 0.8838110553206759423, -60.52272727272730179 ) ) ;
#33810 = CARTESIAN_POINT ( 'NONE',  ( 23.60352091122579665, -18.33564502225974024, -45.61878283607229179 ) ) ;
#33811 = CARTESIAN_POINT ( 'NONE',  ( 64.93084822843239579, 1.265664290790580182, -70.52755531239479581 ) ) ;
#33812 = ORIENTED_EDGE ( 'NONE', *, *, #5224, .F. ) ;
#33813 = CARTESIAN_POINT ( 'NONE',  ( 8.784728771152170879, -63.11543068638779630, -46.67204636145419983 ) ) ;
#33814 = DIRECTION ( 'NONE',  ( 0.3918900565005459247, 0.9200120562340468044, 0.000000000000000000 ) ) ;
#33815 = ORIENTED_EDGE ( 'NONE', *, *, #49, .T. ) ;
#33816 = CARTESIAN_POINT ( 'NONE',  ( 63.88393739769619373, 11.88381105532070059, -61.44999999999999574 ) ) ;
#33817 = CARTESIAN_POINT ( 'NONE',  ( 84.42051414645781904, 12.29857250479571107, -47.44928429649780810 ) ) ;
#33818 = CARTESIAN_POINT ( 'NONE',  ( 12.63580666350229897, -21.74037383255939915, -53.51237412773319591 ) ) ;
#33819 = ADVANCED_FACE ( 'NONE', ( #1263 ), #27909, .T. ) ;
#33820 = CARTESIAN_POINT ( 'NONE',  ( 51.42345381486639866, 19.32773741137469869, -76.23764488133839734 ) ) ;
#33821 = ORIENTED_EDGE ( 'NONE', *, *, #41194, .T. ) ;
#33822 = EDGE_CURVE ( 'NONE', #13283, #32835, #34868, .T. ) ;
#33823 = CARTESIAN_POINT ( 'NONE',  ( 39.83216070239956252, -15.95952177966980123, -34.79644660940672907 ) ) ;
#33824 = CARTESIAN_POINT ( 'NONE',  ( 11.63393739769619906, -41.61618894467930119, -35.14999999999999858 ) ) ;
#33825 = EDGE_CURVE ( 'NONE', #46428, #6450, #17864, .T. ) ;
#33826 = CARTESIAN_POINT ( 'NONE',  ( 12.72001770753569971, -8.110999246539140728, -57.15644495665979719 ) ) ;
#33827 = AXIS2_PLACEMENT_3D ( 'NONE', #35714, #28601, #44602 ) ;
#33828 = CARTESIAN_POINT ( 'NONE',  ( 0.1294298976606224894, -20.72822689018533637, -34.68804011290717426 ) ) ;
#33829 = CARTESIAN_POINT ( 'NONE',  ( 44.57690765188346660, -37.99148801630303751, -67.43510758073952616 ) ) ;
#33830 = ORIENTED_EDGE ( 'NONE', *, *, #13307, .F. ) ;
#33831 = CARTESIAN_POINT ( 'NONE',  ( 56.60227008640750057, -46.16578870400680046, -26.26017074143819841 ) ) ;
#33832 = CARTESIAN_POINT ( 'NONE',  ( 8.758027518364150055, -14.56611882458369855, -41.27767096285609938 ) ) ;
#33833 = CARTESIAN_POINT ( 'NONE',  ( 9.096695146297609114, -18.15749579477679987, -32.14999999999999858 ) ) ;
#33834 = CIRCLE ( 'NONE', #21262, 38.00000000000000000 ) ;
#33835 = CARTESIAN_POINT ( 'NONE',  ( 14.15113475208380045, 20.32108400380180058, -75.32473453343510528 ) ) ;
#33836 = EDGE_CURVE ( 'NONE', #1209, #3482, #48617, .T. ) ;
#33837 = DIRECTION ( 'NONE',  ( 0.000000000000000000, -0.7071067811865492381, -0.7071067811865457964 ) ) ;
#33838 = CARTESIAN_POINT ( 'NONE',  ( 42.34709230781079725, -45.29983228306050336, -6.529037730685770313 ) ) ;
#33839 = CARTESIAN_POINT ( 'NONE',  ( 18.10834526513780318, -7.932589976104685192, -61.08772463901920702 ) ) ;
#33840 = CARTESIAN_POINT ( 'NONE',  ( 9.166234375111990573, -11.20780655449969920, -50.68722986888699467 ) ) ;
#33841 = EDGE_LOOP ( 'NONE', ( #41146, #28133, #283, #4171 ) ) ;
#33842 = CARTESIAN_POINT ( 'NONE',  ( 55.74091017665890035, -46.16737070784190422, -25.61914745244379787 ) ) ;
#33843 = CARTESIAN_POINT ( 'NONE',  ( 15.72113303933780237, -51.10937407131510213, -21.50711442615979863 ) ) ;
#33845 = CARTESIAN_POINT ( 'NONE',  ( 41.79440130354939242, -39.74212845547013018, -77.32389498022952523 ) ) ;
#33844 = CARTESIAN_POINT ( 'NONE',  ( 7.548220943605030264, 28.49602621674689829, -11.72997927153680031 ) ) ;
#33846 = DIRECTION ( 'NONE',  ( 0.6888026391158372785, -0.7071067811865469066, 0.1598465650148877537 ) ) ;
#33847 = DIRECTION ( 'NONE',  ( 0.6676418852213051869, -0.2329255526947263677, -0.7071067811865459074 ) ) ;
#33848 = ORIENTED_EDGE ( 'NONE', *, *, #10313, .T. ) ;
#33849 = CARTESIAN_POINT ( 'NONE',  ( -5.667588108579429296, -46.74622128715009950, -4.590257091596729566 ) ) ;
#33850 = CARTESIAN_POINT ( 'NONE',  ( 47.49000820423450620, 23.36292359865809942, -54.73871130077979785 ) ) ;
#33851 = EDGE_CURVE ( 'NONE', #30043, #25181, #46775, .T. ) ;
#33852 = DIRECTION ( 'NONE',  ( 0.000000000000000000, 0.000000000000000000, -1.000000000000000000 ) ) ;
#33853 = CARTESIAN_POINT ( 'NONE',  ( 63.48611918674540533, 1.385702546077169917, -62.52592200326169092 ) ) ;
#33854 = CARTESIAN_POINT ( 'NONE',  ( 12.94102190407009978, 19.39887560817320278, -21.36191267119590265 ) ) ;
#33855 = DIRECTION ( 'NONE',  ( 0.8059588108975772602, 0.1342272854595020215, -0.5765530599821120372 ) ) ;
#33856 = CARTESIAN_POINT ( 'NONE',  ( 11.31612274021629894, 33.84606982840180223, -16.97569932836579909 ) ) ;
#33857 = DIRECTION ( 'NONE',  ( 0.6339889056055382222, 0.000000000000000000, -0.7733421413379021336 ) ) ;
#33858 = CARTESIAN_POINT ( 'NONE',  ( 38.67452568954060155, -15.61618894467929941, -81.65000000000000568 ) ) ;
#33859 = CARTESIAN_POINT ( 'NONE',  ( 19.50973947245583773, 24.24110967164852681, -75.58682750963716046 ) ) ;
#33860 = FACE_OUTER_BOUND ( 'NONE', #43503, .T. ) ;
#33861 = CARTESIAN_POINT ( 'NONE',  ( 8.223247527389670353, -15.61637340300369914, -74.79233150823711185 ) ) ;
#33862 = EDGE_CURVE ( 'NONE', #31554, #43574, #16773, .T. ) ;
#33863 = AXIS2_PLACEMENT_3D ( 'NONE', #20412, #43517, #35651 ) ;
#33864 = CARTESIAN_POINT ( 'NONE',  ( 51.65752907925219972, 21.59180590640119846, -54.64640228080419604 ) ) ;
#33865 = CARTESIAN_POINT ( 'NONE',  ( 63.25402410758490390, 0.9098571636355720083, -69.14090909090960224 ) ) ;
#33866 = PLANE ( 'NONE',  #31604 ) ;
#33867 = ORIENTED_EDGE ( 'NONE', *, *, #32389, .T. ) ;
#33868 = CARTESIAN_POINT ( 'NONE',  ( 16.13393739769620083, -15.61618894467929941, 10.84999999999999964 ) ) ;
#33869 = CARTESIAN_POINT ( 'NONE',  ( 11.10562983879290044, 32.14491805377860345, -44.25527573442839468 ) ) ;
#33870 = CARTESIAN_POINT ( 'NONE',  ( 72.63889986537131449, 1.416242794301129981, -62.22702189776489945 ) ) ;
#33871 = CARTESIAN_POINT ( 'NONE',  ( 65.13280827392949845, -32.17956496334240057, -17.73393099564480124 ) ) ;
#33872 = CARTESIAN_POINT ( 'NONE',  ( 12.51334738397835800, 24.21952903020473613, -75.31104072287740792 ) ) ;
#33873 = ORIENTED_EDGE ( 'NONE', *, *, #19580, .T. ) ;
#33874 = ORIENTED_EDGE ( 'NONE', *, *, #24191, .T. ) ;
#33875 = CARTESIAN_POINT ( 'NONE',  ( 17.16957703054396944, -23.52717578683977351, -79.96600284943940551 ) ) ;
#33876 = PRESENTATION_LAYER_ASSIGNMENT (  '', '', ( #7936 ) ) ;
#33877 = CARTESIAN_POINT ( 'NONE',  ( 76.55364060230128587, -0.04733056874654922169, -13.45856357439038575 ) ) ;
#33878 = ORIENTED_EDGE ( 'NONE', *, *, #20681, .T. ) ;
#33879 = CARTESIAN_POINT ( 'NONE',  ( 11.26949083597030032, -64.33764097384030833, -44.85617399231739455 ) ) ;
#33880 = CARTESIAN_POINT ( 'NONE',  ( 57.17215292315320596, -45.78104736118029905, -26.23432769010419818 ) ) ;
#33881 = CARTESIAN_POINT ( 'NONE',  ( 20.29256489975345445, -21.02754256757432927, -44.74450245125017744 ) ) ;
#33882 = CARTESIAN_POINT ( 'NONE',  ( 23.83903722046451179, -13.54551130856877350, -63.42433666729781550 ) ) ;
#33883 = ADVANCED_FACE ( 'NONE', ( #19760 ), #11917, .T. ) ;
#33884 = CARTESIAN_POINT ( 'NONE',  ( 64.02475525337911222, 1.458407608744489936, -61.60944193589799767 ) ) ;
#33885 = VERTEX_POINT ( 'NONE', #18265 ) ;
#33886 = CARTESIAN_POINT ( 'NONE',  ( 45.33172459800163523, 6.848706388641467413, -63.66100526906988222 ) ) ;
#33887 = EDGE_CURVE ( 'NONE', #42086, #47971, #31793, .T. ) ;
#33888 = ORIENTED_EDGE ( 'NONE', *, *, #23885, .F. ) ;
#33889 = CARTESIAN_POINT ( 'NONE',  ( 48.84046368175200570, -45.57708435644870093, -11.11574200907650045 ) ) ;
#33890 = CARTESIAN_POINT ( 'NONE',  ( 14.01384274612104264, -23.26046374906674785, -34.37835804628995362 ) ) ;
#33891 = CARTESIAN_POINT ( 'NONE',  ( 16.20840964857710276, 19.86086910830300312, -20.73468313311569844 ) ) ;
#33892 = CARTESIAN_POINT ( 'NONE',  ( 22.90015331880489668, -15.72754863961103844, -50.45805598341791409 ) ) ;
#33893 = VERTEX_POINT ( 'NONE', #26374 ) ;
#33894 = CARTESIAN_POINT ( 'NONE',  ( 24.04493739769619864, -15.61618894467929941, -32.14999999999999858 ) ) ;
#33895 = CARTESIAN_POINT ( 'NONE',  ( 47.10254288570079950, -54.62488891218850284, -75.00961804031550173 ) ) ;
#33896 = CARTESIAN_POINT ( 'NONE',  ( 56.60991603741530298, 12.53331740833790064, -8.242952450017121180 ) ) ;
#33897 = CARTESIAN_POINT ( 'NONE',  ( 47.13393739769619373, 7.029298498933709283, -54.64999999999999858 ) ) ;
#33898 = AXIS2_PLACEMENT_3D ( 'NONE', #17727, #22155, #26874 ) ;
#33899 = CARTESIAN_POINT ( 'NONE',  ( 14.13393739769639801, 10.38381105532069171, -35.01561944896768352 ) ) ;
#33900 = CARTESIAN_POINT ( 'NONE',  ( 51.61430880713380276, 19.94292765148920310, -76.09751503388891081 ) ) ;
#33901 = CARTESIAN_POINT ( 'NONE',  ( 57.86705690550169834, 14.17621725492490015, -26.12831864294430062 ) ) ;
#33902 = CARTESIAN_POINT ( 'NONE',  ( 11.76256125941080022, -22.13368991060269764, -75.97556276872140302 ) ) ;
#33903 = ORIENTED_EDGE ( 'NONE', *, *, #31199, .T. ) ;
#33904 = CARTESIAN_POINT ( 'NONE',  ( 18.06932202639930196, -55.56934008872529773, -76.14999999999999147 ) ) ;
#33905 = CARTESIAN_POINT ( 'NONE',  ( -10.96582629949129917, -41.77786732616849719, -5.028156413135709712 ) ) ;
#33906 = CARTESIAN_POINT ( 'NONE',  ( 15.52232235369950075, -50.77489110054699495, -15.65194195389930165 ) ) ;
#33907 = CARTESIAN_POINT ( 'NONE',  ( 72.88602187343720118, 1.308647200627810259, -68.98304916495260386 ) ) ;
#33908 = CARTESIAN_POINT ( 'NONE',  ( 20.11807775056638192, -22.52870672239707517, -36.12566301408477187 ) ) ;
#33909 = EDGE_CURVE ( 'NONE', #46283, #19834, #2795, .T. ) ;
#33910 = CARTESIAN_POINT ( 'NONE',  ( 24.04461175216078317, -15.61617380819018663, -65.50766589912049653 ) ) ;
#33911 = CARTESIAN_POINT ( 'NONE',  ( 8.222914298532977284, -14.58081029244737792, -58.83400626709403269 ) ) ;
#33912 = CARTESIAN_POINT ( 'NONE',  ( 19.75452607920933090, 24.21953045971935126, -75.31104306443889129 ) ) ;
#33913 = EDGE_CURVE ( 'NONE', #31172, #29730, #28736, .T. ) ;
#33914 = CARTESIAN_POINT ( 'NONE',  ( 76.44596060521568859, -43.25290919633437881, -14.01301206241809183 ) ) ;
#33915 = CARTESIAN_POINT ( 'NONE',  ( 17.99229861434620048, -51.11617952483079108, -74.35192203308130843 ) ) ;
#33916 = CARTESIAN_POINT ( 'NONE',  ( 57.33235504379430125, 13.88381105532070059, -16.73838572529449920 ) ) ;
#33917 = EDGE_CURVE ( 'NONE', #24512, #37059, #34612, .T. ) ;
#33918 = ORIENTED_EDGE ( 'NONE', *, *, #14312, .T. ) ;
#33919 = CARTESIAN_POINT ( 'NONE',  ( 19.55131170787279871, -22.23647950948729957, -53.41566130612969943 ) ) ;
#33920 = CARTESIAN_POINT ( 'NONE',  ( 63.57531447127419710, 1.379674774870449871, -62.12513747322240221 ) ) ;
#33921 = ORIENTED_EDGE ( 'NONE', *, *, #38169, .T. ) ;
#33922 = DIRECTION ( 'NONE',  ( -1.062456999999999985E-16, 7.719205000000000365E-17, 1.000000000000000000 ) ) ;
#33923 = DIRECTION ( 'NONE',  ( -0.1961161351381831008, 1.073215590470984393E-15, -0.9805806756909204447 ) ) ;
#33924 = DIRECTION ( 'NONE',  ( 0.000000000000000000, 1.000000000000000000, 0.000000000000000000 ) ) ;
#33925 = CARTESIAN_POINT ( 'NONE',  ( 21.88292891939993368, -21.05125959484767151, -61.74872814468829318 ) ) ;
#33927 = DIRECTION ( 'NONE',  ( 1.000000000000000000, -0.000000000000000000, 7.105427357601000281E-15 ) ) ;
#33926 = CARTESIAN_POINT ( 'NONE',  ( 43.11479320284178129, 8.644770638213781666, -70.94330782894907372 ) ) ;
#33928 = VECTOR ( 'NONE', #17741, 1000.000000000000114 ) ;
#33929 = CARTESIAN_POINT ( 'NONE',  ( 9.801945429253240860, -18.38258714374390124, -81.23899999999999011 ) ) ;
#33930 = CARTESIAN_POINT ( 'NONE',  ( 44.37469554261519988, -46.00068073351109632, -8.485651053198388638 ) ) ;
#33931 = VERTEX_POINT ( 'NONE', #49994 ) ;
#33932 = AXIS2_PLACEMENT_3D ( 'NONE', #15688, #24290, #35336 ) ;
#33933 = ORIENTED_EDGE ( 'NONE', *, *, #33591, .T. ) ;
#33934 = ORIENTED_EDGE ( 'NONE', *, *, #4259, .T. ) ;
#33935 = CARTESIAN_POINT ( 'NONE',  ( 61.16510488283689995, -45.29379779991980115, -46.73120355716090302 ) ) ;
#33936 = CARTESIAN_POINT ( 'NONE',  ( 51.96920254651271165, -50.49588334902367848, -49.26033372652806008 ) ) ;
#33937 = CARTESIAN_POINT ( 'NONE',  ( 54.94181551684279441, -51.40389681108650421, -53.69988726361309972 ) ) ;
#33938 = ORIENTED_EDGE ( 'NONE', *, *, #8321, .T. ) ;
#33939 = EDGE_CURVE ( 'NONE', #13019, #5352, #19278, .T. ) ;
#33940 = ORIENTED_EDGE ( 'NONE', *, *, #5435, .F. ) ;
#33941 = CARTESIAN_POINT ( 'NONE',  ( 22.90078878137445173, -15.66463057220322064, -72.45510385531270003 ) ) ;
#33942 = DIRECTION ( 'NONE',  ( -0.5877852522924661427, -0.8090169943749525583, 0.000000000000000000 ) ) ;
#33943 = CARTESIAN_POINT ( 'NONE',  ( 22.90093739818529528, -14.73038881013940404, -54.41115656462039141 ) ) ;
#33944 = VERTEX_POINT ( 'NONE', #12165 ) ;
#33945 = CARTESIAN_POINT ( 'NONE',  ( 24.04493739803490371, -15.61633039186437699, -49.50767153938471665 ) ) ;
#33946 = CARTESIAN_POINT ( 'NONE',  ( 53.61341843579059940, -50.67945576140650132, -76.60108205910400159 ) ) ;
#33947 = CARTESIAN_POINT ( 'NONE',  ( 60.26025110216900060, 14.55536647234960057, -47.43140372362420010 ) ) ;
#33948 = CARTESIAN_POINT ( 'NONE',  ( 23.92293678423830272, -14.65794255342009933, -77.97352993585168690 ) ) ;
#33949 = DIRECTION ( 'NONE',  ( 0.000000000000000000, 0.000000000000000000, -1.000000000000000000 ) ) ;
#33950 = CARTESIAN_POINT ( 'NONE',  ( 41.24357956626280242, 13.71928266329340040, -5.592244466849718876 ) ) ;
#33951 = CARTESIAN_POINT ( 'NONE',  ( 42.16710579205339826, -43.32203614284970428, -3.592545294820050472 ) ) ;
#33952 = CARTESIAN_POINT ( 'NONE',  ( 33.13393739769620083, 7.383811055320659733, -84.65000000000000568 ) ) ;
#33953 = DIRECTION ( 'NONE',  ( 0.000000000000000000, 0.000000000000000000, 1.000000000000000000 ) ) ;
#33954 = CARTESIAN_POINT ( 'NONE',  ( 64.39533937344960179, 1.328776533453549957, -70.16816298099379878 ) ) ;
#33955 = AXIS2_PLACEMENT_3D ( 'NONE', #26897, #15631, #31329 ) ;
#33956 = DIRECTION ( 'NONE',  ( 0.5516667872527449834, 0.8340645993220396903, 2.775557561562889194E-17 ) ) ;
#33957 = CARTESIAN_POINT ( 'NONE',  ( 57.24929578595760660, -50.61618894467929408, -75.24227954305044364 ) ) ;
#33958 = ORIENTED_EDGE ( 'NONE', *, *, #2313, .F. ) ;
#33959 = VECTOR ( 'NONE', #11717, 1000.000000000000000 ) ;
#33960 = CARTESIAN_POINT ( 'NONE',  ( 15.05440318628160057, -53.11618894467930119, -76.14999999999999147 ) ) ;
#33961 = CARTESIAN_POINT ( 'NONE',  ( 57.24929575387970004, 19.38381105532069881, -53.91492787281829635 ) ) ;
#33962 = CARTESIAN_POINT ( 'NONE',  ( 9.063308985759819691, 32.62929763576821074, -46.73460937115434888 ) ) ;
#33963 = DIRECTION ( 'NONE',  ( 0.000000000000000000, 1.000000000000000000, 0.000000000000000000 ) ) ;
#33964 = DIRECTION ( 'NONE',  ( 0.6415444970810866288, 0.4854844151940982400, 0.5939070136550167467 ) ) ;
#33965 = CARTESIAN_POINT ( 'NONE',  ( 63.14953303862429124, 0.9272522097098119254, -68.99005086130968323 ) ) ;
#33966 = CARTESIAN_POINT ( 'NONE',  ( 47.92547496200619861, -54.35536316263760170, -54.78476778173359918 ) ) ;
#33967 = CARTESIAN_POINT ( 'NONE',  ( 22.90103018812914115, -15.61618888866172483, -50.84718209631233066 ) ) ;
#33968 = EDGE_CURVE ( 'NONE', #21257, #41771, #113, .T. ) ;
#33969 = STYLED_ITEM ( 'NONE', ( #7507 ), #10093 ) ;
#33970 = CARTESIAN_POINT ( 'NONE',  ( 56.45988843467819862, 19.49067611367820163, -53.39311502846720003 ) ) ;
#33971 = CARTESIAN_POINT ( 'NONE',  ( 9.807724164810522893, -20.47780537512590371, -46.58403036311962353 ) ) ;
#33972 = CARTESIAN_POINT ( 'NONE',  ( 48.03391530370259943, 23.06771420177449983, -54.78057301038420235 ) ) ;
#33973 = ORIENTED_EDGE ( 'NONE', *, *, #3672, .T. ) ;
#33974 = CARTESIAN_POINT ( 'NONE',  ( 22.81273049926999974, -13.34985227930480001, -74.74304765278330365 ) ) ;
#33975 = VERTEX_POINT ( 'NONE', #4807 ) ;
#33976 = VECTOR ( 'NONE', #17763, 1000.000000000000000 ) ;
#33977 = CARTESIAN_POINT ( 'NONE',  ( 82.75389222264627165, 14.36253673539014919, -47.67224619643947392 ) ) ;
#33978 = CARTESIAN_POINT ( 'NONE',  ( 29.46622902366960162, 1.883811055320659955, -54.64999999999999858 ) ) ;
#33979 = CARTESIAN_POINT ( 'NONE',  ( 46.99731062513885149, 8.001896800055366299, -34.80647497723111883 ) ) ;
#33981 = CARTESIAN_POINT ( 'NONE',  ( 63.63393739769619373, -53.11618894467930119, 16.35000000000000142 ) ) ;
#33980 = CARTESIAN_POINT ( 'NONE',  ( 83.63395638909621255, 13.75389496877540019, -47.37153147893519645 ) ) ;
#33982 = CARTESIAN_POINT ( 'NONE',  ( 14.06462975631870016, -22.35863098146390016, -79.04760718966259958 ) ) ;
#33983 = CARTESIAN_POINT ( 'NONE',  ( 19.33046814882964881, -49.25056949571164466, -34.64999999999999858 ) ) ;
#33984 = CARTESIAN_POINT ( 'NONE',  ( 56.87513795754310308, -45.11618894467940066, -15.74603272341079929 ) ) ;
#33985 = LINE ( 'NONE', #38458, #48723 ) ;
#33986 = ORIENTED_EDGE ( 'NONE', *, *, #21041, .T. ) ;
#33987 = CARTESIAN_POINT ( 'NONE',  ( 68.13393739769618662, -0.1661889446793515246, -90.65000000000000568 ) ) ;
#33988 = CIRCLE ( 'NONE', #11429, 39.00000000000000711 ) ;
#33989 = ORIENTED_EDGE ( 'NONE', *, *, #3923, .T. ) ;
#33990 = ORIENTED_EDGE ( 'NONE', *, *, #37546, .F. ) ;
#33991 = CARTESIAN_POINT ( 'NONE',  ( 12.07459604304269973, -64.83039640760800637, -16.11467485433340130 ) ) ;
#33992 = CARTESIAN_POINT ( 'NONE',  ( 54.47259832750690123, 15.01994964729280113, -15.76422791930239953 ) ) ;
#33993 = DIRECTION ( 'NONE',  ( -1.000000000000000000, 0.000000000000000000, 0.000000000000000000 ) ) ;
#33994 = CARTESIAN_POINT ( 'NONE',  ( 10.23245083239389963, -64.79111536624868961, -47.03631047207230154 ) ) ;
#33995 = AXIS2_PLACEMENT_3D ( 'NONE', #24293, #4657, #18461 ) ;
#33996 = VERTEX_POINT ( 'NONE', #36505 ) ;
#33997 = EDGE_LOOP ( 'NONE', ( #41512, #35283, #8967, #14952, #48662, #46789, #15248 ) ) ;
#33998 = EDGE_CURVE ( 'NONE', #11865, #9063, #32055, .T. ) ;
#33999 = CARTESIAN_POINT ( 'NONE',  ( -19.00919503052239889, -32.92138004297220277, -51.31717196595420205 ) ) ;
#34000 = AXIS2_PLACEMENT_3D ( 'NONE', #40260, #44188, #32105 ) ;
#34001 = CARTESIAN_POINT ( 'NONE',  ( -12.25993951570199947, -34.31880250072530458, -34.64999999999999858 ) ) ;
#34002 = CARTESIAN_POINT ( 'NONE',  ( 53.48928929932589682, -49.41396641409689749, -49.16886795839930357 ) ) ;
#34003 = CARTESIAN_POINT ( 'NONE',  ( 49.97469255755120088, 21.36656799640790183, -52.61615532409420126 ) ) ;
#34004 = EDGE_CURVE ( 'NONE', #41906, #12868, #27981, .T. ) ;
#34005 = DIRECTION ( 'NONE',  ( 0.000000000000000000, 0.000000000000000000, -1.000000000000000000 ) ) ;
#34006 = CARTESIAN_POINT ( 'NONE',  ( 51.12541109982870324, -49.03592882882020376, -76.44562399636079419 ) ) ;
#34007 = CARTESIAN_POINT ( 'NONE',  ( 56.54805895952080164, -50.43678705299419818, -52.80479669090900785 ) ) ;
#34008 = ORIENTED_EDGE ( 'NONE', *, *, #26416, .F. ) ;
#34009 = LINE ( 'NONE', #34533, #12432 ) ;
#34010 = CARTESIAN_POINT ( 'NONE',  ( 68.13393739769630031, 16.88381105532149817, -68.79999999999999716 ) ) ;
#34011 = ORIENTED_EDGE ( 'NONE', *, *, #5199, .T. ) ;
#34012 = CARTESIAN_POINT ( 'NONE',  ( 24.04493320937934442, -15.61618918076996110, -53.79232900421944663 ) ) ;
#34013 = DIRECTION ( 'NONE',  ( 0.000000000000000000, 0.000000000000000000, -1.000000000000000000 ) ) ;
#34014 = CARTESIAN_POINT ( 'NONE',  ( 19.00161232051599924, -8.311177779142791877, -39.63156730105999515 ) ) ;
#34015 = CARTESIAN_POINT ( 'NONE',  ( 13.11803215473759998, -50.90931609213659925, -21.59044441884969956 ) ) ;
#34016 = CARTESIAN_POINT ( 'NONE',  ( 56.83869077455450025, 19.41466794163520149, -74.56788156747980167 ) ) ;
#34017 = CARTESIAN_POINT ( 'NONE',  ( 47.39162735359639811, -54.25023534817900384, -75.29717685666371096 ) ) ;
#34018 = ORIENTED_EDGE ( 'NONE', *, *, #37281, .T. ) ;
#34019 = CARTESIAN_POINT ( 'NONE',  ( 55.89836899175390528, 14.67647375536889953, -17.62829706286229836 ) ) ;
#34020 = CARTESIAN_POINT ( 'NONE',  ( 19.54194862422452417, -9.703289362798095397, -78.11948479122949607 ) ) ;
#34021 = CARTESIAN_POINT ( 'NONE',  ( 22.39003682439990328, -12.40129601987878338, -46.69594346447604494 ) ) ;
#34022 = AXIS2_PLACEMENT_3D ( 'NONE', #4025, #44111, #12398 ) ;
#34023 = CARTESIAN_POINT ( 'NONE',  ( 16.89732681591289776, -22.62759363779219868, -41.31265874393579907 ) ) ;
#34024 = FACE_OUTER_BOUND ( 'NONE', #28381, .T. ) ;
#34025 = ORIENTED_EDGE ( 'NONE', *, *, #35472, .T. ) ;
#34026 = B_SPLINE_CURVE_WITH_KNOTS ( 'NONE', 3,
 ( #40525, #28979, #4102, #28713, #40015, #20079, #40272, #36319, #36847, #31866, #41043, #8040, #48391, #28195, #684, #430, #952, #48926 ),
 .UNSPECIFIED., .F., .F.,
 ( 4, 2, 2, 2, 2, 2, 2, 2, 4 ),
 ( 0.4999988359836951002, 0.5624989814857331849, 0.6249991269877712696, 0.6874992724898094654, 0.7499994179918475501, 0.8124995634938856348, 0.8749997089959238306, 0.9374998544979619153, 1.000000000000000000 ),
 .UNSPECIFIED. ) ;
#34027 = CARTESIAN_POINT ( 'NONE',  ( 47.53482544724619885, 23.16677569099900325, -74.95177798121650881 ) ) ;
#34028 = CARTESIAN_POINT ( 'NONE',  ( 65.02205492013339949, 0.9960089569207349891, -60.52992920782880049 ) ) ;
#34029 = CARTESIAN_POINT ( 'NONE',  ( 75.16169728866853461, -29.51520510724298063, -11.85453094363455406 ) ) ;
#34030 = CARTESIAN_POINT ( 'NONE',  ( 68.13393739769625768, -15.41618894467990764, -28.20067248431510976 ) ) ;
#34031 = CARTESIAN_POINT ( 'NONE',  ( 60.14258131274579000, -45.11618894467940066, -25.78020576970689959 ) ) ;
#34032 = AXIS2_PLACEMENT_3D ( 'NONE', #9471, #27623, #32755 ) ;
#34033 = FACE_OUTER_BOUND ( 'NONE', #28452, .T. ) ;
#34034 = CARTESIAN_POINT ( 'NONE',  ( -9.375152675533279023, 14.02725416202859954, -42.91803494044829392 ) ) ;
#34036 = CARTESIAN_POINT ( 'NONE',  ( 46.48809362348643504, -39.29542413733557993, -58.13476177693350877 ) ) ;
#34035 = CARTESIAN_POINT ( 'NONE',  ( 84.19224659786166853, -44.53040250705239345, -48.96577344625911365 ) ) ;
#34037 = EDGE_CURVE ( 'NONE', #6190, #11854, #10469, .T. ) ;
#34038 = CARTESIAN_POINT ( 'NONE',  ( 9.448786886202281465, -11.23620880982031700, -70.69263903080977229 ) ) ;
#34039 = CARTESIAN_POINT ( 'NONE',  ( -32.29328640865499978, -10.93117069805279939, -55.80050612416169997 ) ) ;
#34040 = ORIENTED_EDGE ( 'NONE', *, *, #13028, .T. ) ;
#34041 = CARTESIAN_POINT ( 'NONE',  ( 52.71234499349689884, -49.73836072086629656, -48.66396021830070140 ) ) ;
#34042 = ORIENTED_EDGE ( 'NONE', *, *, #2728, .T. ) ;
#34043 = CARTESIAN_POINT ( 'NONE',  ( 17.27855009702555122, 21.70055148386360244, -76.14999999999999147 ) ) ;
#34044 = LINE ( 'NONE', #26185, #23505 ) ;
#34045 = CARTESIAN_POINT ( 'NONE',  ( 57.64963559888369815, 13.88883635462039834, -25.41607447946719844 ) ) ;
#34046 = CARTESIAN_POINT ( 'NONE',  ( 11.70317949953529890, -10.12884503851570095, -49.73660269612349794 ) ) ;
#34047 = CARTESIAN_POINT ( 'NONE',  ( 50.75795695721529910, 19.32138164550209680, -76.14999999999999147 ) ) ;
#34048 = CARTESIAN_POINT ( 'NONE',  ( 53.26968212669260083, 18.27860782879199775, -49.16957734417170656 ) ) ;
#34049 = CARTESIAN_POINT ( 'NONE',  ( 64.80710063092610085, 1.263823323415670163, -60.83883010097409993 ) ) ;
#34050 = CIRCLE ( 'NONE', #14813, 3.000000000000004885 ) ;
#34051 = CARTESIAN_POINT ( 'NONE',  ( 23.06214062797170072, -27.61618894467930119, -32.14999999999999858 ) ) ;
#34052 = AXIS2_PLACEMENT_3D ( 'NONE', #32395, #29005, #36604 ) ;
#34053 = ORIENTED_EDGE ( 'NONE', *, *, #18756, .F. ) ;
#34054 = CARTESIAN_POINT ( 'NONE',  ( 19.27822296750359854, -8.861918991986240002, -76.70602703883389495 ) ) ;
#34055 = CARTESIAN_POINT ( 'NONE',  ( 54.37486050126969417, 17.76197798406979800, -48.98148910212459839 ) ) ;
#34056 = FACE_OUTER_BOUND ( 'NONE', #3348, .T. ) ;
#34057 = CARTESIAN_POINT ( 'NONE',  ( 72.80287646850248962, 1.383922910988889976, -62.58539998085741018 ) ) ;
#34058 =( BOUNDED_CURVE ( )  B_SPLINE_CURVE ( 3, ( #29659, #1380, #9767, #1638 ),
 .UNSPECIFIED., .F., .T. ) 
 B_SPLINE_CURVE_WITH_KNOTS ( ( 4, 4 ),
 ( 1.755576258187430128, 3.141592653589798445 ),
 .UNSPECIFIED. ) 
 CURVE ( )  GEOMETRIC_REPRESENTATION_ITEM ( )  RATIONAL_B_SPLINE_CURVE ( ( 1.000000000000000000, 0.8462184657327374016, 0.8462184657327374016, 1.000000000000000000 ) ) 
 REPRESENTATION_ITEM ( '' )  );
#34059 = CARTESIAN_POINT ( 'NONE',  ( 10.75976506911110064, -64.96659187203999863, -18.06526995554730064 ) ) ;
#34060 = CARTESIAN_POINT ( 'NONE',  ( 52.84731125486479897, 18.41934504040209930, -48.60966020774090168 ) ) ;
#34061 = CARTESIAN_POINT ( 'NONE',  ( 20.44176770790133801, -21.20055615980069774, -67.13803027069128859 ) ) ;
#34062 = CARTESIAN_POINT ( 'NONE',  ( 12.03301697448477015, -10.16097117192421528, -61.74741793951960034 ) ) ;
#34063 = FACE_OUTER_BOUND ( 'NONE', #28044, .T. ) ;
#34064 = CARTESIAN_POINT ( 'NONE',  ( 64.72741779930989026, 0.8986939045430288875, -70.58925035374339529 ) ) ;
#34065 = ORIENTED_EDGE ( 'NONE', *, *, #31950, .F. ) ;
#34066 = CARTESIAN_POINT ( 'NONE',  ( 9.288932741751329658, -63.21985741985628948, -46.53007890215199893 ) ) ;
#34067 = DIRECTION ( 'NONE',  ( 0.3294064756440890918, -0.9441882088883233326, 0.000000000000000000 ) ) ;
#34068 = ORIENTED_EDGE ( 'NONE', *, *, #37487, .T. ) ;
#34069 = EDGE_CURVE ( 'NONE', #10547, #35448, #19541, .T. ) ;
#34070 = CARTESIAN_POINT ( 'NONE',  ( 68.13393739769618662, -5.818188944679350882, -65.65000000000000568 ) ) ;
#34071 = CARTESIAN_POINT ( 'NONE',  ( 57.05931827775219745, 19.36066449068759709, -53.44572518222490487 ) ) ;
#34072 = CARTESIAN_POINT ( 'NONE',  ( 8.222953841603198200, -16.65185680590451156, -70.46600195478848150 ) ) ;
#34073 = CARTESIAN_POINT ( 'NONE',  ( 53.89956157026149697, 19.40017492853139913, -76.79736723946669485 ) ) ;
#34074 = ORIENTED_EDGE ( 'NONE', *, *, #1960, .F. ) ;
#34075 = CARTESIAN_POINT ( 'NONE',  ( 11.09843494245553330, -65.15652262322491595, -47.26083285147826984 ) ) ;
#34076 = PRODUCT ( 'Height Adjustment Lead Screw', 'Height Adjustment Lead Screw', '', ( #24078 ) ) ;
#34077 = CARTESIAN_POINT ( 'NONE',  ( 58.88690644461912882, 17.44024477555941743, -51.02974587662403394 ) ) ;
#34078 = CARTESIAN_POINT ( 'NONE',  ( 33.20393739732724470, -15.61618894436410088, -14.68999999982327864 ) ) ;
#34079 = AXIS2_PLACEMENT_3D ( 'NONE', #27174, #42665, #22718 ) ;
#34080 = CARTESIAN_POINT ( 'NONE',  ( 24.04476371970871540, -15.55956675530847200, -43.79004723472182548 ) ) ;
#34081 = CARTESIAN_POINT ( 'NONE',  ( 24.32370634531909914, -16.57034021176809802, -53.82924985198769718 ) ) ;
#34082 = CARTESIAN_POINT ( 'NONE',  ( 15.09850012911266681, -23.52720226237179801, -48.04933579400842092 ) ) ;
#34083 = CARTESIAN_POINT ( 'NONE',  ( 43.85723124748935930, -37.89848476597786231, -71.03349786720269776 ) ) ;
#34084 = VERTEX_POINT ( 'NONE', #32816 ) ;
#34085 = CARTESIAN_POINT ( 'NONE',  ( 56.78239028773929675, -46.02921025412519640, -26.24769687010520158 ) ) ;
#34086 = CARTESIAN_POINT ( 'NONE',  ( 10.88607800575399942, -20.90454082475969955, -46.98143399943669607 ) ) ;
#34087 = CARTESIAN_POINT ( 'NONE',  ( 9.231882466319580871, -13.75394085457820026, -32.14999999999999858 ) ) ;
#34088 = CARTESIAN_POINT ( 'NONE',  ( 13.64650866220840086, 20.52576179366219833, -75.06145659859170394 ) ) ;
#34089 = CARTESIAN_POINT ( 'NONE',  ( 64.64302830678670375, 0.9098571636355720083, -70.52991329011129551 ) ) ;
#34090 = CARTESIAN_POINT ( 'NONE',  ( 41.21726802631610553, -44.82489126183570249, -5.423354306796420055 ) ) ;
#34091 = CARTESIAN_POINT ( 'NONE',  ( -18.86606260230390220, 19.38381105532060289, 11.34999999999999964 ) ) ;
#34092 = CARTESIAN_POINT ( 'NONE',  ( 9.384920991318070449, -20.35259034821490332, -64.31288601182949094 ) ) ;
#34093 = ORIENTED_EDGE ( 'NONE', *, *, #39733, .F. ) ;
#34094 = CARTESIAN_POINT ( 'NONE',  ( 54.00053677488939741, -48.28078295432670330, -26.32878014593650207 ) ) ;
#34095 = CARTESIAN_POINT ( 'NONE',  ( 54.28170228800039609, -50.73610625031639643, -76.21973480364219711 ) ) ;
#34097 = CARTESIAN_POINT ( 'NONE',  ( 46.70917532059600319, -39.13647700890110315, -34.65437117444129456 ) ) ;
#34096 = CARTESIAN_POINT ( 'NONE',  ( 7.952424752720789414, 30.74922443327189825, -15.01216219166649957 ) ) ;
#34098 = EDGE_CURVE ( 'NONE', #51131, #41037, #12861, .T. ) ;
#34099 = B_SPLINE_CURVE_WITH_KNOTS ( 'NONE', 3,
 ( #41776, #31184, #5878, #43278, #22101, #29961, #26033, #3441, #42041, #7368, #21847, #37852, #1948, #19412, #17927, #34151, #51390, #45458 ),
 .UNSPECIFIED., .F., .F.,
 ( 4, 2, 2, 2, 2, 2, 2, 2, 4 ),
 ( 0.000000000000000000, 0.09835926191934898921, 0.6036208803096320130, 0.9194093918035598501, 1.116777211487260058, 1.276316813128300032, 1.595396016410379980, 2.105922741661700126, 2.552633626256600063 ),
 .UNSPECIFIED. ) ;
#34100 = LINE ( 'NONE', #14208, #7120 ) ;
#34101 = CARTESIAN_POINT ( 'NONE',  ( 16.13393739769620083, -15.61618894467929941, -32.14999999999999858 ) ) ;
#34102 = ORIENTED_EDGE ( 'NONE', *, *, #6646, .F. ) ;
#34103 = CARTESIAN_POINT ( 'NONE',  ( -7.464592885573059888, -45.40146952839990035, -4.956245330965249885 ) ) ;
#34104 = ADVANCED_FACE ( 'NONE', ( #48582 ), #8745, .F. ) ;
#34105 = CARTESIAN_POINT ( 'NONE',  ( 47.44105247587240370, 23.39273938256710039, -54.71914698481260331 ) ) ;
#34106 = AXIS2_PLACEMENT_3D ( 'NONE', #30663, #9989, #42750 ) ;
#34107 = CARTESIAN_POINT ( 'NONE',  ( 13.33295398203071080, -8.192918865366621617, -65.17746492593889229 ) ) ;
#34108 = CARTESIAN_POINT ( 'NONE',  ( 84.25370905176697534, -44.18318147193002687, -47.43624044261927963 ) ) ;
#34109 = CARTESIAN_POINT ( 'NONE',  ( 12.08205748224539988, 34.04687831868819359, -16.92411159752879968 ) ) ;
#34110 = EDGE_CURVE ( 'NONE', #13022, #51110, #16176, .T. ) ;
#34111 = CARTESIAN_POINT ( 'NONE',  ( 51.62357988847060142, 17.46062716628840050, -76.93789418233430411 ) ) ;
#34112 = DIRECTION ( 'NONE',  ( -1.000000000000000000, 0.000000000000000000, 0.000000000000000000 ) ) ;
#34113 = LINE ( 'NONE', #26513, #37599 ) ;
#34114 = DIRECTION ( 'NONE',  ( 1.000000000000000000, 0.000000000000000000, 0.000000000000000000 ) ) ;
#34115 = CARTESIAN_POINT ( 'NONE',  ( 55.42636091632299866, 15.84296872918980092, -26.34129395571439858 ) ) ;
#34116 = VECTOR ( 'NONE', #20775, 1000.000000000000000 ) ;
#34117 = CARTESIAN_POINT ( 'NONE',  ( 54.40370209750609831, 20.40074845781530044, -53.77986364435489719 ) ) ;
#34118 = CARTESIAN_POINT ( 'NONE',  ( 63.49748922100520332, 1.316033847539019863, -69.19960462970651349 ) ) ;
#34119 = CARTESIAN_POINT ( 'NONE',  ( 53.51287195967390176, 18.19965013284789990, -49.22146522496750265 ) ) ;
#34120 = CARTESIAN_POINT ( 'NONE',  ( 10.10517893431099878, 23.92687708958460036, -21.14999999999999858 ) ) ;
#34121 = DIRECTION ( 'NONE',  ( 1.000000000000000000, 2.460964292799963328E-14, 0.000000000000000000 ) ) ;
#34122 = CARTESIAN_POINT ( 'NONE',  ( 10.97956612247109831, 32.13351753698560032, -44.74505020633399965 ) ) ;
#34123 = DIRECTION ( 'NONE',  ( 0.07088902009066748444, 0.000000000000000000, 0.9974842088126432138 ) ) ;
#34124 = ADVANCED_FACE ( 'NONE', ( #42011 ), #7181, .T. ) ;
#34125 = CARTESIAN_POINT ( 'NONE',  ( 65.88922314972060690, -31.40957022853389802, -17.14610387725419827 ) ) ;
#34126 = CARTESIAN_POINT ( 'NONE',  ( 8.222872596472118545, -15.61638977992110000, -80.50766849176289952 ) ) ;
#34127 = EDGE_LOOP ( 'NONE', ( #45893, #19105, #15874, #9931 ) ) ;
#34128 = EDGE_LOOP ( 'NONE', ( #19633, #14296, #29552, #19061, #38226, #49212 ) ) ;
#34129 = LINE ( 'NONE', #2184, #32850 ) ;
#34130 = FACE_OUTER_BOUND ( 'NONE', #5407, .T. ) ;
#34131 = ORIENTED_EDGE ( 'NONE', *, *, #12996, .F. ) ;
#34132 = EDGE_CURVE ( 'NONE', #1287, #4643, #2530, .T. ) ;
#34133 = CARTESIAN_POINT ( 'NONE',  ( 12.94913857733849838, -65.51469239313858850, -47.64817528796799451 ) ) ;
#34135 = B_SPLINE_CURVE_WITH_KNOTS ( 'NONE', 3,
 ( #35326, #40038, #47402, #3114, #19600, #11755, #47650, #15161, #46891, #51832 ),
 .UNSPECIFIED., .F., .F.,
 ( 4, 2, 2, 2, 4 ),
 ( -0.0004107207313030360294, 0.000000000000000000, 0.01419180571504649949, 0.04450164637014340785, 0.05031563485850510525 ),
 .UNSPECIFIED. ) ;
#34134 = CARTESIAN_POINT ( 'NONE',  ( 56.65742313423940146, -46.03143560913069621, -26.22917644616859789 ) ) ;
#34136 = CARTESIAN_POINT ( 'NONE',  ( 24.04154727951358339, -15.88190596389101117, -77.51834605307320203 ) ) ;
#34137 = CARTESIAN_POINT ( 'NONE',  ( 2.422196078461449797, -25.82482932757800143, -35.02873218748179340 ) ) ;
#34138 = ORIENTED_EDGE ( 'NONE', *, *, #25572, .T. ) ;
#34139 = DIRECTION ( 'NONE',  ( 0.000000000000000000, 0.000000000000000000, -1.000000000000000000 ) ) ;
#34140 = CARTESIAN_POINT ( 'NONE',  ( 45.26400037985666813, 6.841219675276395407, -63.99964612493251792 ) ) ;
#34141 = ORIENTED_EDGE ( 'NONE', *, *, #13335, .T. ) ;
#34142 = CARTESIAN_POINT ( 'NONE',  ( 48.98108981356519820, -45.96115812557660973, -11.58776272563040166 ) ) ;
#34143 = CARTESIAN_POINT ( 'NONE',  ( 24.03431982466308270, -16.03474806585207446, -33.80917298512384406 ) ) ;
#34144 = CARTESIAN_POINT ( 'NONE',  ( 14.79734571144840061, 19.88381641708039993, -22.20703854454670179 ) ) ;
#34145 = DIRECTION ( 'NONE',  ( 0.000000000000000000, -1.000000000000000000, 0.000000000000000000 ) ) ;
#34146 = CARTESIAN_POINT ( 'NONE',  ( 62.13393739769620083, -42.11618894467930119, -65.65000000000000568 ) ) ;
#34147 = CYLINDRICAL_SURFACE ( 'NONE', #50104, 39.00000000000000711 ) ;
#34148 = CARTESIAN_POINT ( 'NONE',  ( 46.35275103504449845, -52.90993241930539881, -76.14999999999999147 ) ) ;
#34149 = CARTESIAN_POINT ( 'NONE',  ( 57.73378796211289909, 13.88381105527449932, -10.52255156732080010 ) ) ;
#34150 = EDGE_CURVE ( 'NONE', #1146, #24768, #36715, .T. ) ;
#34151 = CARTESIAN_POINT ( 'NONE',  ( 50.04022705227350087, -48.91488703454379561, -76.14999999999999147 ) ) ;
#34152 = FACE_OUTER_BOUND ( 'NONE', #13334, .T. ) ;
#34153 = CARTESIAN_POINT ( 'NONE',  ( 51.19516202202900246, 19.86383965925769957, -76.13919812682919996 ) ) ;
#34154 = CARTESIAN_POINT ( 'NONE',  ( 61.66480336386660355, 13.88597247968120030, -28.02007549380890339 ) ) ;
#34155 = CARTESIAN_POINT ( 'NONE',  ( 23.72175950820210133, -18.84228198835780077, -35.63563296679920001 ) ) ;
#34156 = ORIENTED_EDGE ( 'NONE', *, *, #48433, .T. ) ;
#34157 = CARTESIAN_POINT ( 'NONE',  ( 19.21265657477752598, -49.46974233527256359, -34.79644660940672907 ) ) ;
#34158 = CARTESIAN_POINT ( 'NONE',  ( -3.057385712928159638, -49.07295275241269650, -5.614604985102389811 ) ) ;
#34159 = DIRECTION ( 'NONE',  ( 1.000000000000000000, 0.000000000000000000, 0.000000000000000000 ) ) ;
#34160 = CARTESIAN_POINT ( 'NONE',  ( 72.92870999253369746, 1.229734285826180162, -69.07389306497110226 ) ) ;
#34161 = CARTESIAN_POINT ( 'NONE',  ( 16.13393739769620083, -15.61618894467929941, -28.45282021618999835 ) ) ;
#34162 = ADVANCED_FACE ( 'NONE', ( #11687 ), #23444, .T. ) ;
#34163 = B_SPLINE_CURVE_WITH_KNOTS ( 'NONE', 3,
 ( #51440, #3745, #15785, #11872, #43321, #7415, #34920, #10832, #14758, #23114 ),
 .UNSPECIFIED., .F., .F.,
 ( 4, 2, 2, 2, 4 ),
 ( -0.1857717838147150136, -0.1853436703551470111, -0.1652145016229930041, -0.1459149143040530117, -0.1350635247378738635 ),
 .UNSPECIFIED. ) ;
#34164 = CARTESIAN_POINT ( 'NONE',  ( 3.768317948728554079, -22.75548266223732341, -34.65000000000000568 ) ) ;
#34165 = CYLINDRICAL_SURFACE ( 'NONE', #49476, 0.4999999999999980571 ) ;
#34166 = CARTESIAN_POINT ( 'NONE',  ( 42.80229243930720173, 11.48401673206149987, -3.540423289874710111 ) ) ;
#34167 = ADVANCED_FACE ( 'NONE', ( #31570 ), #27651, .T. ) ;
#34168 = CARTESIAN_POINT ( 'NONE',  ( 20.29256161582522822, -21.02754519288219370, -78.74448466050279194 ) ) ;
#34169 = CARTESIAN_POINT ( 'NONE',  ( 60.34379259250669492, 14.63564649040839960, -47.72732609510669732 ) ) ;
#34170 = CARTESIAN_POINT ( 'NONE',  ( 17.16939758333402466, -23.52720141142701848, -56.25068354753920374 ) ) ;
#34171 = CARTESIAN_POINT ( 'NONE',  ( 76.04613871463565999, -43.31687852089314816, -13.66319593086862305 ) ) ;
#34172 = DIRECTION ( 'NONE',  ( 0.000000000000000000, -1.000000000000000000, 0.000000000000000000 ) ) ;
#34173 = ORIENTED_EDGE ( 'NONE', *, *, #15430, .T. ) ;
#34174 = CARTESIAN_POINT ( 'NONE',  ( 13.25818560489270048, -22.48908833027550358, -57.69348358356519668 ) ) ;
#34175 = CARTESIAN_POINT ( 'NONE',  ( 63.90196154687351537, 1.277721627657099956, -61.48328519722549856 ) ) ;
#34176 = ORIENTED_EDGE ( 'NONE', *, *, #18275, .T. ) ;
#34177 = CARTESIAN_POINT ( 'NONE',  ( 10.64863409883700029, 32.21085600226960111, -23.66469670114080159 ) ) ;
#34178 = DIRECTION ( 'NONE',  ( 0.000000000000000000, 0.000000000000000000, -1.000000000000000000 ) ) ;
#34179 = DIRECTION ( 'NONE',  ( 0.000000000000000000, 0.000000000000000000, 1.000000000000000000 ) ) ;
#34180 = AXIS2_PLACEMENT_3D ( 'NONE', #51703, #15794, #11109 ) ;
#34181 = CARTESIAN_POINT ( 'NONE',  ( 8.222921604359401115, -16.65161820214613186, -62.46599063383079198 ) ) ;
#34182 = CARTESIAN_POINT ( 'NONE',  ( 46.03612365166910791, 8.863419595963454967, -56.78333922229177944 ) ) ;
#34183 = CIRCLE ( 'NONE', #39219, 0.4999999999999990008 ) ;
#34184 = CARTESIAN_POINT ( 'NONE',  ( 10.07160187669169993, -18.84535597674730312, -81.23899999999999011 ) ) ;
#34185 = DIRECTION ( 'NONE',  ( 0.000000000000000000, -1.000000000000000000, 0.000000000000000000 ) ) ;
#34186 = ORIENTED_EDGE ( 'NONE', *, *, #23512, .T. ) ;
#34187 = ORIENTED_EDGE ( 'NONE', *, *, #131, .T. ) ;
#34188 = AXIS2_PLACEMENT_3D ( 'NONE', #25995, #22062, #14474 ) ;
#34189 = ORIENTED_EDGE ( 'NONE', *, *, #46584, .T. ) ;
#34190 = CARTESIAN_POINT ( 'NONE',  ( 61.43875230760810524, -45.16919861524459634, -46.56425532763250175 ) ) ;
#34191 = CARTESIAN_POINT ( 'NONE',  ( 28.36591740443274290, -6.729135268073950904, -6.721843382729280059 ) ) ;
#34192 = EDGE_LOOP ( 'NONE', ( #25720, #17438, #45409, #9555, #12956 ) ) ;
#34193 = ORIENTED_EDGE ( 'NONE', *, *, #6010, .F. ) ;
#34194 = DIRECTION ( 'NONE',  ( 0.9999999999999997780, 2.292180684128748550E-25, 1.129617809262089834E-08 ) ) ;
#34195 = CARTESIAN_POINT ( 'NONE',  ( 14.36271553927783096, -22.20706879767622866, -53.03615247297079094 ) ) ;
#34196 = CARTESIAN_POINT ( 'NONE',  ( 22.04684627355322135, -12.20819253758295275, -54.28615617134685323 ) ) ;
#34197 = EDGE_LOOP ( 'NONE', ( #19570, #20324, #10958, #11760, #7335 ) ) ;
#34198 = CARTESIAN_POINT ( 'NONE',  ( 16.15069188244332210, 19.81939201856824795, -15.66900176635303232 ) ) ;
#34199 = CARTESIAN_POINT ( 'NONE',  ( 52.01032223484130412, -50.03877910798939865, -76.70782219912229039 ) ) ;
#34200 = CARTESIAN_POINT ( 'NONE',  ( 60.96305650301830070, 14.21870589704430010, -47.29791441411810382 ) ) ;
#34201 = EDGE_CURVE ( 'NONE', #12115, #36299, #32995, .T. ) ;
#34202 = CARTESIAN_POINT ( 'NONE',  ( 8.290410016103750834, -15.35962354207850034, -77.02290276308829675 ) ) ;
#34203 = EDGE_CURVE ( 'NONE', #12629, #21587, #11179, .T. ) ;
#34204 = DIRECTION ( 'NONE',  ( -0.7071067811865457964, 0.7071067811865492381, 0.000000000000000000 ) ) ;
#34205 = CARTESIAN_POINT ( 'NONE',  ( 41.72083574932489825, 13.70929892781999904, -5.743067283000420353 ) ) ;
#34206 = CARTESIAN_POINT ( 'NONE',  ( 42.84544925522080661, -42.99895311139940191, -4.190148907760479879 ) ) ;
#34207 = EDGE_CURVE ( 'NONE', #37478, #1545, #37959, .T. ) ;
#34208 = FACE_OUTER_BOUND ( 'NONE', #22913, .T. ) ;
#34209 = DIRECTION ( 'NONE',  ( 1.000000000000000000, 0.000000000000000000, 0.000000000000000000 ) ) ;
#34210 = AXIS2_PLACEMENT_3D ( 'NONE', #390, #32847, #41259 ) ;
#34211 = CARTESIAN_POINT ( 'NONE',  ( 64.86412778899749298, 1.402436395646509792, -70.21307676274530252 ) ) ;
#34212 = DIRECTION ( 'NONE',  ( 0.000000000000000000, 1.000000000000000000, 0.000000000000000000 ) ) ;
#34213 = AXIS2_PLACEMENT_3D ( 'NONE', #19393, #8120, #35374 ) ;
#34214 = CARTESIAN_POINT ( 'NONE',  ( 62.03393739769618520, -15.41618894467939782, -65.65000000000000568 ) ) ;
#34215 = ORIENTED_EDGE ( 'NONE', *, *, #27382, .F. ) ;
#34216 = FILL_AREA_STYLE ('',( #22167 ) ) ;
#34218 = CIRCLE ( 'NONE', #23329, 6.100000000000001421 ) ;
#34217 = CARTESIAN_POINT ( 'NONE',  ( 57.29802881897539635, 19.33020836189830050, -53.44853715813179917 ) ) ;
#34219 = CARTESIAN_POINT ( 'NONE',  ( 44.71501321890448821, -40.01020284909822777, -63.19468146700351951 ) ) ;
#34220 = CARTESIAN_POINT ( 'NONE',  ( 0.5716597377992500562, -15.61618894406255365, -7.050000000025706370 ) ) ;
#34221 = CARTESIAN_POINT ( 'NONE',  ( 46.95605112289660354, -54.29280230291429632, -75.52284329973289800 ) ) ;
#34222 = EDGE_CURVE ( 'NONE', #27054, #29219, #22898, .T. ) ;
#34223 = CARTESIAN_POINT ( 'NONE',  ( 63.11571638736320011, 0.9242073871622918935, -68.93904330669420233 ) ) ;
#34224 = CARTESIAN_POINT ( 'NONE',  ( 48.22078997057410277, -54.22619954268040487, -54.83130601189450459 ) ) ;
#34225 = CARTESIAN_POINT ( 'NONE',  ( 16.05499536011143746, -8.563790251354252092, -50.34361688520657196 ) ) ;
#34226 = CARTESIAN_POINT ( 'NONE',  ( 56.50147281689449841, 19.49859888707450040, -53.50280580149869536 ) ) ;
#34227 = CARTESIAN_POINT ( 'NONE',  ( 47.94837612362730539, 23.09355010960259946, -54.72220175608870107 ) ) ;
#34228 = EDGE_LOOP ( 'NONE', ( #2672, #43511, #46226, #40215 ) ) ;
#34229 = CARTESIAN_POINT ( 'NONE',  ( 23.18576810717789982, -15.49684566140489927, -72.84179330725640966 ) ) ;
#34230 = ORIENTED_EDGE ( 'NONE', *, *, #31076, .F. ) ;
#34231 = FACE_OUTER_BOUND ( 'NONE', #11487, .T. ) ;
#34232 = LINE ( 'NONE', #33978, #5139 ) ;
#34233 = CARTESIAN_POINT ( 'NONE',  ( 20.11812595995350250, -8.703699988156179401, -41.17433431193339288 ) ) ;
#34235 = CARTESIAN_POINT ( 'NONE',  ( 55.95580150607140268, 14.65510410099619953, -25.57470036468859931 ) ) ;
#34234 = CARTESIAN_POINT ( 'NONE',  ( 83.54413676250729281, 13.61283532876010050, -47.09683803678880309 ) ) ;
#34236 = CARTESIAN_POINT ( 'NONE',  ( 12.49208382618429880, -9.576365995269719988, -77.78010429264477921 ) ) ;
#34237 = CARTESIAN_POINT ( 'NONE',  ( 9.026390854478798076, 16.60930999848670098, -54.64999999999999858 ) ) ;
#34238 = CARTESIAN_POINT ( 'NONE',  ( 0.4371248283887909647, -22.38658506580789975, -35.02873218748179340 ) ) ;
#34239 = CARTESIAN_POINT ( 'NONE',  ( 56.55522355860080097, -46.21195502513410247, -26.26695352263039851 ) ) ;
#34240 = ORIENTED_EDGE ( 'NONE', *, *, #45715, .F. ) ;
#34241 = CARTESIAN_POINT ( 'NONE',  ( 29.13393739769619728, -33.11618894467940066, -53.85091742636659973 ) ) ;
#34242 = ORIENTED_EDGE ( 'NONE', *, *, #48882, .T. ) ;
#34243 = ORIENTED_EDGE ( 'NONE', *, *, #13315, .T. ) ;
#34244 = CARTESIAN_POINT ( 'NONE',  ( 12.27153357073309969, -64.61912752036219842, -15.84005975574299896 ) ) ;
#34245 = AXIS2_PLACEMENT_3D ( 'NONE', #23969, #32350, #44175 ) ;
#34246 = DIRECTION ( 'NONE',  ( 0.000000000000000000, 0.000000000000000000, -1.000000000000000000 ) ) ;
#34247 = CARTESIAN_POINT ( 'NONE',  ( -33.14629235451220524, -5.854914153751970218, -57.60079496986291048 ) ) ;
#34248 = PLANE ( 'NONE',  #50227 ) ;
#34249 = AXIS2_PLACEMENT_3D ( 'NONE', #31251, #23133, #50937 ) ;
#34250 = ORIENTED_EDGE ( 'NONE', *, *, #14293, .T. ) ;
#34251 = AXIS2_PLACEMENT_3D ( 'NONE', #13146, #25153, #21222 ) ;
#34252 = VECTOR ( 'NONE', #11390, 1000.000000000000000 ) ;
#34253 = ORIENTED_EDGE ( 'NONE', *, *, #22299, .F. ) ;
#34254 = CARTESIAN_POINT ( 'NONE',  ( 0.9246403334604839097, -51.52825870078270043, -34.45773271021280237 ) ) ;
#34255 = CARTESIAN_POINT ( 'NONE',  ( 82.24885320877977790, -45.11618894467940066, -46.39516212021803909 ) ) ;
#34256 = CIRCLE ( 'NONE', #25050, 1.399999999999998579 ) ;
#34257 = CARTESIAN_POINT ( 'NONE',  ( 9.366940099211698012, -15.19984693586703628, -45.47240728461869708 ) ) ;
#34258 = FACE_OUTER_BOUND ( 'NONE', #33503, .T. ) ;
#34259 = CARTESIAN_POINT ( 'NONE',  ( 51.38511839723819463, -50.11055703386340099, -76.33916260165409540 ) ) ;
#34260 = CARTESIAN_POINT ( 'NONE',  ( 57.45637359078290274, -50.19905859961199468, -52.69494871447199813 ) ) ;
#34261 = EDGE_LOOP ( 'NONE', ( #32748, #32310 ) ) ;
#34262 = CARTESIAN_POINT ( 'NONE',  ( 19.63536038757005997, -8.499666568143982914, -33.43793342242106092 ) ) ;
#34263 = CARTESIAN_POINT ( 'NONE',  ( 65.43393739769584272, 16.88381105532339532, -68.79999999999942872 ) ) ;
#34264 = VERTEX_POINT ( 'NONE', #35525 ) ;
#34265 = CARTESIAN_POINT ( 'NONE',  ( 22.90108808520262329, -15.61618901356150069, -52.45282226904397049 ) ) ;
#34266 = CARTESIAN_POINT ( 'NONE',  ( 53.97718803714800373, -49.20306630607990428, -49.10491108831829621 ) ) ;
#34267 = CARTESIAN_POINT ( 'NONE',  ( 17.80009649341840117, -23.28499989940520010, -46.44439537253119710 ) ) ;
#34268 = ADVANCED_FACE ( 'NONE', ( #51517 ), #20293, .T. ) ;
#34269 = CARTESIAN_POINT ( 'NONE',  ( 13.08122484219250126, -50.91564157304479465, -21.57315878215120009 ) ) ;
#34270 = CARTESIAN_POINT ( 'NONE',  ( 55.69862941132319634, 19.50294859112689849, -75.44272654099910369 ) ) ;
#34271 = CARTESIAN_POINT ( 'NONE',  ( 47.61398272666360043, -54.53961310099680304, -74.36298856109941369 ) ) ;
#34272 = ADVANCED_FACE ( 'NONE', ( #35783 ), #51767, .T. ) ;
#34273 = CARTESIAN_POINT ( 'NONE',  ( 56.92544927513679909, 13.88381105532070059, -16.01979077684439901 ) ) ;
#34274 = CARTESIAN_POINT ( 'NONE',  ( 68.13393739771647972, -29.16618894506861892, -49.15000000085210274 ) ) ;
#34275 = CARTESIAN_POINT ( 'NONE',  ( 53.63393739769619373, -53.11618894467930119, 11.84999999999999964 ) ) ;
#34276 = CARTESIAN_POINT ( 'NONE',  ( 9.931764968075150080, -18.97410739629480148, -43.68922667584449471 ) ) ;
#34277 = CARTESIAN_POINT ( 'NONE',  ( 17.63393739769620083, -32.15793020853440254, -34.64999999999999858 ) ) ;
#34278 = ORIENTED_EDGE ( 'NONE', *, *, #7158, .F. ) ;
#34279 = B_SPLINE_CURVE_WITH_KNOTS ( 'NONE', 3,
 ( #38683, #18741, #50978, #14300, #42345, #30269, #11155, #19001, #6447, #30782, #46810, #22918 ),
 .UNSPECIFIED., .F., .F.,
 ( 4, 2, 2, 2, 2, 4 ),
 ( 0.000000000000000000, 0.1249999999999997780, 0.2499999999999995559, 0.4999999999999996669, 0.7499999999999997780, 1.000000000000000000 ),
 .UNSPECIFIED. ) ;
#34280 = CARTESIAN_POINT ( 'NONE',  ( 47.36202810124689933, 22.97939671731930034, -75.36156497780129371 ) ) ;
#34281 = AXIS2_PLACEMENT_3D ( 'NONE', #49980, #49727, #6215 ) ;
#34282 = CARTESIAN_POINT ( 'NONE',  ( 20.03604369380067851, -55.13509060654741489, -18.97520576177407037 ) ) ;
#34283 = B_SPLINE_CURVE_WITH_KNOTS ( 'NONE', 3,
 ( #31083, #11200, #24760, #49176, #21356, #32361, #25542, #48646, #33149, #33413, #45230, #44703, #37103, #9338, #37359, #41289, #940, #48914 ),
 .UNSPECIFIED., .F., .F.,
 ( 4, 2, 2, 2, 2, 2, 2, 2, 4 ),
 ( -2.552633636494849867, -2.105922750108249808, -1.595396022809280279, -1.276316818247430041, -1.116777215966499925, -0.9194146059286070205, -0.6036344298679827691, -0.09838614817098489951, 2.220446049250313081E-15 ),
 .UNSPECIFIED. ) ;
#34284 = AXIS2_PLACEMENT_3D ( 'NONE', #50215, #38414, #9609 ) ;
#34285 = CARTESIAN_POINT ( 'NONE',  ( 75.14303606280716963, -28.31058215067825756, -11.76413862553087952 ) ) ;
#34286 = CARTESIAN_POINT ( 'NONE',  ( 12.88498222292095008, -65.50776629007216911, -23.37250852991978078 ) ) ;
#34287 = CIRCLE ( 'NONE', #10035, 1.999999999999997113 ) ;
#34288 = CYLINDRICAL_SURFACE ( 'NONE', #8082, 2.000000000000001776 ) ;
#34289 = CIRCLE ( 'NONE', #11732, 21.50000000000000000 ) ;
#34290 = AXIS2_PLACEMENT_3D ( 'NONE', #15143, #11479, #3610 ) ;
#34291 = FACE_OUTER_BOUND ( 'NONE', #2705, .T. ) ;
#34292 = EDGE_CURVE ( 'NONE', #6345, #40975, #27903, .T. ) ;
#34293 = B_SPLINE_CURVE_WITH_KNOTS ( 'NONE', 3,
 ( #42426, #23496, #6516, #22990, #15153, #51056, #3362, #47139, #38485, #2585, #6781, #42941, #7039, #43450, #11227, #7552, #19336, #34265 ),
 .UNSPECIFIED., .F., .F.,
 ( 4, 2, 2, 2, 2, 2, 2, 2, 4 ),
 ( 0.000000000000000000, 0.06249983851711840566, 0.1249996770342368113, 0.1874995155513552170, 0.2499993540684736226, 0.3124991925855918895, 0.3749990311027102119, 0.4374988696198284788, 0.4999987081369468012 ),
 .UNSPECIFIED. ) ;
#34294 = CARTESIAN_POINT ( 'NONE',  ( 82.13853704237929776, 13.94246732026510038, -46.86219204859769860 ) ) ;
#34295 = CARTESIAN_POINT ( 'NONE',  ( 0.02643090884201690013, 19.86906729127069937, -34.96342131435890366 ) ) ;
#34297 = CARTESIAN_POINT ( 'NONE',  ( 42.78911202776321687, -38.92818100861666863, -76.46643483648848871 ) ) ;
#34296 = FACE_OUTER_BOUND ( 'NONE', #7304, .T. ) ;
#34298 = AXIS2_PLACEMENT_3D ( 'NONE', #5542, #9475, #25422 ) ;
#34299 = ADVANCED_FACE ( 'NONE', ( #36805 ), #24566, .T. ) ;
#34300 = CARTESIAN_POINT ( 'NONE',  ( 14.84079903770737019, -7.738696850407225547, -70.95619825573045603 ) ) ;
#34301 = B_SPLINE_CURVE_WITH_KNOTS ( 'NONE', 3,
 ( #43992, #44244, #40318, #36369, #4414, #40572, #477, #17756, #40833, #49232, #1001, #25597 ),
 .UNSPECIFIED., .F., .F.,
 ( 4, 2, 2, 2, 2, 4 ),
 ( -1.480557223830589963, -1.376569949160200146, -1.265367455784349948, -1.042962469032639783, -0.6871144902299088919, -0.6744302025021630120 ),
 .UNSPECIFIED. ) ;
#34302 = CARTESIAN_POINT ( 'NONE',  ( -31.82194261889170050, -6.201200042654750000, -55.69495912570319973 ) ) ;
#34303 = ORIENTED_EDGE ( 'NONE', *, *, #47000, .F. ) ;
#34304 = CARTESIAN_POINT ( 'NONE',  ( 53.19708396731179789, -49.47972728580509738, -48.94481821072159278 ) ) ;
#34305 = EDGE_LOOP ( 'NONE', ( #26558, #34391, #10505, #12742 ) ) ;
#34306 = CARTESIAN_POINT ( 'NONE',  ( 46.39380079123251477, 9.013081426918761352, -54.52813979131429534 ) ) ;
#34307 = CARTESIAN_POINT ( 'NONE',  ( 14.36278510963897048, -9.025291076946244218, -41.86948664301885970 ) ) ;
#34308 = CARTESIAN_POINT ( 'NONE',  ( 13.99922743840360084, 19.91584326097130031, -22.43849254327080089 ) ) ;
#34309 = CARTESIAN_POINT ( 'NONE',  ( 55.93328256272239685, 14.78258593416649980, -25.74340590685439878 ) ) ;
#34310 = CARTESIAN_POINT ( 'NONE',  ( 9.524139214987918933, -18.07649922602429982, -41.33939600337990328 ) ) ;
#34311 = DIRECTION ( 'NONE',  ( -0.6047562208151086027, -0.7964106436916998932, 0.000000000000000000 ) ) ;
#34312 = CARTESIAN_POINT ( 'NONE',  ( 52.67785519474879408, 18.53209731767190149, -48.65292259172070288 ) ) ;
#34313 = CARTESIAN_POINT ( 'NONE',  ( 56.06628350373850367, -45.70557515080610500, -17.61155996636929899 ) ) ;
#34314 = DIRECTION ( 'NONE',  ( -0.9151634328772870752, -0.3898247278253974546, -0.1025308378007029897 ) ) ;
#34315 = ORIENTED_EDGE ( 'NONE', *, *, #16036, .T. ) ;
#34316 = CARTESIAN_POINT ( 'NONE',  ( 19.63503279775940058, -21.96029221563379963, -81.40635028194188294 ) ) ;
#34317 = CARTESIAN_POINT ( 'NONE',  ( 11.88236604821880071, -65.43512709907859914, -17.91369388827580167 ) ) ;
#34318 = CARTESIAN_POINT ( 'NONE',  ( 10.05382147007509985, 33.36697451426490346, -46.89254338722109594 ) ) ;
#34319 = CARTESIAN_POINT ( 'NONE',  ( 73.12814476249489815, 0.9958340104639701318, -62.33798249239750078 ) ) ;
#34320 = CARTESIAN_POINT ( 'NONE',  ( 10.62398834541929915, -64.83239605773999870, -18.14938726570430205 ) ) ;
#34321 = DIRECTION ( 'NONE',  ( 0.000000000000000000, -1.000000000000000000, 0.000000000000000000 ) ) ;
#34322 = DIRECTION ( 'NONE',  ( 0.000000000000000000, 0.000000000000000000, -1.000000000000000000 ) ) ;
#34323 = CARTESIAN_POINT ( 'NONE',  ( 14.06327912329211571, -7.911083529862108499, -45.20896163178147020 ) ) ;
#34324 = CARTESIAN_POINT ( 'NONE',  ( 22.04686277055845167, -12.20822342221341827, -58.28615331364241570 ) ) ;
#34325 = CARTESIAN_POINT ( 'NONE',  ( 64.79014552703429786, 0.9971903505820729485, -70.62320069164850622 ) ) ;
#34326 = ORIENTED_EDGE ( 'NONE', *, *, #10474, .T. ) ;
#34327 = CARTESIAN_POINT ( 'NONE',  ( 10.14754812987370158, -63.31247221493028832, -45.99341560559020081 ) ) ;
#34328 = CARTESIAN_POINT ( 'NONE',  ( 22.51821868797902582, -17.99963233150277020, -32.56637983983515028 ) ) ;
#34329 = ORIENTED_EDGE ( 'NONE', *, *, #37197, .F. ) ;
#34330 = DIRECTION ( 'NONE',  ( 0.000000000000000000, 0.000000000000000000, -1.000000000000000000 ) ) ;
#34331 = CARTESIAN_POINT ( 'NONE',  ( 57.24929579703050564, 19.38381106717350022, -53.91492794795360055 ) ) ;
#34332 = CARTESIAN_POINT ( 'NONE',  ( 53.96532849294369782, 19.38571653099999992, -76.95223800223610056 ) ) ;
#34333 = AXIS2_PLACEMENT_3D ( 'NONE', #32393, #12782, #32919 ) ;
#34334 = ORIENTED_EDGE ( 'NONE', *, *, #28370, .F. ) ;
#34335 = CARTESIAN_POINT ( 'NONE',  ( 18.13393739769620083, -41.61618894467930119, -54.64999999999999858 ) ) ;
#34336 = PLANE ( 'NONE',  #51853 ) ;
#34337 = AXIS2_PLACEMENT_3D ( 'NONE', #31043, #629, #19519 ) ;
#34338 = CARTESIAN_POINT ( 'NONE',  ( 0.1457841021255935343, -26.78123956999450428, -34.68167779225149161 ) ) ;
#34339 = CARTESIAN_POINT ( 'NONE',  ( 8.222915508880662472, -14.58080133695443870, -42.83400543223867629 ) ) ;
#34340 = VECTOR ( 'NONE', #34139, 1000.000000000000000 ) ;
#34341 = CIRCLE ( 'NONE', #36855, 5.999999999999998224 ) ;
#34342 = B_SPLINE_SURFACE_WITH_KNOTS ( 'NONE', 3, 3, ( 
 ( #32566, #40461, #32057, #32830, #625, #48856, #7738, #3804, #35763, #51746, #8237, #15844, #31805, #4298, #48078, #39956, #28135, #44141 ),
 ( #24188, #20270, #1929, #5355, #49383, #37311, #33880, #49893, #38092, #42026, #37052, #17659, #49127, #34134, #29175, #25235, #21567, #25749 ),
 ( #50143, #17398, #1411, #13479, #9799, #10053, #5095, #29436, #41757, #24965, #5863, #21049, #17145, #45442, #33096, #45177, #21829, #13988 ),
 ( #37835, #29689, #13226, #49642, #17911, #29945, #9289, #9021, #45959, #26015, #13733, #9544, #45699, #2188, #41242, #6126, #21309, #33366 ),
 ( #22082, #18168, #33625, #28914, #44919, #40983, #1148, #25496, #41498, #5612, #37562, #1671, #26534, #19455, #43320, #14242, #46488, #10317 ),
 ( #26278, #47259, #46749, #15011, #7414, #10578, #43063, #14756, #51182, #22855, #42548, #6638, #14496, #39132, #18938, #22602, #15277, #27059 ),
 ( #47008, #35179, #3223, #22343, #30726, #34919, #7162, #26797, #38617, #27314, #50917, #6903, #38876, #2439, #31233, #19194, #2707, #34655 ),
 ( #2964, #42285, #18682, #11093, #3486, #23359, #39384, #30981, #10831, #38349, #11349, #30212, #46228, #50409, #18422, #23113, #50662, #35441 ),
 ( #6382, #34397, #30468, #42809, #16550, #28332, #27826, #28075, #4498, #4245, #47766, #20731, #32502, #8184, #313, #48529, #31486, #24125 ) ),
 .UNSPECIFIED., .F., .F., .F.,
 ( 4, 1, 1, 1, 1, 1, 4 ),
 ( 4, 2, 2, 2, 2, 2, 2, 2, 4 ),
 ( 0.000000000000000000, 0.1666666666666670182, 0.3333333333333329818, 0.5000000000000000000, 0.6666666666666670737, 0.8333333333333330373, 1.000000000000000000 ),
 ( -0.9973706374895159321, -0.9474515228500450803, -0.8167403652454939822, -0.7016502394537249554, -0.5865601136619560396, -0.4426974564222450059, -0.2988347991825339722, -0.01347842800242600100, 0.07936656096996599907 ),
 .UNSPECIFIED. ) ;
#34343 = CARTESIAN_POINT ( 'NONE',  ( 23.10957479117670132, -11.22037240953919834, -67.61334385705760042 ) ) ;
#34344 = EDGE_CURVE ( 'NONE', #10625, #1162, #320, .T. ) ;
#34345 = DIRECTION ( 'NONE',  ( 0.000000000000000000, 0.000000000000000000, 1.000000000000000000 ) ) ;
#34346 = CARTESIAN_POINT ( 'NONE',  ( 44.45943562239641977, -37.97683504137048516, -68.02249989722677981 ) ) ;
#34347 = VERTEX_POINT ( 'NONE', #28674 ) ;
#34348 = CARTESIAN_POINT ( 'NONE',  ( 56.94970255497029399, -45.93464052491829364, -26.24572100487180037 ) ) ;
#34349 = CARTESIAN_POINT ( 'NONE',  ( 23.24368907943700080, -17.84287366172600287, -56.32926786494380167 ) ) ;
#34350 = CARTESIAN_POINT ( 'NONE',  ( 53.35896811852089883, -49.47778564188549666, -49.18807904032110656 ) ) ;
#34351 = CARTESIAN_POINT ( 'NONE',  ( 8.860320911730040550, -16.94687217539350144, -32.14999999999999858 ) ) ;
#34352 = DIRECTION ( 'NONE',  ( -0.1175431456444907818, -0.8277005620457529300, -0.5487215947100521074 ) ) ;
#34353 = CARTESIAN_POINT ( 'NONE',  ( 23.04647597310426832, -11.63208624730823182, -51.62566268846900641 ) ) ;
#34354 = CARTESIAN_POINT ( 'NONE',  ( 41.62258892463700022, -45.17860157138659360, -6.029592982722220107 ) ) ;
#34355 = CARTESIAN_POINT ( 'NONE',  ( 29.13393739769620083, -15.61618894467929941, -5.690000000000000391 ) ) ;
#34356 = CARTESIAN_POINT ( 'NONE',  ( 24.16486509800989779, -17.48351885160749930, -65.58038890884739658 ) ) ;
#34357 = ORIENTED_EDGE ( 'NONE', *, *, #12349, .T. ) ;
#34358 = CARTESIAN_POINT ( 'NONE',  ( 54.77076828691379973, -47.35498126536249686, -25.79499481954439943 ) ) ;
#34359 = CARTESIAN_POINT ( 'NONE',  ( 55.92110024521279854, -50.72146136133119398, -75.31187564150310720 ) ) ;
#34361 = CARTESIAN_POINT ( 'NONE',  ( 41.20166900923489095, -39.67422119637704725, -80.18288832365365693 ) ) ;
#34360 = CARTESIAN_POINT ( 'NONE',  ( 7.395348223008199717, 28.56816484056830063, -11.82605492805729952 ) ) ;
#34363 = EDGE_CURVE ( 'NONE', #677, #37056, #41263, .T. ) ;
#34362 = CARTESIAN_POINT ( 'NONE',  ( 63.33805919087440373, 1.375383258925270136, -68.56484433753419694 ) ) ;
#34364 = DIRECTION ( 'NONE',  ( 0.000000000000000000, -1.000000000000000000, 0.000000000000000000 ) ) ;
#34365 = CARTESIAN_POINT ( 'NONE',  ( 13.00893739769619906, 34.28605925116850273, -47.75434321273180416 ) ) ;
#34366 = EDGE_LOOP ( 'NONE', ( #33311, #10641, #31843, #34715, #47371 ) ) ;
#34367 =( BOUNDED_CURVE ( )  B_SPLINE_CURVE ( 3, ( #34589, #30653, #7345, #43504 ),
 .UNSPECIFIED., .F., .T. ) 
 B_SPLINE_CURVE_WITH_KNOTS ( ( 4, 4 ),
 ( 4.712388980384689674, 4.724464978221631917 ),
 .UNSPECIFIED. ) 
 CURVE ( )  GEOMETRIC_REPRESENTATION_ITEM ( )  RATIONAL_B_SPLINE_CURVE ( ( 1.000000000000000000, 0.9999878475599406347, 0.9999878475599406347, 1.000000000000000000 ) ) 
 REPRESENTATION_ITEM ( '' )  );
#34368 = CARTESIAN_POINT ( 'NONE',  ( -5.159222269507229619, -47.09623647360059806, -4.453993761141310515 ) ) ;
#34369 = CIRCLE ( 'NONE', #11810, 5.500000000000000000 ) ;
#34370 = CARTESIAN_POINT ( 'NONE',  ( 47.46960547804090425, 23.38441036786990068, -54.88167812123789702 ) ) ;
#34371 = CARTESIAN_POINT ( 'NONE',  ( 9.741321230546846621, -10.90463958868946648, -64.99459759734693876 ) ) ;
#34372 = LINE ( 'NONE', #46204, #43595 ) ;
#34373 = CARTESIAN_POINT ( 'NONE',  ( 20.63393739769599833, 10.38381105532070059, -35.14999999999999858 ) ) ;
#34374 = AXIS2_PLACEMENT_3D ( 'NONE', #4427, #36383, #44782 ) ;
#34375 = CARTESIAN_POINT ( 'NONE',  ( 12.09990282912600001, 34.01294332033750578, -16.83009741454110042 ) ) ;
#34376 = CARTESIAN_POINT ( 'NONE',  ( 22.90120720387987774, -15.61618909956830770, -56.84718059981966576 ) ) ;
#34377 = CARTESIAN_POINT ( 'NONE',  ( 52.99768777340029402, 18.34103694310250177, -48.81581853631149670 ) ) ;
#34378 = CARTESIAN_POINT ( 'NONE',  ( 19.42743748307076501, 24.24785769981644634, -75.66007724762421560 ) ) ;
#34379 = CARTESIAN_POINT ( 'NONE',  ( 17.98749448546718455, 1.245406012443906807, -34.79644291222912500 ) ) ;
#34380 = CARTESIAN_POINT ( 'NONE',  ( 52.72392628394530334, 18.48930238429770156, -28.00962051878589776 ) ) ;
#34381 = CARTESIAN_POINT ( 'NONE',  ( 49.40539548389270408, 22.26547577746099904, -54.15746054661040176 ) ) ;
#34382 = CARTESIAN_POINT ( 'NONE',  ( 63.60417424459109981, 1.405463742252590187, -69.09493810159840166 ) ) ;
#34383 = CARTESIAN_POINT ( 'NONE',  ( 52.69474333003019950, 18.53535902989789719, -48.79529474154600166 ) ) ;
#34384 = CARTESIAN_POINT ( 'NONE',  ( 46.42984739191849997, -45.11618894467940066, -7.676443726158701075 ) ) ;
#34385 = CARTESIAN_POINT ( 'NONE',  ( 22.90113830400267148, -16.70047761723187918, -72.89819816215725723 ) ) ;
#34386 = CARTESIAN_POINT ( 'NONE',  ( 10.97797437399790077, 31.92103424516269783, -44.74231727136250214 ) ) ;
#34387 = DIRECTION ( 'NONE',  ( -0.7071067811865475727, 0.7071067811865475727, 0.000000000000000000 ) ) ;
#34388 = CARTESIAN_POINT ( 'NONE',  ( 65.04835540476229028, -32.26176030518409732, -17.85457486710349784 ) ) ;
#34389 = CARTESIAN_POINT ( 'NONE',  ( 9.449690553371750568, -17.28557240283720020, -47.76865470132936053 ) ) ;
#34390 = B_SPLINE_CURVE_WITH_KNOTS ( 'NONE', 3,
 ( #46437, #8319, #28217, #44218, #43018, #30415, #43275, #31437, #38828, #26744, #40292, #448, #18631, #46960, #6856, #47465 ),
 .UNSPECIFIED., .F., .F.,
 ( 4, 2, 2, 2, 2, 2, 2, 4 ),
 ( 0.000000000000000000, 0.1191611659050043209, 0.1489514573812555642, 0.1787417488575067936, 0.2383223318100099186, 0.2979029147625130158, 0.3574834977150160853, 0.4766446636200218356 ),
 .UNSPECIFIED. ) ;
#34391 = ORIENTED_EDGE ( 'NONE', *, *, #5721, .T. ) ;
#34392 = ORIENTED_EDGE ( 'NONE', *, *, #43709, .F. ) ;
#34393 = CARTESIAN_POINT ( 'NONE',  ( 56.87160281683760132, 19.05665430235150026, -52.71743055004790790 ) ) ;
#34394 = CARTESIAN_POINT ( 'NONE',  ( 49.96674047072312419, -1.429328268333673213, -15.94298744783530175 ) ) ;
#34395 = ORIENTED_EDGE ( 'NONE', *, *, #9053, .T. ) ;
#34396 = CARTESIAN_POINT ( 'NONE',  ( 11.35027784094959991, -64.43558176466569876, -44.57647092392380017 ) ) ;
#34397 = CARTESIAN_POINT ( 'NONE',  ( 57.63180676903699862, -45.11980367247790014, -25.34401879820149617 ) ) ;
#34398 = DIRECTION ( 'NONE',  ( 0.000000000000000000, -1.000000000000000000, 0.000000000000000000 ) ) ;
#34399 = ORIENTED_EDGE ( 'NONE', *, *, #49812, .F. ) ;
#34400 = FACE_OUTER_BOUND ( 'NONE', #30565, .T. ) ;
#34401 = CARTESIAN_POINT ( 'NONE',  ( 45.15161791705966721, 6.828204371508110881, -64.56158714047771241 ) ) ;
#34402 = CARTESIAN_POINT ( 'NONE',  ( -17.65868355449891069, 3.871249156093727439, -50.40641985204897679 ) ) ;
#34403 = VERTEX_POINT ( 'NONE', #9314 ) ;
#34404 = CARTESIAN_POINT ( 'NONE',  ( 55.55365765569959535, -45.11618894467940066, -14.32025624407079967 ) ) ;
#34405 = EDGE_CURVE ( 'NONE', #12296, #22390, #42402, .T. ) ;
#34406 = CARTESIAN_POINT ( 'NONE',  ( 16.13393739769620083, -15.61618894467929941, -644.5164532144519853 ) ) ;
#34407 = CARTESIAN_POINT ( 'NONE',  ( 15.59055465919079886, 19.84640421423560142, -21.35214379961290021 ) ) ;
#34408 = CARTESIAN_POINT ( 'NONE',  ( 15.12341578682209686, -22.32525615540303221, -51.00040296984943211 ) ) ;
#34409 = EDGE_CURVE ( 'NONE', #13535, #50973, #18629, .T. ) ;
#34410 = CYLINDRICAL_SURFACE ( 'NONE', #46953, 2.999999999999994227 ) ;
#34411 = CIRCLE ( 'NONE', #28532, 0.9999999999999974465 ) ;
#34412 = EDGE_CURVE ( 'NONE', #6571, #24387, #40483, .T. ) ;
#34413 = CARTESIAN_POINT ( 'NONE',  ( 73.18782247527531126, 0.8859637708054480809, -68.88406027352149863 ) ) ;
#34414 = CARTESIAN_POINT ( 'NONE',  ( 47.28690122458660028, -54.53046819659620326, -74.94574354657768822 ) ) ;
#34415 = CARTESIAN_POINT ( 'NONE',  ( 41.56665882477770424, 12.62342850819730167, -4.650889749848269084 ) ) ;
#34416 = AXIS2_PLACEMENT_3D ( 'NONE', #38026, #18615, #46162 ) ;
#34417 = ADVANCED_FACE ( 'NONE', ( #12447 ), #2003, .F. ) ;
#34418 = CARTESIAN_POINT ( 'NONE',  ( 49.40552051342540096, 22.26542118999089936, -54.15739458345379376 ) ) ;
#34419 = CARTESIAN_POINT ( 'NONE',  ( 51.74354725780179365, 19.79449691764480335, -76.13548132539280289 ) ) ;
#34420 = CARTESIAN_POINT ( 'NONE',  ( 61.75051681185560426, 13.88381108430350075, -28.08183634978059828 ) ) ;
#34421 = CARTESIAN_POINT ( 'NONE',  ( 13.96079765809810169, -23.15702522818530085, -77.87681711424819753 ) ) ;
#34422 = ORIENTED_EDGE ( 'NONE', *, *, #34098, .T. ) ;
#34423 = CARTESIAN_POINT ( 'NONE',  ( 9.366980835600751121, -15.61636285886159925, -47.84717978380999881 ) ) ;
#34424 = CARTESIAN_POINT ( 'NONE',  ( 0.7492974541592680726, -53.47458583507350482, -7.830755312676159541 ) ) ;
#34425 = CARTESIAN_POINT ( 'NONE',  ( 76.31778600806960355, 0.5058489486935060508, -12.80249019458479864 ) ) ;
#34427 = EDGE_CURVE ( 'NONE', #42834, #3712, #49921, .T. ) ;
#34426 = CARTESIAN_POINT ( 'NONE',  ( 75.28698268395557136, 13.41427130635144493, -14.07372847826834672 ) ) ;
#34428 = CARTESIAN_POINT ( 'NONE',  ( 71.52074786344310553, 0.8966068345641450277, -60.69721413447469871 ) ) ;
#34429 = CARTESIAN_POINT ( 'NONE',  ( 19.86710470927560834, -55.44147536898664441, -75.14569893017471713 ) ) ;
#34430 = CARTESIAN_POINT ( 'NONE',  ( 15.09844748716482599, -7.705181990897977506, -78.96600269184820320 ) ) ;
#34431 = CARTESIAN_POINT ( 'NONE',  ( 57.09195614716849576, -47.42783454384350250, -46.39999999999999858 ) ) ;
#34432 = CARTESIAN_POINT ( 'NONE',  ( 24.04511355972104170, -15.61618909363076924, -51.79233356384455078 ) ) ;
#34433 = CARTESIAN_POINT ( 'NONE',  ( 63.43393739769620510, 1.383811055320669947, -62.79342862858290886 ) ) ;
#34434 = DIRECTION ( 'NONE',  ( 0.000000000000000000, 0.000000000000000000, 1.000000000000000000 ) ) ;
#34435 = CARTESIAN_POINT ( 'NONE',  ( 41.08683620002359760, 13.04363067530499976, -3.799113739079239771 ) ) ;
#34436 = CARTESIAN_POINT ( 'NONE',  ( 61.35893852378349322, -45.52617362054395755, -47.58679445246438888 ) ) ;
#34437 = CARTESIAN_POINT ( 'NONE',  ( 20.13393739768846302, 24.18330853958629234, -74.40623532124070039 ) ) ;
#34438 = DIRECTION ( 'NONE',  ( 0.000000000000000000, 0.000000000000000000, 1.000000000000000000 ) ) ;
#34439 = CARTESIAN_POINT ( 'NONE',  ( 76.02169335355060298, -43.31998441844365288, -13.64721484880164937 ) ) ;
#34440 = CARTESIAN_POINT ( 'NONE',  ( 17.84255373986179904, -51.34461045802749624, -75.09854824053090283 ) ) ;
#34441 = DIRECTION ( 'NONE',  ( -0.8224686640529090820, -0.3976080002595601126, -0.4067593573362717763 ) ) ;
#34442 = VERTEX_POINT ( 'NONE', #44421 ) ;
#34443 = VECTOR ( 'NONE', #22687, 1000.000000000000000 ) ;
#34444 = CARTESIAN_POINT ( 'NONE',  ( 16.53341908198030197, -8.176625199252880449, -56.58441854867459853 ) ) ;
#34445 = CARTESIAN_POINT ( 'NONE',  ( 63.42524119458249743, 1.236214136009519793, -62.08583290503010232 ) ) ;
#34446 = ORIENTED_EDGE ( 'NONE', *, *, #43332, .F. ) ;
#34447 = CARTESIAN_POINT ( 'NONE',  ( -0.09052647982827211059, 22.39771960572409881, -9.857778326383000334 ) ) ;
#34448 = AXIS2_PLACEMENT_3D ( 'NONE', #27889, #39962, #32838 ) ;
#34449 = CARTESIAN_POINT ( 'NONE',  ( 16.13393739769620083, -15.61618894467929941, -7.049999999999999822 ) ) ;
#34450 = CARTESIAN_POINT ( 'NONE',  ( 22.90088226672064664, -16.00112289232146523, -74.86527751735805225 ) ) ;
#34451 = CARTESIAN_POINT ( 'NONE',  ( 7.523314408995544156, -61.08379353316595228, -20.29480228628006699 ) ) ;
#34452 = EDGE_CURVE ( 'NONE', #13586, #43378, #43604, .T. ) ;
#34453 = AXIS2_PLACEMENT_3D ( 'NONE', #41219, #20767, #37290 ) ;
#34454 = CARTESIAN_POINT ( 'NONE',  ( 40.57649240635721100, -15.61618894467929941, -83.97002642401369599 ) ) ;
#34455 = LINE ( 'NONE', #50461, #5222 ) ;
#34456 = ORIENTED_EDGE ( 'NONE', *, *, #3789, .F. ) ;
#34457 = VERTEX_POINT ( 'NONE', #25514 ) ;
#34458 = ORIENTED_EDGE ( 'NONE', *, *, #16508, .F. ) ;
#34459 = DIRECTION ( 'NONE',  ( -0.8224686640529097481, 0.3976080002595595575, -0.4067593573362710546 ) ) ;
#34460 = CARTESIAN_POINT ( 'NONE',  ( 61.06128757285269870, -45.34819059754200765, -46.84339011699150035 ) ) ;
#34461 = CARTESIAN_POINT ( 'NONE',  ( 68.13393739769620083, -42.61618894467930119, -65.65000000000000568 ) ) ;
#34462 = VERTEX_POINT ( 'NONE', #649 ) ;
#34463 = VERTEX_POINT ( 'NONE', #44941 ) ;
#34464 = CARTESIAN_POINT ( 'NONE',  ( 22.68450300562881239, -17.37076631674719351, -72.53614194588162434 ) ) ;
#34465 = APPLICATION_CONTEXT ( 'automotive_design' ) ;
#34466 = DIRECTION ( 'NONE',  ( 0.4872913772396111898, -0.8732394366197182567, 0.000000000000000000 ) ) ;
#34467 = EDGE_CURVE ( 'NONE', #42352, #14961, #9042, .T. ) ;
#34468 = EDGE_LOOP ( 'NONE', ( #27316, #39226, #25862, #3137, #47435 ) ) ;
#34469 = CARTESIAN_POINT ( 'NONE',  ( 15.67962062511290000, 19.63028992866140143, -15.65622423491010196 ) ) ;
#34470 = CARTESIAN_POINT ( 'NONE',  ( 52.12109123451309500, -50.88362419310729479, -76.21339085482510711 ) ) ;
#34471 = CARTESIAN_POINT ( 'NONE',  ( 60.91700494128750165, 14.27513245742689918, -47.41475498393460697 ) ) ;
#34472 = EDGE_CURVE ( 'NONE', #11677, #23424, #1178, .T. ) ;
#34473 = CARTESIAN_POINT ( 'NONE',  ( 23.43533467884909882, -18.49305274663100462, -78.13196779797910096 ) ) ;
#34474 = CARTESIAN_POINT ( 'NONE',  ( 2.428024600086259976, -5.435758813730029892, -34.95504743437659556 ) ) ;
#34475 = CARTESIAN_POINT ( 'NONE',  ( 41.44023858514859882, -43.98147948091650505, -3.815737768197240420 ) ) ;
#34476 = CARTESIAN_POINT ( 'NONE',  ( 23.83903865928639476, -17.68685956421354177, -79.59100355860006459 ) ) ;
#34477 = FACE_OUTER_BOUND ( 'NONE', #50849, .T. ) ;
#34478 = AXIS2_PLACEMENT_3D ( 'NONE', #47373, #43688, #19574 ) ;
#34479 = AXIS2_PLACEMENT_3D ( 'NONE', #2039, #49746, #26126 ) ;
#34480 = CIRCLE ( 'NONE', #11924, 14.49999999999999822 ) ;
#34481 = CARTESIAN_POINT ( 'NONE',  ( 64.39815381769149383, 0.9561815866734409974, -70.34594416269000305 ) ) ;
#34482 = CARTESIAN_POINT ( 'NONE',  ( 46.99617165126079499, 8.227715268217000499, -54.09194780417729476 ) ) ;
#34483 = DIRECTION ( 'NONE',  ( 0.000000000000000000, 1.000000000000000000, 0.000000000000000000 ) ) ;
#34484 = CARTESIAN_POINT ( 'NONE',  ( 9.502098035746389115, -11.42030347669100010, -50.46706696623599697 ) ) ;
#34485 = ORIENTED_EDGE ( 'NONE', *, *, #22929, .T. ) ;
#34486 = B_SPLINE_CURVE_WITH_KNOTS ( 'NONE', 3,
 ( #28930, #40224, #28406, #12713, #29188, #24724 ),
 .UNSPECIFIED., .F., .F.,
 ( 4, 2, 4 ),
 ( -0.1582496144710479891, -0.1579281415405880129, -0.1400863131347609980 ),
 .UNSPECIFIED. ) ;
#34487 = CARTESIAN_POINT ( 'NONE',  ( 14.83462289604239892, -52.80674074535599516, -76.12862656241330228 ) ) ;
#34488 = CARTESIAN_POINT ( 'NONE',  ( 57.55751162087899786, 18.89525652402230094, -52.61703142040180126 ) ) ;
#34490 = ADVANCED_FACE ( 'NONE', ( #17677 ), #26824, .T. ) ;
#34489 = CARTESIAN_POINT ( 'NONE',  ( 71.40227520965750330, 1.367045641526529964, -70.32522074196269557 ) ) ;
#34491 = B_SPLINE_CURVE_WITH_KNOTS ( 'NONE', 3,
 ( #8368, #489, #36137, #36384, #7603, #24058, #24316, #4428, #40335, #39565, #47693, #20397, #43753, #16478, #47949, #12051, #32433, #28003, #48455, #23805, #7855, #40077, #7612, #3929, #8112, #12561, #20146, #43501, #28523, #44521, #19641, #44009, #35633, #11796, #19889, #47346, #6733 ),
 .UNSPECIFIED., .F., .F.,
 ( 4, 2, 2, 2, 1, 1, 1, 2, 2, 2, 2, 1, 1, 2, 2, 2, 2, 1, 1, 2, 2, 4 ),
 ( 0.000000000000000000, 0.2499999999998844258, 0.3749999999998271383, 0.4374999999997926659, 0.4687499999997803424, 0.4843749999997737921, 0.4921874999997742361, 0.4960937499997697397, 0.4999999999997651878, 0.6249999999998444578, 0.6874999999998867573, 0.7187499999999088507, 0.7343749999999165112, 0.7421874999999231726, 0.7499999999999297229, 0.8124999999999729106, 0.8437499999999933387, 0.8593750000000016653, 0.8671875000000058842, 0.8710937500000075495, 0.8750000000000091038, 1.000000000000000000 ),
 .UNSPECIFIED. ) ;
#34492 = CARTESIAN_POINT ( 'NONE',  ( 44.35280653673021334, -39.98289970179189368, -64.95046479719039212 ) ) ;
#34493 = CARTESIAN_POINT ( 'NONE',  ( -9.882013117715120032, -40.49932216338130075, -19.14999999999999858 ) ) ;
#34494 = CARTESIAN_POINT ( 'NONE',  ( 22.02274569102419832, -11.87050655181369940, -32.14999999999999858 ) ) ;
#34495 = CARTESIAN_POINT ( 'NONE',  ( 63.26997363883779713, 1.264791438333819906, -68.87905435786350949 ) ) ;
#34496 = CARTESIAN_POINT ( 'NONE',  ( 47.99585623154239755, -54.37189248632540028, -55.05664384648260068 ) ) ;
#34497 = CARTESIAN_POINT ( 'NONE',  ( 16.13393739769620083, -15.61618894467929941, -22.14999999999999858 ) ) ;
#34498 = CARTESIAN_POINT ( 'NONE',  ( 68.13393739769620083, -42.61618894467930119, -60.14999999999999858 ) ) ;
#34499 = CARTESIAN_POINT ( 'NONE',  ( 47.85506559290410422, 23.21069065499990103, -55.16819991544539903 ) ) ;
#34500 = ORIENTED_EDGE ( 'NONE', *, *, #11252, .F. ) ;
#34501 = CARTESIAN_POINT ( 'NONE',  ( 9.089680483953220147, -15.96404481660830221, -69.83147392683879673 ) ) ;
#34502 = ORIENTED_EDGE ( 'NONE', *, *, #33093, .T. ) ;
#34503 = CARTESIAN_POINT ( 'NONE',  ( 71.45332619318591583, 1.096305581841150012, -70.60102141519101338 ) ) ;
#34504 = CARTESIAN_POINT ( 'NONE',  ( 88.13393739769620083, -15.61618894467929941, -65.65000000000000568 ) ) ;
#34505 = LINE ( 'NONE', #10681, #30251 ) ;
#34507 = CARTESIAN_POINT ( 'NONE',  ( 55.92723414887319677, 14.69231210900940177, -25.58060912393079533 ) ) ;
#34506 = DIRECTION ( 'NONE',  ( -0.8857883891771956009, -0.4640893551880597712, 0.000000000000000000 ) ) ;
#34508 = EDGE_CURVE ( 'NONE', #18282, #26915, #25478, .T. ) ;
#34509 = CARTESIAN_POINT ( 'NONE',  ( 21.59331255549819772, -20.08136325068349848, -76.67103925775420237 ) ) ;
#34510 = CARTESIAN_POINT ( 'NONE',  ( 51.13393739769659874, -50.61618894467899565, 11.34999999999999964 ) ) ;
#34511 = CARTESIAN_POINT ( 'NONE',  ( 71.44807725908989937, 0.8904513541338869853, -70.65165619965230803 ) ) ;
#34512 = CARTESIAN_POINT ( 'NONE',  ( 22.87920564048909000, -16.16927619967657392, -40.47885954242595119 ) ) ;
#34513 = VERTEX_POINT ( 'NONE', #32190 ) ;
#34514 = FACE_OUTER_BOUND ( 'NONE', #40966, .T. ) ;
#34515 = EDGE_CURVE ( 'NONE', #17783, #24458, #44021, .T. ) ;
#34516 = VERTEX_POINT ( 'NONE', #31171 ) ;
#34517 = ORIENTED_EDGE ( 'NONE', *, *, #10538, .T. ) ;
#34518 = CARTESIAN_POINT ( 'NONE',  ( 12.14266246861669885, -64.86007294939740575, -16.13799733648500023 ) ) ;
#34519 = AXIS2_PLACEMENT_3D ( 'NONE', #19065, #39003, #1352 ) ;
#34520 = DIRECTION ( 'NONE',  ( 0.000000000000000000, 0.000000000000000000, -1.000000000000000000 ) ) ;
#34521 = CARTESIAN_POINT ( 'NONE',  ( 12.15396043383179858, -65.41633662578259134, -47.50051160094690772 ) ) ;
#34522 = AXIS2_PLACEMENT_3D ( 'NONE', #39079, #35381, #2384 ) ;
#34523 = ORIENTED_EDGE ( 'NONE', *, *, #12523, .F. ) ;
#34524 = VERTEX_POINT ( 'NONE', #27248 ) ;
#34525 = CARTESIAN_POINT ( 'NONE',  ( 71.46698656264879901, 1.308647200627810259, -60.89791552425909771 ) ) ;
#34526 = DIRECTION ( 'NONE',  ( 0.000000000000000000, 0.000000000000000000, -1.000000000000000000 ) ) ;
#34527 = CARTESIAN_POINT ( 'NONE',  ( 53.52853389627100000, 18.17118327204569894, -49.18229249838620376 ) ) ;
#34528 = CARTESIAN_POINT ( 'NONE',  ( 61.24042730829579995, -2.108457229618950546, -15.95092827701309979 ) ) ;
#34529 = CARTESIAN_POINT ( 'NONE',  ( 50.98146090960219823, -49.40936669674759685, -76.31995468972489505 ) ) ;
#34530 = CARTESIAN_POINT ( 'NONE',  ( 57.99287681093679936, -49.02125455608680227, -51.32482328972750452 ) ) ;
#34531 = EDGE_CURVE ( 'NONE', #28005, #37478, #7613, .T. ) ;
#34532 = ORIENTED_EDGE ( 'NONE', *, *, #14598, .T. ) ;
#34533 = CARTESIAN_POINT ( 'NONE',  ( 14.63393739769620083, -42.11618894467930119, -34.64999999999999858 ) ) ;
#34534 = CARTESIAN_POINT ( 'NONE',  ( 68.13393739769814772, 19.38381105532029736, -71.50000000000200373 ) ) ;
#34535 = ORIENTED_EDGE ( 'NONE', *, *, #11675, .T. ) ;
#34536 = FACE_OUTER_BOUND ( 'NONE', #11040, .T. ) ;
#34537 = DIRECTION ( 'NONE',  ( 0.000000000000000000, 0.000000000000000000, -1.000000000000000000 ) ) ;
#34538 = EDGE_CURVE ( 'NONE', #26276, #2299, #39833, .T. ) ;
#34539 = CARTESIAN_POINT ( 'NONE',  ( 9.169509088546389464, -19.23329910588459768, -44.86001675125889676 ) ) ;
#34540 = CARTESIAN_POINT ( 'NONE',  ( 13.13600760831069891, -50.60910559520539920, -21.36925334575990121 ) ) ;
#34541 = AXIS2_PLACEMENT_3D ( 'NONE', #9470, #13907, #6306 ) ;
#34542 = CARTESIAN_POINT ( 'NONE',  ( 56.60748237810329897, 19.38381105532069881, -75.50618570370070870 ) ) ;
#34543 = CARTESIAN_POINT ( 'NONE',  ( 47.35405898648330236, -54.26885648339170842, -75.29488275581999801 ) ) ;
#34544 = CARTESIAN_POINT ( 'NONE',  ( 57.24676268689880487, 13.88381105532070059, -16.76478824873209916 ) ) ;
#34545 = DIRECTION ( 'NONE',  ( 0.000000000000000000, 0.000000000000000000, -1.000000000000000000 ) ) ;
#34546 = CARTESIAN_POINT ( 'NONE',  ( 56.66762828736870006, -50.37953306433199430, -52.77094437832339935 ) ) ;
#34547 = CARTESIAN_POINT ( 'NONE',  ( 21.74289213372750140, -11.34042165171269900, -44.63985384860789907 ) ) ;
#34548 = CARTESIAN_POINT ( 'NONE',  ( 1.277530937145179957, -21.88413813711040135, -34.64999999999999858 ) ) ;
#34549 = ORIENTED_EDGE ( 'NONE', *, *, #9038, .T. ) ;
#34550 = CARTESIAN_POINT ( 'NONE',  ( 46.35275103504439898, 21.67755452994670406, -76.14999999999999147 ) ) ;
#34551 = CARTESIAN_POINT ( 'NONE',  ( 64.92397392854900318, 1.188582381068100213, -60.69479001402090290 ) ) ;
#34552 = CARTESIAN_POINT ( 'NONE',  ( 9.221480375469107926, -11.63194448996753927, -50.67433467055431606 ) ) ;
#34553 = VECTOR ( 'NONE', #48706, 1000.000000000000000 ) ;
#34554 = CARTESIAN_POINT ( 'NONE',  ( 12.34963117160209833, -65.36344979145191303, -23.59691445115834796 ) ) ;
#34555 = VECTOR ( 'NONE', #9036, 1000.000000000000000 ) ;
#34556 = DIRECTION ( 'NONE',  ( 0.000000000000000000, 0.000000000000000000, 1.000000000000000000 ) ) ;
#34557 = FACE_OUTER_BOUND ( 'NONE', #23256, .T. ) ;
#34558 = CARTESIAN_POINT ( 'NONE',  ( 82.28938727573759593, 13.99365337418919886, -47.03253095781639814 ) ) ;
#34559 = CARTESIAN_POINT ( 'NONE',  ( -21.93025022046069950, -6.936381044561869658, -53.85448886108699185 ) ) ;
#34561 = CARTESIAN_POINT ( 'NONE',  ( 9.221488231078874165, -19.60044682611274069, -58.62566479439444578 ) ) ;
#34560 = CARTESIAN_POINT ( 'NONE',  ( 47.64116066081108158, 23.30216094288792661, -74.19778950641801885 ) ) ;
#34562 = CARTESIAN_POINT ( 'NONE',  ( 24.04283007690743545, -15.41892889378250864, -71.49973720589011350 ) ) ;
#34563 = DIRECTION ( 'NONE',  ( 0.000000000000000000, 1.000000000000000000, 0.000000000000000000 ) ) ;
#34564 = CARTESIAN_POINT ( 'NONE',  ( 12.93945173866060117, 34.17938410075420563, -46.97472070025120416 ) ) ;
#34565 = VERTEX_POINT ( 'NONE', #39320 ) ;
#34566 = CARTESIAN_POINT ( 'NONE',  ( 52.82044787969120136, -49.67922433927950010, -48.83393259163720046 ) ) ;
#34567 = ORIENTED_EDGE ( 'NONE', *, *, #22147, .T. ) ;
#34568 = CARTESIAN_POINT ( 'NONE',  ( 44.98679317390966048, 8.902100338333454488, -61.45383541554941331 ) ) ;
#34569 = CARTESIAN_POINT ( 'NONE',  ( 11.97539538442253537, -10.20477106632094966, -41.74448671497020058 ) ) ;
#34570 = CARTESIAN_POINT ( 'NONE',  ( 14.24102869631679802, 19.87035360122330019, -22.22788221432290001 ) ) ;
#34571 = DIRECTION ( 'NONE',  ( 0.000000000000000000, 0.000000000000000000, -1.000000000000000000 ) ) ;
#34572 = CARTESIAN_POINT ( 'NONE',  ( 21.07660274011399792, -20.64735362191730061, -40.70564455487090072 ) ) ;
#34573 = CARTESIAN_POINT ( 'NONE',  ( 9.366927619519092474, -16.50191557742974524, -77.41115605758611196 ) ) ;
#34574 = CARTESIAN_POINT ( 'NONE',  ( 53.05390108533369897, 18.34295525618989942, -49.03220057305669854 ) ) ;
#34575 = FACE_OUTER_BOUND ( 'NONE', #35980, .T. ) ;
#34576 = CARTESIAN_POINT ( 'NONE',  ( 16.49542438326771787, 19.87930237151499924, -15.67473697716815373 ) ) ;
#34577 = ADVANCED_FACE ( 'NONE', ( #24068 ), #47216, .T. ) ;
#34578 = ORIENTED_EDGE ( 'NONE', *, *, #44902, .T. ) ;
#34579 = CARTESIAN_POINT ( 'NONE',  ( 23.66891508207319816, -13.42282091850420045, -33.19733999436689942 ) ) ;
#34580 = ADVANCED_FACE ( 'NONE', ( #8377 ), #49714, .T. ) ;
#34581 = CARTESIAN_POINT ( 'NONE',  ( 72.79675206836721202, 1.372372808637219999, -68.90857576278480678 ) ) ;
#34582 = CARTESIAN_POINT ( 'NONE',  ( 12.82231730655639979, 34.27273057154270219, -47.70638112247609541 ) ) ;
#34583 = CARTESIAN_POINT ( 'NONE',  ( 73.13235683752471061, 1.096291039689170077, -62.40636042108670267 ) ) ;
#34584 = CARTESIAN_POINT ( 'NONE',  ( 10.88578148292680048, -65.03392828768018319, -17.73314437552549805 ) ) ;
#34585 = CARTESIAN_POINT ( 'NONE',  ( 53.39111139338680090, 18.13443291158960236, -48.76214190021520523 ) ) ;
#34586 = CARTESIAN_POINT ( 'NONE',  ( 15.07403858729344037, -23.52396399615719247, -76.33491533744847857 ) ) ;
#34587 = LINE ( 'NONE', #29622, #21801 ) ;
#34588 = VERTEX_POINT ( 'NONE', #31680 ) ;
#34589 = CARTESIAN_POINT ( 'NONE',  ( 44.07452568954059302, -33.11618894467940066, -54.64999999999999858 ) ) ;
#34590 = VERTEX_POINT ( 'NONE', #51374 ) ;
#34591 = CARTESIAN_POINT ( 'NONE',  ( 9.740906203438708388, -63.25244105705341013, -46.29739040527410054 ) ) ;
#34592 = CIRCLE ( 'NONE', #19525, 5.499999999999998224 ) ;
#34593 = PLANE ( 'NONE',  #34416 ) ;
#34594 = EDGE_LOOP ( 'NONE', ( #10320, #44932, #48437, #44623, #35802 ) ) ;
#34595 = CARTESIAN_POINT ( 'NONE',  ( 31.79224979287389985, -36.11618894467930119, -84.65000000000000568 ) ) ;
#34596 = CARTESIAN_POINT ( 'NONE',  ( 57.27851913721940491, 18.92138913705230152, -52.63313635947250191 ) ) ;
#34597 = CARTESIAN_POINT ( 'NONE',  ( 52.26113487638559718, 18.74837471589070148, -76.96437248003098830 ) ) ;
#34598 = EDGE_LOOP ( 'NONE', ( #18601, #47929, #45575, #18801, #12031 ) ) ;
#34599 = AXIS2_PLACEMENT_3D ( 'NONE', #50418, #42292, #17211 ) ;
#34600 = DIRECTION ( 'NONE',  ( -1.000000000000000000, 0.000000000000000000, 0.000000000000000000 ) ) ;
#34601 = FACE_BOUND ( 'NONE', #17932, .T. ) ;
#34602 = CARTESIAN_POINT ( 'NONE',  ( 82.62219371760957642, -45.06709663929255072, -46.37145547250047173 ) ) ;
#34603 = CARTESIAN_POINT ( 'NONE',  ( 24.04493740212382491, -14.58063858884763775, -69.75066784640594619 ) ) ;
#34604 = ADVANCED_FACE ( 'NONE', ( #4181 ), #6201, .T. ) ;
#34605 = CARTESIAN_POINT ( 'NONE',  ( 24.31016961241860130, -14.55225904714300000, -61.75114295834970335 ) ) ;
#34606 = DIRECTION ( 'NONE',  ( 0.000000000000000000, 0.000000000000000000, -1.000000000000000000 ) ) ;
#34607 = CARTESIAN_POINT ( 'NONE',  ( 45.31728293652347617, -38.07934818043975866, -63.73322212158187483 ) ) ;
#34608 = EDGE_LOOP ( 'NONE', ( #26495, #37686, #12662, #5859 ) ) ;
#34609 = DIRECTION ( 'NONE',  ( 0.000000000000000000, 1.000000000000000000, 0.000000000000000000 ) ) ;
#34610 = CARTESIAN_POINT ( 'NONE',  ( 11.83891062116510007, -9.528542536252919248, -55.53707855430759821 ) ) ;
#34611 = CARTESIAN_POINT ( 'NONE',  ( 9.453617838139571461, -19.16200623842560091, -32.14999999999999858 ) ) ;
#34612 = CIRCLE ( 'NONE', #3661, 30.99999999999999645 ) ;
#34613 = CARTESIAN_POINT ( 'NONE',  ( 17.25678305769739751, -43.96113075119600211, -62.64999999999999858 ) ) ;
#34614 = CARTESIAN_POINT ( 'NONE',  ( 57.36123081458359962, -50.13537923174280309, -52.61896056486340001 ) ) ;
#34615 = DIRECTION ( 'NONE',  ( 0.000000000000000000, 1.000000000000000000, 0.000000000000000000 ) ) ;
#34616 = CARTESIAN_POINT ( 'NONE',  ( 44.59157399860669813, -45.15507410885789596, -7.270416675856879785 ) ) ;
#34617 = DIRECTION ( 'NONE',  ( 0.000000000000000000, -1.000000000000000000, 0.000000000000000000 ) ) ;
#34618 = CARTESIAN_POINT ( 'NONE',  ( 21.17003102617220378, -22.14462533283520074, -67.79851897862869237 ) ) ;
#34619 = ORIENTED_EDGE ( 'NONE', *, *, #26161, .F. ) ;
#34620 = CARTESIAN_POINT ( 'NONE',  ( 52.59996064233959601, -49.82480704385319825, -27.82108120899960113 ) ) ;
#34621 = CARTESIAN_POINT ( 'NONE',  ( 56.46527518672509416, -50.77626718493720404, -74.14938318154928254 ) ) ;
#34623 = CARTESIAN_POINT ( 'NONE',  ( 46.67317881810730285, -39.12423041205359908, -34.65023821785899116 ) ) ;
#34622 = CARTESIAN_POINT ( 'NONE',  ( -6.505945840192179475, 14.80671025396210005, -5.054061883099680408 ) ) ;
#34624 = CARTESIAN_POINT ( 'NONE',  ( 47.54281612864539852, -54.55267448867429891, -54.67232832126270381 ) ) ;
#34625 = CARTESIAN_POINT ( 'NONE',  ( -10.90401617485183294, 10.24444606491774579, -20.56421356237309794 ) ) ;
#34626 = ORIENTED_EDGE ( 'NONE', *, *, #44465, .T. ) ;
#34627 = CARTESIAN_POINT ( 'NONE',  ( 52.82975622904280755, -49.66092049964720445, -48.47378032971909789 ) ) ;
#34628 = CARTESIAN_POINT ( 'NONE',  ( 47.52904197842820366, 23.35432397247770098, -55.02687474755870056 ) ) ;
#34629 = DIRECTION ( 'NONE',  ( 0.000000000000000000, 0.000000000000000000, -1.000000000000000000 ) ) ;
#34630 = CARTESIAN_POINT ( 'NONE',  ( 8.223251455316621161, -15.61600507739779786, -72.79233150823699816 ) ) ;
#34631 = FACE_OUTER_BOUND ( 'NONE', #32705, .T. ) ;
#34632 = CARTESIAN_POINT ( 'NONE',  ( 11.61081905484630106, 34.00625395061120315, -17.07039315353630116 ) ) ;
#34633 = LINE ( 'NONE', #17886, #32411 ) ;
#34634 = CARTESIAN_POINT ( 'NONE',  ( 53.11047200542400049, 18.28146774992270451, -48.81638559825469770 ) ) ;
#34635 = CARTESIAN_POINT ( 'NONE',  ( 22.90086341797264780, -15.61618933298137790, -46.45282805145726002 ) ) ;
#34636 = FACE_OUTER_BOUND ( 'NONE', #33142, .T. ) ;
#34637 = CARTESIAN_POINT ( 'NONE',  ( 53.13638922289359812, 18.11798713974379993, -27.41642391186969974 ) ) ;
#34638 = ADVANCED_FACE ( 'NONE', ( #3681 ), #8, .F. ) ;
#34639 = DIRECTION ( 'NONE',  ( 0.9441240636101839723, 0.3295902797598760925, 0.000000000000000000 ) ) ;
#34640 = CARTESIAN_POINT ( 'NONE',  ( 53.19546650609449756, -49.34483516088236854, -27.47723033151208938 ) ) ;
#34641 = CARTESIAN_POINT ( 'NONE',  ( 53.27384017177119802, 18.28364788282440045, -49.18478595043859514 ) ) ;
#34642 = CARTESIAN_POINT ( 'NONE',  ( 22.46009641123071532, -20.47787541989118409, -75.71601379394873277 ) ) ;
#34643 = CARTESIAN_POINT ( 'NONE',  ( 71.29455428839979447, 0.9209334348186318797, -60.54988453772739376 ) ) ;
#34644 = CARTESIAN_POINT ( 'NONE',  ( 10.49070242014079923, 32.02022178723940016, -45.62562209983570227 ) ) ;
#34645 = CARTESIAN_POINT ( 'NONE',  ( 72.75077066479440191, 1.389801772588449946, -62.42722031148289830 ) ) ;
#34646 = CARTESIAN_POINT ( 'NONE',  ( 65.62514207164689140, -31.75125826519879624, -17.33363148726699876 ) ) ;
#34647 = DIRECTION ( 'NONE',  ( 0.000000000000000000, 0.000000000000000000, -1.000000000000000000 ) ) ;
#34648 = EDGE_LOOP ( 'NONE', ( #11196, #37550, #13727, #27007 ) ) ;
#34649 = EDGE_LOOP ( 'NONE', ( #6239, #28010, #12805, #2066 ) ) ;
#34650 = AXIS2_PLACEMENT_3D ( 'NONE', #15615, #39718, #19794 ) ;
#34651 = CARTESIAN_POINT ( 'NONE',  ( 25.88393739769619728, -15.61618894467930119, -18.10000000000000142 ) ) ;
#34652 = CARTESIAN_POINT ( 'NONE',  ( 50.06027333097009091, -1.288484637660672227, -15.99592958142435961 ) ) ;
#34653 = VERTEX_POINT ( 'NONE', #500 ) ;
#34654 = CARTESIAN_POINT ( 'NONE',  ( 12.30224470026469952, -65.34897662448399558, -46.67366121987959815 ) ) ;
#34655 = CARTESIAN_POINT ( 'NONE',  ( 55.85886099614570099, -46.00927082832929926, -25.54551749004689754 ) ) ;
#34656 = CARTESIAN_POINT ( 'NONE',  ( 8.223516320988901285, -15.61608250808600040, -78.50766849176299900 ) ) ;
#34657 = CARTESIAN_POINT ( 'NONE',  ( 18.21836968370322296, -14.10176024214776547, -40.14999999999999858 ) ) ;
#34658 = CARTESIAN_POINT ( 'NONE',  ( 63.52011431889719972, 1.391252479931859964, -68.77264296518760034 ) ) ;
#34659 = VERTEX_POINT ( 'NONE', #32441 ) ;
#34660 = FACE_BOUND ( 'NONE', #30778, .T. ) ;
#34661 = CARTESIAN_POINT ( 'NONE',  ( 43.60039976138143913, 6.630830045952984975, -72.31767848873290916 ) ) ;
#34662 = CARTESIAN_POINT ( 'NONE',  ( 28.51189741163311098, -6.623074584604310644, -6.649999999999999467 ) ) ;
#34663 = VERTEX_POINT ( 'NONE', #40594 ) ;
#34664 = EDGE_CURVE ( 'NONE', #637, #1577, #4894, .T. ) ;
#34665 = CARTESIAN_POINT ( 'NONE',  ( 11.13175947076070038, -22.17064819186600033, -34.49983067246459001 ) ) ;
#34666 = DIRECTION ( 'NONE',  ( -0.3502816565540492477, 0.000000000000000000, 0.9366444154970182678 ) ) ;
#34667 = AXIS2_PLACEMENT_3D ( 'NONE', #41229, #25739, #34121 ) ;
#34668 = CARTESIAN_POINT ( 'NONE',  ( 15.45006552729070037, 19.88381503651260118, -21.87030236028560282 ) ) ;
#34669 = B_SPLINE_CURVE_WITH_KNOTS ( 'NONE', 3,
 ( #14651, #30621, #46646, #43726, #23262, #8335, #3387, #51337, #47920, #7574, #15435, #7313, #8083, #24029 ),
 .UNSPECIFIED., .F., .F.,
 ( 4, 2, 2, 2, 2, 2, 4 ),
 ( 0.000000000000000000, 0.2230684146599339335, 0.4157015722607838581, 0.5812982619188552524, 0.7468949515769266467, 0.9958599354359034539, 1.000000000000000000 ),
 .UNSPECIFIED. ) ;
#34670 = EDGE_CURVE ( 'NONE', #33885, #19450, #18720, .T. ) ;
#34671 = SHAPE_REPRESENTATION_RELATIONSHIP ( 'NONE' , 'NONE' ,  #28088, #14816 ) ;
#34672 = CARTESIAN_POINT ( 'NONE',  ( 20.95264282180487569, -20.36726231655321229, -46.70056344322360076 ) ) ;
#34673 = CIRCLE ( 'NONE', #43890, 34.41780050634729804 ) ;
#34674 = CARTESIAN_POINT ( 'NONE',  ( 63.15096886846599489, 0.8925687589132619282, -62.30780775221810330 ) ) ;
#34675 = CARTESIAN_POINT ( 'NONE',  ( 47.26708353449659938, -54.64268123122759846, -74.72363872023309739 ) ) ;
#34676 = CARTESIAN_POINT ( 'NONE',  ( 56.35995331962240584, 13.73636655591429978, -9.195822556514428925 ) ) ;
#34677 = CARTESIAN_POINT ( 'NONE',  ( 30.13393739769619728, 7.383811055320659733, -59.64999999999999147 ) ) ;
#34678 =( BOUNDED_CURVE ( )  B_SPLINE_CURVE ( 3, ( #51216, #27604, #35479, #11126 ),
 .UNSPECIFIED., .F., .T. ) 
 B_SPLINE_CURVE_WITH_KNOTS ( ( 4, 4 ),
 ( 4.511031059594358794, 4.587061149216624223 ),
 .UNSPECIFIED. ) 
 CURVE ( )  GEOMETRIC_REPRESENTATION_ITEM ( )  RATIONAL_B_SPLINE_CURVE ( ( 1.000000000000000000, 0.9995183434654335564, 0.9995183434654335564, 1.000000000000000000 ) ) 
 REPRESENTATION_ITEM ( '' )  );
#34679 = CARTESIAN_POINT ( 'NONE',  ( 60.53822230144759686, 13.88381112845349996, -26.37179243457269706 ) ) ;
#34680 = CARTESIAN_POINT ( 'NONE',  ( 8.331257654656530676, -16.45580007440739934, -80.25338504615679369 ) ) ;
#34681 = ORIENTED_EDGE ( 'NONE', *, *, #20937, .T. ) ;
#34682 = FACE_OUTER_BOUND ( 'NONE', #9297, .T. ) ;
#34683 = CIRCLE ( 'NONE', #49748, 28.27108544675919788 ) ;
#34684 = CARTESIAN_POINT ( 'NONE',  ( 2.539252561488040350, -55.76083552616880468, -9.526912277943489826 ) ) ;
#34685 = CARTESIAN_POINT ( 'NONE',  ( 76.41006197761831231, 4.471648996623030392, -13.20456822250660167 ) ) ;
#34686 = CARTESIAN_POINT ( 'NONE',  ( 75.19566803704495328, 13.64401423318863849, -14.39133821584264972 ) ) ;
#34687 = FACE_OUTER_BOUND ( 'NONE', #49856, .T. ) ;
#34688 = CARTESIAN_POINT ( 'NONE',  ( 71.33393739769628894, 10.88381105532070059, -69.84999999999999432 ) ) ;
#34689 = CARTESIAN_POINT ( 'NONE',  ( 22.46010630395649343, -20.47786184072016624, -36.00066267143122900 ) ) ;
#34690 = CARTESIAN_POINT ( 'NONE',  ( 82.13853704237929776, -45.53381088318579373, -47.59887875144359981 ) ) ;
#34691 = CARTESIAN_POINT ( 'NONE',  ( 12.89164060295139969, 19.08427617359420125, -21.19267904405079861 ) ) ;
#34692 = CARTESIAN_POINT ( 'NONE',  ( 11.13393741218609989, -63.52234717531779751, -24.14942545402350049 ) ) ;
#34693 = CARTESIAN_POINT ( 'NONE',  ( 41.67343726859200359, 12.74555918370619878, -4.319880481587650145 ) ) ;
#34694 = CARTESIAN_POINT ( 'NONE',  ( 66.70013194292150160, -29.76883965895079953, -17.02746303015019791 ) ) ;
#34695 = DIRECTION ( 'NONE',  ( 1.000000000000000000, 0.000000000000000000, 0.000000000000000000 ) ) ;
#34696 = CARTESIAN_POINT ( 'NONE',  ( 56.50531572827331672, 19.52721310988098224, -53.84464530972960716 ) ) ;
#34697 = EDGE_CURVE ( 'NONE', #16351, #44858, #46388, .T. ) ;
#34698 = TOROIDAL_SURFACE ( 'NONE', #22121, 32.00000000000000000, 1.000000000000000000 ) ;
#34699 = CARTESIAN_POINT ( 'NONE',  ( 28.13393739769619728, -22.54439217495490055, -47.64999999999999858 ) ) ;
#34700 = CARTESIAN_POINT ( 'NONE',  ( 18.01980923492579834, -51.98087455372210286, -75.71853508996549920 ) ) ;
#34701 = CARTESIAN_POINT ( 'NONE',  ( 60.43008559674330371, -45.11618894467940066, -10.91951671383950107 ) ) ;
#34702 = VERTEX_POINT ( 'NONE', #13105 ) ;
#34703 = EDGE_CURVE ( 'NONE', #18021, #4326, #21253, .T. ) ;
#34704 = CARTESIAN_POINT ( 'NONE',  ( 20.72562825268699882, -21.48330658714520069, -51.35596909847559743 ) ) ;
#34705 = CARTESIAN_POINT ( 'NONE',  ( 63.71314823352749812, 1.019773975906300034, -61.59278770926529489 ) ) ;
#34706 = ORIENTED_EDGE ( 'NONE', *, *, #16874, .T. ) ;
#34707 = DIRECTION ( 'NONE',  ( -0.7071067811865510144, -0.7071067811865440200, 0.000000000000000000 ) ) ;
#34708 = FACE_OUTER_BOUND ( 'NONE', #45583, .T. ) ;
#34709 = CARTESIAN_POINT ( 'NONE',  ( 73.19748134167231512, 1.099973129953850215, -68.78515728267289830 ) ) ;
#34710 = CARTESIAN_POINT ( 'NONE',  ( 14.36277915339450928, -9.025292619810310057, -73.86948688777668792 ) ) ;
#34711 = DIRECTION ( 'NONE',  ( 0.000000000000000000, 0.000000000000000000, -1.000000000000000000 ) ) ;
#34712 = CARTESIAN_POINT ( 'NONE',  ( 40.78718624821470229, -45.20719311071780311, -5.637855430988819805 ) ) ;
#34713 = ORIENTED_EDGE ( 'NONE', *, *, #43332, .T. ) ;
#34714 = VERTEX_POINT ( 'NONE', #13350 ) ;
#34715 = ORIENTED_EDGE ( 'NONE', *, *, #34879, .F. ) ;
#34716 = CARTESIAN_POINT ( 'NONE',  ( 57.30396242925620243, -45.11618894467940066, -16.63931852905170317 ) ) ;
#34717 = CARTESIAN_POINT ( 'NONE',  ( 61.30391243981929961, -45.22107206010090152, -46.44424457753540736 ) ) ;
#34718 = DIRECTION ( 'NONE',  ( 1.000000000000000000, 2.460964292799963328E-14, 0.000000000000000000 ) ) ;
#34719 = ORIENTED_EDGE ( 'NONE', *, *, #36465, .F. ) ;
#34720 = CARTESIAN_POINT ( 'NONE',  ( 41.61626771661330082, 4.883811055320659733, -82.23834840541459812 ) ) ;
#34721 = ORIENTED_EDGE ( 'NONE', *, *, #27786, .F. ) ;
#34722 = CARTESIAN_POINT ( 'NONE',  ( 18.20465886699604852, -7.911100698668976250, -63.37566613559571493 ) ) ;
#34723 = AXIS2_PLACEMENT_3D ( 'NONE', #28024, #20166, #4188 ) ;
#34724 = EDGE_CURVE ( 'NONE', #29477, #28389, #37173, .T. ) ;
#34725 = CARTESIAN_POINT ( 'NONE',  ( 68.13393739769618662, -28.66618894467939782, -100.2061629005786898 ) ) ;
#34726 = ORIENTED_EDGE ( 'NONE', *, *, #19790, .T. ) ;
#34727 = CARTESIAN_POINT ( 'NONE',  ( 0.2019267050626805393, -46.05559318631305388, -34.66067870389102978 ) ) ;
#34728 = CARTESIAN_POINT ( 'NONE',  ( 50.97250182500789606, -50.96425953204839487, -76.14992205317840046 ) ) ;
#34729 = CARTESIAN_POINT ( 'NONE',  ( 60.81754538871109617, 14.28754699922989957, -47.34637945857710406 ) ) ;
#34730 = CARTESIAN_POINT ( 'NONE',  ( 16.13393739769620083, -15.61618894467929941, -23.15000000000000213 ) ) ;
#34731 = CARTESIAN_POINT ( 'NONE',  ( 42.73119093455760265, -42.90850753387979921, -3.876063987003000033 ) ) ;
#34732 = CARTESIAN_POINT ( 'NONE',  ( 16.13393739769620083, -15.61618894467929941, 16.85000000000000142 ) ) ;
#34733 = CARTESIAN_POINT ( 'NONE',  ( -10.41738590414109922, 11.58576686758640051, -6.158695775020420093 ) ) ;
#34734 = CARTESIAN_POINT ( 'NONE',  ( 64.73021287799150514, 1.402114179617120149, -70.19765531490459409 ) ) ;
#34735 = CARTESIAN_POINT ( 'NONE',  ( 18.19108902640490300, -22.36234980482461410, -39.25296653628198129 ) ) ;
#34736 = CARTESIAN_POINT ( 'NONE',  ( 56.16732778809232229, -50.61618894467929408, -76.24890161720091442 ) ) ;
#34737 = CARTESIAN_POINT ( 'NONE',  ( 8.807536104933550547, -18.42876646016020104, -56.17083000281660077 ) ) ;
#34738 = VERTEX_POINT ( 'NONE', #754 ) ;
#34739 = CARTESIAN_POINT ( 'NONE',  ( 14.86387764175020010, -52.78596775754549952, -76.12812327221449493 ) ) ;
#34740 = CARTESIAN_POINT ( 'NONE',  ( 57.41838965642980241, 19.15902291818160208, -52.99946191110650062 ) ) ;
#34741 = PRODUCT_DEFINITION_CONTEXT ( 'detailed design', #34465, 'design' ) ;
#34742 = CARTESIAN_POINT ( 'NONE',  ( 71.56069454884870140, 1.310552739454249993, -70.35422282388560689 ) ) ;
#34743 = CARTESIAN_POINT ( 'NONE',  ( 45.98590630150382452, -40.09308313156154213, -57.02683514883391069 ) ) ;
#34744 = CARTESIAN_POINT ( 'NONE',  ( 15.72190426420170084, 19.65388757372259931, -20.14992017774509847 ) ) ;
#34745 = CARTESIAN_POINT ( 'NONE',  ( 47.10254288570079950, -54.62488891218850284, -75.00961804031550173 ) ) ;
#34746 = AXIS2_PLACEMENT_3D ( 'NONE', #6605, #45662, #46197 ) ;
#34747 = CYLINDRICAL_SURFACE ( 'NONE', #10326, 6.766999999999998572 ) ;
#34748 = CARTESIAN_POINT ( 'NONE',  ( 72.38393739883420608, 20.38443354211860026, -61.34712802272770915 ) ) ;
#34749 = CARTESIAN_POINT ( 'NONE',  ( 47.96382216759450046, -54.39756210150869720, -55.24304179605790210 ) ) ;
#34750 = AXIS2_PLACEMENT_3D ( 'NONE', #18237, #26606, #34204 ) ;
#34751 = DIRECTION ( 'NONE',  ( 0.000000000000000000, 0.000000000000000000, -1.000000000000000000 ) ) ;
#34752 = EDGE_CURVE ( 'NONE', #25873, #8693, #25370, .T. ) ;
#34753 = CARTESIAN_POINT ( 'NONE',  ( 56.47388559847279765, 19.45410061890109787, -53.28105505440650091 ) ) ;
#34754 = CARTESIAN_POINT ( 'NONE',  ( 3.133937397696200389, -15.61618894467929763, -5.690000000000000391 ) ) ;
#34755 = CARTESIAN_POINT ( 'NONE',  ( 18.20459011730063636, -7.911081268728054283, -71.37565166824786900 ) ) ;
#34756 = ORIENTED_EDGE ( 'NONE', *, *, #47912, .T. ) ;
#34757 = EDGE_CURVE ( 'NONE', #27942, #38690, #20465, .T. ) ;
#34758 = CARTESIAN_POINT ( 'NONE',  ( 15.93498023681340037, -22.66622264832809819, -69.35616034045719402 ) ) ;
#34759 = EDGE_CURVE ( 'NONE', #17323, #15326, #17278, .T. ) ;
#34760 = ORIENTED_EDGE ( 'NONE', *, *, #48497, .T. ) ;
#34761 = CARTESIAN_POINT ( 'NONE',  ( 71.48394854028050815, 1.096932441169210071, -70.58143231363629866 ) ) ;
#34762 = CARTESIAN_POINT ( 'NONE',  ( 60.76394125543679792, -45.50397866361529964, -47.09160526915939471 ) ) ;
#34763 = CARTESIAN_POINT ( 'NONE',  ( 82.74185698189259597, 14.32742998458173389, -47.63394792283020962 ) ) ;
#34765 = CARTESIAN_POINT ( 'NONE',  ( 9.660248756158969385, -13.05489770709887232, -57.96762872684301726 ) ) ;
#34764 = CARTESIAN_POINT ( 'NONE',  ( 16.13393739767329649, -15.61618894439989980, -19.08999999984770213 ) ) ;
#34767 = EDGE_CURVE ( 'NONE', #35735, #23493, #27102, .T. ) ;
#34766 = CARTESIAN_POINT ( 'NONE',  ( 16.34294028551579814, -22.66593182482080238, -79.33774565447309612 ) ) ;
#34768 = CARTESIAN_POINT ( 'NONE',  ( 11.27236649766430077, -9.289942694860799932, -67.08399747395723978 ) ) ;
#34769 = CARTESIAN_POINT ( 'NONE',  ( 56.83722670948610300, 19.42668272705650168, -53.85090158270489979 ) ) ;
#34770 = ORIENTED_EDGE ( 'NONE', *, *, #42141, .F. ) ;
#34771 = DIRECTION ( 'NONE',  ( 0.000000000000000000, 0.000000000000000000, 1.000000000000000000 ) ) ;
#34772 = VECTOR ( 'NONE', #34995, 1000.000000000000000 ) ;
#34773 = VERTEX_POINT ( 'NONE', #44792 ) ;
#34774 = ORIENTED_EDGE ( 'NONE', *, *, #43527, .F. ) ;
#34775 = CARTESIAN_POINT ( 'NONE',  ( 12.17667205660399965, -64.95597786680379215, -16.26506704565129979 ) ) ;
#34776 = CARTESIAN_POINT ( 'NONE',  ( 15.09832557892497462, -7.705196720676832811, -39.25065852084387075 ) ) ;
#34777 = CYLINDRICAL_SURFACE ( 'NONE', #10984, 0.5000000000000000000 ) ;
#34778 = CARTESIAN_POINT ( 'NONE',  ( 10.97075952977539970, -64.83014200044789277, -46.68587730848879858 ) ) ;
#34779 = CIRCLE ( 'NONE', #11427, 10.27649999999999686 ) ;
#34780 = VERTEX_POINT ( 'NONE', #24847 ) ;
#34781 = ORIENTED_EDGE ( 'NONE', *, *, #11357, .F. ) ;
#34782 = CARTESIAN_POINT ( 'NONE',  ( 64.93393739769619799, 1.883811055320669947, -60.94999999999999574 ) ) ;
#34783 = VECTOR ( 'NONE', #20830, 1000.000000000000114 ) ;
#34784 = CARTESIAN_POINT ( 'NONE',  ( 56.68140060072190067, 14.86855146348369949, -26.25318016425800138 ) ) ;
#34785 = CARTESIAN_POINT ( 'NONE',  ( 22.90093562328744170, -15.61111289037969563, -46.45258946822546875 ) ) ;
#34786 = CARTESIAN_POINT ( 'NONE',  ( 63.21052810172120218, 0.2212761650789459855, -16.92427711443150073 ) ) ;
#34787 = EDGE_CURVE ( 'NONE', #49131, #26597, #40854, .T. ) ;
#34788 = CARTESIAN_POINT ( 'NONE',  ( 51.63018455908149917, -48.77028295090120480, -76.93968096216320873 ) ) ;
#34789 = CARTESIAN_POINT ( 'NONE',  ( 57.10007285306519975, -49.84413130755979893, -52.15317371639780220 ) ) ;
#34790 = EDGE_LOOP ( 'NONE', ( #46093, #4096, #43883, #1156 ) ) ;
#34791 = CARTESIAN_POINT ( 'NONE',  ( 16.13393739769620083, -15.61618894467929941, -54.64999999999999858 ) ) ;
#34792 = CARTESIAN_POINT ( 'NONE',  ( 17.30144337755940143, -22.57172551362165436, -51.29424405796996211 ) ) ;
#34793 = EDGE_LOOP ( 'NONE', ( #2464, #42278, #3417, #25502 ) ) ;
#34794 = DIRECTION ( 'NONE',  ( 1.000000000000000000, 0.000000000000000000, 0.000000000000000000 ) ) ;
#34795 = CARTESIAN_POINT ( 'NONE',  ( 50.64365103579869754, -45.11618894467940066, -10.74058096729739908 ) ) ;
#34796 = AXIS2_PLACEMENT_3D ( 'NONE', #14334, #18256, #13318 ) ;
#34797 = CARTESIAN_POINT ( 'NONE',  ( 22.97746258194329982, -11.77523715584399966, -41.84969737084139751 ) ) ;
#34798 = TOROIDAL_SURFACE ( 'NONE', #32268, 17.19098300429530113, 0.5000000000822009127 ) ;
#34799 = CARTESIAN_POINT ( 'NONE',  ( 13.72891830083070097, -51.14266425624079915, -22.20512176267040161 ) ) ;
#34800 = CARTESIAN_POINT ( 'NONE',  ( 54.17308252196429663, 19.39393527511609605, -76.74823974466679033 ) ) ;
#34801 = CARTESIAN_POINT ( 'NONE',  ( 21.21177448403727794, -10.72148469424713468, -64.60302447664658132 ) ) ;
#34802 = CARTESIAN_POINT ( 'NONE',  ( 55.75423648348099448, 13.88381105532070059, -14.60095162971360061 ) ) ;
#34803 = CARTESIAN_POINT ( 'NONE',  ( 15.24817962068161670, -8.849184057285455651, -77.91115211152967390 ) ) ;
#34804 = CARTESIAN_POINT ( 'NONE',  ( 56.46340970796750014, -50.48601309047270291, -52.83593731299979623 ) ) ;
#34805 = ADVANCED_FACE ( 'NONE', ( #25107 ), #10948, .T. ) ;
#34806 = CARTESIAN_POINT ( 'NONE',  ( 10.68011837214289983, -11.14422995437500141, -46.06579460775299140 ) ) ;
#34807 = CARTESIAN_POINT ( 'NONE',  ( 46.68560842045859971, -39.85656240628109970, -54.55231085272809821 ) ) ;
#34808 = EDGE_LOOP ( 'NONE', ( #13221, #4222, #10311, #20158, #48045 ) ) ;
#34809 = CARTESIAN_POINT ( 'NONE',  ( 47.56593113937609729, 23.24463118434199771, -74.72646171873358867 ) ) ;
#34810 = CARTESIAN_POINT ( 'NONE',  ( 64.82636581786128716, 1.096153228089730147, -60.69147900812899366 ) ) ;
#34811 = DIRECTION ( 'NONE',  ( 0.5000000000000012212, 0.8660254037844380415, 0.000000000000000000 ) ) ;
#34812 = CARTESIAN_POINT ( 'NONE',  ( 11.27236702745989305, -9.289942295366476088, -57.08399809234570199 ) ) ;
#34813 = CARTESIAN_POINT ( 'NONE',  ( 8.744443678271828446, -48.95118247924426669, -34.77532226276707661 ) ) ;
#34814 = CONICAL_SURFACE ( 'NONE', #12236, 0.6405000000000011795, 1.029744258676660307 ) ;
#34815 = DIRECTION ( 'NONE',  ( -0.6934629132905123505, -0.5038302981000507552, 0.5150380749100490485 ) ) ;
#34816 = CIRCLE ( 'NONE', #18929, 3.500000000000003109 ) ;
#34817 = CARTESIAN_POINT ( 'NONE',  ( 53.91121044660913242, -51.22748541984103809, -75.56421356237309794 ) ) ;
#34818 = CARTESIAN_POINT ( 'NONE',  ( -21.99696017279149984, -6.875435248926140552, -54.08310780595149936 ) ) ;
#34820 = CARTESIAN_POINT ( 'NONE',  ( 20.99565695329222947, -21.94232104174841780, -58.08399797440581125 ) ) ;
#34819 = CARTESIAN_POINT ( 'NONE',  ( 53.11711210633388447, 19.14144468090594842, -77.21690156005293204 ) ) ;
#34821 = CARTESIAN_POINT ( 'NONE',  ( 62.63393739769619373, -53.11618894467930119, 16.35000000000000142 ) ) ;
#34822 = CARTESIAN_POINT ( 'NONE',  ( 49.46107350807110237, 22.52470162032749812, -55.06157209291070131 ) ) ;
#34823 = ORIENTED_EDGE ( 'NONE', *, *, #1995, .F. ) ;
#34824 = EDGE_CURVE ( 'NONE', #6632, #46602, #51563, .T. ) ;
#34825 =( BOUNDED_CURVE ( )  B_SPLINE_CURVE ( 3, ( #20345, #1227, #36331, #17216 ),
 .UNSPECIFIED., .F., .T. ) 
 B_SPLINE_CURVE_WITH_KNOTS ( ( 4, 4 ),
 ( 2.369247656320500273, 2.476279911527849986 ),
 .UNSPECIFIED. ) 
 CURVE ( )  GEOMETRIC_REPRESENTATION_ITEM ( )  RATIONAL_B_SPLINE_CURVE ( ( 1.000000000000000000, 0.9990455691836308549, 0.9990455691836308549, 1.000000000000000000 ) ) 
 REPRESENTATION_ITEM ( '' )  );
#34826 = CARTESIAN_POINT ( 'NONE',  ( 52.81564609458730075, -49.67679338445299919, -48.78617142090899961 ) ) ;
#34827 = VERTEX_POINT ( 'NONE', #15149 ) ;
#34828 = CARTESIAN_POINT ( 'NONE',  ( 44.51201659540226530, 8.863513744426830598, -63.77110661413982484 ) ) ;
#34829 = CIRCLE ( 'NONE', #3911, 0.5000000000000004441 ) ;
#34830 = CARTESIAN_POINT ( 'NONE',  ( -31.36606260230380272, -53.11618894467930119, 16.35000000000000142 ) ) ;
#34831 = CARTESIAN_POINT ( 'NONE',  ( 13.97461707658050045, 19.95444906452859968, -22.92155397991069776 ) ) ;
#34832 = CARTESIAN_POINT ( 'NONE',  ( 51.95832179060779765, -49.45171672659990492, -77.09973274272179822 ) ) ;
#34833 = CARTESIAN_POINT ( 'NONE',  ( 10.59069679657289953, -19.97681302096509981, -43.24065034890669068 ) ) ;
#34835 = EDGE_CURVE ( 'NONE', #4255, #9060, #48887, .T. ) ;
#34834 = CARTESIAN_POINT ( 'NONE',  ( 53.05450032218360690, 18.36301419135650193, -49.09560402782900468 ) ) ;
#34836 = CARTESIAN_POINT ( 'NONE',  ( 54.62219313239500451, -46.21587333935030273, -15.85441571428080110 ) ) ;
#34837 = CARTESIAN_POINT ( 'NONE',  ( 15.29511290902279974, -43.80059717415329601, -59.64999999999999147 ) ) ;
#34838 = VECTOR ( 'NONE', #27377, 1000.000000000000000 ) ;
#34839 = ORIENTED_EDGE ( 'NONE', *, *, #35145, .T. ) ;
#34840 = CARTESIAN_POINT ( 'NONE',  ( 11.75167936957159931, -21.86538255309680068, -31.98264971805809509 ) ) ;
#34841 = VERTEX_POINT ( 'NONE', #35043 ) ;
#34842 = CARTESIAN_POINT ( 'NONE',  ( 10.96947337815119994, -65.06555250629570253, -17.60046538708800057 ) ) ;
#34843 = CARTESIAN_POINT ( 'NONE',  ( 9.227644565586000880, 32.59853923576839918, -46.67822069845360033 ) ) ;
#34844 = CARTESIAN_POINT ( 'NONE',  ( 72.87455824417580175, 1.326134026835569912, -62.35486255807249734 ) ) ;
#34845 = CARTESIAN_POINT ( 'NONE',  ( 18.20454585312310058, -23.32130913405535821, -40.20901186456822529 ) ) ;
#34846 = CARTESIAN_POINT ( 'NONE',  ( 68.13393739769624347, 1.383811055320669947, -71.15000000000000568 ) ) ;
#34847 = CARTESIAN_POINT ( 'NONE',  ( 68.13393739769620083, 1.383811055320669947, -65.65000000000000568 ) ) ;
#34848 = CARTESIAN_POINT ( 'NONE',  ( 50.03996090745119574, -53.49158772749100166, -54.67836234838419784 ) ) ;
#34849 = ORIENTED_EDGE ( 'NONE', *, *, #14209, .F. ) ;
#34850 = DIRECTION ( 'NONE',  ( -0.3502816565540492477, 0.000000000000000000, 0.9366444154970182678 ) ) ;
#34851 = ORIENTED_EDGE ( 'NONE', *, *, #44814, .F. ) ;
#34852 = CARTESIAN_POINT ( 'NONE',  ( 9.734484948842229812, -63.18888116458209936, -46.29877033112669693 ) ) ;
#34853 = AXIS2_PLACEMENT_3D ( 'NONE', #9829, #45996, #25782 ) ;
#34854 = CARTESIAN_POINT ( 'NONE',  ( 20.06281976506910070, -10.10654536788180025, -32.14999999999999858 ) ) ;
#34855 = ORIENTED_EDGE ( 'NONE', *, *, #36672, .F. ) ;
#34856 = CARTESIAN_POINT ( 'NONE',  ( 11.49293641769672547, -64.67039120822151688, -44.68941564908284647 ) ) ;
#34857 = CARTESIAN_POINT ( 'NONE',  ( 57.07894513400979974, 18.98008675654529753, -52.67137582195630330 ) ) ;
#34858 = CARTESIAN_POINT ( 'NONE',  ( 52.87559984714759764, 19.04777732598209994, -77.15855498664130607 ) ) ;
#34859 = ORIENTED_EDGE ( 'NONE', *, *, #76, .T. ) ;
#34860 = CARTESIAN_POINT ( 'NONE',  ( 16.13393739769620083, -15.61618894467929941, -11.54999999999999893 ) ) ;
#34861 = CARTESIAN_POINT ( 'NONE',  ( 51.76047950956269261, 20.08324044957887722, -76.04144537520551239 ) ) ;
#34862 = FACE_OUTER_BOUND ( 'NONE', #50091, .T. ) ;
#34863 = CARTESIAN_POINT ( 'NONE',  ( 17.63393739769620083, -32.15793020853440254, -34.64999999999999858 ) ) ;
#34864 = CARTESIAN_POINT ( 'NONE',  ( 8.220228225067870653, -17.93047656444329974, -62.70177013111309350 ) ) ;
#34865 = LINE ( 'NONE', #10781, #41388 ) ;
#34866 = DIRECTION ( 'NONE',  ( 0.000000000000000000, 0.000000000000000000, 1.000000000000000000 ) ) ;
#34867 = ORIENTED_EDGE ( 'NONE', *, *, #12703, .F. ) ;
#34868 = B_SPLINE_CURVE_WITH_KNOTS ( 'NONE', 3,
 ( #17001, #32948, #48974, #13080 ),
 .UNSPECIFIED., .F., .F.,
 ( 4, 4 ),
 ( 0.000000000000000000, 1.000000000000000000 ),
 .UNSPECIFIED. ) ;
#34869 = EDGE_LOOP ( 'NONE', ( #42223, #3545, #7461, #13323, #27384 ) ) ;
#34870 = DIRECTION ( 'NONE',  ( 1.000000000000000000, 0.000000000000000000, 0.000000000000000000 ) ) ;
#34871 = CARTESIAN_POINT ( 'NONE',  ( 22.70391683925680226, -19.12931631820509892, -58.38896007259789656 ) ) ;
#34872 = AXIS2_PLACEMENT_3D ( 'NONE', #5475, #37432, #25610 ) ;
#34873 = EDGE_CURVE ( 'NONE', #32383, #6259, #43446, .T. ) ;
#34874 = CARTESIAN_POINT ( 'NONE',  ( 9.718208567743850779, -12.68094353378160122, -32.14999999999999858 ) ) ;
#34875 = AXIS2_PLACEMENT_3D ( 'NONE', #41032, #40772, #16406 ) ;
#34876 = EDGE_CURVE ( 'NONE', #25290, #20336, #43022, .T. ) ;
#34877 = CARTESIAN_POINT ( 'NONE',  ( 63.88393739769619373, 20.38443354211860026, -61.34712802272770915 ) ) ;
#34878 = DIRECTION ( 'NONE',  ( 0.2992932829740320710, 0.8274908255099422405, 0.4750604850579560612 ) ) ;
#34879 = EDGE_CURVE ( 'NONE', #16544, #12971, #22876, .T. ) ;
#34880 = DIRECTION ( 'NONE',  ( 0.000000000000000000, 0.000000000000000000, 1.000000000000000000 ) ) ;
#34881 = CARTESIAN_POINT ( 'NONE',  ( 11.89829296290529825, 33.59996124671599915, -16.17105426248049937 ) ) ;
#34882 = CARTESIAN_POINT ( 'NONE',  ( 24.29065960009049974, -14.41177887250970002, -61.46100449353919259 ) ) ;
#34883 = CARTESIAN_POINT ( 'NONE',  ( 19.55461702279360026, -22.74941205225439944, -32.14999999999999858 ) ) ;
#34884 = CARTESIAN_POINT ( 'NONE',  ( 56.68182224158719862, -50.69727463636530018, -74.32273727118189299 ) ) ;
#34886 = DIRECTION ( 'NONE',  ( 1.000000000000000000, 0.000000000000000000, 0.000000000000000000 ) ) ;
#34885 = CARTESIAN_POINT ( 'NONE',  ( 0.9417307494557060066, 22.43464593454210032, -8.026335962152479908 ) ) ;
#34887 = DIRECTION ( 'NONE',  ( -1.000000000000000000, 0.000000000000000000, 0.000000000000000000 ) ) ;
#34888 = DIRECTION ( 'NONE',  ( 0.000000000000000000, 0.000000000000000000, -1.000000000000000000 ) ) ;
#34889 = ORIENTED_EDGE ( 'NONE', *, *, #36465, .T. ) ;
#34890 = CARTESIAN_POINT ( 'NONE',  ( -9.115847631259869743, -44.02029276258719648, -5.453298411520159483 ) ) ;
#34891 = CARTESIAN_POINT ( 'NONE',  ( 47.63955984696239909, 23.29747590340559782, -54.97543810062130376 ) ) ;
#34892 = AXIS2_PLACEMENT_3D ( 'NONE', #2157, #2934, #26502 ) ;
#34893 = CARTESIAN_POINT ( 'NONE',  ( 42.75216321632269967, -44.98233172091430276, -6.093641062779489914 ) ) ;
#34894 = CARTESIAN_POINT ( 'NONE',  ( 68.13393739769618662, -29.16618894467940137, -65.65000000000000568 ) ) ;
#34895 = CARTESIAN_POINT ( 'NONE',  ( 61.22235620690700131, 14.10114171156870100, -47.17370879253629568 ) ) ;
#34896 = CARTESIAN_POINT ( 'NONE',  ( 11.71337180106040066, 34.04767145060470313, -17.10636616733519944 ) ) ;
#34897 = CARTESIAN_POINT ( 'NONE',  ( 51.99246080072069986, 18.79347982688590335, -76.70334503327950415 ) ) ;
#34899 = EDGE_CURVE ( 'NONE', #7417, #1209, #12973, .T. ) ;
#34898 = CARTESIAN_POINT ( 'NONE',  ( 52.81905492317230255, 18.43458074482090225, -48.62056802018800283 ) ) ;
#34900 = CARTESIAN_POINT ( 'NONE',  ( 22.46011244405145746, -20.47785341715781371, -70.00066732382580881 ) ) ;
#34901 = CARTESIAN_POINT ( 'NONE',  ( 53.30277398520820498, -49.41309324413840187, -48.78464791978760218 ) ) ;
#34902 = CARTESIAN_POINT ( 'NONE',  ( 54.50135132931570325, 16.78773581522769831, -26.62868989851730106 ) ) ;
#34903 = CARTESIAN_POINT ( 'NONE',  ( 51.22043009712629669, 21.75654279735209684, -54.39216491918590179 ) ) ;
#34904 = CARTESIAN_POINT ( 'NONE',  ( 54.25582316535073346, -48.40199966990474678, -26.87775820864355936 ) ) ;
#34905 = DIRECTION ( 'NONE',  ( -1.000000000000000000, -1.964275807512749840E-11, -1.002496760437719626E-21 ) ) ;
#34906 = CARTESIAN_POINT ( 'NONE',  ( 17.16946523506752342, -23.52719174747369024, -75.96602405197781138 ) ) ;
#34907 = CARTESIAN_POINT ( 'NONE',  ( 71.01106396815980304, 1.383811055320669947, -60.95624653118409242 ) ) ;
#34908 = CARTESIAN_POINT ( 'NONE',  ( 11.13393739769619906, 32.08797975232909749, -43.91615438303840335 ) ) ;
#34909 = DIRECTION ( 'NONE',  ( 0.000000000000000000, 1.000000000000000000, 0.000000000000000000 ) ) ;
#34910 = CIRCLE ( 'NONE', #21516, 0.5000000000000004441 ) ;
#34911 = CARTESIAN_POINT ( 'NONE',  ( 65.66432530626940434, -32.39603305783209919, -18.02567142080080131 ) ) ;
#34912 = CARTESIAN_POINT ( 'NONE',  ( 48.94270149030809591, -51.80671227847209792, -55.11972614036100282 ) ) ;
#34913 = VERTEX_POINT ( 'NONE', #43193 ) ;
#34914 = EDGE_LOOP ( 'NONE', ( #20466, #38520, #44881, #25745 ) ) ;
#34915 = CARTESIAN_POINT ( 'NONE',  ( 21.99623050575980798, -19.53742327708051008, -37.03483646650040129 ) ) ;
#34916 = CARTESIAN_POINT ( 'NONE',  ( 51.07460838780723122, 0.2638179241706318234, -16.96543469932025872 ) ) ;
#34917 = VERTEX_POINT ( 'NONE', #4833 ) ;
#34918 = CARTESIAN_POINT ( 'NONE',  ( 12.66783529652720119, -65.47373773509440298, -47.23930563553710726 ) ) ;
#34919 = CARTESIAN_POINT ( 'NONE',  ( 57.20761488960310004, -45.15217172719249561, -25.52117527002110009 ) ) ;
#34920 = CARTESIAN_POINT ( 'NONE',  ( 0.7461747575530269794, -8.744437018640690340, -34.70985242058479514 ) ) ;
#34921 = CARTESIAN_POINT ( 'NONE',  ( 6.531828926332683416, -46.09336100234546763, -20.85710678118654471 ) ) ;
#34922 = ORIENTED_EDGE ( 'NONE', *, *, #48165, .T. ) ;
#34923 = CARTESIAN_POINT ( 'NONE',  ( 11.67118088809841403, 34.15913531565607286, -22.47626263540971436 ) ) ;
#34924 = CARTESIAN_POINT ( 'NONE',  ( 44.97616441016351274, 6.807270547622365164, -65.43885644857014938 ) ) ;
#34925 = CARTESIAN_POINT ( 'NONE',  ( 11.31451853429699916, 33.98448577272930038, -22.84783898345410336 ) ) ;
#34926 = ORIENTED_EDGE ( 'NONE', *, *, #37343, .F. ) ;
#34927 = CARTESIAN_POINT ( 'NONE',  ( 14.58885284465669940, -7.517087735128769488, -33.23232777544669148 ) ) ;
#34928 = DIRECTION ( 'NONE',  ( 1.000000000000000000, 0.000000000000000000, 0.000000000000000000 ) ) ;
#34929 = CARTESIAN_POINT ( 'NONE',  ( 8.222678474964419948, -15.61600660124389961, -50.79233150823699816 ) ) ;
#34930 = CARTESIAN_POINT ( 'NONE',  ( 22.77115846768018415, -16.96893195659617959, -50.51679219443402502 ) ) ;
#34931 = CARTESIAN_POINT ( 'NONE',  ( 60.68061620254660227, -29.62692640763259888, -15.93463980944039982 ) ) ;
#34932 = CARTESIAN_POINT ( 'NONE',  ( 22.90112932213407149, -15.61618880384378905, -64.45281843961751633 ) ) ;
#34933 = CARTESIAN_POINT ( 'NONE',  ( 46.88182844640049751, -53.82794794302169805, -75.86076060431129520 ) ) ;
#34934 = CARTESIAN_POINT ( 'NONE',  ( 61.87076928723249836, 12.19882557268090117, -9.590776207249099627 ) ) ;
#34935 = EDGE_CURVE ( 'NONE', #24695, #24503, #24719, .T. ) ;
#34936 = CARTESIAN_POINT ( 'NONE',  ( 74.17629866868290378, -15.61618894467929941, -65.34607522167520699 ) ) ;
#34937 = ADVANCED_FACE ( 'NONE', ( #36792 ), #32955, .T. ) ;
#34938 = AXIS2_PLACEMENT_3D ( 'NONE', #47374, #39504, #11728 ) ;
#34939 = CARTESIAN_POINT ( 'NONE',  ( 59.76051743928839954, 13.88381115859199966, -25.97343284354310100 ) ) ;
#34940 = CARTESIAN_POINT ( 'NONE',  ( 22.96916380865210172, -11.00507187559370159, -35.31875724254479820 ) ) ;
#34941 = ORIENTED_EDGE ( 'NONE', *, *, #14592, .F. ) ;
#34942 = CARTESIAN_POINT ( 'NONE',  ( 56.31078303086230363, -46.45614404618829951, -26.30376438173910358 ) ) ;
#34943 = CARTESIAN_POINT ( 'NONE',  ( 2.219830629761540219, -55.78013387361319531, -9.977522010426989496 ) ) ;
#34944 = CARTESIAN_POINT ( 'NONE',  ( 76.18788946429619102, -8.449960703364579828, -12.23626020543570014 ) ) ;
#34945 = AXIS2_PLACEMENT_3D ( 'NONE', #164, #47867, #412 ) ;
#34946 = DIRECTION ( 'NONE',  ( 1.370459167135278883E-23, -1.000000000000000000, -3.054623595244970244E-12 ) ) ;
#34947 = DIRECTION ( 'NONE',  ( -0.5877852522924764678, 0.8090169943749450088, 0.000000000000000000 ) ) ;
#34948 = CARTESIAN_POINT ( 'NONE',  ( 12.98614995704589248, 18.60725077530888782, -82.44267625234913055 ) ) ;
#34949 = CARTESIAN_POINT ( 'NONE',  ( 47.18324198357279897, 23.57489020266570279, -54.61058319554400242 ) ) ;
#34950 = CARTESIAN_POINT ( 'NONE',  ( 57.24929578595760660, 21.38381105532069881, -74.14999999999999147 ) ) ;
#34951 = CARTESIAN_POINT ( 'NONE',  ( 57.33263043794990210, -50.46433321893989898, -53.14935904668140410 ) ) ;
#34952 = CARTESIAN_POINT ( 'NONE',  ( 41.38588548186360327, 12.78016087411839941, -3.641004086722789523 ) ) ;
#34954 = EDGE_CURVE ( 'NONE', #15334, #21823, #51052, .T. ) ;
#34953 = CYLINDRICAL_SURFACE ( 'NONE', #25872, 0.9999999999999988898 ) ;
#34955 = CARTESIAN_POINT ( 'NONE',  ( 22.90093739769620029, -15.61618894467913243, -28.45282021618999835 ) ) ;
#34956 = DIRECTION ( 'NONE',  ( 1.000000000000000000, 0.000000000000000000, 0.000000000000000000 ) ) ;
#34957 = DIRECTION ( 'NONE',  ( 1.000000000000000000, 0.000000000000000000, 0.000000000000000000 ) ) ;
#34958 = CARTESIAN_POINT ( 'NONE',  ( 68.13393739769658453, -28.80002732851960445, -29.09832030244560741 ) ) ;
#34959 = CARTESIAN_POINT ( 'NONE',  ( 17.78950558660029913, -52.11833314967490338, -75.86497326479759806 ) ) ;
#34960 = EDGE_CURVE ( 'NONE', #41914, #4949, #41354, .T. ) ;
#34961 = B_SPLINE_CURVE_WITH_KNOTS ( 'NONE', 3,
 ( #45288, #24825, #37673, #29787, #1775, #9129, #33727, #45546, #29033, #29287, #5709, #5463, #45808, #9641, #9895, #41604, #1519, #25851 ),
 .UNSPECIFIED., .F., .F.,
 ( 4, 2, 2, 2, 2, 2, 2, 2, 4 ),
 ( 0.4999997121946347378, 0.5624997481703053470, 0.6249997841459757897, 0.6874998201216464544, 0.7499998560973168971, 0.8124998920729877838, 0.8749999280486584485, 0.9374999640243293353, 1.000000000000000000 ),
 .UNSPECIFIED. ) ;
#34962 = CARTESIAN_POINT ( 'NONE',  ( 20.63393739769619017, -41.61618894467939356, -35.01561944896766221 ) ) ;
#34963 = CARTESIAN_POINT ( 'NONE',  ( 13.82979338249550061, -8.531161443281989776, -68.46725820821738751 ) ) ;
#34964 = CARTESIAN_POINT ( 'NONE',  ( 63.44472555293038596, 1.153605328059160051, -61.96710904643580164 ) ) ;
#34965 = EDGE_LOOP ( 'NONE', ( #8045, #36547, #40011, #49189, #13541, #5903 ) ) ;
#34966 = CARTESIAN_POINT ( 'NONE',  ( -5.732063824511490324, 16.49934840382849899, -7.265669357055710265 ) ) ;
#34967 = CARTESIAN_POINT ( 'NONE',  ( 61.36407574442370105, -45.58133505526990348, -47.65743212064420220 ) ) ;
#34968 = CARTESIAN_POINT ( 'NONE',  ( 73.23379646625190276, 0.8840451408750739093, -68.81103260973570457 ) ) ;
#34969 = CARTESIAN_POINT ( 'NONE',  ( 15.29511290902279974, -43.80059717415329601, -59.64999999999999147 ) ) ;
#34970 = DIRECTION ( 'NONE',  ( 0.000000000000000000, 0.000000000000000000, -1.000000000000000000 ) ) ;
#34971 = CARTESIAN_POINT ( 'NONE',  ( 40.74407843658939754, -45.29541405632470230, -5.682185392553109615 ) ) ;
#34972 = ORIENTED_EDGE ( 'NONE', *, *, #27181, .F. ) ;
#34973 = CARTESIAN_POINT ( 'NONE',  ( 17.40131324658650058, 21.55824172761710145, -76.12873484255680978 ) ) ;
#34974 = ORIENTED_EDGE ( 'NONE', *, *, #44946, .F. ) ;
#34975 = ORIENTED_EDGE ( 'NONE', *, *, #44250, .T. ) ;
#34976 = CARTESIAN_POINT ( 'NONE',  ( -13.36606260230359844, -50.61618894467959962, 16.85000000000000142 ) ) ;
#34977 = CARTESIAN_POINT ( 'NONE',  ( 11.13393739769619906, -55.30245861064819479, -43.74348518090240390 ) ) ;
#34978 = FACE_OUTER_BOUND ( 'NONE', #27567, .T. ) ;
#34979 = CONICAL_SURFACE ( 'NONE', #29915, 19.50000000000000000, 0.2449786631268651149 ) ;
#34980 = ORIENTED_EDGE ( 'NONE', *, *, #45330, .F. ) ;
#34981 = CARTESIAN_POINT ( 'NONE',  ( 15.09838326309694878, -7.705189749657031406, -52.96600322570992603 ) ) ;
#34982 = VERTEX_POINT ( 'NONE', #16895 ) ;
#34983 = CYLINDRICAL_SURFACE ( 'NONE', #6867, 1.500000000000001332 ) ;
#34984 = CARTESIAN_POINT ( 'NONE',  ( 16.13393739769620083, -15.61618894467929941, 17.07360679774999923 ) ) ;
#34985 = ORIENTED_EDGE ( 'NONE', *, *, #15848, .F. ) ;
#34986 = CARTESIAN_POINT ( 'NONE',  ( 44.97883126316192204, 2.004041975891398764, -38.63153946226272950 ) ) ;
#34987 = CARTESIAN_POINT ( 'NONE',  ( 51.40458829746259539, -50.54838093730629822, -76.23573209381319771 ) ) ;
#34988 = CARTESIAN_POINT ( 'NONE',  ( 60.47109295822400554, 14.43742118176249889, -47.34531703895609667 ) ) ;
#34989 = CARTESIAN_POINT ( 'NONE',  ( 22.90089492651413394, -15.59142452382446109, -40.45166006685596471 ) ) ;
#34990 = EDGE_CURVE ( 'NONE', #11477, #6439, #21019, .T. ) ;
#34991 = DIRECTION ( 'NONE',  ( -0.2260571801428161443, 0.000000000000000000, 0.9741140340359945027 ) ) ;
#34992 = DIRECTION ( 'NONE',  ( 0.4872913772396113563, 0.8732394366197181457, 0.000000000000000000 ) ) ;
#34993 = CARTESIAN_POINT ( 'NONE',  ( -5.416793657864619860, 16.04363467761240258, -5.522478245015279619 ) ) ;
#34994 = CARTESIAN_POINT ( 'NONE',  ( 0.9903310742090041252, -22.56644434022149781, -34.65032322548069743 ) ) ;
#34995 = DIRECTION ( 'NONE',  ( 0.000000000000000000, 1.000000000000000000, 0.000000000000000000 ) ) ;
#34996 = CARTESIAN_POINT ( 'NONE',  ( 18.92684706093190172, -8.282267497309700133, -54.90332710579859565 ) ) ;
#34997 = VERTEX_POINT ( 'NONE', #19841 ) ;
#34998 = B_SPLINE_CURVE_WITH_KNOTS ( 'NONE', 3,
 ( #33295, #33026, #4232, #49311, #48262, #13406, #28583, #24896, #48783, #44583 ),
 .UNSPECIFIED., .F., .F.,
 ( 4, 2, 2, 2, 4 ),
 ( -0.0003341005055044069861, 0.000000000000000000, 0.01143402714056380130, 0.02281319364104390096, 0.04082353370410345822 ),
 .UNSPECIFIED. ) ;
#34999 = CARTESIAN_POINT ( 'NONE',  ( 60.23130391297029718, 14.55066440145539985, -47.24246919202539630 ) ) ;
#35000 = CARTESIAN_POINT ( 'NONE',  ( 57.46868213755980292, 19.37940608379300045, -53.76542284059749477 ) ) ;
#35001 = CARTESIAN_POINT ( 'NONE',  ( 71.71886329086420631, 0.9254890127224509877, -70.46161719983020078 ) ) ;
#35002 = CARTESIAN_POINT ( 'NONE',  ( 45.56211211820503593, -40.06741977676035305, -59.08583076237255227 ) ) ;
#35003 = CARTESIAN_POINT ( 'NONE',  ( 15.72192118514110071, 19.65389280997749921, -20.20712476364060350 ) ) ;
#35004 = VECTOR ( 'NONE', #25952, 1000.000000000000000 ) ;
#35005 = FILL_AREA_STYLE_COLOUR ( '', #27296 ) ;
#35006 = CIRCLE ( 'NONE', #41717, 1.999999999999999112 ) ;
#35007 = CARTESIAN_POINT ( 'NONE',  ( 9.367379825797401693, -15.61607429561870042, -45.84717978380999881 ) ) ;
#35008 = CARTESIAN_POINT ( 'NONE',  ( 63.29941945011370308, 1.188860127980280179, -69.06196878611640955 ) ) ;
#35009 = CARTESIAN_POINT ( 'NONE',  ( 48.20668737594320419, -54.29411078304290328, -55.27999763446919701 ) ) ;
#35010 = CARTESIAN_POINT ( 'NONE',  ( -0.3347231778644786937, -63.30338805799588897, -50.60099389661421299 ) ) ;
#35011 = CARTESIAN_POINT ( 'NONE',  ( 56.51998432061879640, 19.51919619937510220, -53.72896419663989320 ) ) ;
#35012 = EDGE_CURVE ( 'NONE', #38406, #51314, #33780, .T. ) ;
#35013 = CARTESIAN_POINT ( 'NONE',  ( 56.61928439928507828, -45.32411236664518839, -31.98003398042899903 ) ) ;
#35014 = ORIENTED_EDGE ( 'NONE', *, *, #24854, .T. ) ;
#35015 = CARTESIAN_POINT ( 'NONE',  ( 11.97361496584299978, -21.54889764946979724, -31.76248681540709384 ) ) ;
#35016 = VERTEX_POINT ( 'NONE', #32575 ) ;
#35017 = CARTESIAN_POINT ( 'NONE',  ( 71.27608674571190761, 1.386446979194299933, -70.29126806847389730 ) ) ;
#35018 = CARTESIAN_POINT ( 'NONE',  ( 15.09847197271365182, -23.52719885739764294, -58.04933470294202635 ) ) ;
#35019 = CARTESIAN_POINT ( 'NONE',  ( -0.4410626023037880206, -3.737207156102679839, -35.14999999999999858 ) ) ;
#35020 = LINE ( 'NONE', #15125, #41982 ) ;
#35022 = CARTESIAN_POINT ( 'NONE',  ( 10.12791152504586378, 23.94333337502630243, -23.14397412734966508 ) ) ;
#35021 = FACE_OUTER_BOUND ( 'NONE', #3608, .T. ) ;
#35023 = CARTESIAN_POINT ( 'NONE',  ( 22.90115736359569354, -15.61618877121331295, -78.84717825834033533 ) ) ;
#35024 = CARTESIAN_POINT ( 'NONE',  ( 71.52074786344320501, 0.8966068345641470261, -70.60278586552519187 ) ) ;
#35025 = DIRECTION ( 'NONE',  ( -0.6561787149247867434, 0.000000000000000000, 0.7546055221635046273 ) ) ;
#35026 = ORIENTED_EDGE ( 'NONE', *, *, #45482, .T. ) ;
#35027 = DIRECTION ( 'NONE',  ( 0.000000000000000000, 0.000000000000000000, 1.000000000000000000 ) ) ;
#35028 = ORIENTED_EDGE ( 'NONE', *, *, #24807, .F. ) ;
#35029 = ORIENTED_EDGE ( 'NONE', *, *, #22235, .T. ) ;
#35030 = CARTESIAN_POINT ( 'NONE',  ( 16.13393739769620083, -15.61618894467929941, -28.45282021618999835 ) ) ;
#35031 = CARTESIAN_POINT ( 'NONE',  ( 20.99558919860562867, -9.290002765462324064, -39.50066101904910454 ) ) ;
#35032 = CARTESIAN_POINT ( 'NONE',  ( 76.47487835096482911, -26.73510161258535334, -13.11916531094834149 ) ) ;
#35033 = CARTESIAN_POINT ( 'NONE',  ( 9.628276464716538641, -64.27089026540051009, -46.77858652811859486 ) ) ;
#35034 = ORIENTED_EDGE ( 'NONE', *, *, #5385, .F. ) ;
#35035 = EDGE_LOOP ( 'NONE', ( #30148, #3218, #21093, #26866, #34626 ) ) ;
#35036 = CARTESIAN_POINT ( 'NONE',  ( 52.25041881653689302, 21.33925748481389917, -54.52050471625830141 ) ) ;
#35037 = B_SPLINE_CURVE_WITH_KNOTS ( 'NONE', 3,
 ( #22616, #18696, #3758, #3237, #23375, #11620, #27583, #47022, #35717, #43587 ),
 .UNSPECIFIED., .F., .F.,
 ( 4, 2, 2, 2, 4 ),
 ( 0.4999999271553960956, 0.5624999999993647304, 0.6624999999993823607, 0.8224999999994107025, 1.000000000000000000 ),
 .UNSPECIFIED. ) ;
#35038 = CARTESIAN_POINT ( 'NONE',  ( 82.13853704237929776, -45.11618894467940066, -46.37203261889099792 ) ) ;
#35039 = DIRECTION ( 'NONE',  ( 0.7071067811865457964, 0.7071067811865492381, 0.000000000000000000 ) ) ;
#35040 = CARTESIAN_POINT ( 'NONE',  ( 9.366668810525878186, -15.61604052661200015, -35.45282021618999835 ) ) ;
#35041 = CARTESIAN_POINT ( 'NONE',  ( 59.05492726919700175, -2.399412892946870102, -15.68836725989760161 ) ) ;
#35042 = CARTESIAN_POINT ( 'NONE',  ( 51.73941937002660296, -49.41743988675749222, -76.84325757996180073 ) ) ;
#35043 = CARTESIAN_POINT ( 'NONE',  ( 5.741632552282950108, -21.61618894467929763, -22.14999999999999858 ) ) ;
#35044 = ORIENTED_EDGE ( 'NONE', *, *, #5906, .T. ) ;
#35045 = CARTESIAN_POINT ( 'NONE',  ( 63.08005232011709751, 0.8859637708054499683, -68.88406027352149863 ) ) ;
#35046 = CARTESIAN_POINT ( 'NONE',  ( 20.99566233906968904, -21.94231674831827306, -48.08399959052492534 ) ) ;
#35047 = FACE_BOUND ( 'NONE', #31619, .T. ) ;
#35048 = CIRCLE ( 'NONE', #39215, 2.999999999999994227 ) ;
#35049 = CARTESIAN_POINT ( 'NONE',  ( 16.13393739769620083, -15.61618894467929941, 17.07360679774999923 ) ) ;
#35050 = AXIS2_PLACEMENT_3D ( 'NONE', #6059, #22017, #6320 ) ;
#35051 = CARTESIAN_POINT ( 'NONE',  ( 15.16589166249769960, -7.828401386832981146, -39.47312943893269477 ) ) ;
#35052 = CARTESIAN_POINT ( 'NONE',  ( 13.90103794227359835, -50.94889596342950000, -21.77365670817500032 ) ) ;
#35053 = ADVANCED_FACE ( 'NONE', ( #27701 ), #15403, .F. ) ;
#35054 = CARTESIAN_POINT ( 'NONE',  ( 0.5406133260286609676, 12.32747302715160131, -21.14999999999999858 ) ) ;
#35055 = CARTESIAN_POINT ( 'NONE',  ( 55.99298997062209793, 13.96345059265260069, -15.51995950838309923 ) ) ;
#35057 = EDGE_CURVE ( 'NONE', #14108, #16597, #49392, .T. ) ;
#35056 = CARTESIAN_POINT ( 'NONE',  ( 60.96779371467680164, -45.50112736404290104, -47.44752493507809987 ) ) ;
#35058 = EDGE_CURVE ( 'NONE', #9595, #25307, #28774, .T. ) ;
#35059 = CARTESIAN_POINT ( 'NONE',  ( 82.35517963119028195, 13.87593746180422905, -46.40109284526622702 ) ) ;
#35060 = CARTESIAN_POINT ( 'NONE',  ( 23.18341189490050169, -15.39831630363000059, -40.83734515755419636 ) ) ;
#35061 = CARTESIAN_POINT ( 'NONE',  ( 46.53772422082609950, -40.04183304982790048, -54.64305748561629628 ) ) ;
#35062 = EDGE_CURVE ( 'NONE', #15209, #47941, #427, .T. ) ;
#35063 = ORIENTED_EDGE ( 'NONE', *, *, #46272, .F. ) ;
#35064 = CARTESIAN_POINT ( 'NONE',  ( 14.21262892652819865, -51.28949470891959805, -74.96248001587449039 ) ) ;
#35065 = CARTESIAN_POINT ( 'NONE',  ( 64.92362553771700107, 1.265401080857980087, -60.77621068871049204 ) ) ;
#35066 = CARTESIAN_POINT ( 'NONE',  ( 44.42281161027170100, -46.09301635695339883, -8.582928211182331069 ) ) ;
#35067 = CARTESIAN_POINT ( 'NONE',  ( 11.71911513826172957, -64.93734084241999938, -23.86816772916239415 ) ) ;
#35068 = CARTESIAN_POINT ( 'NONE',  ( 23.83903744840162275, -13.54551243526225868, -47.42433642958721407 ) ) ;
#35069 = AXIS2_PLACEMENT_3D ( 'NONE', #8132, #258, #29065 ) ;
#35070 = DIRECTION ( 'NONE',  ( -0.6676418852213052979, 0.2329255526947255628, -0.7071067811865461294 ) ) ;
#35071 = CARTESIAN_POINT ( 'NONE',  ( 82.41473067501779326, 13.93846136199109864, -46.87530260006650451 ) ) ;
#35072 = CARTESIAN_POINT ( 'NONE',  ( 16.42857207933229091, -7.682041846050376321, -65.01956441179268609 ) ) ;
#35074 = CARTESIAN_POINT ( 'NONE',  ( 46.66163704272000246, -38.09001934925220212, -56.99730829862610193 ) ) ;
#35073 = CARTESIAN_POINT ( 'NONE',  ( 47.53482541495846903, 23.16677570558394095, -74.95177797945758869 ) ) ;
#35075 = PLANE ( 'NONE',  #29367 ) ;
#35076 = EDGE_CURVE ( 'NONE', #14944, #17025, #19613, .T. ) ;
#35077 = DIRECTION ( 'NONE',  ( 1.000000000000000000, 0.000000000000000000, 0.000000000000000000 ) ) ;
#35078 = VERTEX_POINT ( 'NONE', #37061 ) ;
#35079 = AXIS2_PLACEMENT_3D ( 'NONE', #20408, #12838, #20667 ) ;
#35080 = CARTESIAN_POINT ( 'NONE',  ( 53.49062365247959860, -49.35044025281749924, -48.99764540719809958 ) ) ;
#35081 = ORIENTED_EDGE ( 'NONE', *, *, #14477, .T. ) ;
#35082 = AXIS2_PLACEMENT_3D ( 'NONE', #39336, #38565, #3438 ) ;
#35083 = CARTESIAN_POINT ( 'NONE',  ( 45.28026775681226468, 6.614598366022641507, -63.87362864251259964 ) ) ;
#35084 = CARTESIAN_POINT ( 'NONE',  ( 20.11812049527873825, -22.52868116577465685, -74.12566484944238709 ) ) ;
#35085 = CARTESIAN_POINT ( 'NONE',  ( 14.04300386716560034, 19.71129266594920182, -21.72002249118050088 ) ) ;
#35086 = CARTESIAN_POINT ( 'NONE',  ( 52.23706462883279755, -49.75889276274740070, -77.18591504236948708 ) ) ;
#35087 = AXIS2_PLACEMENT_3D ( 'NONE', #5450, #1765, #41336 ) ;
#35088 = CARTESIAN_POINT ( 'NONE',  ( 19.53847090439890266, -9.439481869030970529, -52.11317062803219358 ) ) ;
#35089 = CIRCLE ( 'NONE', #38472, 0.5000000000000000000 ) ;
#35090 = CARTESIAN_POINT ( 'NONE',  ( 52.71531171373420221, 18.50951998324639902, -48.72995709875519310 ) ) ;
#35091 = CARTESIAN_POINT ( 'NONE',  ( 55.63792462483650070, -45.97095330521690215, -16.89987564799369935 ) ) ;
#35092 = CARTESIAN_POINT ( 'NONE',  ( 16.13393739769620083, -15.61618894467929941, -54.64999999999999858 ) ) ;
#35093 = EDGE_LOOP ( 'NONE', ( #35998, #9026, #37352, #35251, #2158, #27630, #38730, #6701, #45953, #27086, #44944, #18162, #38826, #31848 ) ) ;
#35094 = AXIS2_PLACEMENT_3D ( 'NONE', #552, #36193, #5283 ) ;
#35095 = CARTESIAN_POINT ( 'NONE',  ( 22.07392413299059797, -20.74486286528630075, -33.51421571862140070 ) ) ;
#35096 = ORIENTED_EDGE ( 'NONE', *, *, #12958, .T. ) ;
#35097 = CARTESIAN_POINT ( 'NONE',  ( 16.13393739769620083, -15.61618894467929941, -32.14999999999999858 ) ) ;
#35098 = CARTESIAN_POINT ( 'NONE',  ( 8.839329446722729244, 32.18893842050779597, -46.67772192990729252 ) ) ;
#35099 = CARTESIAN_POINT ( 'NONE',  ( 72.78175560864708871, 1.385702546077169917, -62.52592200326169092 ) ) ;
#35100 = DIRECTION ( 'NONE',  ( 0.000000000000000000, 0.000000000000000000, -1.000000000000000000 ) ) ;
#35101 = B_SPLINE_CURVE_WITH_KNOTS ( 'NONE', 3,
 ( #7308, #23259, #4138, #43974, #4917, #16983, #35851, #12268 ),
 .UNSPECIFIED., .F., .F.,
 ( 4, 2, 2, 4 ),
 ( 0.1514974462201259253, 0.1570050336056500184, 0.1722850272388009862, 0.1726615410485390079 ),
 .UNSPECIFIED. ) ;
#35102 = CARTESIAN_POINT ( 'NONE',  ( 53.16274104891702024, -49.55751115293774234, -49.15255090718006414 ) ) ;
#35103 = LINE ( 'NONE', #17014, #9926 ) ;
#35104 = EDGE_CURVE ( 'NONE', #25175, #8004, #1158, .T. ) ;
#35105 = CARTESIAN_POINT ( 'NONE',  ( 50.43862210052599693, -53.32183726795299350, -54.57790968970819989 ) ) ;
#35106 = ORIENTED_EDGE ( 'NONE', *, *, #620, .T. ) ;
#35107 = DIRECTION ( 'NONE',  ( 0.000000000000000000, -1.000000000000000000, 0.000000000000000000 ) ) ;
#35108 = CARTESIAN_POINT ( 'NONE',  ( 10.13445450645889956, -63.11543068638779630, -45.99826666626069738 ) ) ;
#35109 = CARTESIAN_POINT ( 'NONE',  ( 68.13393739769769297, 18.72622661238300168, -73.39853292320978539 ) ) ;
#35110 = ORIENTED_EDGE ( 'NONE', *, *, #28969, .F. ) ;
#35111 = CARTESIAN_POINT ( 'NONE',  ( 51.17464648325179155, -31.65168256193422280, -17.11447666815010749 ) ) ;
#35112 = CARTESIAN_POINT ( 'NONE',  ( 57.26283657379340042, 19.38381106601499937, -53.75815476539330007 ) ) ;
#35113 = CARTESIAN_POINT ( 'NONE',  ( 10.70077573641860447, -9.799726819224163776, -48.76866075350059049 ) ) ;
#35114 = ORIENTED_EDGE ( 'NONE', *, *, #13488, .T. ) ;
#35115 = CARTESIAN_POINT ( 'NONE',  ( 9.496404732828242601, -64.31007825828744728, -46.84592557098148546 ) ) ;
#35116 = DIRECTION ( 'NONE',  ( -1.000000000000000000, 0.000000000000000000, 0.000000000000000000 ) ) ;
#35117 = CARTESIAN_POINT ( 'NONE',  ( 22.90065884458136480, -15.61618680935524317, -64.84717769963093303 ) ) ;
#35118 = FACE_OUTER_BOUND ( 'NONE', #13090, .T. ) ;
#35119 = CARTESIAN_POINT ( 'NONE',  ( 23.59510982153750192, -12.10711127132339904, -63.65239730387659023 ) ) ;
#35120 = CARTESIAN_POINT ( 'NONE',  ( 36.43069203082960428, -15.61618894467929941, 7.530187386896120216 ) ) ;
#35121 = FACE_OUTER_BOUND ( 'NONE', #28596, .T. ) ;
#35122 = EDGE_LOOP ( 'NONE', ( #8508, #13791, #31256, #18228 ) ) ;
#35123 = EDGE_LOOP ( 'NONE', ( #3825, #5460, #13991, #13282 ) ) ;
#35124 = CIRCLE ( 'NONE', #43523, 4.649999999999999467 ) ;
#35125 = VECTOR ( 'NONE', #16973, 1000.000000000000000 ) ;
#35126 = CARTESIAN_POINT ( 'NONE',  ( 43.91474985106849971, -43.54612994170620510, -5.093415854460159764 ) ) ;
#35127 = CARTESIAN_POINT ( 'NONE',  ( 14.36753390939369979, -8.378336188394568396, -59.65646296961590167 ) ) ;
#35128 = VECTOR ( 'NONE', #42657, 1000.000000000000000 ) ;
#35129 = CARTESIAN_POINT ( 'NONE',  ( 55.40394000045360201, 13.88381105524500114, -14.52023566624100148 ) ) ;
#35130 = AXIS2_PLACEMENT_3D ( 'NONE', #10557, #42008, #50641 ) ;
#35131 = CARTESIAN_POINT ( 'NONE',  ( 12.09004633843789911, -22.35834692618010067, -32.14999999999999858 ) ) ;
#35132 = EDGE_CURVE ( 'NONE', #16605, #22390, #45452, .T. ) ;
#35133 = DIRECTION ( 'NONE',  ( -0.4096086573010331855, 0.9122613374817791776, 0.000000000000000000 ) ) ;
#35134 = AXIS2_PLACEMENT_3D ( 'NONE', #8432, #24378, #12623 ) ;
#35135 = CARTESIAN_POINT ( 'NONE',  ( 45.64758691443690708, -45.19790785473080064, -8.164367006753829870 ) ) ;
#35136 = CYLINDRICAL_SURFACE ( 'NONE', #1293, 1.500000000000001332 ) ;
#35137 = CARTESIAN_POINT ( 'NONE',  ( 12.16812838080560155, 33.44776901404870273, -15.91929859868259811 ) ) ;
#35138 = CARTESIAN_POINT ( 'NONE',  ( 16.43585171025809899, -23.85582294485470101, -63.99601028757499677 ) ) ;
#35139 = CARTESIAN_POINT ( 'NONE',  ( 22.37881013509309724, -19.99905837446409862, -32.14999999999999858 ) ) ;
#35140 = CARTESIAN_POINT ( 'NONE',  ( 56.46720558104399856, -50.68772439539020525, -74.89154223783529574 ) ) ;
#35142 = CARTESIAN_POINT ( 'NONE',  ( 10.71234811426425715, -55.24696076757936680, -45.27932796213227107 ) ) ;
#35141 = CARTESIAN_POINT ( 'NONE',  ( 0.6014665695674989987, 22.53381255785799908, -8.430871960909678720 ) ) ;
#35143 = CARTESIAN_POINT ( 'NONE',  ( 47.65526630185220114, -54.48436720726729732, -54.69071458794790175 ) ) ;
#35144 = B_SPLINE_CURVE_WITH_KNOTS ( 'NONE', 3,
 ( #15476, #27771, #31941, #47963 ),
 .UNSPECIFIED., .F., .F.,
 ( 4, 4 ),
 ( 0.000000000000000000, 1.000000000000000000 ),
 .UNSPECIFIED. ) ;
#35145 = EDGE_CURVE ( 'NONE', #25228, #22140, #8741, .T. ) ;
#35146 = DIRECTION ( 'NONE',  ( 0.000000000000000000, 1.000000000000000000, 0.000000000000000000 ) ) ;
#35147 = ORIENTED_EDGE ( 'NONE', *, *, #5685, .F. ) ;
#35148 = CARTESIAN_POINT ( 'NONE',  ( -7.471208905905950104, -45.39622512213500016, -4.913224497761048859 ) ) ;
#35149 = CARTESIAN_POINT ( 'NONE',  ( 47.51738683343549496, 23.35989739960990264, -54.96699491834060325 ) ) ;
#35150 = CARTESIAN_POINT ( 'NONE',  ( 17.87699378894365054, -7.880242123305163382, -65.36294250950261642 ) ) ;
#35151 = DIRECTION ( 'NONE',  ( 0.000000000000000000, 0.000000000000000000, -1.000000000000000000 ) ) ;
#35152 = CARTESIAN_POINT ( 'NONE',  ( 65.27736602627911111, 1.383811055320669947, -60.94999999999999574 ) ) ;
#35153 = CARTESIAN_POINT ( 'NONE',  ( 20.92049246423509601, -21.32544322209390231, -78.51056856275720008 ) ) ;
#35154 = CARTESIAN_POINT ( 'NONE',  ( 51.70526340020489897, 18.12584497879259615, -76.83585703765098174 ) ) ;
#35155 = CARTESIAN_POINT ( 'NONE',  ( 52.85165463198989499, 18.41706942343310160, -48.64955370223109554 ) ) ;
#35156 = DIRECTION ( 'NONE',  ( 0.000000000000000000, 0.000000000000000000, -1.000000000000000000 ) ) ;
#35157 = CARTESIAN_POINT ( 'NONE',  ( 52.84340795157500281, -49.65376797971740075, -48.59551871909959431 ) ) ;
#35158 = CARTESIAN_POINT ( 'NONE',  ( 53.62726140758459792, 17.64839027132520144, -27.04628291361679970 ) ) ;
#35159 = CARTESIAN_POINT ( 'NONE',  ( 49.85715601738330349, 22.13586533569470305, -54.14711712984389891 ) ) ;
#35160 = VECTOR ( 'NONE', #30790, 1000.000000000000000 ) ;
#35161 = CARTESIAN_POINT ( 'NONE',  ( 52.82975622904280755, -49.66092049964720445, -28.15000000000000213 ) ) ;
#35162 = CIRCLE ( 'NONE', #23434, 1.400000000000000133 ) ;
#35163 = DIRECTION ( 'NONE',  ( -0.000000000000000000, 1.000000000000000000, 0.000000000000000000 ) ) ;
#35164 = CARTESIAN_POINT ( 'NONE',  ( 62.10661619914199605, -31.21746242632069723, -16.71838601031609883 ) ) ;
#35165 = CARTESIAN_POINT ( 'NONE',  ( 71.12477309692330607, 1.336371993404959824, -60.77157093307350522 ) ) ;
#35166 = CARTESIAN_POINT ( 'NONE',  ( 11.13393739769619906, 32.13057954558899354, -43.91801182705599871 ) ) ;
#35167 = CARTESIAN_POINT ( 'NONE',  ( 72.42914715746668719, 1.346167254499869959, -61.62073875063699546 ) ) ;
#35168 = CIRCLE ( 'NONE', #46069, 9.703299832284479010 ) ;
#35169 = EDGE_CURVE ( 'NONE', #4288, #41372, #9809, .T. ) ;
#35170 = AXIS2_PLACEMENT_3D ( 'NONE', #1976, #33923, #22905 ) ;
#35171 = CARTESIAN_POINT ( 'NONE',  ( 22.90119541241246637, -15.61618911972255930, -40.84718082130915207 ) ) ;
#35172 = CARTESIAN_POINT ( 'NONE',  ( 19.31348261253770460, -9.577361911703928143, -66.10735234099374225 ) ) ;
#35173 = ORIENTED_EDGE ( 'NONE', *, *, #46268, .T. ) ;
#35174 = ADVANCED_FACE ( 'NONE', ( #5363 ), #17934, .T. ) ;
#35175 = EDGE_LOOP ( 'NONE', ( #50854, #25293, #1475, #41212 ) ) ;
#35176 = CARTESIAN_POINT ( 'NONE',  ( 52.26504646883520167, 18.55116755685089913, -77.19463087837650050 ) ) ;
#35177 = CARTESIAN_POINT ( 'NONE',  ( 50.12347980195983155, -30.03964280096379014, -16.03354426139003053 ) ) ;
#35178 = VERTEX_POINT ( 'NONE', #9553 ) ;
#35179 = CARTESIAN_POINT ( 'NONE',  ( 57.59044435501339620, -45.13211036767589945, -25.55064646906290449 ) ) ;
#35180 = CARTESIAN_POINT ( 'NONE',  ( 8.428814911140731780, -17.68678876403731692, -78.42431588342377324 ) ) ;
#35181 = EDGE_CURVE ( 'NONE', #28327, #42929, #7921, .T. ) ;
#35182 = DIRECTION ( 'NONE',  ( 0.000000000000000000, 0.000000000000000000, -1.000000000000000000 ) ) ;
#35183 = EDGE_LOOP ( 'NONE', ( #10803, #38407, #24753 ) ) ;
#35184 = CARTESIAN_POINT ( 'NONE',  ( 16.38388870865558289, -22.42468798131612928, -80.94130156388325759 ) ) ;
#35185 = CARTESIAN_POINT ( 'NONE',  ( 43.20094691158656985, 6.574965196572723158, -74.31491011093504540 ) ) ;
#35186 = CARTESIAN_POINT ( 'NONE',  ( 42.44161405036800261, -44.94940367324450392, -5.942266020708489194 ) ) ;
#35187 = ORIENTED_EDGE ( 'NONE', *, *, #6662, .T. ) ;
#35188 = CARTESIAN_POINT ( 'NONE',  ( 50.64365103613339869, -45.11618894467940066, -10.74058096682459862 ) ) ;
#35189 = CARTESIAN_POINT ( 'NONE',  ( 51.30165130492172665, 0.6175616045832953427, -17.32271293053486616 ) ) ;
#35190 = DIRECTION ( 'NONE',  ( 0.000000000000000000, 0.9319748226751467524, 0.3625230060280709155 ) ) ;
#35191 = AXIS2_PLACEMENT_3D ( 'NONE', #14320, #13559, #46308 ) ;
#35192 = CARTESIAN_POINT ( 'NONE',  ( 65.46635429658410033, -29.90696431587659987, -16.55440410732879997 ) ) ;
#35193 = ADVANCED_FACE ( 'NONE', ( #23371 ), #23125, .F. ) ;
#35194 = CARTESIAN_POINT ( 'NONE',  ( 10.72262724756561880, -11.45750590540933800, -63.66115401167630949 ) ) ;
#35195 = CARTESIAN_POINT ( 'NONE',  ( 47.13234217445310748, -54.53038550896650349, -75.11917674890220553 ) ) ;
#35196 = CARTESIAN_POINT ( 'NONE',  ( 21.54528678323437063, -19.77482129041136005, -36.66115137938106727 ) ) ;
#35197 = CARTESIAN_POINT ( 'NONE',  ( 40.92025707381650079, 14.03914583310360165, -5.766237210609819641 ) ) ;
#35198 = EDGE_CURVE ( 'NONE', #18843, #16350, #2719, .T. ) ;
#35199 = FACE_OUTER_BOUND ( 'NONE', #25233, .T. ) ;
#35200 = TOROIDAL_SURFACE ( 'NONE', #41858, 17.39999999955150045, 3.400000000022779911 ) ;
#35201 = AXIS2_PLACEMENT_3D ( 'NONE', #49186, #45504, #13281 ) ;
#35202 = CARTESIAN_POINT ( 'NONE',  ( 83.86651039750330483, -44.39461367728179653, -46.90523421348220268 ) ) ;
#35203 = CARTESIAN_POINT ( 'NONE',  ( 61.72362489370979688, 13.88380460837380070, -28.08315270507459971 ) ) ;
#35204 = AXIS2_PLACEMENT_3D ( 'NONE', #50289, #2321, #14376 ) ;
#35205 = CARTESIAN_POINT ( 'NONE',  ( 22.37474952699549746, -21.00460003670480091, -33.73437862127239839 ) ) ;
#35206 = B_SPLINE_SURFACE_WITH_KNOTS ( 'NONE', 3, 3, ( 
 ( #13499, #37330, #8253, #40480, #4319, #24202, #20286, #41258, #40741, #9037, #28933, #13241, #32582, #21324, #17165, #25255 ),
 ( #4842, #8520, #33115, #12981, #36539, #9311, #21069, #32846, #5117, #29454, #29191, #45196, #5370, #44938, #37071, #20809 ),
 ( #1430, #645, #24985, #17414, #36279, #40230, #24727, #33383, #49398, #387, #16373, #32330, #48350, #12444, #28411, #48878 ),
 ( #44418, #24466, #4571, #20543, #12716, #48616, #28670, #44673, #36799, #909, #16904, #39339, #47215, #14002, #46962, #41517 ),
 ( #21581, #33643, #2207, #11303, #9559, #11044, #25511, #19151, #5634, #45979, #49660, #14965, #7116, #43020, #17674, #35129 ),
 ( #15488, #30932, #35393, #37580, #29704, #3180, #27014, #1686, #10070, #23068, #25770, #50163, #18184, #45717, #13750, #51136 ) ),
 .UNSPECIFIED., .F., .F., .F.,
 ( 4, 1, 1, 4 ),
 ( 4, 2, 2, 2, 2, 2, 2, 4 ),
 ( -7.682816665999999629E-06, 0.3333333333333329818, 0.6666666666666670737, 1.000000000266519917 ),
 ( -7.682816665999999629E-06, 2.041349754395100025, 4.374320902275210088, 5.832427869700279821, 6.561481353412809803, 7.727966927352870385, 9.594343845656959857, 11.66486342221729977 ),
 .UNSPECIFIED. ) ;
#35207 = EDGE_LOOP ( 'NONE', ( #18223, #18737, #42605, #40713, #49585, #35514 ) ) ;
#35208 = CARTESIAN_POINT ( 'NONE',  ( 52.82976017067200303, -49.66091843452839782, -28.09469381563379997 ) ) ;
#35209 = CARTESIAN_POINT ( 'NONE',  ( -5.594544317113800069, -47.37070709791210277, -5.716103250782650136 ) ) ;
#35210 = CARTESIAN_POINT ( 'NONE',  ( 76.64846024278141101, 4.391811825665690172, -13.86716462664029947 ) ) ;
#35211 = CARTESIAN_POINT ( 'NONE',  ( 74.97543536360356597, 13.88380951271968478, -15.15463076919403385 ) ) ;
#35212 = CARTESIAN_POINT ( 'NONE',  ( 2.404741263826640107, -5.380232784273969671, -35.14999999999999858 ) ) ;
#35213 = DIRECTION ( 'NONE',  ( 0.000000000000000000, 0.000000000000000000, 1.000000000000000000 ) ) ;
#35214 = CARTESIAN_POINT ( 'NONE',  ( 47.21820949846080140, 23.54718703541459845, -54.61573492153319620 ) ) ;
#35215 = CARTESIAN_POINT ( 'NONE',  ( 82.28938588685190325, -45.22603122459570102, -47.03253084601389844 ) ) ;
#35216 = CARTESIAN_POINT ( 'NONE',  ( 57.41310621417500215, -50.45968287620319614, -53.14417655181500066 ) ) ;
#35217 = CARTESIAN_POINT ( 'NONE',  ( 40.90236900589889757, 13.45839943238190095, -4.970360716545739521 ) ) ;
#35218 = DIRECTION ( 'NONE',  ( 0.000000000000000000, 0.000000000000000000, -1.000000000000000000 ) ) ;
#35219 = CARTESIAN_POINT ( 'NONE',  ( 16.13393739769599833, 14.38381105532070059, -49.33749999999999858 ) ) ;
#35220 = CARTESIAN_POINT ( 'NONE',  ( 55.10584483452489479, -48.49282765683750540, -48.53157258127289708 ) ) ;
#35221 = CARTESIAN_POINT ( 'NONE',  ( 68.13393739769649926, -48.11618894467230234, -75.95000000000109708 ) ) ;
#35222 = CARTESIAN_POINT ( 'NONE',  ( 68.39016279111210395, -1.116426826981149922, -18.15415026710280344 ) ) ;
#35223 = CARTESIAN_POINT ( 'NONE',  ( 17.96588596253970138, -52.24360429457480137, -75.86497326479759806 ) ) ;
#35224 = CARTESIAN_POINT ( 'NONE',  ( 49.80812477255949489, -53.32727295909180043, -54.05131971329959839 ) ) ;
#35225 = CARTESIAN_POINT ( 'NONE',  ( 22.09038143216230310, -11.14098293795579941, -60.86224082610989683 ) ) ;
#35226 = CARTESIAN_POINT ( 'NONE',  ( 20.11809238705456693, -8.703679916704407660, -77.45899608327597718 ) ) ;
#35227 = CARTESIAN_POINT ( 'NONE',  ( 63.27581436415109550, 1.132579237369250036, -62.21177178793440277 ) ) ;
#35228 = ORIENTED_EDGE ( 'NONE', *, *, #13626, .F. ) ;
#35229 = DIRECTION ( 'NONE',  ( 0.000000000000000000, 0.9319748226751467524, 0.3625230060280709155 ) ) ;
#35230 = PLANE ( 'NONE',  #40185 ) ;
#35231 = CARTESIAN_POINT ( 'NONE',  ( 72.80030139158668590, 1.384887413063060180, -68.61455525072810246 ) ) ;
#35232 = CARTESIAN_POINT ( 'NONE',  ( 46.11714933639719760, 8.867842174310458958, -56.39015576205443381 ) ) ;
#35233 = CARTESIAN_POINT ( 'NONE',  ( 9.754056310848479683, -11.79350258725770040, -81.23899999999999011 ) ) ;
#35234 = CARTESIAN_POINT ( 'NONE',  ( 42.70758233787309877, -45.85587203478289808, -7.311889205965530714 ) ) ;
#35235 = VERTEX_POINT ( 'NONE', #3496 ) ;
#35236 = CARTESIAN_POINT ( 'NONE',  ( 17.21347160910339724, 21.88381105532300097, -76.14999999999999147 ) ) ;
#35237 = ORIENTED_EDGE ( 'NONE', *, *, #26436, .T. ) ;
#35238 = ADVANCED_FACE ( 'NONE', ( #42560 ), #42230, .F. ) ;
#35239 = VERTEX_POINT ( 'NONE', #30477 ) ;
#35240 = EDGE_LOOP ( 'NONE', ( #34392, #45082, #49578, #48590 ) ) ;
#35241 = DIRECTION ( 'NONE',  ( -6.128874000000000406E-13, 6.301142999999999861E-13, 1.000000000000000000 ) ) ;
#35242 = CARTESIAN_POINT ( 'NONE',  ( 22.36170331077510198, -10.91435426618479987, -81.23899999999999011 ) ) ;
#35243 = EDGE_CURVE ( 'NONE', #1811, #42352, #17127, .T. ) ;
#35244 = PRODUCT_DEFINITION_FORMATION_WITH_SPECIFIED_SOURCE ( 'ANY', '', #21513, .NOT_KNOWN. ) ;
#35245 = CIRCLE ( 'NONE', #12654, 0.4999999999999982236 ) ;
#35246 = CARTESIAN_POINT ( 'NONE',  ( 16.13393739769620083, -15.61618894467929941, 6.850000000000000533 ) ) ;
#35247 = AXIS2_PLACEMENT_3D ( 'NONE', #43575, #35706, #20215 ) ;
#35248 = ORIENTED_EDGE ( 'NONE', *, *, #6203, .F. ) ;
#35249 = AXIS2_PLACEMENT_3D ( 'NONE', #22015, #33814, #49828 ) ;
#35250 = CARTESIAN_POINT ( 'NONE',  ( 20.99561365428662896, -9.290022285047772499, -53.21600398968095647 ) ) ;
#35251 = ORIENTED_EDGE ( 'NONE', *, *, #14250, .T. ) ;
#35252 = CARTESIAN_POINT ( 'NONE',  ( 56.81354083976449942, -51.38126045871209868, -54.61518503260169410 ) ) ;
#35253 = DIRECTION ( 'NONE',  ( 0.000000000000000000, 0.000000000000000000, -1.000000000000000000 ) ) ;
#35254 = B_SPLINE_CURVE_WITH_KNOTS ( 'NONE', 3,
 ( #8827, #12763, #24255, #435, #47887, #35824, #957, #32120, #16954, #43948, #16422, #32639, #39761 ),
 .UNSPECIFIED., .F., .F.,
 ( 4, 2, 2, 1, 2, 2, 4 ),
 ( 0.000000000000000000, 0.2500000000000033307, 0.3750000000000147660, 0.4375000000000204836, 0.4687500000000233702, 0.5000000000000262013, 1.000000000000000000 ),
 .UNSPECIFIED. ) ;
#35255 = ORIENTED_EDGE ( 'NONE', *, *, #4200, .F. ) ;
#35256 = CARTESIAN_POINT ( 'NONE',  ( 64.93393739769619799, 1.530257664727401767, -69.99644660940670349 ) ) ;
#35257 = CARTESIAN_POINT ( 'NONE',  ( 53.38272228983590395, -51.31658076067470375, -75.68264719383489592 ) ) ;
#35258 = CARTESIAN_POINT ( 'NONE',  ( 60.87207086065609474, 14.42513991272290141, -47.67718664521559901 ) ) ;
#35259 = EDGE_CURVE ( 'NONE', #44094, #25374, #28809, .T. ) ;
#35260 = CYLINDRICAL_SURFACE ( 'NONE', #23003, 6.766999999999998572 ) ;
#35261 = EDGE_CURVE ( 'NONE', #33306, #23870, #46498, .T. ) ;
#35262 = CARTESIAN_POINT ( 'NONE',  ( 40.64814218619559938, -44.65225711300990241, -4.018323718197319927 ) ) ;
#35263 = CARTESIAN_POINT ( 'NONE',  ( -6.149347183000639205, 15.38699437488089927, -5.438307061430879052 ) ) ;
#35264 = CARTESIAN_POINT ( 'NONE',  ( 46.64446957347233536, 22.34959160277791668, -76.02856692476716205 ) ) ;
#35265 = CARTESIAN_POINT ( 'NONE',  ( 21.16241148139313921, -20.56159161423454051, -39.09452867415468802 ) ) ;
#35266 = CARTESIAN_POINT ( 'NONE',  ( 23.68405699770680073, -13.47552498022369960, -49.19956406921799186 ) ) ;
#35267 = ORIENTED_EDGE ( 'NONE', *, *, #23382, .T. ) ;
#35268 = FACE_OUTER_BOUND ( 'NONE', #15620, .T. ) ;
#35269 = CARTESIAN_POINT ( 'NONE',  ( 44.59670004653540332, 14.86796560598379990, -8.701614582662479336 ) ) ;
#35270 = CARTESIAN_POINT ( 'NONE',  ( 71.49710702210251156, 1.370387345317799932, -70.28519118483690420 ) ) ;
#35271 = CARTESIAN_POINT ( 'NONE',  ( 45.79170134131306469, -40.08162185648630782, -57.97045409603698829 ) ) ;
#35272 = CARTESIAN_POINT ( 'NONE',  ( 14.40169973178839946, 19.62547192528419870, -21.38758215360849846 ) ) ;
#35273 = TOROIDAL_SURFACE ( 'NONE', #10185, 25.00000000000000000, 1.000000000000000000 ) ;
#35274 = AXIS2_PLACEMENT_3D ( 'NONE', #4458, #20428, #32726 ) ;
#35275 = CIRCLE ( 'NONE', #47857, 16.00000000000000000 ) ;
#35276 = CARTESIAN_POINT ( 'NONE',  ( 20.83141696938240273, -20.87701063411540048, -45.11516743498959414 ) ) ;
#35277 = FACE_OUTER_BOUND ( 'NONE', #1543, .T. ) ;
#35278 = CARTESIAN_POINT ( 'NONE',  ( 48.73759501478280498, -54.04467100006880287, -55.00375600211459926 ) ) ;
#35279 = CARTESIAN_POINT ( 'NONE',  ( -33.86606260230205123, -20.49712430492939319, -57.75434594776565689 ) ) ;
#35280 = CARTESIAN_POINT ( 'NONE',  ( 64.60839616882741154, 0.9151442779661310700, -70.50513874227569033 ) ) ;
#35281 = CARTESIAN_POINT ( 'NONE',  ( 23.04647360858802330, -19.60029606439469774, -37.67433763517301770 ) ) ;
#35282 = CARTESIAN_POINT ( 'NONE',  ( 14.06320080711358855, -7.911103808508573643, -71.20898408184140749 ) ) ;
#35283 = ORIENTED_EDGE ( 'NONE', *, *, #20863, .T. ) ;
#35284 = CARTESIAN_POINT ( 'NONE',  ( 19.68346084944639784, -21.71073103174810015, -79.17930779234599470 ) ) ;
#35285 = ORIENTED_EDGE ( 'NONE', *, *, #18392, .F. ) ;
#35286 = CARTESIAN_POINT ( 'NONE',  ( 71.48076113803239195, 1.264121749638649872, -70.45005197993600632 ) ) ;
#35287 = CARTESIAN_POINT ( 'NONE',  ( 3.633937397696210159, -8.399310579809009525, -34.64999999999999858 ) ) ;
#35288 = CARTESIAN_POINT ( 'NONE',  ( 61.12977893007705177, 14.02110085376754256, -27.62651976406664645 ) ) ;
#35289 = CARTESIAN_POINT ( 'NONE',  ( 7.433595052712601792, 30.13535813643414585, -19.83583517853763922 ) ) ;
#35291 = CARTESIAN_POINT ( 'NONE',  ( 11.13393739769619906, -15.61618894467929941, -21.14999999999999858 ) ) ;
#35290 = DIRECTION ( 'NONE',  ( 0.000000000000000000, -0.7071067811865466846, -0.7071067811865483499 ) ) ;
#35292 = CARTESIAN_POINT ( 'NONE',  ( -0.1826151910073069984, -10.64742273529058636, -34.92526559962323063 ) ) ;
#35293 = CARTESIAN_POINT ( 'NONE',  ( 8.428886018646599254, -13.54533248524384881, -66.87566464129990607 ) ) ;
#35294 = DIRECTION ( 'NONE',  ( 0.000000000000000000, -1.000000000000000000, 0.000000000000000000 ) ) ;
#35295 = ORIENTED_EDGE ( 'NONE', *, *, #36134, .T. ) ;
#35296 = CARTESIAN_POINT ( 'NONE',  ( 84.32823919854369876, -43.96175172734450598, -47.43652016892809797 ) ) ;
#35297 = ORIENTED_EDGE ( 'NONE', *, *, #42745, .T. ) ;
#35298 = ADVANCED_FACE ( 'NONE', ( #22866 ), #43059, .F. ) ;
#35299 = EDGE_LOOP ( 'NONE', ( #30547, #4826, #48052 ) ) ;
#35300 = CARTESIAN_POINT ( 'NONE',  ( 22.90092760148217010, -15.98535187056947926, -58.86453566420338035 ) ) ;
#35301 = DIRECTION ( 'NONE',  ( 1.000000000000000000, 0.000000000000000000, 0.000000000000000000 ) ) ;
#35302 = CARTESIAN_POINT ( 'NONE',  ( 76.42858925763616185, -23.05672696190767823, -12.91970068794330473 ) ) ;
#35303 = CARTESIAN_POINT ( 'NONE',  ( 11.41669899830660029, -65.09235379784719555, -46.91455955995500204 ) ) ;
#35304 = VERTEX_POINT ( 'NONE', #27324 ) ;
#35305 = EDGE_LOOP ( 'NONE', ( #43970, #7670, #8697, #44658 ) ) ;
#35306 = CARTESIAN_POINT ( 'NONE',  ( 24.01953169521327425, -16.26277958825795977, -55.53370651648724987 ) ) ;
#35307 = CARTESIAN_POINT ( 'NONE',  ( 31.79224979287389985, 4.883811055320679273, -84.65000000000000568 ) ) ;
#35308 = DIRECTION ( 'NONE',  ( 0.000000000000000000, 0.000000000000000000, -1.000000000000000000 ) ) ;
#35309 = CARTESIAN_POINT ( 'NONE',  ( 22.15000760687365045, -12.45670961578212044, -46.29898909444737853 ) ) ;
#35310 = CARTESIAN_POINT ( 'NONE',  ( 59.16375433153790198, -3.121456158035090134, -15.65965500696370150 ) ) ;
#35311 = CARTESIAN_POINT ( 'NONE',  ( 51.84245873739460819, -49.36807171846500353, -76.99756697886049039 ) ) ;
#35312 = DIRECTION ( 'NONE',  ( 0.000000000000000000, 0.000000000000000000, 1.000000000000000000 ) ) ;
#35313 = AXIS2_PLACEMENT_3D ( 'NONE', #35097, #18340, #38798 ) ;
#35314 = EDGE_LOOP ( 'NONE', ( #41751, #29409, #32697, #49680 ) ) ;
#35315 = CARTESIAN_POINT ( 'NONE',  ( 63.43393739769620510, 1.883811055320669947, -65.65000000000000568 ) ) ;
#35317 = CARTESIAN_POINT ( 'NONE',  ( 13.83887629743938952, -22.28516590677773124, -51.45268192009724828 ) ) ;
#35316 = AXIS2_PLACEMENT_3D ( 'NONE', #47618, #46857, #7016 ) ;
#35318 = DIRECTION ( 'NONE',  ( 0.000000000000000000, 0.000000000000000000, -1.000000000000000000 ) ) ;
#35319 = CARTESIAN_POINT ( 'NONE',  ( 55.00894225620579903, -45.11618894467940066, -13.91244749253660018 ) ) ;
#35320 = CARTESIAN_POINT ( 'NONE',  ( 21.59441065045999864, -21.25267538992449801, -56.26754282442009725 ) ) ;
#35321 = EDGE_CURVE ( 'NONE', #42937, #32383, #29744, .T. ) ;
#35322 = CARTESIAN_POINT ( 'NONE',  ( 13.86909323948740180, -50.63828459097629775, -21.27400668797699979 ) ) ;
#35323 = EDGE_CURVE ( 'NONE', #15666, #27249, #40533, .T. ) ;
#35324 = CARTESIAN_POINT ( 'NONE',  ( 9.750628328246584431, -12.76251341456665500, -63.98138790073967641 ) ) ;
#35325 = CARTESIAN_POINT ( 'NONE',  ( 56.65303980391289684, 13.95236716656019915, -16.48307942864150277 ) ) ;
#35326 = CARTESIAN_POINT ( 'NONE',  ( 8.943569970476479725, 18.10127401595480023, -34.64999999999999858 ) ) ;
#35327 = CARTESIAN_POINT ( 'NONE',  ( 56.76343337132740174, -50.53654875555030657, -53.08899915645069711 ) ) ;
#35328 = CARTESIAN_POINT ( 'NONE',  ( 19.43172305938700006, -9.381835016324110654, -50.50205474731569666 ) ) ;
#35329 = CARTESIAN_POINT ( 'NONE',  ( 17.90512765755580205, -9.025299540750683747, -44.03612187393183319 ) ) ;
#35330 = ORIENTED_EDGE ( 'NONE', *, *, #17441, .T. ) ;
#35331 = CARTESIAN_POINT ( 'NONE',  ( 11.67619942398487609, -64.89165360645621661, -46.39999999999999858 ) ) ;
#35332 = CARTESIAN_POINT ( 'NONE',  ( 65.09799605061490979, 1.383357884654609959, -60.97108096920410247 ) ) ;
#35333 = CARTESIAN_POINT ( 'NONE',  ( 8.222546438703959737, -15.61603098320130201, -50.50766849176299900 ) ) ;
#35334 = DIRECTION ( 'NONE',  ( 0.5835456732599438867, -0.8120803206700670795, 0.000000000000000000 ) ) ;
#35335 = CARTESIAN_POINT ( 'NONE',  ( 12.07188106636699843, -8.733914759373510250, -54.83830562705740874 ) ) ;
#35336 = DIRECTION ( 'NONE',  ( 0.4145156864928219442, 0.9100421669633690369, 0.000000000000000000 ) ) ;
#35337 = CARTESIAN_POINT ( 'NONE',  ( 11.73319001778020088, 34.19002770849310480, -18.17421237891140251 ) ) ;
#35338 = CARTESIAN_POINT ( 'NONE',  ( 72.12455669199461283, 1.010053820890669973, -70.13159119767689731 ) ) ;
#35340 = CARTESIAN_POINT ( 'NONE',  ( 47.31175340403380147, -38.13240412724670136, -53.74300098232180289 ) ) ;
#35339 = CARTESIAN_POINT ( 'NONE',  ( 52.28356737878640814, 18.56723623979891258, -77.20029292997260484 ) ) ;
#35341 = CARTESIAN_POINT ( 'NONE',  ( -11.09431950376199971, -42.12535119660120131, -6.431359894498750229 ) ) ;
#35342 = CARTESIAN_POINT ( 'NONE',  ( 49.72648160330969347, 22.41435850158130094, -55.11972614036070439 ) ) ;
#35343 = ORIENTED_EDGE ( 'NONE', *, *, #40931, .T. ) ;
#35344 = CIRCLE ( 'NONE', #33690, 39.99999999999999289 ) ;
#35345 = CARTESIAN_POINT ( 'NONE',  ( 53.21884732239679749, -49.50316525696469228, -49.08533780779099942 ) ) ;
#35346 = VECTOR ( 'NONE', #5237, 1000.000000000000000 ) ;
#35347 = ORIENTED_EDGE ( 'NONE', *, *, #41328, .F. ) ;
#35348 = CARTESIAN_POINT ( 'NONE',  ( 42.84191978890740415, 7.628041268320568946, -76.47496320122499469 ) ) ;
#35349 = DIRECTION ( 'NONE',  ( 0.000000000000000000, 0.000000000000000000, 1.000000000000000000 ) ) ;
#35350 = CARTESIAN_POINT ( 'NONE',  ( 14.18765051980080116, 19.87404487058600111, -22.27225542063749941 ) ) ;
#35351 = CYLINDRICAL_SURFACE ( 'NONE', #15654, 10.00000000000000711 ) ;
#35352 = CARTESIAN_POINT ( 'NONE',  ( 21.26150560491580066, -10.77360668136810062, -50.21191628250519301 ) ) ;
#35353 = CARTESIAN_POINT ( 'NONE',  ( 52.67198247596510186, 18.54881933231609992, -48.75776900890529930 ) ) ;
#35354 = CARTESIAN_POINT ( 'NONE',  ( 55.76692108999159814, -45.94014556479540090, -17.15567225542880081 ) ) ;
#35355 = DIRECTION ( 'NONE',  ( 0.000000000000000000, -3.043741000000000191E-10, -1.000000000000000000 ) ) ;
#35356 = ORIENTED_EDGE ( 'NONE', *, *, #34405, .T. ) ;
#35357 = EDGE_CURVE ( 'NONE', #16668, #26662, #38870, .T. ) ;
#35358 = CARTESIAN_POINT ( 'NONE',  ( 15.99127120266549973, -7.769763351723340428, -34.78171861563929923 ) ) ;
#35359 = ORIENTED_EDGE ( 'NONE', *, *, #49532, .F. ) ;
#35360 = ADVANCED_FACE ( 'NONE', ( #26544 ), #6650, .T. ) ;
#35361 = CARTESIAN_POINT ( 'NONE',  ( 11.08386367325309863, -65.09065137991299821, -17.36951596971170275 ) ) ;
#35362 = CARTESIAN_POINT ( 'NONE',  ( 9.063308985014520758, 32.62929763590770449, -46.73460937141010163 ) ) ;
#35363 = CARTESIAN_POINT ( 'NONE',  ( 73.04596072059979406, 1.186701509386330011, -62.36552507365149722 ) ) ;
#35364 = CARTESIAN_POINT ( 'NONE',  ( 17.16939511183450051, -23.52720176420199039, -40.25067858312961988 ) ) ;
#35366 = EDGE_CURVE ( 'NONE', #27935, #26995, #31050, .T. ) ;
#35365 = FACE_OUTER_BOUND ( 'NONE', #26323, .T. ) ;
#35367 = CARTESIAN_POINT ( 'NONE',  ( 68.13393739769620083, 1.883811055320649963, -65.65000000000000568 ) ) ;
#35368 = EDGE_CURVE ( 'NONE', #44712, #40580, #34683, .T. ) ;
#35369 = EDGE_LOOP ( 'NONE', ( #36186, #33419, #31556, #23726 ) ) ;
#35370 = CARTESIAN_POINT ( 'NONE',  ( 61.32241497109522044, 14.33206721631021274, -47.63528208083148030 ) ) ;
#35371 = CARTESIAN_POINT ( 'NONE',  ( 11.13393739769619906, -63.33602264272540339, -43.74835161547929374 ) ) ;
#35372 = CARTESIAN_POINT ( 'NONE',  ( -1.021187420881286778, 10.64619438059237311, -20.85710678118654471 ) ) ;
#35373 = ORIENTED_EDGE ( 'NONE', *, *, #23701, .T. ) ;
#35374 = DIRECTION ( 'NONE',  ( -0.3918900565005491998, -0.9200120562340454722, 0.000000000000000000 ) ) ;
#35375 = CARTESIAN_POINT ( 'NONE',  ( 15.29152898199282795, -7.731039397677363034, -76.97386002471692734 ) ) ;
#35376 = DIRECTION ( 'NONE',  ( 1.000000000000000000, 0.000000000000000000, 0.000000000000000000 ) ) ;
#35377 = VERTEX_POINT ( 'NONE', #48283 ) ;
#35378 = CARTESIAN_POINT ( 'NONE',  ( 9.221377447920410475, -19.60025744400465086, -62.62566432458431365 ) ) ;
#35379 = CARTESIAN_POINT ( 'NONE',  ( 50.96213159729676789, 19.72522742365540083, -76.14999999999994884 ) ) ;
#35380 = DIRECTION ( 'NONE',  ( -1.062456999999999985E-16, -7.719205000000000365E-17, -1.000000000000000000 ) ) ;
#35381 = DIRECTION ( 'NONE',  ( -1.224646799147365533E-16, 1.000000000000000000, 8.684364315601308223E-16 ) ) ;
#35382 = CARTESIAN_POINT ( 'NONE',  ( 9.274895627196098502, -11.04057247840179912, -66.97959240854859786 ) ) ;
#35383 = CARTESIAN_POINT ( 'NONE',  ( 15.14368416393435801, -8.633212666080043007, -38.30233936351858404 ) ) ;
#35384 = CARTESIAN_POINT ( 'NONE',  ( 46.40825105427388308, -38.19443686813398386, -58.27843028287923488 ) ) ;
#35385 = ORIENTED_EDGE ( 'NONE', *, *, #47379, .F. ) ;
#35386 = EDGE_CURVE ( 'NONE', #7646, #17962, #22109, .T. ) ;
#35387 = ORIENTED_EDGE ( 'NONE', *, *, #20780, .T. ) ;
#35388 = LINE ( 'NONE', #2919, #17520 ) ;
#35389 = B_SPLINE_CURVE_WITH_KNOTS ( 'NONE', 3,
 ( #7761, #11441, #15875, #39472, #43148, #23191, #27655, #27399 ),
 .UNSPECIFIED., .F., .F.,
 ( 4, 2, 2, 4 ),
 ( -0.6744302025021630120, -0.3586151102909330146, -0.07393671731179696227, 0.000000000000000000 ),
 .UNSPECIFIED. ) ;
#35390 = CARTESIAN_POINT ( 'NONE',  ( 11.57272752930120063, -21.50703424409100251, -50.94238055261769915 ) ) ;
#35391 = VECTOR ( 'NONE', #49379, 1000.000000000000000 ) ;
#35392 = CARTESIAN_POINT ( 'NONE',  ( 52.66091685537959677, -49.78821585947670059, -48.73922092854849808 ) ) ;
#35393 = CARTESIAN_POINT ( 'NONE',  ( 47.16461778607949640, 13.88381105532070059, -8.336225867471998896 ) ) ;
#35394 = DIRECTION ( 'NONE',  ( -1.000000000000000000, 0.000000000000000000, 0.000000000000000000 ) ) ;
#35395 = CARTESIAN_POINT ( 'NONE',  ( 47.35709157879159648, 23.41982112160560092, -74.50100479479878857 ) ) ;
#35396 = FACE_OUTER_BOUND ( 'NONE', #26472, .T. ) ;
#35397 = CARTESIAN_POINT ( 'NONE',  ( 9.995687254860799342, 22.60556764129900031, -34.69483829921999529 ) ) ;
#35398 = CARTESIAN_POINT ( 'NONE',  ( 12.15898433499079978, 33.83644259906850493, -16.45263499445269773 ) ) ;
#35399 = EDGE_CURVE ( 'NONE', #26463, #43797, #7951, .T. ) ;
#35400 = CARTESIAN_POINT ( 'NONE',  ( 16.63355634930200111, -7.386176696075330561, -73.02696842882760109 ) ) ;
#35401 = CARTESIAN_POINT ( 'NONE',  ( 21.23861683953670365, -21.46253214949600263, -32.14999999999999858 ) ) ;
#35402 = VECTOR ( 'NONE', #26041, 1000.000000000000000 ) ;
#35403 = CARTESIAN_POINT ( 'NONE',  ( 55.64373403256560380, -50.62227426193150137, -76.08015027475811110 ) ) ;
#35405 = DIRECTION ( 'NONE',  ( -1.000000000000000000, 0.000000000000000000, 0.000000000000000000 ) ) ;
#35404 = CARTESIAN_POINT ( 'NONE',  ( -10.40730447694229888, 11.61126731243840027, -6.269948428629449566 ) ) ;
#35406 = CARTESIAN_POINT ( 'NONE',  ( 63.04027743911709791, 0.9947083095259759977, -68.80546575785609775 ) ) ;
#35407 = DIRECTION ( 'NONE',  ( -1.000000000000000000, 2.473715676742926917E-14, 0.000000000000000000 ) ) ;
#35408 = ORIENTED_EDGE ( 'NONE', *, *, #447, .F. ) ;
#35409 = CARTESIAN_POINT ( 'NONE',  ( 53.06963669637619319, -49.53524040181889632, -48.79723990372909981 ) ) ;
#35410 = CARTESIAN_POINT ( 'NONE',  ( 47.67130882769900069, 23.27448986115780016, -54.89754209372490124 ) ) ;
#35411 = CARTESIAN_POINT ( 'NONE',  ( 57.84505944371250052, -45.56276322640520249, -26.25163502090950018 ) ) ;
#35412 = CARTESIAN_POINT ( 'NONE',  ( 9.586608879048261755, -20.10517931648513468, -66.60093937048264934 ) ) ;
#35413 = CARTESIAN_POINT ( 'NONE',  ( 13.29233961917630147, 19.36776406713639886, -21.35982916590099734 ) ) ;
#35414 = LINE ( 'NONE', #35152, #17302 ) ;
#35415 = CARTESIAN_POINT ( 'NONE',  ( 23.52796006295030296, -16.53003938695930231, -70.27179973214080633 ) ) ;
#35416 = CARTESIAN_POINT ( 'NONE',  ( 51.47835655202189997, 18.57467637314109865, -76.47682125365790284 ) ) ;
#35417 = CARTESIAN_POINT ( 'NONE',  ( 52.86806023909759489, 18.40847406621560012, -48.68114467674470092 ) ) ;
#35418 = CARTESIAN_POINT ( 'NONE',  ( 14.06329888286234286, -23.32129947607171871, -70.37566614802058496 ) ) ;
#35419 = LINE ( 'NONE', #3976, #4986 ) ;
#35420 = CARTESIAN_POINT ( 'NONE',  ( 51.29354596943910138, 21.74684883274469982, -54.72842898864520578 ) ) ;
#35421 = B_SPLINE_CURVE_WITH_KNOTS ( 'NONE', 3,
 ( #8385, #257, #28541, #4445, #16243, #16497 ),
 .UNSPECIFIED., .F., .F.,
 ( 4, 2, 4 ),
 ( 0.000000000000000000, 0.2512731404157662607, 0.5025462808315325214 ),
 .UNSPECIFIED. ) ;
#35422 = EDGE_CURVE ( 'NONE', #51387, #50052, #4536, .T. ) ;
#35423 = AXIS2_PLACEMENT_3D ( 'NONE', #44627, #49615, #37025 ) ;
#35424 = CARTESIAN_POINT ( 'NONE',  ( 21.76696967735496457, -21.17076488492029540, -61.75542963454200418 ) ) ;
#35425 = CARTESIAN_POINT ( 'NONE',  ( 9.221397583389689956, -11.63208602404207248, -36.95899869649823444 ) ) ;
#35426 = CARTESIAN_POINT ( 'NONE',  ( 9.543082305263988374, -17.38750236223247470, -71.36948714414663186 ) ) ;
#35427 = CARTESIAN_POINT ( 'NONE',  ( 60.61936386226810214, -29.82345567790940066, -15.97700830362510160 ) ) ;
#35429 = ADVANCED_FACE ( 'NONE', ( #19722, #4252 ), #3753, .T. ) ;
#35428 = CARTESIAN_POINT ( 'NONE',  ( 71.04878173523039209, 1.375383258925270136, -60.85412179317820147 ) ) ;
#35430 = CARTESIAN_POINT ( 'NONE',  ( 16.13393739769620083, -1.590680505402594314, -34.79644660940672196 ) ) ;
#35431 = AXIS2_PLACEMENT_3D ( 'NONE', #27056, #50913, #15007 ) ;
#35432 = CARTESIAN_POINT ( 'NONE',  ( 72.51559007951500746, 1.439519383694849886, -61.97453994048029813 ) ) ;
#35433 = CARTESIAN_POINT ( 'NONE',  ( 10.66652299674349891, -20.07151597450609870, -41.62953446819029324 ) ) ;
#35434 = EDGE_CURVE ( 'NONE', #49378, #6409, #36212, .T. ) ;
#35435 = CARTESIAN_POINT ( 'NONE',  ( 16.70953489029340844, -8.802035222471227272, -65.98000098515855427 ) ) ;
#35436 = ORIENTED_EDGE ( 'NONE', *, *, #13707, .T. ) ;
#35437 = ORIENTED_EDGE ( 'NONE', *, *, #41564, .F. ) ;
#35438 = DIRECTION ( 'NONE',  ( 0.8320502943378731420, 1.839589000000000426E-27, -0.5547001962251850715 ) ) ;
#35439 = CARTESIAN_POINT ( 'NONE',  ( 17.90524625539175929, -22.20704482888588061, -58.86948671774002406 ) ) ;
#35440 = ORIENTED_EDGE ( 'NONE', *, *, #12660, .F. ) ;
#35441 = CARTESIAN_POINT ( 'NONE',  ( 55.83268520914499788, -46.02255925261680147, -25.40756166689039830 ) ) ;
#35442 = CARTESIAN_POINT ( 'NONE',  ( 20.44745845214795565, -22.25469778744673377, -77.82425224410800979 ) ) ;
#35443 = ORIENTED_EDGE ( 'NONE', *, *, #34363, .F. ) ;
#35444 = CARTESIAN_POINT ( 'NONE',  ( 0.4371248283887909647, -22.38658506580789975, -35.02873218748179340 ) ) ;
#35445 = CARTESIAN_POINT ( 'NONE',  ( 42.66764366557126920, 6.495846304519615977, -76.98140147941434464 ) ) ;
#35446 = EDGE_CURVE ( 'NONE', #11926, #17858, #28339, .T. ) ;
#35447 = CARTESIAN_POINT ( 'NONE',  ( 11.09688807260409860, 33.08637917209059509, -23.87186459811089989 ) ) ;
#35448 = VERTEX_POINT ( 'NONE', #44343 ) ;
#35449 = CARTESIAN_POINT ( 'NONE',  ( 18.91168734512759997, -23.37936002268359914, -34.18295494821020242 ) ) ;
#35450 = AXIS2_PLACEMENT_3D ( 'NONE', #4040, #24433, #24951 ) ;
#35451 = CARTESIAN_POINT ( 'NONE',  ( 51.35264461321370533, 0.6974074393915098424, -17.41533276683830422 ) ) ;
#35452 = CARTESIAN_POINT ( 'NONE',  ( 10.81643727141089961, 33.72113552640900025, -17.63284883033089656 ) ) ;
#35453 = EDGE_CURVE ( 'NONE', #37534, #4707, #50608, .T. ) ;
#35454 = CIRCLE ( 'NONE', #42155, 4.649999999999999467 ) ;
#35455 = CARTESIAN_POINT ( 'NONE',  ( 61.58903658307470153, -29.46446663135400001, -16.00793433331780236 ) ) ;
#35456 =( BOUNDED_CURVE ( )  B_SPLINE_CURVE ( 3, ( #46643, #38506, #34031, #26171 ),
 .UNSPECIFIED., .F., .T. ) 
 B_SPLINE_CURVE_WITH_KNOTS ( ( 4, 4 ),
 ( 0.000000000000000000, 1.220017676946477003 ),
 .UNSPECIFIED. ) 
 CURVE ( )  GEOMETRIC_REPRESENTATION_ITEM ( )  RATIONAL_B_SPLINE_CURVE ( ( 1.000000000000000000, 0.8797619696931662236, 0.8797619696931662236, 1.000000000000000000 ) ) 
 REPRESENTATION_ITEM ( '' )  );
#35457 = CARTESIAN_POINT ( 'NONE',  ( 14.36273055480719485, -9.025305204108461155, -63.86948780716260643 ) ) ;
#35458 = CARTESIAN_POINT ( 'NONE',  ( 47.02648735467300156, -54.07884064525359946, -75.65465545553870186 ) ) ;
#35459 = CARTESIAN_POINT ( 'NONE',  ( 17.69707065050570094, -7.925716785862018554, -69.57632324310809224 ) ) ;
#35460 = DIRECTION ( 'NONE',  ( -0.7071067811865475727, 0.000000000000000000, 0.7071067811865475727 ) ) ;
#35461 = CARTESIAN_POINT ( 'NONE',  ( 42.04041500005769194, 14.50277640103930032, -6.805323752375540103 ) ) ;
#35462 = CYLINDRICAL_SURFACE ( 'NONE', #39338, 7.910999999999997812 ) ;
#35463 = AXIS2_PLACEMENT_3D ( 'NONE', #6695, #10365, #1718 ) ;
#35464 = VECTOR ( 'NONE', #39781, 1000.000000000000000 ) ;
#35465 = CARTESIAN_POINT ( 'NONE',  ( 82.76927220787739259, -45.23714010519090323, -47.14638044783710313 ) ) ;
#35466 = AXIS2_PLACEMENT_3D ( 'NONE', #23517, #4139, #35334 ) ;
#35467 = CARTESIAN_POINT ( 'NONE',  ( 60.91810547036719470, 13.88381111439859872, -26.64295475793029766 ) ) ;
#35468 = ADVANCED_FACE ( 'NONE', ( #15543 ), #40670, .T. ) ;
#35469 = CARTESIAN_POINT ( 'NONE',  ( 7.888783485131068751, -15.60363238914669992, -44.50815324592469580 ) ) ;
#35470 = EDGE_LOOP ( 'NONE', ( #36985, #48905, #8819, #33598, #6745, #7788, #38978 ) ) ;
#35472 = EDGE_CURVE ( 'NONE', #5521, #10190, #40928, .T. ) ;
#35471 = CARTESIAN_POINT ( 'NONE',  ( 52.82976017067200303, -49.66091843452839782, -28.15000000000000213 ) ) ;
#35473 = CARTESIAN_POINT ( 'NONE',  ( 15.94238461914479821, -50.98711296417160099, -20.23090583108240281 ) ) ;
#35474 = CARTESIAN_POINT ( 'NONE',  ( 76.15791883449350053, -18.73183087738710029, -12.10556864792070009 ) ) ;
#35475 = CARTESIAN_POINT ( 'NONE',  ( 75.44523968101177047, 12.62269330545501056, -13.52496103299877817 ) ) ;
#35476 = APPLICATION_CONTEXT ( 'automotive_design' ) ;
#35477 = DIRECTION ( 'NONE',  ( 0.7071067811865475727, 0.7071067811865475727, 0.000000000000000000 ) ) ;
#35478 = DIRECTION ( 'NONE',  ( 0.000000000000000000, -1.000000000000000000, 0.000000000000000000 ) ) ;
#35479 = CARTESIAN_POINT ( 'NONE',  ( 10.12791152504585490, -55.17571126438489415, -23.14397412734965442 ) ) ;
#35480 = CARTESIAN_POINT ( 'NONE',  ( 82.81464131963001307, 11.88381105532070059, -49.28546657628889704 ) ) ;
#35481 = CARTESIAN_POINT ( 'NONE',  ( 82.54539245911229273, -45.15147844613900219, -46.85686783343579975 ) ) ;
#35482 = CARTESIAN_POINT ( 'NONE',  ( 57.32397924865310301, -50.46483022149049447, -53.14987063508399956 ) ) ;
#35483 = CARTESIAN_POINT ( 'NONE',  ( 41.87524974339859796, 13.12449424351239990, -5.012953160694429755 ) ) ;
#35484 = CARTESIAN_POINT ( 'NONE',  ( 47.64115382883381500, -54.53453007756522197, -74.19838441416023045 ) ) ;
#35485 = LINE ( 'NONE', #38913, #5679 ) ;
#35486 = CARTESIAN_POINT ( 'NONE',  ( 57.45452828658709876, -47.23787284142349563, -47.71980555553449932 ) ) ;
#35487 = CARTESIAN_POINT ( 'NONE',  ( 69.22748654599975282, -50.70395984887971252, -73.25000000000218847 ) ) ;
#35488 = AXIS2_PLACEMENT_3D ( 'NONE', #392, #47842, #16376 ) ;
#35489 = CARTESIAN_POINT ( 'NONE',  ( 66.71250208829920325, -1.458054078887639937, -17.03570979604049995 ) ) ;
#35490 = CARTESIAN_POINT ( 'NONE',  ( 18.21961131258260380, -52.14694418483640703, -75.69083100613939052 ) ) ;
#35491 = CARTESIAN_POINT ( 'NONE',  ( 50.09219850407249908, -44.97296149410799870, -7.597817017042959975 ) ) ;
#35492 = EDGE_CURVE ( 'NONE', #51786, #37751, #7307, .T. ) ;
#35493 = CARTESIAN_POINT ( 'NONE',  ( 8.935742952634630143, -13.69455134371859906, -68.15038248396290044 ) ) ;
#35494 = CARTESIAN_POINT ( 'NONE',  ( 14.16187783161720048, 19.11875810978959933, -20.85710678118659800 ) ) ;
#35495 = FACE_BOUND ( 'NONE', #3029, .T. ) ;
#35496 = EDGE_LOOP ( 'NONE', ( #5046, #48787, #42557, #23231 ) ) ;
#35497 = DIRECTION ( 'NONE',  ( -1.000000000000000000, 0.000000000000000000, 0.000000000000000000 ) ) ;
#35498 = CARTESIAN_POINT ( 'NONE',  ( 12.03010629790625252, -21.02215419574001132, -35.15951470918400190 ) ) ;
#35499 = CARTESIAN_POINT ( 'NONE',  ( 72.87639502376930523, 1.370118064600889918, -68.71049874078630637 ) ) ;
#35500 = DIRECTION ( 'NONE',  ( -0.3294064756441338893, -0.9441882088883076785, 0.000000000000000000 ) ) ;
#35501 = CARTESIAN_POINT ( 'NONE',  ( 12.03971614317870120, -9.101958363581481137, -81.23899999999999011 ) ) ;
#35502 = ADVANCED_FACE ( 'NONE', ( #45126 ), #2868, .T. ) ;
#35503 = VERTEX_POINT ( 'NONE', #17096 ) ;
#35504 = CARTESIAN_POINT ( 'NONE',  ( 17.53794073517549990, 21.17773733622360410, -76.03043890231919022 ) ) ;
#35505 = ORIENTED_EDGE ( 'NONE', *, *, #48493, .F. ) ;
#35506 = TOROIDAL_SURFACE ( 'NONE', #43884, 13.00000000000000000, 0.5000000000000000000 ) ;
#35507 = EDGE_LOOP ( 'NONE', ( #49172, #26271, #38033, #28983 ) ) ;
#35508 = CARTESIAN_POINT ( 'NONE',  ( 16.13393739769639623, 7.383811055320659733, 4.943674098299959851 ) ) ;
#35509 = CARTESIAN_POINT ( 'NONE',  ( 21.67336050504559708, -10.00387830695770042, -81.23899999999999011 ) ) ;
#35510 = CIRCLE ( 'NONE', #45532, 13.50000000000000178 ) ;
#35511 = CARTESIAN_POINT ( 'NONE',  ( 61.63216019317309957, 14.00749853620810015, -47.06783276606689981 ) ) ;
#35512 = EDGE_LOOP ( 'NONE', ( #47700, #46537 ) ) ;
#35513 = LINE ( 'NONE', #47326, #18226 ) ;
#35514 = ORIENTED_EDGE ( 'NONE', *, *, #22468, .T. ) ;
#35515 = CARTESIAN_POINT ( 'NONE',  ( 33.13393739769620083, 7.383811055320659733, -59.64999999999999147 ) ) ;
#35516 = DIRECTION ( 'NONE',  ( -1.000000000000000000, -0.000000000000000000, -0.000000000000000000 ) ) ;
#35517 = VERTEX_POINT ( 'NONE', #45643 ) ;
#35518 = LINE ( 'NONE', #38946, #23290 ) ;
#35519 = CARTESIAN_POINT ( 'NONE',  ( 51.84413677266599763, -51.33743803777170456, -76.02231597519390505 ) ) ;
#35520 = CARTESIAN_POINT ( 'NONE',  ( 60.69877040361549092, 14.44127893251400074, -47.62175228562969664 ) ) ;
#35521 = LINE ( 'NONE', #51513, #40603 ) ;
#35522 = AXIS2_PLACEMENT_3D ( 'NONE', #43074, #38358, #18432 ) ;
#35523 = DIRECTION ( 'NONE',  ( 1.071169953407190059E-15, 3.740764114965449782E-16, -1.000000000000000000 ) ) ;
#35524 = CARTESIAN_POINT ( 'NONE',  ( -7.971602555222980335, 13.89700050900779971, -5.685733215756870074 ) ) ;
#35525 = CARTESIAN_POINT ( 'NONE',  ( 64.43393739769619799, 11.38381105532070059, -68.84999999999999432 ) ) ;
#35526 = DIRECTION ( 'NONE',  ( 1.000000000000000000, 0.000000000000000000, 0.000000000000000000 ) ) ;
#35527 = ADVANCED_FACE ( 'NONE', ( #9994 ), #29387, .F. ) ;
#35528 = AXIS2_PLACEMENT_3D ( 'NONE', #41333, #20623, #8856 ) ;
#35529 = CARTESIAN_POINT ( 'NONE',  ( 9.038446734346580413, -12.26346461519720066, -54.42801351941700005 ) ) ;
#35530 = ORIENTED_EDGE ( 'NONE', *, *, #9625, .F. ) ;
#35532 = EDGE_CURVE ( 'NONE', #20094, #39800, #21254, .T. ) ;
#35531 = CARTESIAN_POINT ( 'NONE',  ( 38.67452568954050207, 4.883811055320659733, -81.65000000000000568 ) ) ;
#35533 = CIRCLE ( 'NONE', #30506, 1.999999999999997558 ) ;
#35534 = CARTESIAN_POINT ( 'NONE',  ( 57.28143945796900027, 19.37965786551299985, -53.75925914748309964 ) ) ;
#35535 = CARTESIAN_POINT ( 'NONE',  ( 71.57077554288350996, 1.229987811083010030, -70.43721585241399907 ) ) ;
#35536 = EDGE_CURVE ( 'NONE', #10825, #39256, #5455, .T. ) ;
#35537 = CARTESIAN_POINT ( 'NONE',  ( 43.73738396686909624, -39.93285218904156864, -67.93068977794935392 ) ) ;
#35538 = CARTESIAN_POINT ( 'NONE',  ( 15.70006563680709988, 19.64728943285669871, -20.26432904851870020 ) ) ;
#35539 = SURFACE_STYLE_USAGE ( .BOTH. , #19805 ) ;
#35540 = CARTESIAN_POINT ( 'NONE',  ( 9.367802395840252316, -16.31250631742587132, -45.81442615037286004 ) ) ;
#35541 = CARTESIAN_POINT ( 'NONE',  ( 63.22121223625129716, 0.9369374701296400154, -69.09468190869459647 ) ) ;
#35542 = CARTESIAN_POINT ( 'NONE',  ( 48.58275802200249416, -54.12519460547050443, -55.12629154858839797 ) ) ;
#35543 = DIRECTION ( 'NONE',  ( -0.9750030843198951302, 0.2182216943050036273, -0.04181241085306048461 ) ) ;
#35544 = DIRECTION ( 'NONE',  ( 0.000000000000000000, 1.000000000000000000, 0.000000000000000000 ) ) ;
#35545 = CARTESIAN_POINT ( 'NONE',  ( 9.221478158419834870, -19.60042960929790112, -38.34100232044492884 ) ) ;
#35546 = CARTESIAN_POINT ( 'NONE',  ( 47.84066234768640413, 23.15588260058000003, -54.73860067540169894 ) ) ;
#35547 = ORIENTED_EDGE ( 'NONE', *, *, #24931, .T. ) ;
#35548 = CARTESIAN_POINT ( 'NONE',  ( 23.55285262543469926, -16.29911733182590083, -37.09656150702409860 ) ) ;
#35549 = CARTESIAN_POINT ( 'NONE',  ( 87.61621807841599718, 1.883811055320649963, -61.12885639714370001 ) ) ;
#35550 = ORIENTED_EDGE ( 'NONE', *, *, #18802, .T. ) ;
#35551 = CARTESIAN_POINT ( 'NONE',  ( 71.60000756020500035, 0.9395704634982890990, -70.54765821028050254 ) ) ;
#35552 = CARTESIAN_POINT ( 'NONE',  ( 60.50030625420910013, -45.69302653460029973, -47.49279232948880036 ) ) ;
#35553 = CARTESIAN_POINT ( 'NONE',  ( 16.13393739769620083, -15.61618894467929941, 7.944363289481099599 ) ) ;
#35554 = DIRECTION ( 'NONE',  ( 0.000000000000000000, 0.000000000000000000, 1.000000000000000000 ) ) ;
#35556 = DIRECTION ( 'NONE',  ( -1.000000000000000000, 0.000000000000000000, 0.000000000000000000 ) ) ;
#35555 = CARTESIAN_POINT ( 'NONE',  ( -31.07316938349034885, 21.88381105532059934, 17.05710678118654755 ) ) ;
#35557 = CARTESIAN_POINT ( 'NONE',  ( 2.277530937145189949, -15.61618894467929941, -24.14999999999999858 ) ) ;
#35558 = CARTESIAN_POINT ( 'NONE',  ( 56.57438608727660068, 19.50039335391339890, -53.83822343184270665 ) ) ;
#35559 = EDGE_CURVE ( 'NONE', #29501, #9653, #39715, .T. ) ;
#35560 = ORIENTED_EDGE ( 'NONE', *, *, #28773, .T. ) ;
#35561 = CARTESIAN_POINT ( 'NONE',  ( 0.1094292354459709959, 19.93927366128230005, -35.12965084568739371 ) ) ;
#35562 = AXIS2_PLACEMENT_3D ( 'NONE', #46175, #34606, #46434 ) ;
#35563 = ORIENTED_EDGE ( 'NONE', *, *, #27033, .T. ) ;
#35564 = DIRECTION ( 'NONE',  ( 0.000000000000000000, 0.000000000000000000, -1.000000000000000000 ) ) ;
#35565 = CARTESIAN_POINT ( 'NONE',  ( 7.853097003783780394, -60.52042854835909935, -20.86915960608759946 ) ) ;
#35566 = LINE ( 'NONE', #7275, #16020 ) ;
#35567 = CARTESIAN_POINT ( 'NONE',  ( 8.875293479575059763, -63.51482374901029715, -46.68678635115289666 ) ) ;
#35568 = ORIENTED_EDGE ( 'NONE', *, *, #29319, .F. ) ;
#35569 = ORIENTED_EDGE ( 'NONE', *, *, #13218, .T. ) ;
#35570 = CARTESIAN_POINT ( 'NONE',  ( 56.10252018248599626, 19.69840918101340321, -53.89291062689480327 ) ) ;
#35571 = CIRCLE ( 'NONE', #18023, 4.000000000000050626 ) ;
#35572 = CARTESIAN_POINT ( 'NONE',  ( 18.16448196509431057, -8.861961676679264599, -32.44013846481051644 ) ) ;
#35573 = CARTESIAN_POINT ( 'NONE',  ( 56.50147281689459788, -50.73097677643320225, -53.50280580149859588 ) ) ;
#35574 = VECTOR ( 'NONE', #31007, 1000.000000000000227 ) ;
#35575 = CARTESIAN_POINT ( 'NONE',  ( 71.63393739769620083, -15.61618894467929941, -10.21818181818179916 ) ) ;
#35576 = CARTESIAN_POINT ( 'NONE',  ( 62.92431185641218860, -0.4811861693229420034, -16.47144764524460214 ) ) ;
#35577 = CARTESIAN_POINT ( 'NONE',  ( 51.34762213876319947, -48.99373472892960280, -76.60870781533139962 ) ) ;
#35578 = CARTESIAN_POINT ( 'NONE',  ( 47.40322300430479885, -54.65574458090379295, -64.38029159777090626 ) ) ;
#35579 = VERTEX_POINT ( 'NONE', #25187 ) ;
#35580 = CARTESIAN_POINT ( 'NONE',  ( 63.15932386229340523, 0.8936201581567920771, -69.00461532610479765 ) ) ;
#35581 = CARTESIAN_POINT ( 'NONE',  ( 71.33393739769628894, 1.883811055320669947, -69.84999999999999432 ) ) ;
#35582 = CARTESIAN_POINT ( 'NONE',  ( 22.89179345042635561, -15.09430521664105207, -34.42831083698472128 ) ) ;
#35583 = B_SPLINE_CURVE_WITH_KNOTS ( 'NONE', 3,
 ( #2305, #42406, #17518, #22459, #50525, #18543, #33489, #49503, #41884, #13592, #29556, #39757, #27692, #31095, #15396, #47125 ),
 .UNSPECIFIED., .F., .F.,
 ( 4, 2, 2, 2, 2, 2, 2, 4 ),
 ( -4.585261641054179549, -4.291753173737439475, -3.753927176172620062, -2.893405580068910243, -2.204988303185950294, -1.516571026302980130, -0.4151033832902326637, 0.01085480678109984609 ),
 .UNSPECIFIED. ) ;
#35584 = LINE ( 'NONE', #43958, #3567 ) ;
#35585 = CARTESIAN_POINT ( 'NONE',  ( 10.49363452053940016, -10.15965789963630073, -53.25722344400259800 ) ) ;
#35586 = CARTESIAN_POINT ( 'NONE',  ( 12.86227365120030086, -49.99703835600479351, -21.07384430431449829 ) ) ;
#35587 = CARTESIAN_POINT ( 'NONE',  ( 56.77603274427010405, 19.38693246832160000, -75.16653984338270789 ) ) ;
#35588 = CARTESIAN_POINT ( 'NONE',  ( 5.133937397696200833, -15.61618894467929763, -19.83999999999999986 ) ) ;
#35589 = CARTESIAN_POINT ( 'NONE',  ( 68.13393739769790614, -49.95860450174320277, -71.35146707679190570 ) ) ;
#35590 = CARTESIAN_POINT ( 'NONE',  ( 61.22240636566869654, -45.33348669533059905, -47.17363803446809811 ) ) ;
#35591 = DIRECTION ( 'NONE',  ( 0.000000000000000000, 1.000000000000000000, 0.000000000000000000 ) ) ;
#35592 = CARTESIAN_POINT ( 'NONE',  ( 14.67229395948390014, -22.51591050674119998, -55.41362847326009700 ) ) ;
#35593 = CARTESIAN_POINT ( 'NONE',  ( 46.92619617342869986, -39.55025295385299700, -54.22374093852179300 ) ) ;
#35594 = VERTEX_POINT ( 'NONE', #41192 ) ;
#35595 = CIRCLE ( 'NONE', #38971, 0.9999999999999940048 ) ;
#35597 = EDGE_CURVE ( 'NONE', #362, #8932, #45390, .T. ) ;
#35596 = CARTESIAN_POINT ( 'NONE',  ( 13.96137116643440024, -51.22777015964090452, -74.58518005236030035 ) ) ;
#35598 = CARTESIAN_POINT ( 'NONE',  ( 65.11238450761909746, 1.383161449028130097, -60.96613084263369586 ) ) ;
#35599 = CARTESIAN_POINT ( 'NONE',  ( 44.73511642677699740, -46.10436220937679508, -8.795271389338660484 ) ) ;
#35600 = CIRCLE ( 'NONE', #36407, 1.000000000000000888 ) ;
#35601 = DIRECTION ( 'NONE',  ( 0.7071067811865475727, 0.7071067811865475727, 0.000000000000000000 ) ) ;
#35602 = CARTESIAN_POINT ( 'NONE',  ( 11.27233469758729534, -9.289966755700637790, -46.79933556288879970 ) ) ;
#35603 = CARTESIAN_POINT ( 'NONE',  ( 10.72320681400480069, -64.90816318788569106, -17.84617904804760258 ) ) ;
#35604 = CIRCLE ( 'NONE', #1307, 20.79999999999999716 ) ;
#35605 = CARTESIAN_POINT ( 'NONE',  ( 8.222913476524595922, -14.68340101419122767, -64.54520946242661239 ) ) ;
#35607 = CARTESIAN_POINT ( 'NONE',  ( 46.89115067490939737, -38.09589644477580350, -55.84613562826960020 ) ) ;
#35606 = CARTESIAN_POINT ( 'NONE',  ( 9.367118387258660306, -15.61602127472129986, -41.45282021618999835 ) ) ;
#35608 = DIRECTION ( 'NONE',  ( -1.000000000000000000, 0.000000000000000000, 0.000000000000000000 ) ) ;
#35609 = DIRECTION ( 'NONE',  ( 0.000000000000000000, 0.000000000000000000, 1.000000000000000000 ) ) ;
#35610 = CARTESIAN_POINT ( 'NONE',  ( 49.45469051709869746, 22.31164040509669988, -54.26811687044270371 ) ) ;
#35611 = EDGE_LOOP ( 'NONE', ( #44961, #34176, #48084, #9539, #5804, #6151, #22667, #18470 ) ) ;
#35612 = CARTESIAN_POINT ( 'NONE',  ( 52.65605657214259594, -49.77872703647310715, -48.59647644059229776 ) ) ;
#35613 = VERTEX_POINT ( 'NONE', #5562 ) ;
#35614 = AXIS2_PLACEMENT_3D ( 'NONE', #36907, #1270, #48982 ) ;
#35615 = CARTESIAN_POINT ( 'NONE',  ( 47.55417156253681554, 6.784838323329733356, -52.48116776818960716 ) ) ;
#35616 = DIRECTION ( 'NONE',  ( 5.675813951744191581E-32, -1.000000000000000000, -5.351958659602149705E-17 ) ) ;
#35617 = DIRECTION ( 'NONE',  ( 0.000000000000000000, 0.000000000000000000, 1.000000000000000000 ) ) ;
#35618 = CARTESIAN_POINT ( 'NONE',  ( 46.99244837402765995, -39.23262767327315714, -34.80140398659612089 ) ) ;
#35619 = CARTESIAN_POINT ( 'NONE',  ( 9.261484497740870125, -17.20110213931209842, -53.38067352504999263 ) ) ;
#35620 = CARTESIAN_POINT ( 'NONE',  ( 52.56949858562949629, 18.62486711300499920, -48.49330934070029997 ) ) ;
#35621 = CARTESIAN_POINT ( 'NONE',  ( 57.24436374624130508, -45.12772278168660023, -17.69927926731909906 ) ) ;
#35622 = EDGE_CURVE ( 'NONE', #5583, #34588, #12116, .T. ) ;
#35623 = LINE ( 'NONE', #51610, #18114 ) ;
#35624 = B_SPLINE_CURVE_WITH_KNOTS ( 'NONE', 3,
 ( #51567, #27954, #48672, #39521, #16690, #20602, #12250, #32647, #11748, #36597, #12776, #36087, #32386, #8061, #20347, #24267 ),
 .UNSPECIFIED., .F., .F.,
 ( 4, 2, 2, 2, 2, 2, 2, 4 ),
 ( 0.000000000000000000, 0.07216186899278899392, 0.1546325764131200042, 0.2061767685508260062, 0.2319488646196799786, 0.2731842183298449633, 0.3391607842661090166, 0.4123535371016520124 ),
 .UNSPECIFIED. ) ;
#35625 = VERTEX_POINT ( 'NONE', #18361 ) ;
#35626 = CARTESIAN_POINT ( 'NONE',  ( 11.08120865841010172, -21.62091045948539758, -40.01016806583820085 ) ) ;
#35627 = EDGE_CURVE ( 'NONE', #51462, #12691, #24601, .T. ) ;
#35628 = ORIENTED_EDGE ( 'NONE', *, *, #25299, .F. ) ;
#35629 = CARTESIAN_POINT ( 'NONE',  ( 11.62127297442820151, -65.32903965486170250, -17.36671640434929742 ) ) ;
#35630 = CARTESIAN_POINT ( 'NONE',  ( 13.00893739769619906, 34.28605925116850273, -47.75434321273180416 ) ) ;
#35631 = CARTESIAN_POINT ( 'NONE',  ( 72.73458218292580568, 1.393731187554809958, -62.48946499964799983 ) ) ;
#35632 = DIRECTION ( 'NONE',  ( -0.9223605572461988089, 0.3863301728269249447, 0.000000000000000000 ) ) ;
#35633 = CARTESIAN_POINT ( 'NONE',  ( 11.62625575059174388, -65.37594719773773022, -22.52256012421784348 ) ) ;
#35634 = CARTESIAN_POINT ( 'NONE',  ( 9.366937397696199596, -15.61618894467949836, -28.45282021618999835 ) ) ;
#35635 = VECTOR ( 'NONE', #21144, 1000.000000000000000 ) ;
#35636 = EDGE_LOOP ( 'NONE', ( #30007, #22650, #14982, #26332, #24069, #21022 ) ) ;
#35637 = CARTESIAN_POINT ( 'NONE',  ( 64.83879995576880617, 1.326134026835569912, -70.39062084647959239 ) ) ;
#35638 = AXIS2_PLACEMENT_3D ( 'NONE', #22635, #35213, #30756 ) ;
#35639 = CARTESIAN_POINT ( 'NONE',  ( 11.10572538624809980, -63.45979201291619631, -44.26003604607290498 ) ) ;
#35640 = CARTESIAN_POINT ( 'NONE',  ( 66.23540447448930024, 18.72622661238738573, -69.60146707679315625 ) ) ;
#35641 = EDGE_LOOP ( 'NONE', ( #43293, #31155, #40737, #51020, #26060 ) ) ;
#35642 = CARTESIAN_POINT ( 'NONE',  ( 24.04406723441278615, -15.74292296389717016, -43.79742354999311260 ) ) ;
#35643 = CARTESIAN_POINT ( 'NONE',  ( 56.85837506870640112, 19.39490789456009878, -53.45324575393789956 ) ) ;
#35644 = CARTESIAN_POINT ( 'NONE',  ( 22.65454694203958041, -11.11335924479742232, -49.31532081587366889 ) ) ;
#35645 = EDGE_LOOP ( 'NONE', ( #45183, #49302, #21304, #50285 ) ) ;
#35646 = CARTESIAN_POINT ( 'NONE',  ( 17.16944623581769136, -23.52719446311581564, -62.25066316136566513 ) ) ;
#35647 = DIRECTION ( 'NONE',  ( 0.3805321250008311118, 0.000000000000000000, -0.9247677015566405645 ) ) ;
#35648 = CARTESIAN_POINT ( 'NONE',  ( 0.1457841021255935343, -8.319710351909083812, -34.68167779225149161 ) ) ;
#35649 = CARTESIAN_POINT ( 'NONE',  ( 60.36615763377369603, 14.63541242539259990, -47.74315751841469790 ) ) ;
#35650 = CARTESIAN_POINT ( 'NONE',  ( 8.764411544466659265, -19.31386507361439797, -76.64430199831019763 ) ) ;
#35651 = DIRECTION ( 'NONE',  ( 0.8889875008987390137, -0.4579314612972278375, 0.000000000000000000 ) ) ;
#35652 = CARTESIAN_POINT ( 'NONE',  ( 11.96660005458890019, -42.11618894467939356, -34.64999999999999858 ) ) ;
#35653 = ITEM_DEFINED_TRANSFORMATION ( 'NONE', 'NONE', #9301,  #20940 ) ;
#35654 = EDGE_LOOP ( 'NONE', ( #2287, #41187, #8562, #25806 ) ) ;
#35655 = ORIENTED_EDGE ( 'NONE', *, *, #21166, .F. ) ;
#35656 = CARTESIAN_POINT ( 'NONE',  ( 21.93377459515039973, -20.29257454556510254, -60.44865228025199144 ) ) ;
#35657 = CARTESIAN_POINT ( 'NONE',  ( 52.90415637000559457, -49.66383135056049980, -49.01931408368830034 ) ) ;
#35658 = CIRCLE ( 'NONE', #35614, 0.5000000000000004441 ) ;
#35659 = CARTESIAN_POINT ( 'NONE',  ( 16.13393739769620083, -15.61618894467929941, -35.02873218748179340 ) ) ;
#35660 = DIRECTION ( 'NONE',  ( 0.6668512999106330774, -0.3436531272335560661, -0.6612199875609450217 ) ) ;
#35662 = ADVANCED_FACE ( 'NONE', ( #46694 ), #30492, .T. ) ;
#35661 = CARTESIAN_POINT ( 'NONE',  ( 47.25421481023769843, 23.38596379756510046, -74.80705470093730014 ) ) ;
#35663 = LINE ( 'NONE', #30681, #40970 ) ;
#35664 = PRODUCT ( 'Top Mounting Plate', 'Top Mounting Plate', '', ( #16245 ) ) ;
#35665 = CARTESIAN_POINT ( 'NONE',  ( 10.04852440033089600, 22.72579217771966142, -34.76477869314942382 ) ) ;
#35666 = CARTESIAN_POINT ( 'NONE',  ( 11.93287529299120031, 33.86695641789320632, -16.56789608241509626 ) ) ;
#35667 = AXIS2_PLACEMENT_3D ( 'NONE', #27471, #19358, #7579 ) ;
#35668 = CARTESIAN_POINT ( 'NONE',  ( 18.42842099012590040, -23.53566277524700112, -71.91790339393689635 ) ) ;
#35669 = CARTESIAN_POINT ( 'NONE',  ( 55.48119774689679673, -46.46934856230480193, -25.44854998053999751 ) ) ;
#35670 = AXIS2_PLACEMENT_3D ( 'NONE', #28137, #31807, #4823 ) ;
#35671 = CARTESIAN_POINT ( 'NONE',  ( 55.66467133867650574, -50.64778639553559714, -75.85212640423078767 ) ) ;
#35673 = CARTESIAN_POINT ( 'NONE',  ( 17.90512446449194783, -9.025298638364542825, -60.03612613525060482 ) ) ;
#35672 = CARTESIAN_POINT ( 'NONE',  ( -0.9227428731364130110, 21.52761613755500036, -9.384612575603730633 ) ) ;
#35674 = CARTESIAN_POINT ( 'NONE',  ( 63.43729419656740731, 1.382840740411490188, -68.63401718432778864 ) ) ;
#35675 = CARTESIAN_POINT ( 'NONE',  ( 61.25410332236540256, 14.01664428061980061, -46.70604314720559813 ) ) ;
#35676 = CARTESIAN_POINT ( 'NONE',  ( 44.13393739769620083, -33.11618894467940066, -54.35294145922159714 ) ) ;
#35677 = CARTESIAN_POINT ( 'NONE',  ( 72.13393739769620083, -1.116188944679340045, -20.65000000000000213 ) ) ;
#35678 = EDGE_LOOP ( 'NONE', ( #42421, #14143, #7278, #42033, #19348, #31485 ) ) ;
#35679 = CARTESIAN_POINT ( 'NONE',  ( 52.79916199400859966, -49.67749117070789566, -48.53936745044679668 ) ) ;
#35680 = CARTESIAN_POINT ( 'NONE',  ( 59.90835834505130464, -45.34291689336190245, -26.75034159233819864 ) ) ;
#35681 = CARTESIAN_POINT ( 'NONE',  ( 4.133937397696209715, -22.54439217495480108, -35.14999999999999858 ) ) ;
#35682 = CARTESIAN_POINT ( 'NONE',  ( 61.50409964634459925, -45.37406455498979341, -47.35437808299670337 ) ) ;
#35683 = CARTESIAN_POINT ( 'NONE',  ( 8.773421182200600299, -14.46315171779890107, -73.28211911255840505 ) ) ;
#35684 = CARTESIAN_POINT ( 'NONE',  ( 52.11372286138289667, 18.47999854749260251, -77.07264542598700530 ) ) ;
#35685 = CARTESIAN_POINT ( 'NONE',  ( 53.13753015649290035, 18.27140341915590227, -48.89206902239920538 ) ) ;
#35686 = CARTESIAN_POINT ( 'NONE',  ( -14.86606260230379917, -15.61618894467929941, -20.15000000000000213 ) ) ;
#35687 = DIRECTION ( 'NONE',  ( 1.000000000000000000, 0.000000000000000000, 0.000000000000000000 ) ) ;
#35688 = VERTEX_POINT ( 'NONE', #39081 ) ;
#35689 = CARTESIAN_POINT ( 'NONE',  ( 22.89855976872829046, -15.80993452990232129, -40.46193658699167628 ) ) ;
#35690 = EDGE_CURVE ( 'NONE', #42806, #31006, #34865, .T. ) ;
#35691 = CARTESIAN_POINT ( 'NONE',  ( 47.69847251993340365, -54.50500465509079362, -55.01789699801200584 ) ) ;
#35692 = CARTESIAN_POINT ( 'NONE',  ( 9.807754884354935143, -10.75453309769691757, -37.00066549356353818 ) ) ;
#35693 = CARTESIAN_POINT ( 'NONE',  ( 10.47081843707173299, 11.49830782136799634, -84.65000000000000568 ) ) ;
#35694 = CARTESIAN_POINT ( 'NONE',  ( 60.83822960227499976, -30.17641036977770241, -16.10447917479509883 ) ) ;
#35695 = CARTESIAN_POINT ( 'NONE',  ( 71.40678801050209756, 1.186856010528209993, -60.73114026433219692 ) ) ;
#35696 = CARTESIAN_POINT ( 'NONE',  ( -8.191285341990415247, -39.36383343069419993, -41.88932412146674267 ) ) ;
#35697 = CARTESIAN_POINT ( 'NONE',  ( 72.61552859537209770, 1.010053820890850051, -61.65938070570050655 ) ) ;
#35698 = CARTESIAN_POINT ( 'NONE',  ( 68.13393739769630031, -48.11618894467697061, -70.54999999999976978 ) ) ;
#35699 = AXIS2_PLACEMENT_3D ( 'NONE', #29982, #46006, #34441 ) ;
#35700 = CARTESIAN_POINT ( 'NONE',  ( 60.90240720208950620, -45.28704519797054928, -27.40842581354857188 ) ) ;
#35701 = ORIENTED_EDGE ( 'NONE', *, *, #30369, .T. ) ;
#35702 = ORIENTED_EDGE ( 'NONE', *, *, #33163, .T. ) ;
#35703 = DIRECTION ( 'NONE',  ( 0.000000000000000000, -1.000000000000000000, 0.000000000000000000 ) ) ;
#35704 = CARTESIAN_POINT ( 'NONE',  ( 49.87066309494894512, -29.65878804270703029, -15.89390192910206068 ) ) ;
#35705 = VERTEX_POINT ( 'NONE', #31177 ) ;
#35706 = DIRECTION ( 'NONE',  ( 0.000000000000000000, 0.000000000000000000, 1.000000000000000000 ) ) ;
#35707 = CARTESIAN_POINT ( 'NONE',  ( 21.72379952060926911, -21.21416803257280037, -77.75789285207679313 ) ) ;
#35708 = ORIENTED_EDGE ( 'NONE', *, *, #15093, .F. ) ;
#35709 = DIRECTION ( 'NONE',  ( 0.000000000000000000, 0.000000000000000000, 1.000000000000000000 ) ) ;
#35710 = CARTESIAN_POINT ( 'NONE',  ( 44.06836400025156308, 6.694124833047266243, -69.97780465984523346 ) ) ;
#35711 = CARTESIAN_POINT ( 'NONE',  ( 63.88393739769619373, 20.38443354211860026, -61.34712802272770915 ) ) ;
#35712 = CARTESIAN_POINT ( 'NONE',  ( 18.18491397528629960, -7.630187746700939577, -43.37235095159000053 ) ) ;
#35713 = AXIS2_PLACEMENT_3D ( 'NONE', #49342, #1626, #38306 ) ;
#35714 = CARTESIAN_POINT ( 'NONE',  ( 23.08393739769629960, -15.61618894467929941, -20.74999999999999289 ) ) ;
#35715 = CARTESIAN_POINT ( 'NONE',  ( 24.04488077751907582, -15.64853513552632513, -49.79363160827950452 ) ) ;
#35716 = CARTESIAN_POINT ( 'NONE',  ( 64.76670119014970339, -29.83072655109479854, -16.45448121326970181 ) ) ;
#35717 = CARTESIAN_POINT ( 'NONE',  ( 14.34417029195965476, 19.88381105532280557, -74.33587756533812296 ) ) ;
#35718 = CARTESIAN_POINT ( 'NONE',  ( 11.65110190134180002, -22.05753457305690191, -76.70602703883379547 ) ) ;
#35719 = CARTESIAN_POINT ( 'NONE',  ( 55.65311171412380276, 14.73495305830999946, -16.92919767242679896 ) ) ;
#35720 = CARTESIAN_POINT ( 'NONE',  ( 41.13178742825800072, 13.81684675789199979, -5.658924883871920386 ) ) ;
#35721 = ADVANCED_FACE ( 'NONE', ( #47207 ), #2136, .T. ) ;
#35722 = CARTESIAN_POINT ( 'NONE',  ( 9.446663254046249847, 23.82152373690511382, -46.46212477756636616 ) ) ;
#35723 = ADVANCED_FACE ( 'NONE', ( #14958 ), #27256, .T. ) ;
#35724 = CARTESIAN_POINT ( 'NONE',  ( 83.99291904213089310, -44.37437668906760280, -47.15152633430140838 ) ) ;
#35725 = CIRCLE ( 'NONE', #22314, 16.00000000000000000 ) ;
#35726 = FACE_OUTER_BOUND ( 'NONE', #47895, .T. ) ;
#35727 = ADVANCED_FACE ( 'NONE', ( #51128 ), #43939, .F. ) ;
#35728 = CARTESIAN_POINT ( 'NONE',  ( 23.25356989242479955, -11.45763705141400202, -41.33939600337990328 ) ) ;
#35729 = ORIENTED_EDGE ( 'NONE', *, *, #28140, .T. ) ;
#35730 = DIRECTION ( 'NONE',  ( 0.000000000000000000, -1.000000000000000000, 0.000000000000000000 ) ) ;
#35731 = CARTESIAN_POINT ( 'NONE',  ( 12.13729495418210114, -65.03660448042120379, -16.30611525569679898 ) ) ;
#35732 = CARTESIAN_POINT ( 'NONE',  ( 50.93875529876952868, -35.32972334367127587, -76.36830481639776735 ) ) ;
#35733 = CARTESIAN_POINT ( 'NONE',  ( 61.75019934789347076, -45.11618894468048779, -46.51053312274786578 ) ) ;
#35734 = DIRECTION ( 'NONE',  ( 1.000000000000000000, 0.000000000000000000, 0.000000000000000000 ) ) ;
#35735 = VERTEX_POINT ( 'NONE', #35120 ) ;
#35736 = CARTESIAN_POINT ( 'NONE',  ( -5.675882129932829478, -46.90160876882899998, -5.248560459082940000 ) ) ;
#35737 = CARTESIAN_POINT ( 'NONE',  ( 47.18324198357279897, 23.57489020266570279, -54.61058319554400242 ) ) ;
#35738 = AXIS2_PLACEMENT_3D ( 'NONE', #15642, #31595, #38983 ) ;
#35739 = CARTESIAN_POINT ( 'NONE',  ( 20.29261426253945899, -21.02750317140192493, -48.74448829848160614 ) ) ;
#35740 = CARTESIAN_POINT ( 'NONE',  ( 63.31614497232158811, 1.328073773609210084, -62.51929651814780442 ) ) ;
#35741 = CARTESIAN_POINT ( 'NONE',  ( 57.55751162054249903, -50.55753267974190379, -53.43780795143099738 ) ) ;
#35742 = CARTESIAN_POINT ( 'NONE',  ( 42.88515050839449572, 12.54233113675140032, -4.897272209574110136 ) ) ;
#35743 = LINE ( 'NONE', #868, #28385 ) ;
#35744 = CARTESIAN_POINT ( 'NONE',  ( 64.14331810339589879, 1.010053820890960186, -61.16840880232479805 ) ) ;
#35745 = CARTESIAN_POINT ( 'NONE',  ( 53.87565362894249432, -49.13748779640440034, -48.87968056552790586 ) ) ;
#35746 = CARTESIAN_POINT ( 'NONE',  ( 15.09829013782090179, -7.705200998933884549, -75.25071684570102093 ) ) ;
#35747 = CARTESIAN_POINT ( 'NONE',  ( 66.54986620728139712, -1.029621168181320101, -16.95609984218899768 ) ) ;
#35748 = CARTESIAN_POINT ( 'NONE',  ( 17.58070283336819983, -52.47980496485550361, -76.04476946176040997 ) ) ;
#35749 = EDGE_CURVE ( 'NONE', #17972, #18282, #42957, .T. ) ;
#35750 = CARTESIAN_POINT ( 'NONE',  ( 22.82027184960839961, -12.32991051224040113, -62.92193303376410540 ) ) ;
#35751 = CARTESIAN_POINT ( 'NONE',  ( 23.83903868892194211, -13.54551848185154306, -41.42433399449730302 ) ) ;
#35752 = CARTESIAN_POINT ( 'NONE',  ( 55.02371555901009970, -47.79053722659219972, -47.27949281187280661 ) ) ;
#35753 = ORIENTED_EDGE ( 'NONE', *, *, #37023, .T. ) ;
#35754 = CARTESIAN_POINT ( 'NONE',  ( 16.13393739769620083, -15.61618894467929941, -35.14999999999999858 ) ) ;
#35755 = CARTESIAN_POINT ( 'NONE',  ( 9.366924169342379258, -16.21927461595470987, -35.42444116589499004 ) ) ;
#35756 = CARTESIAN_POINT ( 'NONE',  ( 72.78346131865960444, 1.386342629514219826, -68.66646381051069170 ) ) ;
#35757 = CARTESIAN_POINT ( 'NONE',  ( -10.90401617485185604, -41.47682395427644764, -20.56421356237309439 ) ) ;
#35758 = CARTESIAN_POINT ( 'NONE',  ( 10.56495154625470079, -10.52090938289240007, -81.23899999999999011 ) ) ;
#35759 = ORIENTED_EDGE ( 'NONE', *, *, #34344, .F. ) ;
#35760 = CARTESIAN_POINT ( 'NONE',  ( 17.34361748118760005, 21.51730579194029858, -76.12465403027070465 ) ) ;
#35761 = ORIENTED_EDGE ( 'NONE', *, *, #41504, .F. ) ;
#35762 = VERTEX_POINT ( 'NONE', #43270 ) ;
#35763 = CARTESIAN_POINT ( 'NONE',  ( 57.07404348378830861, -45.88224062731829633, -26.24937804946210207 ) ) ;
#35764 = CARTESIAN_POINT ( 'NONE',  ( 22.28740654554379930, -10.80186921573359982, -81.23899999999999011 ) ) ;
#35765 =( BOUNDED_SURFACE ( )  B_SPLINE_SURFACE ( 2, 2, ( 
 ( #14797, #47303, #27101, #27355, #35221, #38660, #15318, #43361, #23406 ),
 ( #22897, #39427, #2748, #19497, #46785, #42849, #42325, #10874, #50448 ),
 ( #6425, #22382, #38387, #2484, #14535, #30505, #46529, #26572, #42586 ),
 ( #22643, #26839, #3005, #32294, #40706, #605, #35487, #44124, #4036 ),
 ( #48062, #4804, #15823, #15578, #4283, #51479, #27612, #16338, #44635 ) ),
 .UNSPECIFIED., .F., .T., .T. ) 
 B_SPLINE_SURFACE_WITH_KNOTS ( ( 3, 2, 3 ),
 ( 3, 2, 2, 2, 3 ),
 ( -0.003205554299145560102, 0.8238407534178779912, 1.650887061134900025 ),
 ( -3.141592653589790007, -1.570796326794899889, 0.000000000000000000, 1.570796326794899889, 3.141592653589790007 ),
 .UNSPECIFIED. ) 
 GEOMETRIC_REPRESENTATION_ITEM ( )  RATIONAL_B_SPLINE_SURFACE ( (
 ( 1.000000000000000000, 0.7071067811865480168, 1.000000000000000000, 0.7071067811865480168, 1.000000000000000000, 0.7071067811865480168, 1.000000000000000000, 0.7071067811865480168, 1.000000000000000000),
 ( 0.9157107718028779653, 0.6475052963473819645, 0.9157107718028779653, 0.6475052963473819645, 0.9157107718028779653, 0.6475052963473819645, 0.9157107718028779653, 0.6475052963473819645, 0.9157107718028779653),
 ( 1.000000000000000000, 0.7071067811865480168, 1.000000000000000000, 0.7071067811865480168, 1.000000000000000000, 0.7071067811865480168, 1.000000000000000000, 0.7071067811865480168, 1.000000000000000000),
 ( 0.9157107718028449916, 0.6475052963473589829, 0.9157107718028449916, 0.6475052963473589829, 0.9157107718028449916, 0.6475052963473589829, 0.9157107718028449916, 0.6475052963473589829, 0.9157107718028449916),
 ( 1.000000000000000000, 0.7071067811865480168, 1.000000000000000000, 0.7071067811865480168, 1.000000000000000000, 0.7071067811865480168, 1.000000000000000000, 0.7071067811865480168, 1.000000000000000000) ) ) 
 REPRESENTATION_ITEM ( '' )  SURFACE ( )  );
#35766 = CARTESIAN_POINT ( 'NONE',  ( 8.222937397696199469, -15.61618894467929941, -32.14999999999999858 ) ) ;
#35767 = B_SPLINE_CURVE_WITH_KNOTS ( 'NONE', 3,
 ( #23915, #12162, #31533, #31788, #47551, #20254, #11647, #43618, #48315, #8740, #12411, #19996 ),
 .UNSPECIFIED., .F., .F.,
 ( 4, 2, 2, 2, 1, 1, 4 ),
 ( 0.000000000000000000, 0.5000000000000769385, 0.5625000000000804912, 0.5937500000000822675, 0.6250000000000840439, 0.7500000000000469624, 1.000000000000000000 ),
 .UNSPECIFIED. ) ;
#35768 = EDGE_CURVE ( 'NONE', #51745, #51329, #22290, .T. ) ;
#35769 = ORIENTED_EDGE ( 'NONE', *, *, #23403, .F. ) ;
#35770 = FACE_OUTER_BOUND ( 'NONE', #1085, .T. ) ;
#35771 = ORIENTED_EDGE ( 'NONE', *, *, #21820, .F. ) ;
#35772 = CARTESIAN_POINT ( 'NONE',  ( 9.807814359748768140, -10.75445678515254855, -63.00066530372220797 ) ) ;
#35773 = CARTESIAN_POINT ( 'NONE',  ( 83.95017420394412966, 13.51629706050414370, -47.46180916972096497 ) ) ;
#35774 = ORIENTED_EDGE ( 'NONE', *, *, #50275, .F. ) ;
#35775 = EDGE_LOOP ( 'NONE', ( #3601, #33164, #15634, #33483 ) ) ;
#35776 = CARTESIAN_POINT ( 'NONE',  ( 44.73223296007571292, 1.943966071894212222, -43.46537174154696004 ) ) ;
#35777 = CARTESIAN_POINT ( 'NONE',  ( 16.13393739769620083, -15.61618894467929941, 6.789625226207629538 ) ) ;
#35778 = CARTESIAN_POINT ( 'NONE',  ( 61.28822732917949878, 14.34385274781909914, -47.65091293713199860 ) ) ;
#35779 = AXIS2_PLACEMENT_3D ( 'NONE', #10692, #3089, #23481 ) ;
#35780 = CARTESIAN_POINT ( 'NONE',  ( 65.03603135424580728, -1.463538230407920082, -19.52361391316370032 ) ) ;
#35781 = DIRECTION ( 'NONE',  ( -2.840828347717470042E-11, 6.470619327693540153E-12, 1.000000000000000000 ) ) ;
#35782 = CARTESIAN_POINT ( 'NONE',  ( -7.622325105801039946, 14.20602405906790011, -5.644196242347629955 ) ) ;
#35783 = FACE_OUTER_BOUND ( 'NONE', #22858, .T. ) ;
#35784 = LINE ( 'NONE', #26614, #8860 ) ;
#35785 = EDGE_CURVE ( 'NONE', #11209, #34917, #42266, .T. ) ;
#35786 = CARTESIAN_POINT ( 'NONE',  ( 12.35809383743469958, -8.736526627994370742, -66.62772890321430452 ) ) ;
#35787 = ORIENTED_EDGE ( 'NONE', *, *, #36862, .F. ) ;
#35788 = CARTESIAN_POINT ( 'NONE',  ( 71.83406239764909174, 11.38381102407070067, -62.44999999999999574 ) ) ;
#35789 = CARTESIAN_POINT ( 'NONE',  ( 42.14447631745849776, 14.59219016048480100, -6.935681727894889015 ) ) ;
#35790 = CARTESIAN_POINT ( 'NONE',  ( 12.96406378549919935, 34.28324915656980210, -47.66759396750580180 ) ) ;
#35791 = PRODUCT_DEFINITION_CONTEXT ( 'detailed design', #4024, 'design' ) ;
#35792 = CARTESIAN_POINT ( 'NONE',  ( 72.16319864705920395, 1.346167254499869959, -69.94520975977049204 ) ) ;
#35793 = CARTESIAN_POINT ( 'NONE',  ( 43.64323166376460961, -39.92453440565081024, -68.38731717000798938 ) ) ;
#35794 = CARTESIAN_POINT ( 'NONE',  ( 14.63393739769630031, 1.354373803797940035, -35.14999999999999858 ) ) ;
#35795 = DIRECTION ( 'NONE',  ( 1.000000000000000000, 0.000000000000000000, 0.000000000000000000 ) ) ;
#35796 = CARTESIAN_POINT ( 'NONE',  ( 63.27438507250460020, 1.187296498006439993, -69.02170307486190381 ) ) ;
#35797 = CARTESIAN_POINT ( 'NONE',  ( 48.29537619369070001, -54.13523159704990206, -54.65524445810709864 ) ) ;
#35798 = CARTESIAN_POINT ( 'NONE',  ( 51.92090233143009215, -32.82639329994397315, -18.96879582027110800 ) ) ;
#35799 = CARTESIAN_POINT ( 'NONE',  ( 58.92073396209919878, -3.116188944679349593, -15.65000000000000036 ) ) ;
#35800 = B_SPLINE_CURVE_WITH_KNOTS ( 'NONE', 3,
 ( #39076, #35379, #22798, #47707, #3167, #3427, #51632, #34861, #50861, #11290, #27251, #43265, #7354, #39579, #15988, #14954, #19399, #15727 ),
 .UNSPECIFIED., .F., .F.,
 ( 4, 2, 2, 2, 2, 2, 2, 2, 4 ),
 ( 0.000000000000000000, 0.01645396295165469855, 0.1775000000000971079, 0.3375000000000846212, 0.4375000000000769385, 0.5000000000000713873, 0.6250000000000630607, 0.7632212076873368112, 1.000000000000000000 ),
 .UNSPECIFIED. ) ;
#35801 = CARTESIAN_POINT ( 'NONE',  ( 47.75420808716030052, 23.23832663738040338, -54.93836825444449801 ) ) ;
#35802 = ORIENTED_EDGE ( 'NONE', *, *, #40971, .T. ) ;
#35803 = CARTESIAN_POINT ( 'NONE',  ( 22.99024908015519841, -18.53126775147510230, -35.19530716149729699 ) ) ;
#35804 = CARTESIAN_POINT ( 'NONE',  ( 64.60023990589328946, 0.9543424661148549593, -60.80063435388460391 ) ) ;
#35805 = ORIENTED_EDGE ( 'NONE', *, *, #35399, .T. ) ;
#35806 = CARTESIAN_POINT ( 'NONE',  ( 71.62124566564099837, 0.9425424353906030062, -70.53248918539379986 ) ) ;
#35807 = CARTESIAN_POINT ( 'NONE',  ( 60.72309646253260240, -45.59317018174599667, -47.46061744060280319 ) ) ;
#35808 = CARTESIAN_POINT ( 'NONE',  ( 47.83393063578103011, -54.38673743207323241, -54.71871010756845521 ) ) ;
#35809 = AXIS2_PLACEMENT_3D ( 'NONE', #35850, #23775, #16189 ) ;
#35810 = CARTESIAN_POINT ( 'NONE',  ( 64.64302830678670375, 0.9098571636355720083, -60.77008670988870165 ) ) ;
#35812 = CARTESIAN_POINT ( 'NONE',  ( 16.13393739769620083, -15.61618894467929941, 7.530187386896120216 ) ) ;
#35811 = CARTESIAN_POINT ( 'NONE',  ( 41.11789956691032444, 8.431943849971739624, -80.58643109008846750 ) ) ;
#35813 = ORIENTED_EDGE ( 'NONE', *, *, #22969, .F. ) ;
#35814 = CARTESIAN_POINT ( 'NONE',  ( 44.07452568954059302, 1.883811055320659955, -54.64999999999999858 ) ) ;
#35815 = VERTEX_POINT ( 'NONE', #2658 ) ;
#35816 = CIRCLE ( 'NONE', #30753, 33.00000000000000000 ) ;
#35817 = VERTEX_POINT ( 'NONE', #50609 ) ;
#35818 = CARTESIAN_POINT ( 'NONE',  ( 53.63393739769619373, -53.11618894467930119, 17.35000000000000142 ) ) ;
#35819 = CARTESIAN_POINT ( 'NONE',  ( 52.27429601900837497, -49.79159170706056159, -77.19751337257605428 ) ) ;
#35820 = CARTESIAN_POINT ( 'NONE',  ( 76.60309355059160907, -33.99212704518571826, -13.67166368881104965 ) ) ;
#35821 = ORIENTED_EDGE ( 'NONE', *, *, #16851, .T. ) ;
#35822 = EDGE_CURVE ( 'NONE', #14168, #5719, #18883, .T. ) ;
#35823 = VERTEX_POINT ( 'NONE', #10524 ) ;
#35824 = CARTESIAN_POINT ( 'NONE',  ( -0.1397480543147154586, 14.29295295954979927, -34.88775788892196061 ) ) ;
#35825 = CARTESIAN_POINT ( 'NONE',  ( 16.13393739769620083, -15.61618894467929941, -35.02873218748179340 ) ) ;
#35826 = ADVANCED_FACE ( 'NONE', ( #18627 ), #26737, .T. ) ;
#35827 = CYLINDRICAL_SURFACE ( 'NONE', #16961, 7.910999999999997812 ) ;
#35828 = CARTESIAN_POINT ( 'NONE',  ( 10.06369629474122185, 22.76024865223496363, -34.79644414665609986 ) ) ;
#35829 = CARTESIAN_POINT ( 'NONE',  ( 62.05917851177209599, -0.7776122089247741176, -16.28509574527020121 ) ) ;
#35830 = CARTESIAN_POINT ( 'NONE',  ( 51.50420586855599936, -49.40990438562260323, -76.63112831509690182 ) ) ;
#35831 = EDGE_CURVE ( 'NONE', #49915, #46911, #13795, .T. ) ;
#35832 = ORIENTED_EDGE ( 'NONE', *, *, #30989, .F. ) ;
#35833 = CARTESIAN_POINT ( 'NONE',  ( 8.643872352929088620, -48.75656286698969666, -35.12503119152809461 ) ) ;
#35834 = PLANE ( 'NONE',  #1654 ) ;
#35835 = CARTESIAN_POINT ( 'NONE',  ( 60.30540951500742608, 14.59285682385894845, -47.61343627861142380 ) ) ;
#35836 = DIRECTION ( 'NONE',  ( 0.000000000000000000, 0.000000000000000000, 1.000000000000000000 ) ) ;
#35837 = CARTESIAN_POINT ( 'NONE',  ( 14.71722765695869839, -7.897401403745059945, -49.45471475294879582 ) ) ;
#35838 = CARTESIAN_POINT ( 'NONE',  ( 17.98749078828947745, -41.76263555408611694, -34.79644660940672907 ) ) ;
#35839 = DIRECTION ( 'NONE',  ( -0.2260571801428170324, 0.000000000000000000, 0.9741140340359940586 ) ) ;
#35840 = CARTESIAN_POINT ( 'NONE',  ( 70.83393739769719843, -48.11618894467220287, -73.25000000000000000 ) ) ;
#35841 = CARTESIAN_POINT ( 'NONE',  ( 16.15069456443690044, 19.81939336389048734, -17.90311212357439885 ) ) ;
#35842 = CARTESIAN_POINT ( 'NONE',  ( 22.90095859539430379, -15.61618916398383661, -38.45281773784812174 ) ) ;
#35843 = AXIS2_PLACEMENT_3D ( 'NONE', #47637, #51315, #48147 ) ;
#35844 = CARTESIAN_POINT ( 'NONE',  ( 20.53618552854030099, -10.10594661162980046, -52.56174695496989102 ) ) ;
#35845 = CARTESIAN_POINT ( 'NONE',  ( 46.56799392459599574, -40.00405894838129939, -54.63041858883969581 ) ) ;
#35846 = EDGE_CURVE ( 'NONE', #12246, #13362, #35421, .T. ) ;
#35847 = VERTEX_POINT ( 'NONE', #27777 ) ;
#35848 = LINE ( 'NONE', #35331, #23797 ) ;
#35849 = CARTESIAN_POINT ( 'NONE',  ( 47.24353709908209709, -54.76064543437800580, -54.64904795778859636 ) ) ;
#35850 = CARTESIAN_POINT ( 'NONE',  ( 68.13393739769618662, -31.81618894467930403, -65.65000000000000568 ) ) ;
#35851 = CARTESIAN_POINT ( 'NONE',  ( 0.3198708682049009600, 19.48717932910869877, -34.64999999999999858 ) ) ;
#35852 = CARTESIAN_POINT ( 'NONE',  ( 17.78608069253172275, 20.27135663923038678, -75.33783710294622438 ) ) ;
#35853 = CARTESIAN_POINT ( 'NONE',  ( 15.54400293349995543, -50.81696016472969291, -20.39351698354824549 ) ) ;
#35854 = CARTESIAN_POINT ( 'NONE',  ( 8.513496274260603514, -13.18580911493815933, -54.60561559637670115 ) ) ;
#35855 = CARTESIAN_POINT ( 'NONE',  ( 19.54188148977384643, -9.703249216854988646, -76.11946519189100968 ) ) ;
#35856 = CARTESIAN_POINT ( 'NONE',  ( 10.66246720353709954, 33.63422984119760173, -18.01843150758180201 ) ) ;
#35857 = CARTESIAN_POINT ( 'NONE',  ( 10.43817627109141277, -10.06373200202189899, -64.75374759500355992 ) ) ;
#35859 = CARTESIAN_POINT ( 'NONE',  ( 13.43643019722925303, -51.25329737159583487, -22.14276204152384508 ) ) ;
#35858 = DIRECTION ( 'NONE',  ( -1.000000000000000000, 0.000000000000000000, 0.000000000000000000 ) ) ;
#35860 = DIRECTION ( 'NONE',  ( 2.812429781167509836E-09, -3.628863640055339935E-09, 1.000000000000000000 ) ) ;
#35861 = CARTESIAN_POINT ( 'NONE',  ( 49.07389894158890087, 22.56707546824529942, -54.57361176007880488 ) ) ;
#35862 = ORIENTED_EDGE ( 'NONE', *, *, #40516, .F. ) ;
#35863 = CARTESIAN_POINT ( 'NONE',  ( 52.62463376634079992, -49.80324691087879785, -48.47378032971909789 ) ) ;
#35864 = EDGE_LOOP ( 'NONE', ( #38665, #7363, #35813, #24177, #14693, #35805, #17799 ) ) ;
#35865 = CARTESIAN_POINT ( 'NONE',  ( 46.43281365467359478, 6.703450485939987047, -58.09721321091641499 ) ) ;
#35866 = CYLINDRICAL_SURFACE ( 'NONE', #8501, 2.000000000000001776 ) ;
#35867 = CARTESIAN_POINT ( 'NONE',  ( 11.89321892211240161, 34.20364954171930094, -18.17421237891140251 ) ) ;
#35868 = CARTESIAN_POINT ( 'NONE',  ( 83.11128256222379207, 13.68219656570800069, -46.57919617705099569 ) ) ;
#35869 = CARTESIAN_POINT ( 'NONE',  ( 11.46379677190219937, -20.90129492582429904, -57.18318221610359586 ) ) ;
#35870 = CARTESIAN_POINT ( 'NONE',  ( 8.223148984577919762, -15.61599292915740023, -40.79233150823699816 ) ) ;
#35871 = CARTESIAN_POINT ( 'NONE',  ( 56.39638450836229566, -45.38884808781619995, -17.16969890501229656 ) ) ;
#35872 = CARTESIAN_POINT ( 'NONE',  ( 54.11082558918479890, 16.90719386950179626, -26.08329795554919883 ) ) ;
#35873 = ORIENTED_EDGE ( 'NONE', *, *, #39466, .T. ) ;
#35874 = CARTESIAN_POINT ( 'NONE',  ( 23.97713974386040192, -15.88250668781109809, -47.29830972369129682 ) ) ;
#35875 = ORIENTED_EDGE ( 'NONE', *, *, #27849, .T. ) ;
#35876 = CARTESIAN_POINT ( 'NONE',  ( 12.01336146540229954, -65.33303523161541193, -17.10865960907919714 ) ) ;
#35877 = CARTESIAN_POINT ( 'NONE',  ( 11.81672205559790179, 34.07977438613860244, -47.29989710098740119 ) ) ;
#35878 = CARTESIAN_POINT ( 'NONE',  ( 73.11690592692660573, 0.8925687589132640376, -62.30780775221820278 ) ) ;
#35879 = CARTESIAN_POINT ( 'NONE',  ( 20.99557161890594514, -21.94238916341829082, -40.08401076356010861 ) ) ;
#35880 = CARTESIAN_POINT ( 'NONE',  ( 8.801404170410069838, 31.97031994814190270, -46.67014817202279886 ) ) ;
#35881 = CARTESIAN_POINT ( 'NONE',  ( 10.80839229981719818, 21.91123435898759908, -23.15000000000000213 ) ) ;
#35882 = CIRCLE ( 'NONE', #32516, 6.999999999999999112 ) ;
#35883 = AXIS2_PLACEMENT_3D ( 'NONE', #16486, #32970, #20662 ) ;
#35884 = VERTEX_POINT ( 'NONE', #32198 ) ;
#35885 = CARTESIAN_POINT ( 'NONE',  ( 13.61938558349279305, 20.19483563131725035, -22.88820058412975555 ) ) ;
#35886 = CARTESIAN_POINT ( 'NONE',  ( 11.10535958650110011, -63.15872092784729830, -44.25018693357320387 ) ) ;
#35887 = EDGE_CURVE ( 'NONE', #8473, #33996, #32155, .T. ) ;
#35888 = CARTESIAN_POINT ( 'NONE',  ( 68.13393739769706769, 17.98087126524489321, -74.20351669811762463 ) ) ;
#35889 = ORIENTED_EDGE ( 'NONE', *, *, #48865, .T. ) ;
#35890 = CARTESIAN_POINT ( 'NONE',  ( 11.18784974601570781, -64.00854372606637810, -43.96560395573440871 ) ) ;
#35891 = CARTESIAN_POINT ( 'NONE',  ( 56.56050783432609563, 19.48343119352850294, -53.48830978460669883 ) ) ;
#35892 = FACE_OUTER_BOUND ( 'NONE', #30321, .T. ) ;
#35893 = ADVANCED_FACE ( 'NONE', ( #7624 ), #24336, .T. ) ;
#35894 = CARTESIAN_POINT ( 'NONE',  ( 16.13393739769620083, -15.61618894467929941, -35.14999999999999858 ) ) ;
#35895 = ORIENTED_EDGE ( 'NONE', *, *, #14353, .F. ) ;
#35896 = PRESENTATION_STYLE_ASSIGNMENT (( #43765 ) ) ;
#35897 = CARTESIAN_POINT ( 'NONE',  ( 52.82975622904289992, 18.42854261028849905, -48.47378032971769812 ) ) ;
#35898 = DIRECTION ( 'NONE',  ( 0.000000000000000000, 0.000000000000000000, -1.000000000000000000 ) ) ;
#35899 = CARTESIAN_POINT ( 'NONE',  ( 2.422700639432790126, -25.82238555492689969, -35.02127583263639821 ) ) ;
#35900 = CARTESIAN_POINT ( 'NONE',  ( 14.23508833078220093, -7.592655291916660332, -75.21836123916510530 ) ) ;
#35901 = CARTESIAN_POINT ( 'NONE',  ( 21.45406565774166197, -10.98598436268488143, -38.61921508777308532 ) ) ;
#35902 = CARTESIAN_POINT ( 'NONE',  ( 46.00717017453583679, -38.15421180662563216, -60.28378775688172198 ) ) ;
#35903 = ORIENTED_EDGE ( 'NONE', *, *, #33100, .T. ) ;
#35904 = CARTESIAN_POINT ( 'NONE',  ( 10.84925596614229981, -20.86774452109049705, -62.98365807428779561 ) ) ;
#35905 = DIRECTION ( 'NONE',  ( 0.5835456732599438867, -0.8120803206700667465, 0.000000000000000000 ) ) ;
#35906 = CARTESIAN_POINT ( 'NONE',  ( 9.901323237974340330, -20.02052287148769949, -32.14999999999999858 ) ) ;
#35907 = EDGE_CURVE ( 'NONE', #23424, #24662, #21325, .T. ) ;
#35908 = CARTESIAN_POINT ( 'NONE',  ( 47.37032927764419554, 23.44277963338160120, -74.14999585054489728 ) ) ;
#35909 = EDGE_CURVE ( 'NONE', #39386, #667, #12882, .T. ) ;
#35910 = CARTESIAN_POINT ( 'NONE',  ( 71.15040120820690106, 1.386342629514219826, -61.00047607903670155 ) ) ;
#35911 = PLANE ( 'NONE',  #13863 ) ;
#35912 = CIRCLE ( 'NONE', #13340, 1.500000000000001332 ) ;
#35913 = CARTESIAN_POINT ( 'NONE',  ( 11.97330428935280011, 33.54929834488839901, -16.08313759590789971 ) ) ;
#35915 = CIRCLE ( 'NONE', #51000, 5.499999999999998224 ) ;
#35914 = CARTESIAN_POINT ( 'NONE',  ( 11.54117676686140115, -22.46376300392310199, -76.19572567137230124 ) ) ;
#35916 = CARTESIAN_POINT ( 'NONE',  ( 56.14177628828820588, -50.61618684426799319, -75.89576364164580013 ) ) ;
#35918 = DIRECTION ( 'NONE',  ( -0.2260571801428090388, -1.168509733417976470E-14, 0.9741140340359961680 ) ) ;
#35917 = CARTESIAN_POINT ( 'NONE',  ( 57.45269164250755267, 19.38381105532069881, -53.92796674552833736 ) ) ;
#35919 = CARTESIAN_POINT ( 'NONE',  ( 63.20675433611359750, 1.270877794983130027, -68.75550371754310675 ) ) ;
#35920 = CARTESIAN_POINT ( 'NONE',  ( 61.36488470523620009, 14.00771087096500089, -46.95107575060279714 ) ) ;
#35921 = DIRECTION ( 'NONE',  ( -1.451273000000000212E-17, 7.532081000000000189E-18, -1.000000000000000000 ) ) ;
#35922 = ORIENTED_EDGE ( 'NONE', *, *, #4774, .F. ) ;
#35923 = CARTESIAN_POINT ( 'NONE',  ( 52.81415492500530462, -49.66954405245009951, -48.60515561007039764 ) ) ;
#35924 = CARTESIAN_POINT ( 'NONE',  ( 57.60436885384490324, -45.58916000359799625, -26.22003782303439934 ) ) ;
#35925 = CARTESIAN_POINT ( 'NONE',  ( 8.933902816692604887, -18.95954763342607308, -66.65399573834119451 ) ) ;
#35926 = CARTESIAN_POINT ( 'NONE',  ( 61.34434154007890072, 14.12414198815389810, -47.30220718113330491 ) ) ;
#35927 = CARTESIAN_POINT ( 'NONE',  ( 18.94916917498509790, -22.51409905175449921, -76.60931421723030610 ) ) ;
#35928 = CARTESIAN_POINT ( 'NONE',  ( 51.81521015446629974, 18.95104292838230009, -76.50775191966720001 ) ) ;
#35929 = CARTESIAN_POINT ( 'NONE',  ( 53.45012425301570147, 18.11191960133640322, -48.87690323765099976 ) ) ;
#35930 = CARTESIAN_POINT ( 'NONE',  ( 0.2609591194317602558, -4.650627301100893618, -34.64999999999999858 ) ) ;
#35931 = CARTESIAN_POINT ( 'NONE',  ( 53.00700885799259510, -49.56805288106040308, -48.78176285252619948 ) ) ;
#35932 = ORIENTED_EDGE ( 'NONE', *, *, #50164, .F. ) ;
#35933 = FACE_OUTER_BOUND ( 'NONE', #18355, .T. ) ;
#35934 = CARTESIAN_POINT ( 'NONE',  ( 47.64800064284560221, -54.53209002898449853, -55.13447052885069866 ) ) ;
#35935 = CARTESIAN_POINT ( 'NONE',  ( 38.67452568954060155, -33.99486860111965569, -83.77132034355965118 ) ) ;
#35936 = CARTESIAN_POINT ( 'NONE',  ( 11.97534166513855780, -21.02756618211127204, -71.16115446403824762 ) ) ;
#35937 = CARTESIAN_POINT ( 'NONE',  ( 61.21881494710749649, -30.86421509516850037, -16.47078615167890092 ) ) ;
#35938 = CARTESIAN_POINT ( 'NONE',  ( 71.50903575780739629, 0.9989215084293960878, -60.69776330465320058 ) ) ;
#35939 = CARTESIAN_POINT ( 'NONE',  ( 72.13898961932780196, 1.457833794292699992, -61.50804513633939763 ) ) ;
#35940 = CARTESIAN_POINT ( 'NONE',  ( 51.34657278755454968, -34.59080035391762209, -76.64439721256748328 ) ) ;
#35941 = ORIENTED_EDGE ( 'NONE', *, *, #15977, .T. ) ;
#35942 = CARTESIAN_POINT ( 'NONE',  ( 12.30296576684403931, -10.01166978920420370, -65.76193325973878245 ) ) ;
#35943 = ORIENTED_EDGE ( 'NONE', *, *, #765, .T. ) ;
#35944 = ORIENTED_EDGE ( 'NONE', *, *, #3477, .T. ) ;
#35945 = CARTESIAN_POINT ( 'NONE',  ( 57.27851913721940491, 18.92138913705230152, -52.63313635947250191 ) ) ;
#35946 = ADVANCED_FACE ( 'NONE', ( #40096 ), #19658, .T. ) ;
#35947 = CARTESIAN_POINT ( 'NONE',  ( 51.17464648325179155, -31.65168256193422280, -17.11447666815010749 ) ) ;
#35948 = ORIENTED_EDGE ( 'NONE', *, *, #22386, .T. ) ;
#35949 = CARTESIAN_POINT ( 'NONE',  ( 9.807698685860906096, -10.75460520716508839, -58.71597766615245462 ) ) ;
#35950 = CARTESIAN_POINT ( 'NONE',  ( 11.45435236478304475, -10.68831163810841467, -49.71098155378554395 ) ) ;
#35951 = AXIS2_PLACEMENT_3D ( 'NONE', #15179, #26960, #31137 ) ;
#35952 = VECTOR ( 'NONE', #33570, 1000.000000000000000 ) ;
#35953 = ORIENTED_EDGE ( 'NONE', *, *, #44674, .F. ) ;
#35954 = CARTESIAN_POINT ( 'NONE',  ( 10.63867022051679179, 32.44496671321559234, -23.65473282282058420 ) ) ;
#35955 = AXIS2_PLACEMENT_3D ( 'NONE', #28811, #28287, #4201 ) ;
#35956 = CARTESIAN_POINT ( 'NONE',  ( 17.68664282411139865, 0.9736865341432859866, -34.65032322548090349 ) ) ;
#35957 = CARTESIAN_POINT ( 'NONE',  ( 60.59736966202989805, 14.55571675506389973, -47.75487759591599968 ) ) ;
#35958 = AXIS2_PLACEMENT_3D ( 'NONE', #43360, #27866, #28116 ) ;
#35959 = AXIS2_PLACEMENT_3D ( 'NONE', #45939, #33344, #10028 ) ;
#35960 = CARTESIAN_POINT ( 'NONE',  ( 22.77612783160510190, -10.73110692943910038, -45.59048102137129632 ) ) ;
#35961 = CARTESIAN_POINT ( 'NONE',  ( 23.04646376015080378, -19.60031448718766001, -67.67433282024596508 ) ) ;
#35962 = AXIS2_PLACEMENT_3D ( 'NONE', #46011, #49939, #14546 ) ;
#35963 = CARTESIAN_POINT ( 'NONE',  ( 16.09564338120661020, -23.54783898205173287, -50.29378284779397745 ) ) ;
#35964 = CARTESIAN_POINT ( 'NONE',  ( 61.85129338415519840, -29.25620428968700182, -16.03819528988000087 ) ) ;
#35965 = CARTESIAN_POINT ( 'NONE',  ( 11.01561765541599947, -63.47447192843999630, -24.03168025771979899 ) ) ;
#35966 = CARTESIAN_POINT ( 'NONE',  ( 23.32207194523900284, -13.65725674267400080, -34.14796716713039615 ) ) ;
#35967 = CARTESIAN_POINT ( 'NONE',  ( 43.08932009041299693, 14.67167452393280058, -7.588662368344499143 ) ) ;
#35968 = EDGE_CURVE ( 'NONE', #29219, #5979, #39840, .T. ) ;
#35969 = CARTESIAN_POINT ( 'NONE',  ( 9.875683499728980408, 23.89112191037431998, -46.19193022289812234 ) ) ;
#35970 = CARTESIAN_POINT ( 'NONE',  ( 82.92203328426339226, -45.19260144532690049, -47.12557951548500057 ) ) ;
#35971 = DIRECTION ( 'NONE',  ( 0.000000000000000000, 1.474514954580241538E-14, -1.000000000000000000 ) ) ;
#35972 = CARTESIAN_POINT ( 'NONE',  ( 10.42770386432230012, -21.56779541449689930, -46.25096972932420414 ) ) ;
#35973 = ORIENTED_EDGE ( 'NONE', *, *, #47727, .F. ) ;
#35974 = CARTESIAN_POINT ( 'NONE',  ( 55.38239457922570352, -47.12167877862870569, -26.35045493482720147 ) ) ;
#35975 = CARTESIAN_POINT ( 'NONE',  ( 14.73074138132800037, -50.58571459616789667, -20.78918949795549764 ) ) ;
#35976 = CARTESIAN_POINT ( 'NONE',  ( 19.85413879631180833, -22.62203224873998408, -39.85232524897160289 ) ) ;
#35977 = CARTESIAN_POINT ( 'NONE',  ( 22.24871428180610167, -12.10163878397787407, -56.68113137028124271 ) ) ;
#35978 = FACE_OUTER_BOUND ( 'NONE', #45506, .T. ) ;
#35979 = VECTOR ( 'NONE', #36329, 1000.000000000000000 ) ;
#35980 = EDGE_LOOP ( 'NONE', ( #8881, #39721, #49989, #1119, #26801 ) ) ;
#35981 = AXIS2_PLACEMENT_3D ( 'NONE', #43455, #11232, #31372 ) ;
#35982 = CARTESIAN_POINT ( 'NONE',  ( -2.927826903739159992, -49.19980423205150544, -5.740514721019640554 ) ) ;
#35983 = CIRCLE ( 'NONE', #13424, 23.50000000000000000 ) ;
#35984 = DIRECTION ( 'NONE',  ( 1.000000000000000000, 0.000000000000000000, 0.000000000000000000 ) ) ;
#35986 = AXIS2_PLACEMENT_3D ( 'NONE', #4367, #2194, #38098 ) ;
#35985 = CARTESIAN_POINT ( 'NONE',  ( 19.54197644776506593, -21.52907189293042833, -48.78615488187620741 ) ) ;
#35987 = CARTESIAN_POINT ( 'NONE',  ( 63.07934790479939835, 0.9219904752505979628, -62.41704322431660046 ) ) ;
#35988 = CARTESIAN_POINT ( 'NONE',  ( 57.48162049234600346, -50.51349954334200021, -53.28834583854860085 ) ) ;
#35989 = CARTESIAN_POINT ( 'NONE',  ( 41.60772419834029989, 13.38923699642720067, -5.233302257662570511 ) ) ;
#35990 = CARTESIAN_POINT ( 'NONE',  ( 15.09842764044654118, -7.705184387498995591, -61.25066341985870366 ) ) ;
#35991 = DIRECTION ( 'NONE',  ( 0.000000000000000000, 0.000000000000000000, -1.000000000000000000 ) ) ;
#35992 = CARTESIAN_POINT ( 'NONE',  ( 68.13393739769620083, 0.8838110553206759423, -60.14999999999999858 ) ) ;
#35993 = CARTESIAN_POINT ( 'NONE',  ( 18.20455060651569568, -7.911070096530949058, -75.37571502603971396 ) ) ;
#35994 = CARTESIAN_POINT ( 'NONE',  ( 17.90515954968781287, -22.20706941336631601, -62.86948484627593814 ) ) ;
#35995 = DIRECTION ( 'NONE',  ( 0.000000000000000000, 0.000000000000000000, -1.000000000000000000 ) ) ;
#35996 = CARTESIAN_POINT ( 'NONE',  ( 15.09849723051076253, -7.705175977862010583, -72.96600150002632290 ) ) ;
#35997 = FACE_OUTER_BOUND ( 'NONE', #27238, .T. ) ;
#35998 = ORIENTED_EDGE ( 'NONE', *, *, #35104, .F. ) ;
#35999 = CARTESIAN_POINT ( 'NONE',  ( 8.815605939025839888, 32.05029769251469673, -46.67186391138339729 ) ) ;
#36000 = CARTESIAN_POINT ( 'NONE',  ( 16.13393739769620083, -15.61618894467929941, -34.64999999999999858 ) ) ;
#36001 = CARTESIAN_POINT ( 'NONE',  ( 11.53903724180579893, -9.499211462746920631, -81.23899999999999011 ) ) ;
#36002 = ORIENTED_EDGE ( 'NONE', *, *, #26884, .F. ) ;
#36003 = CARTESIAN_POINT ( 'NONE',  ( 17.32180797866010025, 21.73127465433789851, -76.14999999999999147 ) ) ;
#36004 = ORIENTED_EDGE ( 'NONE', *, *, #28769, .T. ) ;
#36005 = EDGE_LOOP ( 'NONE', ( #15529, #51564, #18644, #5768 ) ) ;
#36006 = ADVANCED_FACE ( 'NONE', ( #19909 ), #16, .T. ) ;
#36007 = VERTEX_POINT ( 'NONE', #31945 ) ;
#36008 = DIRECTION ( 'NONE',  ( 0.000000000000000000, -1.000000000000000000, 0.000000000000000000 ) ) ;
#36009 = CARTESIAN_POINT ( 'NONE',  ( 23.41817524370990000, -13.41780268114560037, -81.23899999999999011 ) ) ;
#36010 = EDGE_CURVE ( 'NONE', #18473, #11039, #48964, .T. ) ;
#36011 = CARTESIAN_POINT ( 'NONE',  ( 61.53217244954870324, 14.11227144105590092, -47.30221341948519864 ) ) ;
#36012 = EDGE_CURVE ( 'NONE', #51752, #29183, #27169, .T. ) ;
#36013 = ORIENTED_EDGE ( 'NONE', *, *, #11532, .F. ) ;
#36014 = ADVANCED_FACE ( 'NONE', ( #44028 ), #3432, .T. ) ;
#36015 = LINE ( 'NONE', #895, #33297 ) ;
#36016 = ORIENTED_EDGE ( 'NONE', *, *, #12958, .F. ) ;
#36017 = CARTESIAN_POINT ( 'NONE',  ( 11.26840393093330128, -10.51039387845690065, -42.10484805457209490 ) ) ;
#36018 = CARTESIAN_POINT ( 'NONE',  ( 52.10267382257649871, 1.883811055284760005, -77.60820171200670359 ) ) ;
#36020 = ORIENTED_EDGE ( 'NONE', *, *, #46627, .T. ) ;
#36019 = AXIS2_PLACEMENT_3D ( 'NONE', #6138, #38106, #45453 ) ;
#36021 = ORIENTED_EDGE ( 'NONE', *, *, #29680, .F. ) ;
#36022 = CARTESIAN_POINT ( 'NONE',  ( 9.366937397696199596, -15.61618894467949836, -28.45282021618999835 ) ) ;
#36023 = DIRECTION ( 'NONE',  ( -1.224650050763873077E-16, 1.000000000000000000, -1.784227544494129617E-11 ) ) ;
#36024 = TOROIDAL_SURFACE ( 'NONE', #35201, 18.00000000000000000, 2.000000000000000000 ) ;
#36025 = CARTESIAN_POINT ( 'NONE',  ( 60.37925162440420479, 14.51570526242369930, -47.49800878376869662 ) ) ;
#36026 = ADVANCED_FACE ( 'NONE', ( #24076 ), #15481, .T. ) ;
#36027 = CLOSED_SHELL ( 'NONE', ( #43194, #7321, #21526, #16065, #46675, #34577, #44231, #13921, #1699, #42612, #13427, #41454, #39890, #39865, #47472, #37029, #2082, #19804, #10806, #29896, #28299, #4242, #9346, #31566, #24980, #13048, #27560, #42415, #21280, #5781, #46294, #4198, #26669, #3488, #11617, #28016, #50983, #16970, #39570, #4612, #4721, #31209, #32139, #47050, #37426, #40289, #8451, #35429, #42550, #8197, #11233, #44825, #14184, #38459, #35174, #32391, #48505, #29094, #25424, #24915, #9105, #10933, #14917, #13099, #49819, #13598, #23699, #37069, #29075, #27080, #29209, #2886, #42374, #11851, #27728, #40629, #33578, #20512, #40261, #25854, #13986, #35721, #32507, #39390, #21169, #18439, #43718, #31686, #1531, #6965, #5137, #4966, #29006, #42162, #47629, #17408, #21376, #24572, #28665, #41584, #12245, #15363, #48680, #26143, #31373, #14055, #4180, #45128, #9058, #49168, #25568, #44608, #24343, #18934, #8575, #7763, #512 ) ) ;
#36028 = CARTESIAN_POINT ( 'NONE',  ( 22.90092895423980224, -15.60382985759644292, -40.45224344630474178 ) ) ;
#36029 = EDGE_CURVE ( 'NONE', #23707, #45957, #43091, .T. ) ;
#36030 = CARTESIAN_POINT ( 'NONE',  ( 41.72053737372350213, -43.71151935359279861, -3.400228435618770195 ) ) ;
#36031 = CARTESIAN_POINT ( 'NONE',  ( -5.340849039197499870, 15.73968974017349964, -4.544762132180990122 ) ) ;
#36032 = CARTESIAN_POINT ( 'NONE',  ( 46.95605112311885421, 23.06042441339815596, -75.52284329971668342 ) ) ;
#36033 = CARTESIAN_POINT ( 'NONE',  ( 60.51336243011509453, 14.11231868582309978, -27.14572052912820155 ) ) ;
#36034 = CARTESIAN_POINT ( 'NONE',  ( 9.270589976214530736, -11.81077039276889806, -60.44865228025189907 ) ) ;
#36035 = VERTEX_POINT ( 'NONE', #1297 ) ;
#36036 =( NAMED_UNIT ( * ) PLANE_ANGLE_UNIT ( ) SI_UNIT ( $, .RADIAN. ) );
#36037 = DIRECTION ( 'NONE',  ( -2.217154000000000151E-17, -9.040936000000000316E-17, 1.000000000000000000 ) ) ;
#36038 = CARTESIAN_POINT ( 'NONE',  ( 11.20590614228649962, 32.84406522022800345, -44.01467685434810306 ) ) ;
#36039 = CARTESIAN_POINT ( 'NONE',  ( 72.55316574448160338, 1.396295651964220008, -69.41420804701510860 ) ) ;
#36040 = CARTESIAN_POINT ( 'NONE',  ( 42.72381319638073194, -39.83914644532161731, -72.83559664042903137 ) ) ;
#36042 = EDGE_CURVE ( 'NONE', #586, #45208, #37846, .T. ) ;
#36041 = CARTESIAN_POINT ( 'NONE',  ( 54.66064891145146731, -55.47029091092863240, 17.35000000000000142 ) ) ;
#36043 = CARTESIAN_POINT ( 'NONE',  ( 12.91619884388280148, 18.87515571072599840, -21.10294288757389936 ) ) ;
#36044 = CARTESIAN_POINT ( 'NONE',  ( 46.97135722600339847, 23.04975284684289960, -75.52157732621060404 ) ) ;
#36045 = CARTESIAN_POINT ( 'NONE',  ( 48.61347624589569705, -53.95572845601289913, -54.54157758230459763 ) ) ;
#36046 = CARTESIAN_POINT ( 'NONE',  ( 51.85725430794233404, -32.72518063342734962, -18.71155503439485912 ) ) ;
#36047 = CARTESIAN_POINT ( 'NONE',  ( 16.13393739769609780, -15.61618894467929941, 8.449999999999999289 ) ) ;
#36048 = CARTESIAN_POINT ( 'NONE',  ( 14.32489919860644179, -32.43785826095948721, -34.75586992539663811 ) ) ;
#36049 = CARTESIAN_POINT ( 'NONE',  ( 56.43809645418499343, 13.88381105532070059, -15.14067943257860094 ) ) ;
#36050 = ORIENTED_EDGE ( 'NONE', *, *, #33227, .T. ) ;
#36051 = CIRCLE ( 'NONE', #38587, 1.500000000000001332 ) ;
#36052 = CARTESIAN_POINT ( 'NONE',  ( 9.121577334681090221, -16.37075734277619787, -79.81305924085489778 ) ) ;
#36053 =( BOUNDED_CURVE ( )  B_SPLINE_CURVE ( 3, ( #50125, #26514, #18400, #42530 ),
 .UNSPECIFIED., .F., .T. ) 
 B_SPLINE_CURVE_WITH_KNOTS ( ( 4, 4 ),
 ( 0.3742143439991775233, 0.4392488787996949862 ),
 .UNSPECIFIED. ) 
 CURVE ( )  GEOMETRIC_REPRESENTATION_ITEM ( )  RATIONAL_B_SPLINE_CURVE ( ( 1.000000000000000000, 0.9996475734957616099, 0.9996475734957616099, 1.000000000000000000 ) ) 
 REPRESENTATION_ITEM ( '' )  );
#36054 = CARTESIAN_POINT ( 'NONE',  ( 20.29255783753004039, -21.02754820491093213, -76.74449668442458972 ) ) ;
#36055 = EDGE_LOOP ( 'NONE', ( #50236, #9304, #34502, #47449 ) ) ;
#36056 = CARTESIAN_POINT ( 'NONE',  ( 71.50564047255809896, 1.187296498006439993, -70.50955232519169158 ) ) ;
#36057 = TOROIDAL_SURFACE ( 'NONE', #35951, 25.00000000000000000, 1.000000000000000000 ) ;
#36058 = CARTESIAN_POINT ( 'NONE',  ( 60.49551174326319369, -45.65747614152789424, -47.34056711453400368 ) ) ;
#36059 = CARTESIAN_POINT ( 'NONE',  ( 8.133937397696209715, 28.10308010054979988, -21.14999999999999858 ) ) ;
#36060 = DIRECTION ( 'NONE',  ( -9.408764999999898798E-18, 1.274833000000000002E-16, 1.000000000000000000 ) ) ;
#36062 = CARTESIAN_POINT ( 'NONE',  ( 15.09835279927984963, -23.52718445968407224, -78.33399673690963994 ) ) ;
#36061 = CARTESIAN_POINT ( 'NONE',  ( 41.39457728824679350, 8.464282045044221547, -79.25350500381260588 ) ) ;
#36063 = CARTESIAN_POINT ( 'NONE',  ( 30.43389199679464241, 4.399289011473882738, -84.61061572685468946 ) ) ;
#36064 = CARTESIAN_POINT ( 'NONE',  ( 47.40322300430410252, -54.65574458090419796, -54.88279555090289819 ) ) ;
#36065 = ORIENTED_EDGE ( 'NONE', *, *, #10588, .T. ) ;
#36066 = DIRECTION ( 'NONE',  ( 0.000000000000000000, 1.000000000000000000, 0.000000000000000000 ) ) ;
#36067 = ORIENTED_EDGE ( 'NONE', *, *, #22207, .T. ) ;
#36068 = EDGE_LOOP ( 'NONE', ( #49427, #41176, #34721 ) ) ;
#36069 = VERTEX_POINT ( 'NONE', #13113 ) ;
#36070 = CARTESIAN_POINT ( 'NONE',  ( 1.027904703268269992, 11.45423359053189927, -20.15000000000000213 ) ) ;
#36071 = CARTESIAN_POINT ( 'NONE',  ( 52.56724181638659843, -49.85961536077480361, -48.49338281493830038 ) ) ;
#36072 = DIRECTION ( 'NONE',  ( 0.000000000000000000, 0.000000000000000000, 1.000000000000000000 ) ) ;
#36073 = CARTESIAN_POINT ( 'NONE',  ( 76.39106947318838081, -16.04540269916347839, -12.75801850546862504 ) ) ;
#36074 = CARTESIAN_POINT ( 'NONE',  ( 52.56495426071009547, -52.43765526798470233, -54.45623365677440120 ) ) ;
#36075 = ORIENTED_EDGE ( 'NONE', *, *, #39016, .T. ) ;
#36076 = EDGE_LOOP ( 'NONE', ( #26763, #1193, #48543, #39621, #4959, #42853, #37299 ) ) ;
#36077 = EDGE_CURVE ( 'NONE', #16351, #23557, #28801, .T. ) ;
#36078 = CARTESIAN_POINT ( 'NONE',  ( 48.08607070564750074, 23.01868680830909852, -54.70522948828759979 ) ) ;
#36079 = CARTESIAN_POINT ( 'NONE',  ( -20.88509709344132759, -3.337410866617939842, -53.17709637982930104 ) ) ;
#36080 = CARTESIAN_POINT ( 'NONE',  ( 56.33973444090680260, -50.60696655799740284, -52.96824549530209936 ) ) ;
#36081 = CARTESIAN_POINT ( 'NONE',  ( 14.36277414553998000, -9.025293915162313496, -35.86948574067652373 ) ) ;
#36082 = CARTESIAN_POINT ( 'NONE',  ( 64.07109745055549865, 0.6782384520987629895, -17.38429331904790232 ) ) ;
#36083 = CARTESIAN_POINT ( 'NONE',  ( 52.26505149639999814, -49.78354415430390389, -77.19463936772501711 ) ) ;
#36084 = ORIENTED_EDGE ( 'NONE', *, *, #4549, .F. ) ;
#36085 = CARTESIAN_POINT ( 'NONE',  ( 64.93393739769616957, 11.38381105532080184, -61.44999999999993889 ) ) ;
#36086 = DIRECTION ( 'NONE',  ( -0.2260571801428149508, -1.665334536937734318E-16, 0.9741140340359947247 ) ) ;
#36087 = CARTESIAN_POINT ( 'NONE',  ( 64.74712693194929614, 0.8966068345641450277, -70.60278586552529134 ) ) ;
#36088 = CARTESIAN_POINT ( 'NONE',  ( 22.90093739769620029, -15.61618894467913243, -28.45282021618999835 ) ) ;
#36089 = CARTESIAN_POINT ( 'NONE',  ( 9.575251713171320844, -11.30685144534250064, -51.19753123634840364 ) ) ;
#36090 = CARTESIAN_POINT ( 'NONE',  ( 12.94463750493000020, -50.31721522897190368, -21.18967265423650304 ) ) ;
#36091 = DIRECTION ( 'NONE',  ( 0.000000000000000000, 0.000000000000000000, -1.000000000000000000 ) ) ;
#36092 = EDGE_CURVE ( 'NONE', #7993, #51855, #8664, .T. ) ;
#36093 = CARTESIAN_POINT ( 'NONE',  ( 18.43801701820914118, -51.25800930999477600, -15.70152999933596760 ) ) ;
#36094 = CARTESIAN_POINT ( 'NONE',  ( 65.43393739769578588, -48.11618894467640217, -73.25000000000000000 ) ) ;
#36095 = CARTESIAN_POINT ( 'NONE',  ( 61.48324819819570308, -45.36430604964360214, -47.33702497767190209 ) ) ;
#36096 = CIRCLE ( 'NONE', #16838, 48.00000000000000000 ) ;
#36097 = CARTESIAN_POINT ( 'NONE',  ( 41.64265090548720138, 15.19461330351670014, -4.296538310234230273 ) ) ;
#36098 = VECTOR ( 'NONE', #1087, 1000.000000000000000 ) ;
#36099 = CARTESIAN_POINT ( 'NONE',  ( 9.092282930800720919, -16.01325511460819939, -53.82924985198780377 ) ) ;
#36100 = CARTESIAN_POINT ( 'NONE',  ( 14.06336169935696034, -7.911062148213927614, -41.20899793506684006 ) ) ;
#36101 = AXIS2_PLACEMENT_3D ( 'NONE', #30978, #13984, #29941 ) ;
#36102 = ORIENTED_EDGE ( 'NONE', *, *, #21391, .T. ) ;
#36103 = CARTESIAN_POINT ( 'NONE',  ( 14.34420985974599816, -51.11618894649849665, -74.14993593045390696 ) ) ;
#36104 = CARTESIAN_POINT ( 'NONE',  ( 47.36653643891619936, -54.67788820370529379, -54.81260825270820192 ) ) ;
#36105 = CARTESIAN_POINT ( 'NONE',  ( 16.13393739769620083, -15.61618894467929941, -44.64999999999999858 ) ) ;
#36106 = CARTESIAN_POINT ( 'NONE',  ( 11.27226101419321402, -9.290022498966679976, -36.79933602528976877 ) ) ;
#36107 = CARTESIAN_POINT ( 'NONE',  ( 17.80740971062453326, 20.21129459968210895, -75.25166008038893040 ) ) ;
#36108 = CARTESIAN_POINT ( 'NONE',  ( 60.90761281762335244, -45.44548680042808542, -47.17297249547537774 ) ) ;
#36109 = ADVANCED_FACE ( 'NONE', ( #37198 ), #2988, .T. ) ;
#36110 = CARTESIAN_POINT ( 'NONE',  ( 21.54526339463619777, -11.45752448184413019, -76.24446912191029924 ) ) ;
#36112 = EDGE_CURVE ( 'NONE', #46925, #23386, #14027, .T. ) ;
#36111 = CYLINDRICAL_SURFACE ( 'NONE', #40936, 0.4999999999999982236 ) ;
#36114 = CARTESIAN_POINT ( 'NONE',  ( 11.27228881102597136, -21.94237641914053683, -52.50066408798487316 ) ) ;
#36113 = DIRECTION ( 'NONE',  ( -1.000000000000000000, 0.000000000000000000, 0.000000000000000000 ) ) ;
#36115 = DIRECTION ( 'NONE',  ( 1.000000000000000000, 0.000000000000000000, 0.000000000000000000 ) ) ;
#36116 = CARTESIAN_POINT ( 'NONE',  ( 48.54174064777019737, 22.83460439869960013, -54.75827641492099929 ) ) ;
#36117 = ORIENTED_EDGE ( 'NONE', *, *, #40810, .T. ) ;
#36118 = CARTESIAN_POINT ( 'NONE',  ( 52.92824266770190178, -49.62542305747680160, -48.92669095312290040 ) ) ;
#36119 = ORIENTED_EDGE ( 'NONE', *, *, #5945, .T. ) ;
#36120 = CARTESIAN_POINT ( 'NONE',  ( 44.44997065502152367, 7.812898992897342687, -68.49922028869087853 ) ) ;
#36121 = CARTESIAN_POINT ( 'NONE',  ( -21.36606260230379917, 31.59091783650714547, 17.05710678118654755 ) ) ;
#36123 = CARTESIAN_POINT ( 'NONE',  ( 52.67058128702819175, 18.52949274918249856, -27.99782339546649723 ) ) ;
#36122 = CARTESIAN_POINT ( 'NONE',  ( 84.44784216359251161, 11.88381105532070059, -47.47585302082339354 ) ) ;
#36124 = CARTESIAN_POINT ( 'NONE',  ( 22.97503138632190200, -17.33141246813480052, -66.53101608161080094 ) ) ;
#36125 = CARTESIAN_POINT ( 'NONE',  ( 52.58363278054860501, 18.61045885154019786, -48.51250198868969932 ) ) ;
#36126 = CARTESIAN_POINT ( 'NONE',  ( 55.85583526904490270, -45.19818891271899730, -15.37717892060849856 ) ) ;
#36127 = CARTESIAN_POINT ( 'NONE',  ( 16.65420337941066720, -51.11618894467930119, -21.07727733026462857 ) ) ;
#36128 = ORIENTED_EDGE ( 'NONE', *, *, #39861, .T. ) ;
#36129 = CARTESIAN_POINT ( 'NONE',  ( 23.97791451297860021, -15.37376122739139994, -41.27767096285609938 ) ) ;
#36130 = ORIENTED_EDGE ( 'NONE', *, *, #40036, .T. ) ;
#36131 = CARTESIAN_POINT ( 'NONE',  ( 11.74133921615520038, -65.36765915750379463, -17.40968291634680298 ) ) ;
#36132 = CARTESIAN_POINT ( 'NONE',  ( 10.22956136350960143, 32.89403351977829715, -46.33680948560530055 ) ) ;
#36133 = CARTESIAN_POINT ( 'NONE',  ( 17.00689302767908728, -16.25042833492357985, -9.392532499999980189 ) ) ;
#36134 = EDGE_CURVE ( 'NONE', #32056, #6345, #12982, .T. ) ;
#36135 = AXIS2_PLACEMENT_3D ( 'NONE', #36811, #36037, #15623 ) ;
#36136 = CARTESIAN_POINT ( 'NONE',  ( 48.34931318170839631, -53.91658640633450261, -54.01551401094359761 ) ) ;
#36137 = CARTESIAN_POINT ( 'NONE',  ( 10.65676624057133637, -63.90657753633119142, -23.61757751456070764 ) ) ;
#36138 = DIRECTION ( 'NONE',  ( 0.000000000000000000, 0.000000000000000000, -1.000000000000000000 ) ) ;
#36139 = AXIS2_PLACEMENT_3D ( 'NONE', #47073, #27129, #14825 ) ;
#36140 = VERTEX_POINT ( 'NONE', #17223 ) ;
#36141 = EDGE_CURVE ( 'NONE', #27219, #47951, #3771, .T. ) ;
#36142 = CARTESIAN_POINT ( 'NONE',  ( 12.14971266001781380, -8.703718556933592865, -74.84097244948981142 ) ) ;
#36143 = CARTESIAN_POINT ( 'NONE',  ( 11.13393739769619906, -63.27446496484219551, -43.91455789178539248 ) ) ;
#36144 = DIRECTION ( 'NONE',  ( 1.000000000000000000, 2.460964292799963328E-14, 0.000000000000000000 ) ) ;
#36145 = ORIENTED_EDGE ( 'NONE', *, *, #21916, .T. ) ;
#36146 = CARTESIAN_POINT ( 'NONE',  ( 24.04472027134544021, -15.61619704117925522, -43.79232540400376905 ) ) ;
#36147 = CARTESIAN_POINT ( 'NONE',  ( 50.12211818213420145, -48.61618485716249438, -76.14999999999999147 ) ) ;
#36148 = CARTESIAN_POINT ( 'NONE',  ( 8.222911833873924436, -14.62160878757158500, -48.54769499149303869 ) ) ;
#36149 = ORIENTED_EDGE ( 'NONE', *, *, #32037, .T. ) ;
#36150 = CARTESIAN_POINT ( 'NONE',  ( 9.807731639197928786, -20.47781496564226700, -62.58399752867111232 ) ) ;
#36151 = CARTESIAN_POINT ( 'NONE',  ( 18.11714455905750043, -32.59356659976219817, -35.02127583263639821 ) ) ;
#36152 = CYLINDRICAL_SURFACE ( 'NONE', #25167, 0.5000000000000049960 ) ;
#36153 = CARTESIAN_POINT ( 'NONE',  ( 55.40055888017540298, 20.31707842463499958, -53.98551680322430713 ) ) ;
#36154 = CARTESIAN_POINT ( 'NONE',  ( 22.84106276893500009, -20.41172742439350074, -69.98991178896608290 ) ) ;
#36155 = CARTESIAN_POINT ( 'NONE',  ( 68.13393739769618662, -2.166188944679360073, -65.65000000000000568 ) ) ;
#36156 = CARTESIAN_POINT ( 'NONE',  ( 51.13393739769659874, -50.61618894467899565, 14.21249999999999858 ) ) ;
#36157 = EDGE_LOOP ( 'NONE', ( #46492, #12293, #35081 ) ) ;
#36158 = CARTESIAN_POINT ( 'NONE',  ( 13.53986639234880052, -22.60027724769790325, -68.84585897299571400 ) ) ;
#36159 = CARTESIAN_POINT ( 'NONE',  ( 8.222937397696199469, -15.61618894467929941, -32.14999999999999858 ) ) ;
#36160 = DIRECTION ( 'NONE',  ( -1.000000000000000000, 0.000000000000000000, 0.000000000000000000 ) ) ;
#36161 = CARTESIAN_POINT ( 'NONE',  ( 46.84179439965980407, 22.69619787130520194, -75.82399969562499109 ) ) ;
#36162 = CARTESIAN_POINT ( 'NONE',  ( 71.25658036288379549, 1.391252479931859964, -61.03617692120100457 ) ) ;
#36163 = CARTESIAN_POINT ( 'NONE',  ( 53.41693480164780539, 18.12090330447910347, -48.75416851879779756 ) ) ;
#36164 = AXIS2_PLACEMENT_3D ( 'NONE', #35030, #11210, #43433 ) ;
#36165 = DIRECTION ( 'NONE',  ( 0.000000000000000000, 0.000000000000000000, 1.000000000000000000 ) ) ;
#36166 = CARTESIAN_POINT ( 'NONE',  ( 13.85074091091579973, -23.53892423692099811, -78.09698001689919522 ) ) ;
#36167 = EDGE_CURVE ( 'NONE', #10465, #29313, #18825, .T. ) ;
#36168 = CARTESIAN_POINT ( 'NONE',  ( 56.69209721199219842, -50.61618744975589834, -75.40240639624190067 ) ) ;
#36170 = CARTESIAN_POINT ( 'NONE',  ( 41.25851182071981071, -39.72332991368651278, -79.73195694794895871 ) ) ;
#36169 = FACE_OUTER_BOUND ( 'NONE', #20025, .T. ) ;
#36171 = CARTESIAN_POINT ( 'NONE',  ( 63.28287142701668699, 1.331842543267529821, -68.70530175958410268 ) ) ;
#36172 = CARTESIAN_POINT ( 'NONE',  ( 61.11825904928579689, 14.08859410275880109, -46.89980876084979400 ) ) ;
#36173 = CARTESIAN_POINT ( 'NONE',  ( 9.807825181025211947, -10.75444290033733452, -78.71600221907445416 ) ) ;
#36174 = CARTESIAN_POINT ( 'NONE',  ( 16.13393739769620083, -15.61618894467929941, -35.12503119152809461 ) ) ;
#36175 = EDGE_CURVE ( 'NONE', #2647, #23957, #21386, .T. ) ;
#36176 = VERTEX_POINT ( 'NONE', #5687 ) ;
#36177 = CARTESIAN_POINT ( 'NONE',  ( 52.94585587482559674, -49.60009264233129755, -48.75076953771959865 ) ) ;
#36178 = CARTESIAN_POINT ( 'NONE',  ( 59.00011887688039991, -45.52336115602069810, -26.53752582118919889 ) ) ;
#36179 = CARTESIAN_POINT ( 'NONE',  ( 22.46007903505417502, -20.47789928629981304, -72.00068286951631080 ) ) ;
#36180 = CARTESIAN_POINT ( 'NONE',  ( 57.42933415471480174, 14.50457775711600128, -26.26072587755309939 ) ) ;
#36181 = CARTESIAN_POINT ( 'NONE',  ( 12.28685844389720039, -9.236010473171079482, -77.55994138999389520 ) ) ;
#36182 = CARTESIAN_POINT ( 'NONE',  ( 50.97631217574399898, 18.77236619143900143, -76.22722516077449484 ) ) ;
#36183 = CARTESIAN_POINT ( 'NONE',  ( 53.21743490025700396, 18.23051946133029944, -48.89816786641330282 ) ) ;
#36184 = CARTESIAN_POINT ( 'NONE',  ( 71.30558087559749936, 1.190292248953970011, -70.62687270921169613 ) ) ;
#36185 = FACE_BOUND ( 'NONE', #7862, .T. ) ;
#36186 = ORIENTED_EDGE ( 'NONE', *, *, #2171, .F. ) ;
#36187 = CARTESIAN_POINT ( 'NONE',  ( 64.93393739769619799, 1.883811055320669947, -62.44999999999999574 ) ) ;
#36188 = CARTESIAN_POINT ( 'NONE',  ( 47.52380275344859939, -54.58920838926499641, -55.02111885050249640 ) ) ;
#36189 = CARTESIAN_POINT ( 'NONE',  ( 11.90611060579353087, -65.43712337795734868, -18.00436963408782987 ) ) ;
#36190 = CARTESIAN_POINT ( 'NONE',  ( 10.13393739769589885, 22.91950879131600161, -54.64999999999999858 ) ) ;
#36191 = CARTESIAN_POINT ( 'NONE',  ( 59.48605679216419873, -29.56288290624030068, -15.85191620889269970 ) ) ;
#36192 = CARTESIAN_POINT ( 'NONE',  ( 71.51817256006181367, 0.9307121176571799825, -60.69545425604199806 ) ) ;
#36193 = DIRECTION ( 'NONE',  ( 0.000000000000000000, 0.000000000000000000, 1.000000000000000000 ) ) ;
#36194 = CARTESIAN_POINT ( 'NONE',  ( 72.14208904168791037, 1.345243094457279964, -61.33716833010870317 ) ) ;
#36195 = CARTESIAN_POINT ( 'NONE',  ( 51.63119803174421918, -34.05402968804899189, -76.94892812354784439 ) ) ;
#36196 = EDGE_CURVE ( 'NONE', #19506, #16944, #15480, .T. ) ;
#36197 = CARTESIAN_POINT ( 'NONE',  ( 65.14310169846920928, 1.336371993404949832, -70.52842906692660563 ) ) ;
#36198 = ORIENTED_EDGE ( 'NONE', *, *, #21264, .T. ) ;
#36199 = ORIENTED_EDGE ( 'NONE', *, *, #32788, .T. ) ;
#36200 = CARTESIAN_POINT ( 'NONE',  ( -1.057045605833899948, -15.61618894397629731, 14.85000000069720549 ) ) ;
#36201 = CARTESIAN_POINT ( 'NONE',  ( 50.18734600372286536, -30.13642185530741457, -16.07512387930005815 ) ) ;
#36202 = ORIENTED_EDGE ( 'NONE', *, *, #38745, .F. ) ;
#36203 = CARTESIAN_POINT ( 'NONE',  ( 11.27217187505504725, -9.290089935112355590, -58.79930474092849124 ) ) ;
#36204 = DIRECTION ( 'NONE',  ( 0.000000000000000000, 0.000000000000000000, 1.000000000000000000 ) ) ;
#36205 = AXIS2_PLACEMENT_3D ( 'NONE', #17212, #20858, #45251 ) ;
#36206 = ORIENTED_EDGE ( 'NONE', *, *, #2613, .F. ) ;
#36207 = AXIS2_PLACEMENT_3D ( 'NONE', #31366, #51568, #19593 ) ;
#36208 = CARTESIAN_POINT ( 'NONE',  ( 16.13393739769620083, -15.61618894467929941, -14.65000000000000036 ) ) ;
#36209 = CARTESIAN_POINT ( 'NONE',  ( 17.83125332364319959, 1.104866772713940071, -34.68801049095939959 ) ) ;
#36210 = CARTESIAN_POINT ( 'NONE',  ( 20.08011741788975613, -22.53811379943914872, -65.84286859354855892 ) ) ;
#36211 = CARTESIAN_POINT ( 'NONE',  ( 10.54937000320200013, -9.550273756326699726, -43.05547522733549926 ) ) ;
#36212 = LINE ( 'NONE', #47519, #38040 ) ;
#36213 = CARTESIAN_POINT ( 'NONE',  ( 42.94456142498044926, -37.76943540611747352, -75.59687433678018920 ) ) ;
#36214 = CARTESIAN_POINT ( 'NONE',  ( 0.000000000000000000, 0.000000000000000000, 0.000000000000000000 ) ) ;
#36215 = ORIENTED_EDGE ( 'NONE', *, *, #48033, .T. ) ;
#36216 = CARTESIAN_POINT ( 'NONE',  ( 11.31451853429699916, -65.21686366208800223, -22.84783898345410336 ) ) ;
#36217 = CARTESIAN_POINT ( 'NONE',  ( 14.73780803183720067, -8.297888458486630370, -33.67265358074869397 ) ) ;
#36218 = CARTESIAN_POINT ( 'NONE',  ( 45.18452561082949615, 14.58898524498980009, -8.866308698657380916 ) ) ;
#36219 = CARTESIAN_POINT ( 'NONE',  ( 14.03951828119850020, 20.70615929725470039, -75.58342519351550948 ) ) ;
#36220 = CARTESIAN_POINT ( 'NONE',  ( 23.76270136862467908, -17.78029879744761388, -59.88032873326731931 ) ) ;
#36221 = CARTESIAN_POINT ( 'NONE',  ( 82.72635976414500192, -45.16472152492289638, -46.96146434100139544 ) ) ;
#36222 = CARTESIAN_POINT ( 'NONE',  ( 64.75240447675760436, 1.412311545208970065, -70.17188921921470524 ) ) ;
#36223 = B_SPLINE_CURVE_WITH_KNOTS ( 'NONE', 3,
 ( #38906, #26044, #2996, #10609, #34429, #50438, #7187, #14527, #46777, #2219, #29974, #18198, #18966, #30240 ),
 .UNSPECIFIED., .F., .F.,
 ( 4, 2, 2, 2, 1, 1, 2, 4 ),
 ( 0.000000000000000000, 0.2471173528950156018, 0.3706760293425299113, 0.4324553675662862195, 0.4633450366781692309, 0.4787898712341108753, 0.4865122885120863327, 0.4942347057900616236 ),
 .UNSPECIFIED. ) ;
#36224 = CARTESIAN_POINT ( 'NONE',  ( 8.030996740944530643, -17.14100808875369708, -42.44846103827049433 ) ) ;
#36225 = ORIENTED_EDGE ( 'NONE', *, *, #38637, .T. ) ;
#36226 = CARTESIAN_POINT ( 'NONE',  ( 54.16580280984440776, -48.35420548540910346, -26.76702793006570147 ) ) ;
#36227 = EDGE_CURVE ( 'NONE', #11818, #25290, #27243, .T. ) ;
#36228 = CARTESIAN_POINT ( 'NONE',  ( 15.53208191793540038, -50.86428735276679447, -20.56249370038110058 ) ) ;
#36229 = CARTESIAN_POINT ( 'NONE',  ( 16.00113812002476621, -23.55770649663861604, -40.01306273174144224 ) ) ;
#36230 = DIRECTION ( 'NONE',  ( 0.000000000000000000, 0.000000000000000000, 1.000000000000000000 ) ) ;
#36231 = CARTESIAN_POINT ( 'NONE',  ( 61.68773928233808590, -45.18163828788996739, -46.89102616239745913 ) ) ;
#36232 = CARTESIAN_POINT ( 'NONE',  ( 12.76120697008239802, -49.98606222100620045, -21.08963178055790166 ) ) ;
#36233 = ORIENTED_EDGE ( 'NONE', *, *, #41068, .T. ) ;
#36234 = CARTESIAN_POINT ( 'NONE',  ( -9.500613363851449833, -43.72129052405930594, -5.962761149281509354 ) ) ;
#36235 = AXIS2_PLACEMENT_3D ( 'NONE', #47526, #43083, #11623 ) ;
#36237 = CARTESIAN_POINT ( 'NONE',  ( 47.31587322217479397, 23.47801198921460397, -54.77833839503799851 ) ) ;
#36236 = AXIS2_PLACEMENT_3D ( 'NONE', #32523, #8203, #40169 ) ;
#36238 = CYLINDRICAL_SURFACE ( 'NONE', #31216, 1.999999999999997113 ) ;
#36239 = CARTESIAN_POINT ( 'NONE',  ( 63.08453170404659716, 0.9940423591679348192, -62.42346963566990325 ) ) ;
#36240 = FACE_OUTER_BOUND ( 'NONE', #27381, .T. ) ;
#36241 = CARTESIAN_POINT ( 'NONE',  ( 41.82061708364619790, 12.78867990672720012, -4.552229662895129536 ) ) ;
#36242 = DIRECTION ( 'NONE',  ( 0.000000000000000000, 0.000000000000000000, -1.000000000000000000 ) ) ;
#36243 = DIRECTION ( 'NONE',  ( 0.000000000000000000, 0.000000000000000000, 1.000000000000000000 ) ) ;
#36244 = DIRECTION ( 'NONE',  ( 0.000000000000000000, 0.000000000000000000, 1.000000000000000000 ) ) ;
#36245 = CARTESIAN_POINT ( 'NONE',  ( 57.13638867421310152, -47.42892726663239955, -48.04708942102450209 ) ) ;
#36246 = B_SPLINE_CURVE_WITH_KNOTS ( 'NONE', 3,
 ( #45293, #1268, #49496, #25351, #32953, #29039, #5468, #9646, #13583, #29548, #9134, #45034, #17761, #25089, #33732, #49745 ),
 .UNSPECIFIED., .F., .F.,
 ( 4, 2, 2, 2, 2, 2, 2, 4 ),
 ( -1.165733999999999982E-15, 0.07319275283555999601, 0.1391693187718409941, 0.1804046724820169978, 0.2061767685508770209, 0.2577209606885970117, 0.3401916681089490191, 0.4123535371017569839 ),
 .UNSPECIFIED. ) ;
#36247 = CARTESIAN_POINT ( 'NONE',  ( 44.12711257345860361, -33.11618894467940066, -54.38706558040979644 ) ) ;
#36248 = CARTESIAN_POINT ( 'NONE',  ( 64.76726729265010363, 1.264689361399219836, -60.86115090893359536 ) ) ;
#36249 = CARTESIAN_POINT ( 'NONE',  ( 12.14992344158154935, -8.703599321502185404, -72.84100158868179165 ) ) ;
#36250 = CARTESIAN_POINT ( 'NONE',  ( 63.55847417696450208, 1.399433130755639798, -62.41600958228519858 ) ) ;
#36251 = ORIENTED_EDGE ( 'NONE', *, *, #14626, .F. ) ;
#36252 = CARTESIAN_POINT ( 'NONE',  ( 74.13393739769620083, 0.8838110553206759423, -65.65000000000000568 ) ) ;
#36253 = CARTESIAN_POINT ( 'NONE',  ( 8.813920544456330219, 32.04044820803110127, -46.67144773886860065 ) ) ;
#36254 = CARTESIAN_POINT ( 'NONE',  ( 22.90093740082441798, -15.61701879830229700, -34.45285756426908819 ) ) ;
#36255 = CARTESIAN_POINT ( 'NONE',  ( 10.21207254689429966, -11.00732563776159978, -81.23899999999999011 ) ) ;
#36256 = ORIENTED_EDGE ( 'NONE', *, *, #16484, .T. ) ;
#36257 = EDGE_CURVE ( 'NONE', #35579, #8558, #33032, .T. ) ;
#36258 = CARTESIAN_POINT ( 'NONE',  ( 18.08040100137599993, 20.38364582413090176, -75.40982873507010709 ) ) ;
#36259 = ORIENTED_EDGE ( 'NONE', *, *, #31513, .F. ) ;
#36260 = ORIENTED_EDGE ( 'NONE', *, *, #6403, .T. ) ;
#36261 = EDGE_CURVE ( 'NONE', #19147, #21117, #20462, .T. ) ;
#36262 = ORIENTED_EDGE ( 'NONE', *, *, #4303, .F. ) ;
#36263 = CARTESIAN_POINT ( 'NONE',  ( -14.01196063605389774, -47.08947743092479499, 17.35000000000000142 ) ) ;
#36264 = CARTESIAN_POINT ( 'NONE',  ( 18.38973105523400164, -21.99613282959019500, -81.23899999999999011 ) ) ;
#36265 = CARTESIAN_POINT ( 'NONE',  ( 8.428869108528790122, -13.54539397395445022, -62.59100196226616220 ) ) ;
#36266 = CARTESIAN_POINT ( 'NONE',  ( 20.11812032201747868, -8.703696620057041144, -73.45899818277568727 ) ) ;
#36267 = CARTESIAN_POINT ( 'NONE',  ( 75.43171768290677903, 10.53008244115809866, -13.17417775896968735 ) ) ;
#36268 = CARTESIAN_POINT ( 'NONE',  ( 12.12757535754312421, 33.95539782499548664, -16.69244757705873283 ) ) ;
#36269 = ORIENTED_EDGE ( 'NONE', *, *, #2977, .F. ) ;
#36270 = CARTESIAN_POINT ( 'NONE',  ( 11.65410534970359713, -64.86784288575155699, -23.89686975621782139 ) ) ;
#36271 = CARTESIAN_POINT ( 'NONE',  ( 57.34776334542480214, -45.81180625069929846, -26.27178910182970029 ) ) ;
#36272 = EDGE_LOOP ( 'NONE', ( #51030, #48807, #16815, #38496 ) ) ;
#36273 = VECTOR ( 'NONE', #32102, 1000.000000000000000 ) ;
#36274 = EDGE_LOOP ( 'NONE', ( #16998, #511 ) ) ;
#36275 = DIRECTION ( 'NONE',  ( 0.000000000000000000, 0.000000000000000000, -1.000000000000000000 ) ) ;
#36277 = DIRECTION ( 'NONE',  ( 0.000000000000000000, -1.000000000000000000, 0.000000000000000000 ) ) ;
#36276 = AXIS2_PLACEMENT_3D ( 'NONE', #10827, #15530, #51179 ) ;
#36278 = CARTESIAN_POINT ( 'NONE',  ( 61.11504165468770111, 14.39036167884340145, -47.68917451007700237 ) ) ;
#36279 = CARTESIAN_POINT ( 'NONE',  ( 48.24989815756970302, 14.34044383502719988, -10.69710604161790002 ) ) ;
#36280 = CARTESIAN_POINT ( 'NONE',  ( -3.202629701451740196, 17.10292418714999840, -4.381046808933160008 ) ) ;
#36281 = DIRECTION ( 'NONE',  ( 0.000000000000000000, 0.000000000000000000, -1.000000000000000000 ) ) ;
#36282 = CARTESIAN_POINT ( 'NONE',  ( 61.24683137928700205, 13.99389904076519997, -27.77110181634639829 ) ) ;
#36283 = CARTESIAN_POINT ( 'NONE',  ( 10.10036780576549909, -10.59794361762400072, -62.50834448790610054 ) ) ;
#36284 = ORIENTED_EDGE ( 'NONE', *, *, #2891, .T. ) ;
#36285 = CARTESIAN_POINT ( 'NONE',  ( 59.00597303369990243, 15.28899821959569927, -47.85315989107520807 ) ) ;
#36286 = AXIS2_PLACEMENT_3D ( 'NONE', #35894, #19651, #28271 ) ;
#36287 = ADVANCED_FACE ( 'NONE', ( #1232 ), #32650, .T. ) ;
#36288 = CARTESIAN_POINT ( 'NONE',  ( 23.34813653593170102, -49.28809633162250492, -34.65024031912469837 ) ) ;
#36289 = CARTESIAN_POINT ( 'NONE',  ( 11.53659969949129938, 33.50198822980290458, -44.98688683885700357 ) ) ;
#36290 = CARTESIAN_POINT ( 'NONE',  ( 72.49788296046230585, 1.442158793902679870, -69.35604527063249236 ) ) ;
#36291 = CARTESIAN_POINT ( 'NONE',  ( 42.94172388228522408, -39.86051557588725558, -71.78134772292702337 ) ) ;
#36292 = CARTESIAN_POINT ( 'NONE',  ( 11.63393739769600010, 10.38381105532060111, -34.64999999999999858 ) ) ;
#36293 = CARTESIAN_POINT ( 'NONE',  ( 47.14848365886989967, 23.49639526634990006, -74.72737464375309457 ) ) ;
#36294 = CARTESIAN_POINT ( 'NONE',  ( 48.71774127335779525, -54.07467890585870407, -55.20634912303470543 ) ) ;
#36295 = CARTESIAN_POINT ( 'NONE',  ( -6.923935172077830380, 14.83398127567929947, -5.625849176739690094 ) ) ;
#36296 = CARTESIAN_POINT ( 'NONE',  ( 50.03007040746459921, -48.61618894467930119, -76.14999999999999147 ) ) ;
#36297 = CARTESIAN_POINT ( 'NONE',  ( 66.50379331185658316, -33.11590393224402362, -20.28030461099050896 ) ) ;
#36298 = LINE ( 'NONE', #4863, #34783 ) ;
#36299 = VERTEX_POINT ( 'NONE', #29514 ) ;
#36300 = CIRCLE ( 'NONE', #30436, 0.5000000000000002220 ) ;
#36301 = CARTESIAN_POINT ( 'NONE',  ( 23.58066320393950122, -15.38603876551069938, -41.05750806020520116 ) ) ;
#36302 = CARTESIAN_POINT ( 'NONE',  ( 17.90515509213406631, -22.20707059168299935, -76.86949976336627799 ) ) ;
#36303 = ORIENTED_EDGE ( 'NONE', *, *, #8710, .T. ) ;
#36304 = DIRECTION ( 'NONE',  ( -0.1999849291395982553, -0.9797989733190325401, 0.000000000000000000 ) ) ;
#36305 = CARTESIAN_POINT ( 'NONE',  ( 60.57316152011729571, -45.60666961708100331, -47.23474488792719939 ) ) ;
#36306 = CARTESIAN_POINT ( 'NONE',  ( 16.13393739769620083, -15.61618894467929941, -74.14999999999999147 ) ) ;
#36307 = CARTESIAN_POINT ( 'NONE',  ( 13.29299421628470057, 18.84434172282420050, -21.00266242605139766 ) ) ;
#36309 = CARTESIAN_POINT ( 'NONE',  ( -0.01592648613901413018, -8.413074003574475768, -34.78031642072628671 ) ) ;
#36308 = CARTESIAN_POINT ( 'NONE',  ( 41.00753304566280377, 8.418767411291142366, -81.11804229810685740 ) ) ;
#36310 = DIRECTION ( 'NONE',  ( 0.000000000000000000, 0.000000000000000000, 1.000000000000000000 ) ) ;
#36311 = FACE_OUTER_BOUND ( 'NONE', #18781, .T. ) ;
#36312 = ORIENTED_EDGE ( 'NONE', *, *, #51637, .F. ) ;
#36313 = CARTESIAN_POINT ( 'NONE',  ( 84.41763914545359171, -43.52694424673759954, -47.43918784650069398 ) ) ;
#36314 = VERTEX_POINT ( 'NONE', #45518 ) ;
#36315 = VERTEX_POINT ( 'NONE', #25569 ) ;
#36316 = ADVANCED_FACE ( 'NONE', ( #446 ), #9098, .F. ) ;
#36317 = VERTEX_POINT ( 'NONE', #32390 ) ;
#36318 = DIRECTION ( 'NONE',  ( 1.000000000000000000, 2.460964292799963328E-14, 0.000000000000000000 ) ) ;
#36319 = CARTESIAN_POINT ( 'NONE',  ( 18.20465248542906878, -7.911098894993664032, -79.37566619958934666 ) ) ;
#36320 = CARTESIAN_POINT ( 'NONE',  ( 76.40205803391916106, -11.62003586772016739, -12.80537183077186114 ) ) ;
#36321 = CARTESIAN_POINT ( 'NONE',  ( 53.77933314157539968, -51.92037616820480395, -54.11586239492699235 ) ) ;
#36322 = ORIENTED_EDGE ( 'NONE', *, *, #39214, .T. ) ;
#36323 = VERTEX_POINT ( 'NONE', #48677 ) ;
#36324 = CARTESIAN_POINT ( 'NONE',  ( 9.807675336324628290, -20.47774281110765671, -56.29929133037190070 ) ) ;
#36325 = CARTESIAN_POINT ( 'NONE',  ( 23.00624656684072988, -16.56722779529380674, -32.89035143740448319 ) ) ;
#36326 = LINE ( 'NONE', #11481, #13628 ) ;
#36327 = AXIS2_PLACEMENT_3D ( 'NONE', #21576, #50671, #14768 ) ;
#36328 = CARTESIAN_POINT ( 'NONE',  ( -9.882013117715120032, 9.266944274022621997, -19.14999999999999858 ) ) ;
#36329 = DIRECTION ( 'NONE',  ( 0.000000000000000000, 0.000000000000000000, -1.000000000000000000 ) ) ;
#36330 = ORIENTED_EDGE ( 'NONE', *, *, #8613, .T. ) ;
#36331 = CARTESIAN_POINT ( 'NONE',  ( 57.42459889539989604, -50.12148349570598782, -52.60814563364522911 ) ) ;
#36332 = CARTESIAN_POINT ( 'NONE',  ( 53.10748497486810038, -50.46803858881009575, -76.94545506623299502 ) ) ;
#36333 = CARTESIAN_POINT ( 'NONE',  ( 15.91507200766546148, -15.77520395844511292, -41.53556505950739819 ) ) ;
#36334 = LINE ( 'NONE', #27955, #32821 ) ;
#36335 = CARTESIAN_POINT ( 'NONE',  ( 23.41669115755540176, -12.69245071001490111, -53.89097489251149398 ) ) ;
#36336 = CARTESIAN_POINT ( 'NONE',  ( 13.63995620566349842, -50.25144441423690012, -20.99590322994719926 ) ) ;
#36337 = LINE ( 'NONE', #48946, #46426 ) ;
#36338 = AXIS2_PLACEMENT_3D ( 'NONE', #8991, #29407, #33846 ) ;
#36339 = DIRECTION ( 'NONE',  ( 0.2771081164311157696, -0.6505467637364703570, -0.7071067811865504593 ) ) ;
#36340 = DIRECTION ( 'NONE',  ( 0.000000000000000000, 0.000000000000000000, 1.000000000000000000 ) ) ;
#36341 = CARTESIAN_POINT ( 'NONE',  ( 68.13393739769649926, -48.11618894467230234, -75.95000000000109708 ) ) ;
#36342 = CARTESIAN_POINT ( 'NONE',  ( 53.41693480164780539, 18.12090330447910347, -48.75416851879779756 ) ) ;
#36343 = AXIS2_PLACEMENT_3D ( 'NONE', #3979, #24372, #44061 ) ;
#36344 = DIRECTION ( 'NONE',  ( 0.7071067811865457964, -0.7071067811865492381, 0.000000000000000000 ) ) ;
#36345 = CARTESIAN_POINT ( 'NONE',  ( 22.60505408289549933, -18.42104331184100019, -50.97736833369739884 ) ) ;
#36346 = CARTESIAN_POINT ( 'NONE',  ( 8.223569788570660677, -15.61625877447020017, -68.79233150823709764 ) ) ;
#36347 = ORIENTED_EDGE ( 'NONE', *, *, #23030, .T. ) ;
#36348 = CARTESIAN_POINT ( 'NONE',  ( 14.56865064373200092, -51.74824662968959643, -75.61048537065330777 ) ) ;
#36349 = EDGE_CURVE ( 'NONE', #25361, #42283, #22146, .T. ) ;
#36350 = CARTESIAN_POINT ( 'NONE',  ( 47.30244424245569945, -54.71834446448549727, -54.68559897975160311 ) ) ;
#36351 = SURFACE_STYLE_FILL_AREA ( #32148 ) ;
#36352 = CARTESIAN_POINT ( 'NONE',  ( 1.633937397696199056, -15.61618894467930119, -7.139181489322110608 ) ) ;
#36353 = CARTESIAN_POINT ( 'NONE',  ( 65.03603135424580728, -29.76883965895079953, -19.52361391316370032 ) ) ;
#36354 = EDGE_CURVE ( 'NONE', #20085, #47128, #19382, .T. ) ;
#36355 = CARTESIAN_POINT ( 'NONE',  ( 18.31496508388832822, -7.941593517220971066, -55.09610085757195463 ) ) ;
#36356 = CARTESIAN_POINT ( 'NONE',  ( 55.36020812945222502, -46.03748402870435541, -16.50346261846816631 ) ) ;
#36357 = EDGE_CURVE ( 'NONE', #6962, #434, #44998, .T. ) ;
#36358 = CARTESIAN_POINT ( 'NONE',  ( 11.73919149118469996, 34.19054207972979498, -18.11861173564810201 ) ) ;
#36359 = AXIS2_PLACEMENT_3D ( 'NONE', #36155, #7360, #48218 ) ;
#36361 = CARTESIAN_POINT ( 'NONE',  ( 12.14990264437689227, -22.52876680156642308, -74.17433492201509182 ) ) ;
#36360 = DIRECTION ( 'NONE',  ( 0.000000000000000000, 0.000000000000000000, 1.000000000000000000 ) ) ;
#36362 = CARTESIAN_POINT ( 'NONE',  ( 17.21347160910390173, -53.11618894467930119, -76.14999999999999147 ) ) ;
#36363 = CARTESIAN_POINT ( 'NONE',  ( 48.42745381579229758, 22.84070070992420298, -54.64141748400979992 ) ) ;
#36364 = ORIENTED_EDGE ( 'NONE', *, *, #35909, .T. ) ;
#36365 = CARTESIAN_POINT ( 'NONE',  ( 53.51329535007300109, -49.35893701318239835, -49.05665458397329814 ) ) ;
#36366 = ORIENTED_EDGE ( 'NONE', *, *, #40536, .F. ) ;
#36367 = LINE ( 'NONE', #44242, #13671 ) ;
#36368 = LINE ( 'NONE', #27221, #44439 ) ;
#36369 = CARTESIAN_POINT ( 'NONE',  ( 56.91872543024629749, -50.64361015893049967, -53.86107397448480327 ) ) ;
#36371 = CARTESIAN_POINT ( 'NONE',  ( 54.07036167138819849, 17.11098462788829977, -26.64338358489850123 ) ) ;
#36370 = CARTESIAN_POINT ( 'NONE',  ( 82.53147610877040563, 13.90223449766140007, -46.79182873648620244 ) ) ;
#36372 = CARTESIAN_POINT ( 'NONE',  ( 16.22559063631150167, -8.563944026890579764, -67.95695684075589327 ) ) ;
#36373 = CARTESIAN_POINT ( 'NONE',  ( 53.02879948416539690, 18.37809327181799901, -49.09530617495999394 ) ) ;
#36374 = CARTESIAN_POINT ( 'NONE',  ( 57.22186383486660333, -45.12778674492059849, -17.46691603967050099 ) ) ;
#36375 = FACE_OUTER_BOUND ( 'NONE', #20831, .T. ) ;
#36376 = ORIENTED_EDGE ( 'NONE', *, *, #45568, .F. ) ;
#36377 =( GEOMETRIC_REPRESENTATION_CONTEXT ( 3 ) GLOBAL_UNCERTAINTY_ASSIGNED_CONTEXT ( ( #30032 ) ) GLOBAL_UNIT_ASSIGNED_CONTEXT ( ( #38433, #36036, #31318 ) ) REPRESENTATION_CONTEXT ( 'NONE', 'WORKASPACE' ) );
#36378 = EDGE_CURVE ( 'NONE', #11300, #16107, #28735, .T. ) ;
#36379 = ORIENTED_EDGE ( 'NONE', *, *, #8675, .T. ) ;
#36380 = CARTESIAN_POINT ( 'NONE',  ( 11.10018451884070068, -65.04197989738689500, -17.19464565520879873 ) ) ;
#36381 = CARTESIAN_POINT ( 'NONE',  ( 12.86387693150249945, 34.27459056366519974, -47.65248693957870074 ) ) ;
#36382 = DIRECTION ( 'NONE',  ( -1.000000000000000000, 0.000000000000000000, 0.000000000000000000 ) ) ;
#36383 = DIRECTION ( 'NONE',  ( -0.7089970498513425978, -0.7052114458104695727, -4.077736999999996963E-16 ) ) ;
#36384 = CARTESIAN_POINT ( 'NONE',  ( 10.73247463706263893, -64.25243278916070722, -23.51162531654635046 ) ) ;
#36385 = DIRECTION ( 'NONE',  ( 0.000000000000000000, 0.000000000000000000, -1.000000000000000000 ) ) ;
#36386 = ORIENTED_EDGE ( 'NONE', *, *, #24263, .T. ) ;
#36387 = CARTESIAN_POINT ( 'NONE',  ( 10.90462426371155757, 24.04048178864984209, -44.90618065568715167 ) ) ;
#36388 = CARTESIAN_POINT ( 'NONE',  ( 11.13393739769619906, -63.20626152654000407, -43.91299082816230026 ) ) ;
#36389 = CARTESIAN_POINT ( 'NONE',  ( 20.11806024363774625, -22.52871719054864386, -59.84102336720449955 ) ) ;
#36390 = CARTESIAN_POINT ( 'NONE',  ( 24.04492193170107939, -15.63426495621359358, -43.79305225079668418 ) ) ;
#36391 = CARTESIAN_POINT ( 'NONE',  ( 63.49388541862201407, 1.387412027389909985, -62.60488565353588797 ) ) ;
#36392 = CARTESIAN_POINT ( 'NONE',  ( 9.807770915243924748, -20.47786536020769077, -44.29935507129472683 ) ) ;
#36393 = VERTEX_POINT ( 'NONE', #8840 ) ;
#36394 = B_SPLINE_CURVE_WITH_KNOTS ( 'NONE', 3,
 ( #12921, #28875, #26235, #34353, #5572, #13942, #17618, #42241, #22038, #45653, #18377, #30169, #41981, #50100, #38574, #10272, #2393, #22300 ),
 .UNSPECIFIED., .F., .F.,
 ( 4, 2, 2, 2, 2, 2, 2, 2, 4 ),
 ( 0.5000012918607925627, 0.5625011303781934924, 0.6250009688955943110, 0.6875008074129951297, 0.7500006459303960593, 0.8125004844477969890, 0.8750003229651980297, 0.9375001614825990703, 1.000000000000000000 ),
 .UNSPECIFIED. ) ;
#36395 = DIRECTION ( 'NONE',  ( 0.000000000000000000, 0.000000000000000000, -1.000000000000000000 ) ) ;
#36396 = CARTESIAN_POINT ( 'NONE',  ( 10.11211546542380013, 22.87009133999800170, -34.93361312117499295 ) ) ;
#36397 = CARTESIAN_POINT ( 'NONE',  ( 56.83258908092710016, -50.30522036972260480, -52.72698303625519856 ) ) ;
#36398 = CARTESIAN_POINT ( 'NONE',  ( 2.446837772604945727, -25.70616092178045875, -34.84133294386909085 ) ) ;
#36399 = EDGE_CURVE ( 'NONE', #32624, #1526, #24793, .T. ) ;
#36400 = CARTESIAN_POINT ( 'NONE',  ( 12.77254040467190066, -8.087329116576368548, -73.15866903151089673 ) ) ;
#36401 = CIRCLE ( 'NONE', #50678, 23.50000000000000000 ) ;
#36402 = DIRECTION ( 'NONE',  ( -1.000000000000000000, 0.000000000000000000, 0.000000000000000000 ) ) ;
#36403 = CARTESIAN_POINT ( 'NONE',  ( 55.93861191783509668, 19.62789642752380104, -74.87542895885140126 ) ) ;
#36404 = APPLICATION_PROTOCOL_DEFINITION ( 'draft international standard', 'automotive_design', 1998, #37159 ) ;
#36405 = CARTESIAN_POINT ( 'NONE',  ( 47.43575969855930197, -54.63575133606219936, -74.19794602913619030 ) ) ;
#36406 = ORIENTED_EDGE ( 'NONE', *, *, #29611, .T. ) ;
#36407 = AXIS2_PLACEMENT_3D ( 'NONE', #27325, #23126, #31498 ) ;
#36408 = CARTESIAN_POINT ( 'NONE',  ( 22.46248482608730157, -19.54762395644669937, -64.40959883343299452 ) ) ;
#36409 = DIRECTION ( 'NONE',  ( 0.000000000000000000, 0.000000000000000000, 1.000000000000000000 ) ) ;
#36410 = CARTESIAN_POINT ( 'NONE',  ( 11.67619456822290047, 33.65927054772580362, -23.88710972541020183 ) ) ;
#36411 = CARTESIAN_POINT ( 'NONE',  ( 46.88047926045639713, 22.77644039600379600, -75.76367657470891004 ) ) ;
#36412 = CARTESIAN_POINT ( 'NONE',  ( 70.99050876911339003, 1.383811055320669947, -60.94999999999999574 ) ) ;
#36413 = DIRECTION ( 'NONE',  ( 1.000000000000000000, 0.000000000000000000, 0.000000000000000000 ) ) ;
#36414 = EDGE_CURVE ( 'NONE', #32635, #12694, #32916, .T. ) ;
#36415 = CARTESIAN_POINT ( 'NONE',  ( 41.54743507844230521, -44.83695157103969819, -5.527281617101080791 ) ) ;
#36416 = CARTESIAN_POINT ( 'NONE',  ( 12.31509292275960021, 33.40570322225389788, -15.85496248756799709 ) ) ;
#36417 = CARTESIAN_POINT ( 'NONE',  ( 19.61369162610559869, -8.141295552874010966, -77.14635284413580507 ) ) ;
#36418 = EDGE_CURVE ( 'NONE', #41267, #5478, #42621, .T. ) ;
#36419 = CARTESIAN_POINT ( 'NONE',  ( 56.87436366836959678, -50.61618764704540041, -75.17316017584860788 ) ) ;
#36421 = CARTESIAN_POINT ( 'NONE',  ( 41.01311687426999697, -39.69858908207098125, -80.89458633909558216 ) ) ;
#36420 = DIRECTION ( 'NONE',  ( -1.000000000000000000, 0.000000000000000000, 0.000000000000000000 ) ) ;
#36422 = CARTESIAN_POINT ( 'NONE',  ( 63.08005232011719698, 0.8859637708054489691, -68.88406027352149863 ) ) ;
#36423 = CARTESIAN_POINT ( 'NONE',  ( 61.49092242389700402, 13.92534852783209942, -46.59258487662240356 ) ) ;
#36424 = CARTESIAN_POINT ( 'NONE',  ( -0.08095109960796090243, -61.40204063968959503, -48.64221216126409786 ) ) ;
#36425 = ORIENTED_EDGE ( 'NONE', *, *, #20197, .T. ) ;
#36426 = CARTESIAN_POINT ( 'NONE',  ( 52.90855289046140086, -49.61963672099809486, -48.71990427169439641 ) ) ;
#36427 = CARTESIAN_POINT ( 'NONE',  ( 60.64762851420100276, -45.11618901004540305, -26.44263184015450108 ) ) ;
#36428 = AXIS2_PLACEMENT_3D ( 'NONE', #15751, #19925, #43791 ) ;
#36429 = CARTESIAN_POINT ( 'NONE',  ( 9.221335198055678362, -19.60018521617414322, -72.62567728624490826 ) ) ;
#36430 = CARTESIAN_POINT ( 'NONE',  ( 56.87603334809730171, 14.74005630904309960, -26.24549249933449957 ) ) ;
#36431 = CARTESIAN_POINT ( 'NONE',  ( 9.325642639948160451, -13.77508026015089904, -37.53688731232609399 ) ) ;
#36432 = CARTESIAN_POINT ( 'NONE',  ( 50.45186278194579899, 18.80186278247199994, -76.14999999999999147 ) ) ;
#36433 = CARTESIAN_POINT ( 'NONE',  ( 53.10876373110949800, 18.29129782088910261, -48.93018544281289905 ) ) ;
#36434 = CARTESIAN_POINT ( 'NONE',  ( 71.06936022730370439, 1.374300485541529948, -70.43861994117489189 ) ) ;
#36435 = PLANE ( 'NONE',  #12546 ) ;
#36436 = CARTESIAN_POINT ( 'NONE',  ( 68.83419609097690284, -44.96193019449670203, -12.58053924570920046 ) ) ;
#36437 = AXIS2_PLACEMENT_3D ( 'NONE', #51215, #3518, #11385 ) ;
#36438 = ORIENTED_EDGE ( 'NONE', *, *, #27373, .F. ) ;
#36439 = CARTESIAN_POINT ( 'NONE',  ( -11.59939519444589529, 2.705059169678001307, -49.87766025524430091 ) ) ;
#36440 = B_SPLINE_CURVE_WITH_KNOTS ( 'NONE', 3,
 ( #48206, #12309, #28268, #44269, #8375, #24845, #17019, #1025, #5229, #29053, #40342, #4436, #44529, #12832, #48728, #49252, #45048, #9418, #17276, #24324 ),
 .UNSPECIFIED., .F., .F.,
 ( 4, 2, 2, 2, 2, 2, 2, 2, 2, 4 ),
 ( 0.000000000000000000, 0.08842663232653856509, 0.2261948956664324439, 0.3749999999999999445, 0.5000000000000005551, 0.5625000000000004441, 0.6625000000000004219, 0.7983826544682063320, 0.9363829142882441614, 1.000000000000000000 ),
 .UNSPECIFIED. ) ;
#36441 = CARTESIAN_POINT ( 'NONE',  ( 47.68328361370659962, -54.50666145107209815, -54.95376626878769599 ) ) ;
#36442 = CARTESIAN_POINT ( 'NONE',  ( -6.441449436378089644, 14.95323763072200052, -4.672284527633559392 ) ) ;
#36443 = CARTESIAN_POINT ( 'NONE',  ( 20.29259189943645580, -21.02752101800459172, -70.74448910382146494 ) ) ;
#36444 = CARTESIAN_POINT ( 'NONE',  ( 57.72747068869959719, 18.67975836146520052, -52.38194251579410121 ) ) ;
#36445 = CARTESIAN_POINT ( 'NONE',  ( 71.19853741683878923, 1.383922910988889976, -60.98106092919370269 ) ) ;
#36446 = CARTESIAN_POINT ( 'NONE',  ( 68.13393739769620083, 16.88381105532069881, -75.00000000000000000 ) ) ;
#36447 = CARTESIAN_POINT ( 'NONE',  ( 71.60533839042560089, 1.134292167764330062, -60.81357835167419523 ) ) ;
#36448 = CARTESIAN_POINT ( 'NONE',  ( 11.27214737950822077, -21.94226950413872146, -72.21594989029324552 ) ) ;
#36449 = CARTESIAN_POINT ( 'NONE',  ( 64.96708350509699414, 1.267233196669030004, -70.54626486029009413 ) ) ;
#36450 = ORIENTED_EDGE ( 'NONE', *, *, #12770, .T. ) ;
#36451 = EDGE_LOOP ( 'NONE', ( #21119, #51757, #45285, #47822, #47735 ) ) ;
#36452 = CARTESIAN_POINT ( 'NONE',  ( -6.866062602303800055, -15.61618894467929586, -14.65000000000000036 ) ) ;
#36453 = CARTESIAN_POINT ( 'NONE',  ( 68.13393739769627189, -15.41618894467990586, -28.20067248431511331 ) ) ;
#36454 = ORIENTED_EDGE ( 'NONE', *, *, #5133, .F. ) ;
#36455 = DIRECTION ( 'NONE',  ( 0.000000000000000000, 0.000000000000000000, -1.000000000000000000 ) ) ;
#36456 = CARTESIAN_POINT ( 'NONE',  ( 22.41796512503769989, 0.7774003680457489684, -74.14999999999999147 ) ) ;
#36457 = DIRECTION ( 'NONE',  ( -1.000000000000000000, 0.000000000000000000, 0.000000000000000000 ) ) ;
#36458 = ORIENTED_EDGE ( 'NONE', *, *, #38935, .F. ) ;
#36459 = CARTESIAN_POINT ( 'NONE',  ( 55.80143501159700747, -48.88742250280260038, -53.84278118897339738 ) ) ;
#36460 = CARTESIAN_POINT ( 'NONE',  ( 42.13803780587668513, 6.413235773433889619, -79.62945665582455490 ) ) ;
#36461 = CARTESIAN_POINT ( 'NONE',  ( 24.04461175216078317, -15.61617380819018663, -65.50766589912049653 ) ) ;
#36462 = EDGE_CURVE ( 'NONE', #41688, #36323, #16291, .T. ) ;
#36463 = CARTESIAN_POINT ( 'NONE',  ( 8.406715080065760404, -18.49242873124940090, -40.67890729542689598 ) ) ;
#36464 = CIRCLE ( 'NONE', #23914, 3.000000000000001776 ) ;
#36465 = EDGE_CURVE ( 'NONE', #29849, #11777, #22970, .T. ) ;
#36466 = CARTESIAN_POINT ( 'NONE',  ( 45.22285809734859896, 2.278851623075559996, -34.76403944585129580 ) ) ;
#36467 = CARTESIAN_POINT ( 'NONE',  ( 41.87134808728646362, -37.60294274168957429, -80.96289175035070684 ) ) ;
#36468 = EDGE_CURVE ( 'NONE', #18307, #44616, #47289, .T. ) ;
#36469 = VERTEX_POINT ( 'NONE', #2524 ) ;
#36470 = CARTESIAN_POINT ( 'NONE',  ( 17.16956147491267615, -23.52717800495802791, -42.25066452978246190 ) ) ;
#36471 = CARTESIAN_POINT ( 'NONE',  ( 13.40559671880919979, -8.258002636450779477, -79.39947069499679344 ) ) ;
#36472 = CIRCLE ( 'NONE', #45704, 21.19999999999999929 ) ;
#36473 = CARTESIAN_POINT ( 'NONE',  ( 43.05627104033619901, 14.74862409592560120, -7.622843372308340193 ) ) ;
#36474 = VECTOR ( 'NONE', #44143, 1000.000000000000114 ) ;
#36475 = CARTESIAN_POINT ( 'NONE',  ( 14.38413149323399942, 20.42705216602020357, -75.51240970683940645 ) ) ;
#36476 = DIRECTION ( 'NONE',  ( 3.191443934968489902E-12, -1.000000000000000000, -2.813979115193090113E-11 ) ) ;
#36477 = CARTESIAN_POINT ( 'NONE',  ( 10.03393739769619941, -15.61618894467929941, 2.750000000000000000 ) ) ;
#36478 = CARTESIAN_POINT ( 'NONE',  ( 63.99083253892909084, 1.458411868502019981, -69.65665569611660146 ) ) ;
#36479 = CARTESIAN_POINT ( 'NONE',  ( 10.82531766377809923, -21.92501428935559815, -40.23033096848919854 ) ) ;
#36480 = ADVANCED_FACE ( 'NONE', ( #2002 ), #37909, .F. ) ;
#36481 = ORIENTED_EDGE ( 'NONE', *, *, #9876, .F. ) ;
#36482 = CARTESIAN_POINT ( 'NONE',  ( 53.04388686265919972, -49.43765248974969495, -27.51561755457979785 ) ) ;
#36483 = CARTESIAN_POINT ( 'NONE',  ( 14.79307399752550012, -50.68537516129959641, -20.88395191203650114 ) ) ;
#36484 = CARTESIAN_POINT ( 'NONE',  ( 50.03007040746459921, -36.85417771443089663, -76.14999999999999147 ) ) ;
#36485 = CARTESIAN_POINT ( 'NONE',  ( 9.807868667392284578, -20.47799079033555003, -64.58399863705557209 ) ) ;
#36486 = CARTESIAN_POINT ( 'NONE',  ( 75.45209363691283500, 12.55602155768010952, -13.50097026880459339 ) ) ;
#36487 = DIRECTION ( 'NONE',  ( -1.000000000000000000, 0.000000000000000000, 0.000000000000000000 ) ) ;
#36488 = EDGE_LOOP ( 'NONE', ( #18323, #3409, #18430, #6554, #37737, #30322 ) ) ;
#36489 = CARTESIAN_POINT ( 'NONE',  ( -7.450541063502280181, -45.60837410880110099, -5.667773980459688943 ) ) ;
#36490 = CARTESIAN_POINT ( 'NONE',  ( 47.41680556257099965, 23.40808140825799910, -54.70932877154390184 ) ) ;
#36491 = VECTOR ( 'NONE', #18538, 1000.000000000000000 ) ;
#36492 = FACE_OUTER_BOUND ( 'NONE', #41705, .T. ) ;
#36493 = CARTESIAN_POINT ( 'NONE',  ( 63.46757340380580814, 1.384887413063070172, -62.68544474927200127 ) ) ;
#36494 = CARTESIAN_POINT ( 'NONE',  ( 13.58674547247159836, 19.15744735761279927, -21.11651667334109916 ) ) ;
#36495 = CARTESIAN_POINT ( 'NONE',  ( 54.99093226003984114, 16.49184862051891898, -26.61807943321322156 ) ) ;
#36496 = CARTESIAN_POINT ( 'NONE',  ( 11.78395113718259957, 34.19034018254340168, -17.88069380536899899 ) ) ;
#36497 = DIRECTION ( 'NONE',  ( 0.000000000000000000, 0.000000000000000000, -1.000000000000000000 ) ) ;
#36498 = CARTESIAN_POINT ( 'NONE',  ( 22.46011041234203987, -10.75452168438129164, -61.58399571921993498 ) ) ;
#36499 = CARTESIAN_POINT ( 'NONE',  ( 8.222930619450961487, -15.61639179890759976, -64.50766849176299900 ) ) ;
#36500 = CARTESIAN_POINT ( 'NONE',  ( 53.59080506099410002, -49.40678926384370584, -49.22648751777380483 ) ) ;
#36501 = CIRCLE ( 'NONE', #49107, 50.00000000000000000 ) ;
#36502 = DIRECTION ( 'NONE',  ( 1.000000000000000000, 0.000000000000000000, 0.000000000000000000 ) ) ;
#36503 = CARTESIAN_POINT ( 'NONE',  ( 64.89503925317040967, 1.371509258145880095, -60.97885864891310348 ) ) ;
#36504 = CARTESIAN_POINT ( 'NONE',  ( 17.90951780689729844, -52.52234239888379363, -75.96669286083250938 ) ) ;
#36505 = CARTESIAN_POINT ( 'NONE',  ( 50.03007040746459921, 5.621799825072190337, -76.14999999999999147 ) ) ;
#36506 =( BOUNDED_CURVE ( )  B_SPLINE_CURVE ( 3, ( #18395, #30703, #6613, #34373 ),
 .UNSPECIFIED., .F., .T. ) 
 B_SPLINE_CURVE_WITH_KNOTS ( ( 4, 4 ),
 ( 2.356194490192396351, 3.141592653589795781 ),
 .UNSPECIFIED. ) 
 CURVE ( )  GEOMETRIC_REPRESENTATION_ITEM ( )  RATIONAL_B_SPLINE_CURVE ( ( 1.000000000000000000, 0.9492530216741973392, 0.9492530216741973392, 1.000000000000000000 ) ) 
 REPRESENTATION_ITEM ( '' )  );
#36507 = CARTESIAN_POINT ( 'NONE',  ( 12.84391639521409978, -21.85461860611620111, -81.10729939731689342 ) ) ;
#36508 = FACE_OUTER_BOUND ( 'NONE', #38612, .T. ) ;
#36509 = ORIENTED_EDGE ( 'NONE', *, *, #26068, .T. ) ;
#36510 = DIRECTION ( 'NONE',  ( 1.000000000000000000, 0.000000000000000000, 0.000000000000000000 ) ) ;
#36511 = CARTESIAN_POINT ( 'NONE',  ( 9.280056505173840620, 31.92632265388400370, -46.53174294612239947 ) ) ;
#36512 = DIRECTION ( 'NONE',  ( 1.000000000000000000, 0.000000000000000000, 0.000000000000000000 ) ) ;
#36513 = VECTOR ( 'NONE', #14791, 1000.000000000000000 ) ;
#36514 = CARTESIAN_POINT ( 'NONE',  ( 66.98667323035849108, -30.07752074129929909, -17.21848267116260089 ) ) ;
#36515 = ORIENTED_EDGE ( 'NONE', *, *, #1221, .T. ) ;
#36516 = CARTESIAN_POINT ( 'NONE',  ( 18.50593879142590126, 20.63771170940629673, -75.29799846200430125 ) ) ;
#36517 = VERTEX_POINT ( 'NONE', #9867 ) ;
#36518 = ORIENTED_EDGE ( 'NONE', *, *, #40283, .F. ) ;
#36519 = ORIENTED_EDGE ( 'NONE', *, *, #31789, .T. ) ;
#36520 = CARTESIAN_POINT ( 'NONE',  ( 11.80925469686000007, -65.15757697063340004, -46.63650775655830216 ) ) ;
#36521 = DIRECTION ( 'NONE',  ( 1.000000000000000000, 2.460964292799963328E-14, 0.000000000000000000 ) ) ;
#36522 = CARTESIAN_POINT ( 'NONE',  ( 21.76556302292190281, -19.92121040802560117, -81.23899999999999011 ) ) ;
#36523 = CARTESIAN_POINT ( 'NONE',  ( -11.80944000494499768, -34.05870648691990255, -45.03554556751409166 ) ) ;
#36524 = ORIENTED_EDGE ( 'NONE', *, *, #22738, .F. ) ;
#36525 = ORIENTED_EDGE ( 'NONE', *, *, #19264, .F. ) ;
#36526 = CARTESIAN_POINT ( 'NONE',  ( 12.21895745972638814, 33.73857834413064438, -16.28177270833691992 ) ) ;
#36527 = ORIENTED_EDGE ( 'NONE', *, *, #13276, .F. ) ;
#36528 = CARTESIAN_POINT ( 'NONE',  ( 11.32194239187774443, -64.37711270544450315, -24.04756285534320526 ) ) ;
#36529 = ADVANCED_FACE ( 'NONE', ( #18754 ), #22175, .T. ) ;
#36530 = CARTESIAN_POINT ( 'NONE',  ( 14.74689884928131356, -52.86909450409968514, -76.12392058103056058 ) ) ;
#36531 = DIRECTION ( 'NONE',  ( -1.000000000000000000, 0.000000000000000000, 0.000000000000000000 ) ) ;
#36532 = ADVANCED_FACE ( 'NONE', ( #14832 ), #17983, .T. ) ;
#36533 = ORIENTED_EDGE ( 'NONE', *, *, #35887, .T. ) ;
#36534 = VERTEX_POINT ( 'NONE', #30795 ) ;
#36535 = FACE_OUTER_BOUND ( 'NONE', #35175, .T. ) ;
#36536 = LINE ( 'NONE', #47837, #824 ) ;
#36537 = CARTESIAN_POINT ( 'NONE',  ( 70.56366411589620213, 13.88381105527240145, -14.05866322138230018 ) ) ;
#36538 = VECTOR ( 'NONE', #34556, 1000.000000000000000 ) ;
#36539 = CARTESIAN_POINT ( 'NONE',  ( 48.07720450831519798, 14.71742899414569905, -10.94662572293029967 ) ) ;
#36540 = CARTESIAN_POINT ( 'NONE',  ( 38.67452568954060155, 4.883811055320659733, -81.65000000000000568 ) ) ;
#36541 = CARTESIAN_POINT ( 'NONE',  ( -9.444509380504280571, 12.50088983498840101, -5.686455919239249646 ) ) ;
#36542 = CARTESIAN_POINT ( 'NONE',  ( -2.328172376426727475, -49.80836506692148191, -5.964500925750916061 ) ) ;
#36543 = AXIS2_PLACEMENT_3D ( 'NONE', #33023, #43629, #31799 ) ;
#36544 = CARTESIAN_POINT ( 'NONE',  ( 57.59507381935979708, 14.35784622530070109, -26.21889295923039853 ) ) ;
#36545 = CARTESIAN_POINT ( 'NONE',  ( 23.54765475985599821, -13.04256444658469860, -59.18114938323410001 ) ) ;
#36546 = EDGE_CURVE ( 'NONE', #7583, #40660, #46022, .T. ) ;
#36547 = ORIENTED_EDGE ( 'NONE', *, *, #44547, .T. ) ;
#36548 = CARTESIAN_POINT ( 'NONE',  ( 53.59007319642030609, 18.17385789206429791, -49.22505640095140222 ) ) ;
#36549 = CARTESIAN_POINT ( 'NONE',  ( 24.04513741079867017, -15.61618875311435417, -79.79232954107749265 ) ) ;
#36550 = CARTESIAN_POINT ( 'NONE',  ( 52.10267382254159685, -33.11618894467940066, -20.65000000000000213 ) ) ;
#36551 = EDGE_CURVE ( 'NONE', #29481, #13261, #46302, .T. ) ;
#36552 = CARTESIAN_POINT ( 'NONE',  ( 72.43587670424329872, 1.060191324942699964, -69.83271228958450649 ) ) ;
#36553 = CARTESIAN_POINT ( 'NONE',  ( 42.93292300981802612, -39.85965248063442345, -71.82398325773546333 ) ) ;
#36554 = CARTESIAN_POINT ( 'NONE',  ( 8.222942234697445230, -16.65177182868387717, -36.75066472735249334 ) ) ;
#36555 = CARTESIAN_POINT ( 'NONE',  ( 13.32695066795020011, 18.94061603315460118, -21.04411651763339819 ) ) ;
#36556 = DIRECTION ( 'NONE',  ( 1.000000000000000000, 0.000000000000000000, 0.000000000000000000 ) ) ;
#36557 = CARTESIAN_POINT ( 'NONE',  ( 49.20993668789899544, -53.61219117315689431, -54.26298610208100115 ) ) ;
#36558 = LINE ( 'NONE', #39992, #50739 ) ;
#36559 = AXIS2_PLACEMENT_3D ( 'NONE', #41322, #24275, #1237 ) ;
#36560 = CARTESIAN_POINT ( 'NONE',  ( 11.06214720078926739, -21.70954254531401872, -34.22858903880150905 ) ) ;
#36561 = CARTESIAN_POINT ( 'NONE',  ( -0.4123484725610440105, 14.05881538531380137, -35.12503119152799513 ) ) ;
#36562 = EDGE_LOOP ( 'NONE', ( #3376, #10433, #48177, #36117 ) ) ;
#36563 = CARTESIAN_POINT ( 'NONE',  ( 20.39734384171130088, -9.506355900195050168, -46.76127109678569838 ) ) ;
#36564 = CARTESIAN_POINT ( 'NONE',  ( 64.01157812772038369, 1.056850087111250058, -61.28959142989100428 ) ) ;
#36565 = EDGE_LOOP ( 'NONE', ( #30662, #34093, #1715, #28401, #17297, #4695 ) ) ;
#36566 = CARTESIAN_POINT ( 'NONE',  ( 55.40393386216474170, -45.11618894460369944, -14.52023105806692449 ) ) ;
#36567 = CARTESIAN_POINT ( 'NONE',  ( 60.90533690232570763, -45.43405919436199980, -47.09747221447039323 ) ) ;
#36568 = CARTESIAN_POINT ( 'NONE',  ( 57.18371624257370200, 19.38400875315740279, -53.90359198932329576 ) ) ;
#36569 = CARTESIAN_POINT ( 'NONE',  ( 43.91475033527959937, -43.54611815821230891, -5.093413304872340674 ) ) ;
#36571 = CARTESIAN_POINT ( 'NONE',  ( 24.04493740182211425, -16.65173924940748051, -77.83399516818887776 ) ) ;
#36570 = CARTESIAN_POINT ( 'NONE',  ( 42.91356006583662008, 8.625454777037399268, -71.91745137691370360 ) ) ;
#36572 = DIRECTION ( 'NONE',  ( -0.5720614028176880250, -0.7071067811865480168, -0.4156269377774474139 ) ) ;
#36573 = DIRECTION ( 'NONE',  ( 0.000000000000000000, 1.000000000000000000, 0.000000000000000000 ) ) ;
#36574 = VERTEX_POINT ( 'NONE', #10912 ) ;
#36575 = CARTESIAN_POINT ( 'NONE',  ( 84.02215818083939780, -44.41825355194460201, -47.25304732090640414 ) ) ;
#36576 = ORIENTED_EDGE ( 'NONE', *, *, #48613, .T. ) ;
#36577 = ORIENTED_EDGE ( 'NONE', *, *, #33749, .T. ) ;
#36578 = ORIENTED_EDGE ( 'NONE', *, *, #14670, .T. ) ;
#36579 = CARTESIAN_POINT ( 'NONE',  ( 61.37876400707010305, -45.32826204942830373, -47.24547059479539968 ) ) ;
#36580 = CARTESIAN_POINT ( 'NONE',  ( 53.02878878271380358, -49.61118882884069592, -49.09724721214779919 ) ) ;
#36581 = DIRECTION ( 'NONE',  ( 0.000000000000000000, 1.000000000000000000, 0.000000000000000000 ) ) ;
#36582 = CARTESIAN_POINT ( 'NONE',  ( 76.40558626391258201, -11.02804892670111059, -12.82057542108343640 ) ) ;
#36583 = CARTESIAN_POINT ( 'NONE',  ( 54.00935231632030309, -51.82239677024340097, -54.07713036160949827 ) ) ;
#36584 = TOROIDAL_SURFACE ( 'NONE', #31565, 36.00000000000000000, 2.000000000000000000 ) ;
#36585 = ORIENTED_EDGE ( 'NONE', *, *, #1007, .T. ) ;
#36586 = ORIENTED_EDGE ( 'NONE', *, *, #4960, .T. ) ;
#36587 = CARTESIAN_POINT ( 'NONE',  ( 49.30929069640199458, 22.32182524534569978, -54.21028152426279689 ) ) ;
#36588 = CARTESIAN_POINT ( 'NONE',  ( 52.13393739769618662, -0.3411889446793609504, -65.65000000000000568 ) ) ;
#36589 = CYLINDRICAL_SURFACE ( 'NONE', #11946, 13.50000000000000178 ) ;
#36590 = EDGE_CURVE ( 'NONE', #3072, #28015, #42882, .T. ) ;
#36591 = CARTESIAN_POINT ( 'NONE',  ( 8.802047646820330584, -63.20618355599279425, -46.67014429624759941 ) ) ;
#36592 = CARTESIAN_POINT ( 'NONE',  ( 24.04492500195047455, -15.60001557533511019, -59.79167491129597067 ) ) ;
#36593 = CARTESIAN_POINT ( 'NONE',  ( 11.13393739769619906, -63.11543068638779630, -43.74348518090240390 ) ) ;
#36594 = EDGE_LOOP ( 'NONE', ( #7438, #39193, #30066, #10315 ) ) ;
#36595 = CARTESIAN_POINT ( 'NONE',  ( 14.34417030258640047, -52.11618895234509807, -23.15000000571859928 ) ) ;
#36596 = CARTESIAN_POINT ( 'NONE',  ( 53.44459314798190519, -50.52658309343919996, -77.05819699307679116 ) ) ;
#36597 = CARTESIAN_POINT ( 'NONE',  ( 64.79174514991440503, 0.8925687589132599298, -70.63296852923029689 ) ) ;
#36598 = CARTESIAN_POINT ( 'NONE',  ( 8.222955699658124118, -16.65187040858989675, -54.46600195242484688 ) ) ;
#36599 = CARTESIAN_POINT ( 'NONE',  ( 11.28616805192099903, -21.78756480114309824, -66.72444172481789337 ) ) ;
#36600 = DIRECTION ( 'NONE',  ( 0.000000000000000000, 0.000000000000000000, -1.000000000000000000 ) ) ;
#36601 = CARTESIAN_POINT ( 'NONE',  ( 41.34908647067909726, -44.75253358332089704, -5.352709625395250193 ) ) ;
#36602 = DIRECTION ( 'NONE',  ( 1.000000000000000000, 2.460964292799963328E-14, 0.000000000000000000 ) ) ;
#36603 = CARTESIAN_POINT ( 'NONE',  ( 61.28189544230230013, -45.60274550571363505, -47.67949669012001834 ) ) ;
#36604 = DIRECTION ( 'NONE',  ( -1.000000000000000000, 0.000000000000000000, 0.000000000000000000 ) ) ;
#36605 = CARTESIAN_POINT ( 'NONE',  ( 63.77399527780870869, 1.113947854059440079, -69.76572286218529939 ) ) ;
#36606 = FACE_OUTER_BOUND ( 'NONE', #48984, .T. ) ;
#36607 = ORIENTED_EDGE ( 'NONE', *, *, #13707, .F. ) ;
#36608 = CARTESIAN_POINT ( 'NONE',  ( 14.66320343668420101, -52.01451994755070274, -75.82251062550810161 ) ) ;
#36609 = CARTESIAN_POINT ( 'NONE',  ( 47.31046770529280110, -54.71181978270450230, -54.66537007426079953 ) ) ;
#36610 = EDGE_CURVE ( 'NONE', #42739, #29610, #13802, .T. ) ;
#36611 = CARTESIAN_POINT ( 'NONE',  ( 55.52753008314243033, -15.61618894467857110, -5.093415854460129566 ) ) ;
#36612 = CARTESIAN_POINT ( 'NONE',  ( 19.13393739769620083, -49.61618894467939356, -35.14999999999999858 ) ) ;
#36613 = AXIS2_PLACEMENT_3D ( 'NONE', #27636, #44926, #40990 ) ;
#36614 = CARTESIAN_POINT ( 'NONE',  ( 22.81209844268250109, -13.20389820966570049, -32.14999999999999858 ) ) ;
#36615 = DIRECTION ( 'NONE',  ( 0.000000000000000000, 0.000000000000000000, -1.000000000000000000 ) ) ;
#36616 = CARTESIAN_POINT ( 'NONE',  ( 47.66469316585200033, -54.52497965065870034, -55.13865833718669762 ) ) ;
#36618 = CARTESIAN_POINT ( 'NONE',  ( 11.28396737011271433, 33.05014951446679561, -24.06589613998641042 ) ) ;
#36617 = FACE_OUTER_BOUND ( 'NONE', #41103, .T. ) ;
#36619 = AXIS2_PLACEMENT_3D ( 'NONE', #18146, #41475, #33857 ) ;
#36620 = CARTESIAN_POINT ( 'NONE',  ( 56.45386930879750054, 19.54637801841160183, -53.73844136669490013 ) ) ;
#36621 = CARTESIAN_POINT ( 'NONE',  ( 42.53968774895909633, 12.99877935903693604, -5.088323967986317697 ) ) ;
#36622 = CARTESIAN_POINT ( 'NONE',  ( 48.58882027194280084, 22.89737091365429933, -55.21892047541300741 ) ) ;
#36623 = ORIENTED_EDGE ( 'NONE', *, *, #43459, .F. ) ;
#36624 = CARTESIAN_POINT ( 'NONE',  ( 17.25281598583540088, -22.57971318743560118, -67.29646813280298545 ) ) ;
#36625 = ORIENTED_EDGE ( 'NONE', *, *, #19210, .F. ) ;
#36626 = DIRECTION ( 'NONE',  ( 0.000000000000000000, 0.000000000000000000, -1.000000000000000000 ) ) ;
#36627 = CARTESIAN_POINT ( 'NONE',  ( 33.38393739769599478, 10.88381105532080007, -35.14999999999999858 ) ) ;
#36628 = DIRECTION ( 'NONE',  ( 0.000000000000000000, 0.000000000000000000, 1.000000000000000000 ) ) ;
#36630 = CARTESIAN_POINT ( 'NONE',  ( 52.61201187087419839, 18.58180915112900067, -28.06837461485350005 ) ) ;
#36629 = CARTESIAN_POINT ( 'NONE',  ( 83.94975121583560451, 13.06368244423120117, -46.94103493214879563 ) ) ;
#36631 = CARTESIAN_POINT ( 'NONE',  ( 9.083428079434199276, -15.43486864872139996, -61.46100449353919259 ) ) ;
#36632 = DIRECTION ( 'NONE',  ( 0.1564344650402237358, -0.9876883405951387696, 0.000000000000000000 ) ) ;
#36633 = CARTESIAN_POINT ( 'NONE',  ( 56.17636210926850282, -45.40492621701339715, -16.65164697100100000 ) ) ;
#36634 = CARTESIAN_POINT ( 'NONE',  ( 23.83903838438579115, -17.68686092435233803, -79.87566697560022533 ) ) ;
#36635 = ORIENTED_EDGE ( 'NONE', *, *, #10432, .F. ) ;
#36636 = ORIENTED_EDGE ( 'NONE', *, *, #47061, .T. ) ;
#36637 = CARTESIAN_POINT ( 'NONE',  ( 12.01906023896859921, -65.22423223438029538, -16.79721265542299946 ) ) ;
#36638 = CARTESIAN_POINT ( 'NONE',  ( 10.55882748421930017, 32.87867648022200484, -46.00924270197130284 ) ) ;
#36639 = CARTESIAN_POINT ( 'NONE',  ( 61.19898206724911915, -45.31222199280929885, -47.06086663119204871 ) ) ;
#36640 = CARTESIAN_POINT ( 'NONE',  ( 52.74267556208770458, -49.67209455079629521, -48.33969704999849881 ) ) ;
#36641 = CARTESIAN_POINT ( 'NONE',  ( 16.13393739769620083, -15.61618894467929941, -32.14999999999999858 ) ) ;
#36642 = EDGE_LOOP ( 'NONE', ( #23309, #51067, #37488, #9157 ) ) ;
#36643 = CARTESIAN_POINT ( 'NONE',  ( 0.7740850027469919903, -51.13355895648079752, -34.09234346398749693 ) ) ;
#36644 = CARTESIAN_POINT ( 'NONE',  ( 57.31821422653260356, 14.58415143128349811, -26.26832944716249685 ) ) ;
#36645 = EDGE_CURVE ( 'NONE', #37059, #9540, #2263, .T. ) ;
#36646 = CARTESIAN_POINT ( 'NONE',  ( 53.61470614374690058, 18.14682731116949554, -49.19246808621250722 ) ) ;
#36647 = CARTESIAN_POINT ( 'NONE',  ( 47.47987687170398630, 23.37779866404240536, -54.97289240249585163 ) ) ;
#36648 = CARTESIAN_POINT ( 'NONE',  ( 50.48048509850679721, -50.09185786847800159, -76.14999999999999147 ) ) ;
#36649 = ADVANCED_FACE ( 'NONE', ( #50482, #14058 ), #30017, .T. ) ;
#36650 = CARTESIAN_POINT ( 'NONE',  ( 16.13393739769620083, -15.61618894467929941, -20.15000000000000213 ) ) ;
#36651 = ORIENTED_EDGE ( 'NONE', *, *, #15208, .F. ) ;
#36652 = ADVANCED_FACE ( 'NONE', ( #10389 ), #38167, .T. ) ;
#36653 = DIRECTION ( 'NONE',  ( 0.000000000000000000, 0.000000000000000000, 1.000000000000000000 ) ) ;
#36654 = ORIENTED_EDGE ( 'NONE', *, *, #10284, .T. ) ;
#36655 = CARTESIAN_POINT ( 'NONE',  ( 56.87160283908409752, -50.28903218254829710, -52.71743054463500044 ) ) ;
#36656 = AXIS2_PLACEMENT_3D ( 'NONE', #757, #13606, #49514 ) ;
#36657 = DIRECTION ( 'NONE',  ( -1.000000000000000000, 0.000000000000000000, 0.000000000000000000 ) ) ;
#36658 = EDGE_CURVE ( 'NONE', #28507, #47320, #43133, .T. ) ;
#36659 = CARTESIAN_POINT ( 'NONE',  ( 8.368826086083149818, -12.84386746725390083, -74.90148551491050455 ) ) ;
#36660 = CARTESIAN_POINT ( 'NONE',  ( 13.89744741416839879, -51.22086835498220125, -22.99801680307020035 ) ) ;
#36661 = CARTESIAN_POINT ( 'NONE',  ( 56.23294450515269460, 19.54859116196450231, -74.77228800217299920 ) ) ;
#36662 = PRODUCT_CONTEXT ( 'NONE', #38860, 'mechanical' ) ;
#36663 = CARTESIAN_POINT ( 'NONE',  ( 46.87509678320709838, -53.74177327554130557, -75.90467361879859709 ) ) ;
#36664 = ORIENTED_EDGE ( 'NONE', *, *, #26021, .F. ) ;
#36665 = CARTESIAN_POINT ( 'NONE',  ( 17.90519802043555586, -22.20705845982418936, -36.86948528380446533 ) ) ;
#36666 = CARTESIAN_POINT ( 'NONE',  ( 20.54387153675149946, -9.611259744901818891, -63.93428524705119287 ) ) ;
#36667 = CARTESIAN_POINT ( 'NONE',  ( 52.88366625939990229, -49.67299857165690469, -49.00384039304309880 ) ) ;
#36668 = CARTESIAN_POINT ( 'NONE',  ( 15.67962062511290000, 19.63028992866140143, -15.65622423491010196 ) ) ;
#36669 = CARTESIAN_POINT ( 'NONE',  ( 11.83166319397156308, 33.82478071477750348, -23.81848075244050378 ) ) ;
#36670 = CARTESIAN_POINT ( 'NONE',  ( 46.48959969234209666, 21.91510670762199808, -76.13710305591399674 ) ) ;
#36671 = CARTESIAN_POINT ( 'NONE',  ( 71.17189893730710537, 1.387131204727290124, -61.00757424182599920 ) ) ;
#36672 = EDGE_CURVE ( 'NONE', #18872, #8034, #49081, .T. ) ;
#36673 = CARTESIAN_POINT ( 'NONE',  ( 59.94414702407019746, 14.70111394113749981, -47.28272102067069937 ) ) ;
#36674 = CARTESIAN_POINT ( 'NONE',  ( 12.36320305067610015, 33.31445045643330616, -15.76422791930239953 ) ) ;
#36675 = B_SPLINE_CURVE_WITH_KNOTS ( 'NONE', 3,
 ( #7529, #11722, #47119, #27686, #19828, #39752, #23736, #15647, #19052, #35561, #43686, #7786 ),
 .UNSPECIFIED., .F., .F.,
 ( 4, 2, 2, 2, 2, 4 ),
 ( 5.801249110064609653E-07, 0.01391382196184159925, 0.02795653394361129543, 0.04029818000215710377, 0.05270323408096880269, 0.05591482578471518999 ),
 .UNSPECIFIED. ) ;
#36676 = DIRECTION ( 'NONE',  ( -1.000000000000000000, 0.000000000000000000, 0.000000000000000000 ) ) ;
#36677 = CARTESIAN_POINT ( 'NONE',  ( 0.4047412638266219553, -8.844334399411719616, -35.14999999999999858 ) ) ;
#36679 = CARTESIAN_POINT ( 'NONE',  ( 30.03924614610626520, -35.61560227024466485, -84.60794077557196147 ) ) ;
#36678 = DIRECTION ( 'NONE',  ( 0.000000000000000000, 0.000000000000000000, 1.000000000000000000 ) ) ;
#36680 = CARTESIAN_POINT ( 'NONE',  ( 63.13746035244330557, 0.8910129994591549085, -68.97194292341539779 ) ) ;
#36681 = CARTESIAN_POINT ( 'NONE',  ( 61.42395427194719559, 13.96908307647129988, -46.82082490102270356 ) ) ;
#36682 = CARTESIAN_POINT ( 'NONE',  ( 20.99564080419046164, -9.290043960182757132, -79.21600316462195224 ) ) ;
#36683 = CARTESIAN_POINT ( 'NONE',  ( -0.4230338164578509863, -63.17480145319609619, -49.86202923830769862 ) ) ;
#36684 = ORIENTED_EDGE ( 'NONE', *, *, #15359, .F. ) ;
#36685 = CARTESIAN_POINT ( 'NONE',  ( 52.75740204447090065, -49.70242901905119481, -48.47378032971909789 ) ) ;
#36686 = VECTOR ( 'NONE', #11678, 1000.000000000000000 ) ;
#36687 = ADVANCED_FACE ( 'NONE', ( #44155 ), #35260, .T. ) ;
#36688 = CARTESIAN_POINT ( 'NONE',  ( 61.70176194880070142, -45.11618250747869752, -27.87045028019250026 ) ) ;
#36689 = CARTESIAN_POINT ( 'NONE',  ( 48.20452265730930463, -54.29503287064159167, -55.30665343754630214 ) ) ;
#36690 = CARTESIAN_POINT ( 'NONE',  ( 56.37055690849290102, 14.89250931428609803, -26.19214289511259608 ) ) ;
#36691 = CARTESIAN_POINT ( 'NONE',  ( 23.16503989757309867, -15.06287498962899996, -36.42782227743549583 ) ) ;
#36693 = CARTESIAN_POINT ( 'NONE',  ( 51.58108482517790350, 19.09072979187009977, -76.34882618429139711 ) ) ;
#36692 = CIRCLE ( 'NONE', #23407, 2.000000000000000000 ) ;
#36694 = CARTESIAN_POINT ( 'NONE',  ( 53.06129597024689559, 18.31052047746409883, -48.87622692185889406 ) ) ;
#36695 = CARTESIAN_POINT ( 'NONE',  ( 71.23719564129540061, 1.194703186106690129, -70.66446396659920026 ) ) ;
#36696 = DIRECTION ( 'NONE',  ( 0.6888026391158391659, 0.7071067811865435759, 0.1598465650148942763 ) ) ;
#36697 = CARTESIAN_POINT ( 'NONE',  ( 69.03514090041920781, -44.31906284533980767, -11.86759013202009960 ) ) ;
#36698 = ORIENTED_EDGE ( 'NONE', *, *, #20278, .F. ) ;
#36699 = CARTESIAN_POINT ( 'NONE',  ( 63.43393739769620510, 1.883811055320669947, -68.84999999999999432 ) ) ;
#36700 = CARTESIAN_POINT ( 'NONE',  ( 23.12959127530770331, -18.17890647944599891, -61.17911655036449758 ) ) ;
#36701 = CARTESIAN_POINT ( 'NONE',  ( 73.08617409304301304, 0.9989215084294049696, -69.02509836011120115 ) ) ;
#36702 = CARTESIAN_POINT ( 'NONE',  ( 47.54355032392420100, -54.57327899847110331, -54.86427360055650126 ) ) ;
#36703 = DIRECTION ( 'NONE',  ( -0.1686178020941830058, -0.6660492713794510244, 0.7265992051412039077 ) ) ;
#36704 = CARTESIAN_POINT ( 'NONE',  ( 73.08275130671789555, 1.274277262446069869, -62.58867475943009850 ) ) ;
#36705 = CARTESIAN_POINT ( 'NONE',  ( 59.12201268170110069, 16.79103452985640033, -50.30506373816950116 ) ) ;
#36706 = CARTESIAN_POINT ( 'NONE',  ( 71.33702656696020483, 1.265664290790580182, -60.77244468760530083 ) ) ;
#36707 = DIRECTION ( 'NONE',  ( 0.000000000000000000, 0.000000000000000000, -1.000000000000000000 ) ) ;
#36708 = CARTESIAN_POINT ( 'NONE',  ( 72.23076864380078632, 1.112168069084249922, -61.27267649081910150 ) ) ;
#36709 = CARTESIAN_POINT ( 'NONE',  ( 71.33393739769628894, 11.38381105532070059, -61.94999999999999574 ) ) ;
#36710 = CARTESIAN_POINT ( 'NONE',  ( 65.00498282733049393, 1.269319268680890067, -70.56549354633131088 ) ) ;
#36711 = ORIENTED_EDGE ( 'NONE', *, *, #554, .T. ) ;
#36712 = ORIENTED_EDGE ( 'NONE', *, *, #34069, .T. ) ;
#36713 = CARTESIAN_POINT ( 'NONE',  ( 71.33393739769809372, 11.38381103969570063, -61.94987500004359759 ) ) ;
#36714 = CARTESIAN_POINT ( 'NONE',  ( 59.34499803081109803, -3.116188944679349593, -15.68015151901639825 ) ) ;
#36715 = B_SPLINE_CURVE_WITH_KNOTS ( 'NONE', 3,
 ( #2789, #3046, #19018, #34994, #8000, #43907, #11434, #27140, #48096, #39976 ),
 .UNSPECIFIED., .F., .F.,
 ( 4, 2, 2, 2, 4 ),
 ( -0.0004281134593881059914, 0.000000000000000000, 0.02012916873249290597, 0.03942875605179270437, 0.05028014561811239291 ),
 .UNSPECIFIED. ) ;
#36716 = EDGE_LOOP ( 'NONE', ( #49884, #8758, #51117 ) ) ;
#36717 = CARTESIAN_POINT ( 'NONE',  ( 9.367097141674031846, -15.61601956221279863, -71.84717978381000592 ) ) ;
#36718 = CARTESIAN_POINT ( 'NONE',  ( 84.32823744777105901, 12.72937168411247555, -47.43651528304791043 ) ) ;
#36719 = CARTESIAN_POINT ( 'NONE',  ( 9.922022971808480918, -12.84297312065496754, -49.58660389420793280 ) ) ;
#36720 = CARTESIAN_POINT ( 'NONE',  ( 52.02214979817979668, 19.08406620782900021, -76.54113483184499955 ) ) ;
#36721 = EDGE_LOOP ( 'NONE', ( #312, #3176, #19871, #433, #13354 ) ) ;
#36722 = CARTESIAN_POINT ( 'NONE',  ( 64.93393739763529027, 1.883811055311890081, -62.44999999997569518 ) ) ;
#36723 = CARTESIAN_POINT ( 'NONE',  ( 42.40479495363826601, 6.455874691308983948, -78.29570199813332465 ) ) ;
#36724 = CARTESIAN_POINT ( 'NONE',  ( 24.04493740857834538, -14.58064761262398790, -35.46599892844898250 ) ) ;
#36725 = EDGE_CURVE ( 'NONE', #44314, #3281, #424, .T. ) ;
#36726 = CARTESIAN_POINT ( 'NONE',  ( 19.35590054169199803, -23.20576558337710082, -44.16454026222609741 ) ) ;
#36727 = CARTESIAN_POINT ( 'NONE',  ( 22.58446406675447449, -13.52685100215215641, -56.35316686890462989 ) ) ;
#36728 = CARTESIAN_POINT ( 'NONE',  ( 43.30851615596512971, -37.82231177387381393, -73.77704280282122795 ) ) ;
#36729 = VERTEX_POINT ( 'NONE', #16112 ) ;
#36730 = CARTESIAN_POINT ( 'NONE',  ( 11.97296053931879989, -65.41364856023331242, -22.92423455041799940 ) ) ;
#36731 = CARTESIAN_POINT ( 'NONE',  ( 20.66546011552009787, -21.52990145569759761, -36.52453509903889994 ) ) ;
#36732 = CIRCLE ( 'NONE', #42626, 3.000000000000005773 ) ;
#36733 = DIRECTION ( 'NONE',  ( 0.000000000000000000, 0.000000000000000000, 1.000000000000000000 ) ) ;
#36734 = CARTESIAN_POINT ( 'NONE',  ( 14.49280304823600041, 21.09308431968760189, -75.96462645239850531 ) ) ;
#36735 = EDGE_CURVE ( 'NONE', #25918, #47312, #14686, .T. ) ;
#36736 = CARTESIAN_POINT ( 'NONE',  ( 14.72050101380589915, -23.46848077975802127, -60.34919524473630048 ) ) ;
#36737 = CARTESIAN_POINT ( 'NONE',  ( 16.13393739769620083, -15.61618894467929941, -8.849999999999999645 ) ) ;
#36738 = CARTESIAN_POINT ( 'NONE',  ( 10.85466640524320070, 33.73459223951330443, -17.55961383757199812 ) ) ;
#36739 = CARTESIAN_POINT ( 'NONE',  ( 10.11025315938129943, -9.986095792159350282, -52.74692207654089060 ) ) ;
#36740 = ORIENTED_EDGE ( 'NONE', *, *, #37815, .T. ) ;
#36741 = CARTESIAN_POINT ( 'NONE',  ( 53.73571933783139798, -48.69420006231280240, -26.82704014588000163 ) ) ;
#36742 = CARTESIAN_POINT ( 'NONE',  ( 16.62868081655000196, -51.11618894343789776, -20.46561682067509835 ) ) ;
#36743 = CARTESIAN_POINT ( 'NONE',  ( 50.80150374823916337, -35.57053178561582030, -76.30434720868854015 ) ) ;
#36744 = CARTESIAN_POINT ( 'NONE',  ( 46.58046218066166233, 12.29309675584422479, -5.686836593841567478 ) ) ;
#36745 = CARTESIAN_POINT ( 'NONE',  ( 75.47966807050509885, 12.14072485751589880, -13.40512917118210012 ) ) ;
#36746 = DIRECTION ( 'NONE',  ( 0.000000000000000000, 0.000000000000000000, -1.000000000000000000 ) ) ;
#36747 = ORIENTED_EDGE ( 'NONE', *, *, #25145, .T. ) ;
#36748 = CARTESIAN_POINT ( 'NONE',  ( -9.505843262714801511, -43.70152617308460208, -5.901968664759829508 ) ) ;
#36749 = CARTESIAN_POINT ( 'NONE',  ( 47.24062726108790145, 23.53053415419130090, -54.65361905327920056 ) ) ;
#36750 = EDGE_CURVE ( 'NONE', #46034, #12879, #42304, .T. ) ;
#36751 = FACE_OUTER_BOUND ( 'NONE', #15852, .T. ) ;
#36752 = CARTESIAN_POINT ( 'NONE',  ( 63.11000452699359897, 0.9945465939392541532, -62.38364600848370145 ) ) ;
#36753 = CARTESIAN_POINT ( 'NONE',  ( 57.25380931998220291, -50.61618894467930119, -53.86267003311080259 ) ) ;
#36754 = CARTESIAN_POINT ( 'NONE',  ( 43.75992007200080280, 12.39321587781959977, -5.076600545294299494 ) ) ;
#36755 = DIRECTION ( 'NONE',  ( 1.000000000000000000, 0.000000000000000000, 0.000000000000000000 ) ) ;
#36756 = CARTESIAN_POINT ( 'NONE',  ( 15.24822960659503046, -22.38319987333287031, -64.99448789959322426 ) ) ;
#36757 = CARTESIAN_POINT ( 'NONE',  ( 72.68796522584510456, 1.404650034022369987, -62.35426166056780062 ) ) ;
#36758 = CARTESIAN_POINT ( 'NONE',  ( 60.34379256561119576, -45.86802437250690190, -47.72732608210879590 ) ) ;
#36759 = CARTESIAN_POINT ( 'NONE',  ( 17.19412305922981332, -22.35806894703990366, -66.90336922568695854 ) ) ;
#36760 = ADVANCED_FACE ( 'NONE', ( #19533 ), #51764, .T. ) ;
#36761 = CARTESIAN_POINT ( 'NONE',  ( 64.80090148641959047, 1.186614556332910020, -60.76691531849380112 ) ) ;
#36762 = CARTESIAN_POINT ( 'NONE',  ( 17.63565729903150014, -52.02998614742870132, -75.83262351151699932 ) ) ;
#36763 = EDGE_CURVE ( 'NONE', #15443, #17150, #26362, .T. ) ;
#36764 = CARTESIAN_POINT ( 'NONE',  ( 8.222963321015376081, -14.58045169080828707, -72.54933512887784275 ) ) ;
#36765 = CARTESIAN_POINT ( 'NONE',  ( 49.01168265654600020, 13.88381105532070059, -9.596379464580280683 ) ) ;
#36766 = ORIENTED_EDGE ( 'NONE', *, *, #35057, .F. ) ;
#36767 = CARTESIAN_POINT ( 'NONE',  ( -0.2149313111747337413, -10.70936568845926828, -34.95336413010216603 ) ) ;
#36768 = CARTESIAN_POINT ( 'NONE',  ( 10.14085492948789913, 31.97598296081329750, -45.99401054949460388 ) ) ;
#36769 = CARTESIAN_POINT ( 'NONE',  ( 58.92073396209919878, -3.116188944679349593, -15.65000000000000036 ) ) ;
#36770 = AXIS2_PLACEMENT_3D ( 'NONE', #4011, #7943, #2985 ) ;
#36771 = VECTOR ( 'NONE', #4282, 1000.000000000000000 ) ;
#36772 = VECTOR ( 'NONE', #27352, 1000.000000000000000 ) ;
#36773 = CARTESIAN_POINT ( 'NONE',  ( 66.87128124109968041, -31.56637477442769679, -17.65462924257609956 ) ) ;
#36774 = VERTEX_POINT ( 'NONE', #51259 ) ;
#36775 = CARTESIAN_POINT ( 'NONE',  ( 17.85968403959190098, 20.22256044820920096, -75.26885115310530239 ) ) ;
#36776 = ORIENTED_EDGE ( 'NONE', *, *, #42948, .F. ) ;
#36777 = ORIENTED_EDGE ( 'NONE', *, *, #24738, .T. ) ;
#36778 = VECTOR ( 'NONE', #21234, 1000.000000000000000 ) ;
#36779 = ORIENTED_EDGE ( 'NONE', *, *, #3182, .T. ) ;
#36780 = CARTESIAN_POINT ( 'NONE',  ( 12.62246544811769944, -65.46760815329750471, -47.29889843674509819 ) ) ;
#36781 = PLANE ( 'NONE',  #19344 ) ;
#36782 = CARTESIAN_POINT ( 'NONE',  ( 22.58000039849400054, -18.80532364725490169, -81.23899999999999011 ) ) ;
#36783 = CARTESIAN_POINT ( 'NONE',  ( 2.633937397696199945, -15.61618894467929763, -6.189999999999999503 ) ) ;
#36784 = EDGE_CURVE ( 'NONE', #22924, #27937, #35521, .T. ) ;
#36785 = CARTESIAN_POINT ( 'NONE',  ( 61.67706982099739577, 13.89683601203829966, -46.59487708233500314 ) ) ;
#36786 = ORIENTED_EDGE ( 'NONE', *, *, #47664, .F. ) ;
#36787 = DIRECTION ( 'NONE',  ( 0.000000000000000000, 0.000000000000000000, 1.000000000000000000 ) ) ;
#36788 = EDGE_CURVE ( 'NONE', #37013, #9540, #24720, .T. ) ;
#36789 = CARTESIAN_POINT ( 'NONE',  ( -9.882013117715120032, 9.266944274022621997, -21.14999999999999858 ) ) ;
#36790 = EDGE_LOOP ( 'NONE', ( #22406, #37829, #6839, #8799 ) ) ;
#36791 = CARTESIAN_POINT ( 'NONE',  ( 20.84741856749390365, -10.36969921949989981, -42.58016164095369760 ) ) ;
#36792 = FACE_OUTER_BOUND ( 'NONE', #33664, .T. ) ;
#36793 = CARTESIAN_POINT ( 'NONE',  ( 10.26917183476574991, -55.18446999559061084, -45.87608767524120168 ) ) ;
#36794 = ORIENTED_EDGE ( 'NONE', *, *, #29640, .T. ) ;
#36795 = ORIENTED_EDGE ( 'NONE', *, *, #13127, .F. ) ;
#36796 = DIRECTION ( 'NONE',  ( 0.000000000000000000, 0.000000000000000000, 1.000000000000000000 ) ) ;
#36797 = CARTESIAN_POINT ( 'NONE',  ( 33.53393739662440254, -15.61618894541809688, -10.45000000053580180 ) ) ;
#36798 = CARTESIAN_POINT ( 'NONE',  ( 66.45612384051480603, 13.88381326200750010, -12.57322850638879963 ) ) ;
#36799 = CARTESIAN_POINT ( 'NONE',  ( 50.81599192650290320, 13.97286014258159881, -11.75472651265789992 ) ) ;
#36800 = CARTESIAN_POINT ( 'NONE',  ( 9.221442925756241138, -19.60036937649121214, -68.62566444102958485 ) ) ;
#36801 = CARTESIAN_POINT ( 'NONE',  ( -3.204518368035979670, 17.10185219687699743, -4.296538305020969339 ) ) ;
#36802 = VECTOR ( 'NONE', #42367, 1000.000000000000000 ) ;
#36803 = CIRCLE ( 'NONE', #20899, 5.500000000000000000 ) ;
#36804 = AXIS2_PLACEMENT_3D ( 'NONE', #12479, #44450, #28447 ) ;
#36805 = FACE_OUTER_BOUND ( 'NONE', #21602, .T. ) ;
#36806 = CARTESIAN_POINT ( 'NONE',  ( 55.45321058330383579, 14.78278210347054689, -16.61881412770280875 ) ) ;
#36807 = CIRCLE ( 'NONE', #34290, 21.96784688337769964 ) ;
#36808 = CARTESIAN_POINT ( 'NONE',  ( 22.87033105319540027, -19.64207377926320319, -63.45897166066949069 ) ) ;
#36809 = ORIENTED_EDGE ( 'NONE', *, *, #45668, .T. ) ;
#36810 = CARTESIAN_POINT ( 'NONE',  ( 58.55123287010390243, 15.52708936521539940, -47.93263078914269926 ) ) ;
#36812 = AXIS2_PLACEMENT_3D ( 'NONE', #40909, #28846, #44849 ) ;
#36811 = CARTESIAN_POINT ( 'NONE',  ( 16.13393739769620083, -15.61618894467929941, -7.393828452885189861 ) ) ;
#36813 = CARTESIAN_POINT ( 'NONE',  ( 53.62552786343490396, -51.33071804962359153, -75.58099297212140755 ) ) ;
#36814 = PRODUCT_DEFINITION_CONTEXT ( 'detailed design', #10382, 'design' ) ;
#36815 = CARTESIAN_POINT ( 'NONE',  ( 72.31224245611890922, 1.117804454683279936, -69.95018517907431033 ) ) ;
#36816 = CARTESIAN_POINT ( 'NONE',  ( 71.45588032111159293, 0.8910129994591539093, -60.65352295474710331 ) ) ;
#36817 = CARTESIAN_POINT ( 'NONE',  ( 42.22674147479784068, -39.78872467147441938, -75.23666230762985663 ) ) ;
#36818 =( BOUNDED_CURVE ( )  B_SPLINE_CURVE ( 2, ( #39993, #20307, #51278 ),
 .UNSPECIFIED., .F., .T. ) 
 B_SPLINE_CURVE_WITH_KNOTS ( ( 3, 3 ),
 ( 2.168627590050209886, 3.232274745523169734 ),
 .UNSPECIFIED. ) 
 CURVE ( )  GEOMETRIC_REPRESENTATION_ITEM ( )  RATIONAL_B_SPLINE_CURVE ( ( 1.425426480542939967, 1.425426480542939967, 1.323085463760209857 ) ) 
 REPRESENTATION_ITEM ( '' )  );
#36819 = CARTESIAN_POINT ( 'NONE',  ( 16.65420337941059969, -49.11618894467930829, -17.90311212357429937 ) ) ;
#36820 = CARTESIAN_POINT ( 'NONE',  ( 72.40605974471309025, 1.033004162168289941, -69.86315739208511388 ) ) ;
#36821 = CARTESIAN_POINT ( 'NONE',  ( 47.20319461169519570, 23.55908263626179888, -74.17383159930358261 ) ) ;
#36822 = CARTESIAN_POINT ( 'NONE',  ( 48.90836479786370461, -53.96901701391990258, -54.96636899373179830 ) ) ;
#36823 = CYLINDRICAL_SURFACE ( 'NONE', #28946, 7.910999999999997812 ) ;
#36824 = EDGE_CURVE ( 'NONE', #425, #15778, #11942, .T. ) ;
#36825 = CARTESIAN_POINT ( 'NONE',  ( 76.70719566378195964, -43.18885252246143125, -14.39567811762877447 ) ) ;
#36826 = LINE ( 'NONE', #929, #15423 ) ;
#36827 = CARTESIAN_POINT ( 'NONE',  ( 22.90012247355228325, -16.27786605360535077, -70.87830227662946925 ) ) ;
#36828 = EDGE_CURVE ( 'NONE', #8412, #13106, #24710, .T. ) ;
#36829 = ORIENTED_EDGE ( 'NONE', *, *, #13315, .F. ) ;
#36830 = CARTESIAN_POINT ( 'NONE',  ( 23.49301428767259736, -16.77837725375670175, -43.11720026785929605 ) ) ;
#36831 = CARTESIAN_POINT ( 'NONE',  ( 64.00784214253330617, 1.443555314919450216, -61.59234650647290010 ) ) ;
#36832 = ORIENTED_EDGE ( 'NONE', *, *, #44437, .T. ) ;
#36833 = DIRECTION ( 'NONE',  ( 0.000000000000000000, 0.000000000000000000, -1.000000000000000000 ) ) ;
#36834 = CARTESIAN_POINT ( 'NONE',  ( 60.85189549106659967, -45.66403237420649930, -47.67927086682649929 ) ) ;
#36835 = CARTESIAN_POINT ( 'NONE',  ( 12.89372882336123638, -8.399748356796177262, -81.15800232914327239 ) ) ;
#36837 = CARTESIAN_POINT ( 'NONE',  ( 12.14976757460917867, -22.52869039637574033, -78.45899712908982337 ) ) ;
#36836 = CARTESIAN_POINT ( 'NONE',  ( 40.88902997202897183, 8.404135775541593745, -81.68995767638860173 ) ) ;
#36838 = CARTESIAN_POINT ( 'NONE',  ( 51.42797784481540191, -51.20406220416529663, -76.10787249881708760 ) ) ;
#36839 = LINE ( 'NONE', #28971, #10224 ) ;
#36840 = VERTEX_POINT ( 'NONE', #49144 ) ;
#36841 = CARTESIAN_POINT ( 'NONE',  ( 84.01174786492798319, -44.61701663110100213, -47.41946551740999638 ) ) ;
#36842 = VERTEX_POINT ( 'NONE', #1169 ) ;
#36843 = ORIENTED_EDGE ( 'NONE', *, *, #35386, .F. ) ;
#36844 = ORIENTED_EDGE ( 'NONE', *, *, #41852, .T. ) ;
#36845 = CARTESIAN_POINT ( 'NONE',  ( 61.71627407764110274, -45.13006394953620770, -46.64368077600400397 ) ) ;
#36846 = AXIS2_PLACEMENT_3D ( 'NONE', #51506, #11676, #899 ) ;
#36847 = CARTESIAN_POINT ( 'NONE',  ( 17.16951619896303782, -7.705193419797750742, -79.33399943592132786 ) ) ;
#36848 = AXIS2_PLACEMENT_3D ( 'NONE', #40035, #36340, #40802 ) ;
#36849 = CARTESIAN_POINT ( 'NONE',  ( 76.48708243442970911, -3.703201758521061482, -13.17175452297058236 ) ) ;
#36850 = DIRECTION ( 'NONE',  ( -0.8660254037844380415, 0.5000000000000012212, -1.387778780781449373E-16 ) ) ;
#36851 = VECTOR ( 'NONE', #17078, 1000.000000000000000 ) ;
#36852 = ORIENTED_EDGE ( 'NONE', *, *, #22435, .F. ) ;
#36853 = ORIENTED_EDGE ( 'NONE', *, *, #5964, .T. ) ;
#36854 = TOROIDAL_SURFACE ( 'NONE', #32637, 25.00000000000000000, 3.569999999999939888 ) ;
#36855 = AXIS2_PLACEMENT_3D ( 'NONE', #12433, #13231, #631 ) ;
#36856 = ADVANCED_FACE ( 'NONE', ( #8776 ), #35206, .T. ) ;
#36857 = CARTESIAN_POINT ( 'NONE',  ( 17.16939711463305684, -23.52720157518136546, -55.96593682117922697 ) ) ;
#36858 = CARTESIAN_POINT ( 'NONE',  ( 56.57438608727660068, 19.50039335391339890, -53.83822343184270665 ) ) ;
#36859 = CARTESIAN_POINT ( 'NONE',  ( -15.44067079850665181, 7.275931003700006450, -48.50294866079644862 ) ) ;
#36860 = CARTESIAN_POINT ( 'NONE',  ( 16.13393739769620083, -15.61618894467929941, -8.655000000000001137 ) ) ;
#36861 = DIRECTION ( 'NONE',  ( -7.539420000000001133E-18, 1.452687000000000165E-17, 1.000000000000000000 ) ) ;
#36862 = EDGE_CURVE ( 'NONE', #34982, #41459, #44793, .T. ) ;
#36863 = DIRECTION ( 'NONE',  ( -1.000000000000000000, 0.000000000000000000, 0.000000000000000000 ) ) ;
#36864 = CARTESIAN_POINT ( 'NONE',  ( 9.367491665984019278, -15.61623476897930018, -53.45282021618999124 ) ) ;
#36865 = ORIENTED_EDGE ( 'NONE', *, *, #6384, .T. ) ;
#36866 = FACE_OUTER_BOUND ( 'NONE', #19979, .T. ) ;
#36867 = CARTESIAN_POINT ( 'NONE',  ( 8.773163715961540987, -48.44626589138000128, -41.74835364836469864 ) ) ;
#36868 = CARTESIAN_POINT ( 'NONE',  ( 21.93099174023785025, -19.12845236462728238, -46.62617237298687911 ) ) ;
#36869 = CARTESIAN_POINT ( 'NONE',  ( 83.69028012337390976, -45.07031254642157592, -47.49659995980665173 ) ) ;
#36870 = CARTESIAN_POINT ( 'NONE',  ( 16.28635962228009859, -23.46243104246319788, -64.50631165503649811 ) ) ;
#36871 = CARTESIAN_POINT ( 'NONE',  ( 83.89200044194980421, -50.09049722508079583, -52.57651812407429759 ) ) ;
#36872 = CARTESIAN_POINT ( 'NONE',  ( 41.75077191591359593, -44.42764855811009994, -5.046633188611889587 ) ) ;
#36873 = DIRECTION ( 'NONE',  ( 0.8263629291053539161, 0.3519990991163989835, -0.4395690430656639669 ) ) ;
#36874 = VECTOR ( 'NONE', #41912, 1000.000000000000000 ) ;
#36875 = CYLINDRICAL_SURFACE ( 'NONE', #45461, 7.910999999999997812 ) ;
#36876 = CARTESIAN_POINT ( 'NONE',  ( 61.34439110493909908, -45.35647919298600073, -47.30212553788380347 ) ) ;
#36877 = CARTESIAN_POINT ( 'NONE',  ( 64.02817266311009803, 1.026090475080779996, -70.02573918086800120 ) ) ;
#36878 = DIRECTION ( 'NONE',  ( -1.000000000000000000, 0.000000000000000000, 0.000000000000000000 ) ) ;
#36879 = CARTESIAN_POINT ( 'NONE',  ( 65.81145605635769869, 1.573399105534700082, -18.80820005952190144 ) ) ;
#36880 = VERTEX_POINT ( 'NONE', #27265 ) ;
#36881 = CARTESIAN_POINT ( 'NONE',  ( 13.99023357302460013, -52.20804236601910020, -75.66803551354809088 ) ) ;
#36882 = CARTESIAN_POINT ( 'NONE',  ( 47.37397992040639849, -54.67284273012320739, -54.79488902382239957 ) ) ;
#36883 = CARTESIAN_POINT ( 'NONE',  ( 11.86093866209844983, 34.13069104536225495, -47.45833196164814183 ) ) ;
#36884 = CARTESIAN_POINT ( 'NONE',  ( 30.63393739769619728, -15.61618894467929941, -20.58999999999999986 ) ) ;
#36885 = AXIS2_PLACEMENT_3D ( 'NONE', #22317, #35151, #43040 ) ;
#36886 = CARTESIAN_POINT ( 'NONE',  ( 16.26610795940585774, -7.638794151532966481, -55.01276702998251977 ) ) ;
#36887 = AXIS2_PLACEMENT_3D ( 'NONE', #26861, #10375, #34718 ) ;
#36888 = CARTESIAN_POINT ( 'NONE',  ( 23.27131239030429910, -14.57976881098799815, -32.14999999999999858 ) ) ;
#36889 = DIRECTION ( 'NONE',  ( 0.000000000000000000, -1.000000000000000000, 0.000000000000000000 ) ) ;
#36890 = CARTESIAN_POINT ( 'NONE',  ( 68.13393739769620083, 1.383811055320669947, -65.65000000000000568 ) ) ;
#36892 = CARTESIAN_POINT ( 'NONE',  ( 24.04493738366187827, -16.65172975277582168, -73.54933447873786179 ) ) ;
#36891 = CARTESIAN_POINT ( 'NONE',  ( 16.13393739769620083, -15.61618894467929941, -1.149999999999999911 ) ) ;
#36893 = EDGE_CURVE ( 'NONE', #24734, #50083, #34099, .T. ) ;
#36894 = CARTESIAN_POINT ( 'NONE',  ( 23.36719009658099822, -48.14181044607700244, -48.24693240285689910 ) ) ;
#36895 = CARTESIAN_POINT ( 'NONE',  ( 48.40781919080369988, 22.97605840957759682, -55.28683361800550244 ) ) ;
#36896 = ORIENTED_EDGE ( 'NONE', *, *, #14510, .F. ) ;
#36897 = CARTESIAN_POINT ( 'NONE',  ( 22.65185334536269934, -12.92187439852739850, -68.72240889194819147 ) ) ;
#36898 = VERTEX_POINT ( 'NONE', #49908 ) ;
#36899 = DIRECTION ( 'NONE',  ( -0.8545454545454580497, -2.306495000000000021E-16, 0.5193766129849289870 ) ) ;
#36900 = CARTESIAN_POINT ( 'NONE',  ( 53.59008489733366787, -49.40624463047604564, -49.22507928152084844 ) ) ;
#36901 = CARTESIAN_POINT ( 'NONE',  ( 13.73527022026379996, 18.97497658877130178, -20.93080062776429884 ) ) ;
#36903 = CARTESIAN_POINT ( 'NONE',  ( 54.15723598241670089, 16.86721667791090340, -26.23832647098850046 ) ) ;
#36902 = CARTESIAN_POINT ( 'NONE',  ( 84.42050518244910506, 12.05117995606869918, -47.35805390042769858 ) ) ;
#36904 = CARTESIAN_POINT ( 'NONE',  ( 10.29205353740080042, -19.56776478976249933, -65.26351318459290951 ) ) ;
#36905 = FACE_OUTER_BOUND ( 'NONE', #20992, .T. ) ;
#36906 = CARTESIAN_POINT ( 'NONE',  ( 57.04515152503049791, -45.11618894467940066, -16.25132461468449918 ) ) ;
#36907 = CARTESIAN_POINT ( 'NONE',  ( 64.93393739769619799, 10.88381105532070059, -69.34999999999999432 ) ) ;
#36908 = ORIENTED_EDGE ( 'NONE', *, *, #7339, .T. ) ;
#36909 = ORIENTED_EDGE ( 'NONE', *, *, #32159, .T. ) ;
#36910 = CARTESIAN_POINT ( 'NONE',  ( 11.86340152621610144, -64.99742207597500965, -16.42027960340800163 ) ) ;
#36911 = CARTESIAN_POINT ( 'NONE',  ( 12.53186402970929869, 34.21131896774730308, -47.19092881324929323 ) ) ;
#36912 = LINE ( 'NONE', #28001, #46644 ) ;
#36913 = CARTESIAN_POINT ( 'NONE',  ( 51.77723966175119585, -50.84882725107309653, -50.47693161301669562 ) ) ;
#36914 = CARTESIAN_POINT ( 'NONE',  ( 19.53299984191638927, 24.23912880602019726, -75.56421462368636810 ) ) ;
#36915 = EDGE_LOOP ( 'NONE', ( #30307, #26073, #20074, #47318 ) ) ;
#36916 = EDGE_CURVE ( 'NONE', #28125, #51191, #6142, .T. ) ;
#36917 = DIRECTION ( 'NONE',  ( 0.000000000000000000, 0.000000000000000000, -1.000000000000000000 ) ) ;
#36918 = CARTESIAN_POINT ( 'NONE',  ( 51.13393739769620083, 19.38381105532069881, 11.34999999999999964 ) ) ;
#36919 = DIRECTION ( 'NONE',  ( -1.000000000000000000, 0.000000000000000000, 0.000000000000000000 ) ) ;
#36920 = EDGE_CURVE ( 'NONE', #44651, #51663, #36401, .T. ) ;
#36921 = FACE_OUTER_BOUND ( 'NONE', #37893, .T. ) ;
#36922 = CARTESIAN_POINT ( 'NONE',  ( 50.55764114179640245, -49.80772761642590041, -76.16355215278129265 ) ) ;
#36923 = DIRECTION ( 'NONE',  ( 0.000000000000000000, 0.000000000000000000, -1.000000000000000000 ) ) ;
#36924 = CIRCLE ( 'NONE', #4301, 1.000000000000001554 ) ;
#36925 = ORIENTED_EDGE ( 'NONE', *, *, #9571, .T. ) ;
#36926 = CARTESIAN_POINT ( 'NONE',  ( 10.22109382420207346, -12.20808149134441756, -67.61948648231498282 ) ) ;
#36928 = CARTESIAN_POINT ( 'NONE',  ( 65.03603135424580728, -1.463538230407920082, -19.52361391316370032 ) ) ;
#36927 = AXIS2_PLACEMENT_3D ( 'NONE', #38408, #31040, #47322 ) ;
#36929 = ORIENTED_EDGE ( 'NONE', *, *, #37514, .F. ) ;
#36930 = CARTESIAN_POINT ( 'NONE',  ( 68.13393739769620083, 4.883811055320659733, -73.60861006572370968 ) ) ;
#36931 = CARTESIAN_POINT ( 'NONE',  ( 49.42578290888749848, -46.18034399694119685, -12.04424791257699923 ) ) ;
#36932 = VECTOR ( 'NONE', #561, 1000.000000000000114 ) ;
#36933 = CARTESIAN_POINT ( 'NONE',  ( 8.499441539007790425, -17.43311507835980123, -36.93812364489689770 ) ) ;
#36934 = CARTESIAN_POINT ( 'NONE',  ( 52.90670265584750354, -49.65877502917909680, -49.00842844558349753 ) ) ;
#36935 = CARTESIAN_POINT ( 'NONE',  ( 68.13393739769819035, 19.47158195952109594, -72.59354914830207406 ) ) ;
#36936 = CARTESIAN_POINT ( 'NONE',  ( 54.91244656393700296, 19.73665118953919873, -75.41285438732109014 ) ) ;
#36937 = CARTESIAN_POINT ( 'NONE',  ( 46.49593472332909982, -53.10326984347969415, -76.13971323818920212 ) ) ;
#36938 = VERTEX_POINT ( 'NONE', #39847 ) ;
#36939 = CARTESIAN_POINT ( 'NONE',  ( -0.8602693046289541234, -18.80587780509931051, -35.51452756723926996 ) ) ;
#36940 = CARTESIAN_POINT ( 'NONE',  ( 57.26071802646550424, -50.61617465155239870, -53.75790974367630071 ) ) ;
#36941 = CARTESIAN_POINT ( 'NONE',  ( 9.367206039829609310, -15.61603166621950045, -73.45282021618999124 ) ) ;
#36942 = CARTESIAN_POINT ( 'NONE',  ( 0.1457841021255935343, -22.91266753744946527, -34.68167779225149161 ) ) ;
#36943 = CARTESIAN_POINT ( 'NONE',  ( 47.11902681095249790, 23.00695196644999641, -75.46775895608919882 ) ) ;
#36944 = CARTESIAN_POINT ( 'NONE',  ( 48.94270149030929673, 20.57433438911350265, -55.11972614036160678 ) ) ;
#36945 = PRODUCT_RELATED_PRODUCT_CATEGORY ( 'part', '', ( #21513 ) ) ;
#36946 = CARTESIAN_POINT ( 'NONE',  ( 55.00867404205060041, 17.28694651894000245, -48.28813249775050309 ) ) ;
#36947 = CARTESIAN_POINT ( 'NONE',  ( 12.36320305067610015, 33.31445045643330616, -15.76422791930239953 ) ) ;
#36948 = CARTESIAN_POINT ( 'NONE',  ( 14.68576648362313541, -49.61617023087686817, -83.19397497661746854 ) ) ;
#36949 = CARTESIAN_POINT ( 'NONE',  ( 73.17080802144360518, 1.198183261254770038, -68.71131498411249083 ) ) ;
#36950 = CARTESIAN_POINT ( 'NONE',  ( -18.86606260230390220, 19.38381105532060289, 11.97999999999999865 ) ) ;
#36951 = EDGE_CURVE ( 'NONE', #611, #39828, #30389, .T. ) ;
#36952 = CARTESIAN_POINT ( 'NONE',  ( 63.22191407479270708, 1.186701509386330011, -68.93447492634859941 ) ) ;
#36953 = CARTESIAN_POINT ( 'NONE',  ( 61.21881552187829811, 14.03327925050890101, -46.68011238816460207 ) ) ;
#36954 = CARTESIAN_POINT ( 'NONE',  ( -32.74859963536999885, -25.24211673056830207, -56.32353328738960130 ) ) ;
#36955 = EDGE_CURVE ( 'NONE', #40855, #39471, #16504, .T. ) ;
#36956 = ORIENTED_EDGE ( 'NONE', *, *, #1192, .T. ) ;
#36957 = AXIS2_PLACEMENT_3D ( 'NONE', #5760, #28816, #45341 ) ;
#36958 = CARTESIAN_POINT ( 'NONE',  ( 52.77841038127930773, -49.69307296738830360, -48.67385971155560043 ) ) ;
#36959 = EDGE_CURVE ( 'NONE', #14025, #39703, #27202, .T. ) ;
#36960 = AXIS2_PLACEMENT_3D ( 'NONE', #5106, #20799, #8244 ) ;
#36961 = CARTESIAN_POINT ( 'NONE',  ( 59.25763488836199855, -45.11616244058109970, -25.82585945883460354 ) ) ;
#36962 = CARTESIAN_POINT ( 'NONE',  ( 24.04380548879042223, -15.76082440701389054, -65.79815003220092251 ) ) ;
#36963 = CARTESIAN_POINT ( 'NONE',  ( 57.05654409593750387, 14.11921858418430098, -25.89448720482640098 ) ) ;
#36964 = CONICAL_SURFACE ( 'NONE', #12705, 1.715179901029911802, 0.08257045569470247703 ) ;
#36965 = CARTESIAN_POINT ( 'NONE',  ( 9.294393911660149499, -12.66194776880280060, -81.36245008104749843 ) ) ;
#36966 = CARTESIAN_POINT ( 'NONE',  ( 50.77884152257319528, 18.99564097152240194, -76.16429374177040756 ) ) ;
#36967 = CARTESIAN_POINT ( 'NONE',  ( 53.36583835243820317, 18.19133335057600220, -49.05762109479490363 ) ) ;
#36968 = CARTESIAN_POINT ( 'NONE',  ( 71.20883305211729919, 1.369885150286779929, -70.38694600888931063 ) ) ;
#36969 = CARTESIAN_POINT ( 'NONE',  ( 41.06001671441600109, -44.29932858193080136, -3.719606166043670115 ) ) ;
#36970 = CARTESIAN_POINT ( 'NONE',  ( 47.23343138990082934, 22.78429296043502816, -75.61476957820426037 ) ) ;
#36971 = ORIENTED_EDGE ( 'NONE', *, *, #37604, .F. ) ;
#36972 = CARTESIAN_POINT ( 'NONE',  ( 17.06628174423480004, -8.224475449209380784, -78.60728138436078893 ) ) ;
#36973 = ORIENTED_EDGE ( 'NONE', *, *, #6939, .F. ) ;
#36974 = CARTESIAN_POINT ( 'NONE',  ( 72.91105647262868672, 1.325839985408290067, -68.86912414701170349 ) ) ;
#36975 = CARTESIAN_POINT ( 'NONE',  ( 47.48078737089889501, -54.60317255200649811, -54.76237954934830299 ) ) ;
#36976 = CARTESIAN_POINT ( 'NONE',  ( 11.93174526809839975, -65.43929183185349530, -17.93019253464870033 ) ) ;
#36977 = CARTESIAN_POINT ( 'NONE',  ( 73.09272852564158995, 1.276058558775519991, -62.60937635806730839 ) ) ;
#36978 = DIRECTION ( 'NONE',  ( 0.02902962677397545252, 0.04063306972650054805, 0.9987523388778446476 ) ) ;
#36979 = CARTESIAN_POINT ( 'NONE',  ( 71.60000756020500035, 0.9395704634982890990, -60.75234178971950172 ) ) ;
#36980 = DIRECTION ( 'NONE',  ( 0.000000000000000000, -1.000000000000000000, 0.000000000000000000 ) ) ;
#36981 = CARTESIAN_POINT ( 'NONE',  ( 71.61582913010290952, 1.408710407022130129, -61.13660121446530127 ) ) ;
#36982 = DIRECTION ( 'NONE',  ( 0.000000000000000000, 0.000000000000000000, -1.000000000000000000 ) ) ;
#36983 = CARTESIAN_POINT ( 'NONE',  ( 64.90928650851499526, 1.188042061556800144, -70.59681938162209747 ) ) ;
#36984 = ORIENTED_EDGE ( 'NONE', *, *, #11590, .T. ) ;
#36985 = ORIENTED_EDGE ( 'NONE', *, *, #6820, .T. ) ;
#36986 = CARTESIAN_POINT ( 'NONE',  ( 14.03111719126319912, -51.16607778863529887, -22.86119528526040057 ) ) ;
#36987 = DIRECTION ( 'NONE',  ( -0.6801873868961743064, -8.329893061828022439E-17, -0.7330382791555664079 ) ) ;
#36988 = ORIENTED_EDGE ( 'NONE', *, *, #35768, .T. ) ;
#36989 = EDGE_CURVE ( 'NONE', #6854, #51808, #30076, .T. ) ;
#36990 = DIRECTION ( 'NONE',  ( 0.8090169943749490056, 0.5877852522924709167, 0.000000000000000000 ) ) ;
#36991 = CARTESIAN_POINT ( 'NONE',  ( 24.04475233726670780, -15.61618925176752271, -59.50766149565701113 ) ) ;
#36992 = CARTESIAN_POINT ( 'NONE',  ( 16.13393739769620083, -15.61618894467929941, -23.15000000000000213 ) ) ;
#36993 = CARTESIAN_POINT ( 'NONE',  ( 53.51849367552510017, 19.79182752219439934, -75.95517943487810442 ) ) ;
#36994 = ORIENTED_EDGE ( 'NONE', *, *, #24854, .F. ) ;
#36995 = CYLINDRICAL_SURFACE ( 'NONE', #2471, 1.500000000000001332 ) ;
#36996 = CARTESIAN_POINT ( 'NONE',  ( 42.05506414891981848, 6.400113107552978242, -80.04430332523035929 ) ) ;
#36997 = CARTESIAN_POINT ( 'NONE',  ( 68.13393739769620083, 0.8838110553206759423, -65.65000000000000568 ) ) ;
#36998 = CARTESIAN_POINT ( 'NONE',  ( 24.14537261347669883, -17.56545184108060198, -49.86830329880680068 ) ) ;
#36999 = CARTESIAN_POINT ( 'NONE',  ( 17.27328981822006781, -8.887235580817069547, -56.00650926761637294 ) ) ;
#37000 = CARTESIAN_POINT ( 'NONE',  ( 42.64819641985740617, -37.72516299508219362, -77.07863785855882099 ) ) ;
#37001 = ORIENTED_EDGE ( 'NONE', *, *, #4468, .F. ) ;
#37002 = CIRCLE ( 'NONE', #22763, 2.576499999999998902 ) ;
#37003 = DIRECTION ( 'NONE',  ( 0.000000000000000000, 1.000000000000000000, 0.000000000000000000 ) ) ;
#37004 = CARTESIAN_POINT ( 'NONE',  ( 17.51573946485870081, -8.295170104904951103, -37.79203799605679848 ) ) ;
#37005 = AXIS2_PLACEMENT_3D ( 'NONE', #32484, #12102, #12350 ) ;
#37006 = CARTESIAN_POINT ( 'NONE',  ( 17.16941988147922160, -7.705179696712606940, -33.04933253539134341 ) ) ;
#37007 = CARTESIAN_POINT ( 'NONE',  ( 14.55217714119870109, 21.30155813473500004, -76.03742712147929694 ) ) ;
#37008 = B_SPLINE_CURVE_WITH_KNOTS ( 'NONE', 3,
 ( #49572, #25936, #49818, #13405, #29364, #45887, #34060, #9974, #50069, #1076, #41951, #22008, #38017, #42211, #33025, #45369, #17074, #37496, #13156, #1596, #17584, #29106, #45105, #9211, #33554, #29618, #30902, #10758, #34585, #50846 ),
 .UNSPECIFIED., .F., .F.,
 ( 4, 2, 2, 2, 2, 2, 2, 2, 2, 2, 2, 2, 2, 2, 4 ),
 ( -1.979528000000000055E-13, 0.03743706954986000118, 0.1081389423207600037, 0.1523276128025730092, 0.1872210672024020028, 0.2221145216022309965, 0.2911209749156069559, 0.3342500082364670555, 0.3773790415573270440, 0.4312903332084020436, 0.4852016248594769876, 0.5714596915011970202, 0.6485557695154610114, 0.7719094943382839302, 0.8625806664170020399 ),
 .UNSPECIFIED. ) ;
#37009 = CARTESIAN_POINT ( 'NONE',  ( 23.93131328127537216, -16.97972217673644835, -59.84741592005993027 ) ) ;
#37010 = B_SPLINE_CURVE_WITH_KNOTS ( 'NONE', 3,
 ( #40992, #48342, #48603, #36017, #11936, #16105, #36791, #28143, #20535, #28923 ),
 .UNSPECIFIED., .F., .F.,
 ( 4, 1, 1, 1, 1, 1, 1, 4 ),
 ( 0.000000000000000000, 0.04961520431741933690, 0.1288341353810688872, 0.2080530664447206579, 0.2872719975083702360, 0.3664909285720209242, 0.4457098596356703912, 0.4999963331327971772 ),
 .UNSPECIFIED. ) ;
#37011 = CARTESIAN_POINT ( 'NONE',  ( 84.42050518244900559, -43.28355784542729623, -47.35805390042769858 ) ) ;
#37012 = CARTESIAN_POINT ( 'NONE',  ( 8.436496967347979492, -18.57120697004150145, -56.39099290546749899 ) ) ;
#37013 = VERTEX_POINT ( 'NONE', #36668 ) ;
#37014 = CARTESIAN_POINT ( 'NONE',  ( 55.96445070656709930, -46.24620190255259899, -26.04161240161580082 ) ) ;
#37015 = CARTESIAN_POINT ( 'NONE',  ( 14.24082757525520115, -51.10274004714279528, -22.22799665057710072 ) ) ;
#37016 = CARTESIAN_POINT ( 'NONE',  ( 9.637419681166790042, -20.21905395439925002, -40.31160479408269737 ) ) ;
#37017 = CARTESIAN_POINT ( 'NONE',  ( 57.26283657379340042, 19.38381106601499937, -53.75815476539330007 ) ) ;
#37018 = EDGE_CURVE ( 'NONE', #37975, #50570, #18003, .T. ) ;
#37019 = CARTESIAN_POINT ( 'NONE',  ( 9.367509130462650546, -15.61619940421079988, -51.84717978381009118 ) ) ;
#37020 = CARTESIAN_POINT ( 'NONE',  ( 45.07858682377059978, 14.88010818488339915, -9.026855431852879974 ) ) ;
#37021 = ORIENTED_EDGE ( 'NONE', *, *, #37853, .T. ) ;
#37022 = CARTESIAN_POINT ( 'NONE',  ( -6.896370999502840604, -45.95266115723829614, -5.351785064663849845 ) ) ;
#37023 = EDGE_CURVE ( 'NONE', #35823, #21743, #15998, .T. ) ;
#37024 = CARTESIAN_POINT ( 'NONE',  ( 47.20755063152770248, 23.55563156955719961, -54.64231554542519831 ) ) ;
#37025 = DIRECTION ( 'NONE',  ( 0.000000000000000000, -1.000000000000000000, 0.000000000000000000 ) ) ;
#37026 = CARTESIAN_POINT ( 'NONE',  ( 63.22121223625140374, 0.9369374701296400154, -62.20531809130540069 ) ) ;
#37027 = CARTESIAN_POINT ( 'NONE',  ( 68.13393739769840352, -50.61618894467879670, -73.25000000000220268 ) ) ;
#37028 = CARTESIAN_POINT ( 'NONE',  ( 11.88973808303819979, 34.20270277534309855, -17.85918046449339869 ) ) ;
#37029 = ADVANCED_FACE ( 'NONE', ( #44545 ), #18869, .T. ) ;
#37030 = DIRECTION ( 'NONE',  ( 1.000000000000000000, 0.000000000000000000, 0.000000000000000000 ) ) ;
#37031 = DIRECTION ( 'NONE',  ( -0.8090169943749466741, -0.5877852522924741363, 0.000000000000000000 ) ) ;
#37032 = LINE ( 'NONE', #12939, #38331 ) ;
#37033 = CARTESIAN_POINT ( 'NONE',  ( 58.68718041671409935, -46.61650995022520050, -47.74352678257979221 ) ) ;
#37034 = CARTESIAN_POINT ( 'NONE',  ( 13.35882351263044221, -21.87618856300440839, -67.08522217579282199 ) ) ;
#37035 = CARTESIAN_POINT ( 'NONE',  ( 52.77452256448989942, 20.89620967665909745, -53.50297542258699934 ) ) ;
#37036 = CARTESIAN_POINT ( 'NONE',  ( 11.27230809297926051, -9.289986881467834579, -77.08399725981655592 ) ) ;
#37037 = CARTESIAN_POINT ( 'NONE',  ( 20.29259450369849560, -10.20485895348243410, -48.16115496514827754 ) ) ;
#37038 = VERTEX_POINT ( 'NONE', #40356 ) ;
#37039 = CARTESIAN_POINT ( 'NONE',  ( 34.63393739890910439, -15.61618894518879941, 4.349999999448538546 ) ) ;
#37040 = CARTESIAN_POINT ( 'NONE',  ( 8.972584494015238832, 32.01420432709309694, -46.63288471805530122 ) ) ;
#37041 = VECTOR ( 'NONE', #6068, 1000.000000000000000 ) ;
#37042 = DIRECTION ( 'NONE',  ( 0.000000000000000000, -0.7071067811865475727, 0.7071067811865475727 ) ) ;
#37043 = CARTESIAN_POINT ( 'NONE',  ( 66.69979053676949832, -29.76856963367809783, -17.02723542833530246 ) ) ;
#37044 = ORIENTED_EDGE ( 'NONE', *, *, #12964, .T. ) ;
#37045 = CARTESIAN_POINT ( 'NONE',  ( 18.42983928211069866, 20.84559406376740043, -75.48537863783369062 ) ) ;
#37046 = ORIENTED_EDGE ( 'NONE', *, *, #34670, .T. ) ;
#37047 = ORIENTED_EDGE ( 'NONE', *, *, #4336, .T. ) ;
#37048 = CARTESIAN_POINT ( 'NONE',  ( 48.47823774206090519, 22.94606279175499708, -55.31601837894839946 ) ) ;
#37049 = EDGE_LOOP ( 'NONE', ( #2830, #8133, #43437, #29246, #13662, #11408, #41611 ) ) ;
#37050 = ADVANCED_FACE ( 'NONE', ( #20419 ), #40613, .T. ) ;
#37051 = CARTESIAN_POINT ( 'NONE',  ( 13.00893739769619906, -65.51843714052719747, -47.75434321273180416 ) ) ;
#37052 = CARTESIAN_POINT ( 'NONE',  ( 56.92231951192260198, -45.87375801872750003, -26.22432845751160002 ) ) ;
#37053 = CARTESIAN_POINT ( 'NONE',  ( 20.11399144799549887, -21.27607163836539783, -81.23899999999999011 ) ) ;
#37054 = CARTESIAN_POINT ( 'NONE',  ( 61.43383643809819716, 14.05069848591710091, -47.14994843957639858 ) ) ;
#37055 = CARTESIAN_POINT ( 'NONE',  ( 64.88669131378958355, 1.400446703426900141, -61.07889042780649902 ) ) ;
#37056 = VERTEX_POINT ( 'NONE', #20679 ) ;
#37057 = DIRECTION ( 'NONE',  ( 1.000000000000000000, 0.000000000000000000, 0.000000000000000000 ) ) ;
#37058 = CARTESIAN_POINT ( 'NONE',  ( 12.08205733926943637, 34.04687828595569243, -16.92411153880798125 ) ) ;
#37059 = VERTEX_POINT ( 'NONE', #47974 ) ;
#37060 = CARTESIAN_POINT ( 'NONE',  ( 13.61100063765979407, -17.44920979631380220, -28.02168704970069868 ) ) ;
#37061 = CARTESIAN_POINT ( 'NONE',  ( -0.007164426707907000161, -50.71887597443840434, -34.77269723932290191 ) ) ;
#37062 = CARTESIAN_POINT ( 'NONE',  ( 16.13393739769620083, -15.61618894467929941, -7.393828452885189861 ) ) ;
#37063 = VERTEX_POINT ( 'NONE', #19914 ) ;
#37064 = ORIENTED_EDGE ( 'NONE', *, *, #9214, .T. ) ;
#37065 = B_SPLINE_CURVE_WITH_KNOTS ( 'NONE', 3,
 ( #16590, #28375, #8222, #8484, #7720, #24430, #20509, #40444, #4535, #32543, #28117, #47805, #48579, #27867, #28634, #23665, #39679, #3785, #35993, #19755, #35746, #40193, #11911, #43867, #39940, #109, #16081, #32040, #33861 ),
 .UNSPECIFIED., .F., .F.,
 ( 4, 2, 1, 1, 1, 1, 1, 2, 2, 2, 2, 2, 2, 2, 2, 2, 4 ),
 ( 0.5000038086628445511, 0.5002479474281459337, 0.5004920861934472054, 0.5009803637240499707, 0.5019569187852552794, 0.5039100289076660077, 0.5078162491524875755, 0.5156286896421305999, 0.5312535706214167597, 0.5625033325799890793, 0.6250028564971334966, 0.6875023804142779138, 0.7500019043314223310, 0.8125014282485667483, 0.8750009521657111655, 0.9375004760828555828, 1.000000000000000000 ),
 .UNSPECIFIED. ) ;
#37066 = CARTESIAN_POINT ( 'NONE',  ( 68.13393739769620083, 19.38381105532069881, -71.50000000000000000 ) ) ;
#37067 = CARTESIAN_POINT ( 'NONE',  ( 47.15605882434359586, -54.68808827254829907, -74.81076251056920512 ) ) ;
#37068 = CARTESIAN_POINT ( 'NONE',  ( 16.13393739769620083, -15.61618894467929941, 6.072546842075589701 ) ) ;
#37069 = ADVANCED_FACE ( 'NONE', ( #23828 ), #31380, .F. ) ;
#37070 = EDGE_CURVE ( 'NONE', #26662, #16668, #8816, .T. ) ;
#37071 = CARTESIAN_POINT ( 'NONE',  ( 53.99077097435189643, 14.78852379608610157, -15.26363591289520016 ) ) ;
#37072 = CARTESIAN_POINT ( 'NONE',  ( 8.428856657643047257, -17.68693864638044744, -68.70899797463333414 ) ) ;
#37073 = CARTESIAN_POINT ( 'NONE',  ( -7.623077062098630563, 14.06405699089660111, -5.205469451225369859 ) ) ;
#37074 = VECTOR ( 'NONE', #37537, 1000.000000000000000 ) ;
#37075 = AXIS2_PLACEMENT_3D ( 'NONE', #42623, #18240, #34992 ) ;
#37076 = CARTESIAN_POINT ( 'NONE',  ( 22.64876182410736050, -18.03120546031163585, -54.96075032149187933 ) ) ;
#37077 = CARTESIAN_POINT ( 'NONE',  ( 60.70254012041490199, 13.94047785219770041, -26.91002252692619834 ) ) ;
#37078 = CARTESIAN_POINT ( 'NONE',  ( 19.22389005490540015, -22.82999104616420283, -75.65868704446690174 ) ) ;
#37079 = ORIENTED_EDGE ( 'NONE', *, *, #45508, .T. ) ;
#37080 = CARTESIAN_POINT ( 'NONE',  ( 55.02590511137680096, 17.27791867893839850, -48.37054070093110170 ) ) ;
#37081 = CARTESIAN_POINT ( 'NONE',  ( -9.957799118347489653, -43.31361225047390207, -6.454149760335369912 ) ) ;
#37082 = LINE ( 'NONE', #37863, #51321 ) ;
#37083 = CARTESIAN_POINT ( 'NONE',  ( 72.72018323891309421, 1.017423949636760083, -69.51966756621098398 ) ) ;
#37084 = EDGE_CURVE ( 'NONE', #26020, #21076, #51527, .T. ) ;
#37085 = CARTESIAN_POINT ( 'NONE',  ( 14.37540540599763794, 10.62527906362193519, -34.70142521051219120 ) ) ;
#37086 = CARTESIAN_POINT ( 'NONE',  ( 11.19961949155312553, 34.01496270439587732, -18.17421237848505911 ) ) ;
#37087 = CARTESIAN_POINT ( 'NONE',  ( 13.03467379948559923, 18.88909056995609603, -21.08705176942839898 ) ) ;
#37088 = EDGE_CURVE ( 'NONE', #27935, #25861, #12075, .T. ) ;
#37089 = CARTESIAN_POINT ( 'NONE',  ( 47.12095841086310344, 23.37868049473910048, -75.00831431077000389 ) ) ;
#37090 = CARTESIAN_POINT ( 'NONE',  ( 49.50151222300969778, -53.58170550938950072, -54.38302206046300569 ) ) ;
#37091 = CARTESIAN_POINT ( 'NONE',  ( 42.80890084010550112, -44.10023144781310123, -5.063862467037759885 ) ) ;
#37092 = AXIS2_PLACEMENT_3D ( 'NONE', #11857, #12104, #27812 ) ;
#37093 = CARTESIAN_POINT ( 'NONE',  ( 8.291851457509455514, -16.78737382061565953, -34.46050489558400187 ) ) ;
#37094 = CARTESIAN_POINT ( 'NONE',  ( 65.03603135455020379, -32.24781572988710110, -17.83403478221860183 ) ) ;
#37095 = FACE_OUTER_BOUND ( 'NONE', #35183, .T. ) ;
#37096 = EDGE_LOOP ( 'NONE', ( #34567, #36956, #51293, #42817 ) ) ;
#37097 = CARTESIAN_POINT ( 'NONE',  ( 9.205714170480751690, -12.87640478306839853, -48.18721185593089729 ) ) ;
#37098 = CARTESIAN_POINT ( 'NONE',  ( 64.36548184775359971, 0.9973858971043548793, -60.98020530084170332 ) ) ;
#37099 = ORIENTED_EDGE ( 'NONE', *, *, #44404, .T. ) ;
#37100 = CARTESIAN_POINT ( 'NONE',  ( 83.63329919740728258, -44.53040215208500996, -46.55718455497714103 ) ) ;
#37101 = CARTESIAN_POINT ( 'NONE',  ( 60.90580219148289842, -45.59792408994620416, -47.59486805843899759 ) ) ;
#37102 = CARTESIAN_POINT ( 'NONE',  ( 57.24718408628069710, 19.38381105960650075, -53.91456318494540056 ) ) ;
#37103 = CARTESIAN_POINT ( 'NONE',  ( 50.52803440128089818, 19.14656596045000114, -76.14999999999999147 ) ) ;
#37105 = LINE ( 'NONE', #13530, #8925 ) ;
#37104 = CARTESIAN_POINT ( 'NONE',  ( 45.05697163777319503, 8.802134928348412046, -61.53621250105515372 ) ) ;
#37106 = CARTESIAN_POINT ( 'NONE',  ( 18.71043739769620018, -15.61618894467929941, -31.39999999999999858 ) ) ;
#37107 = DIRECTION ( 'NONE',  ( 1.000000000000000000, 0.000000000000000000, 0.000000000000000000 ) ) ;
#37108 = ORIENTED_EDGE ( 'NONE', *, *, #25115, .T. ) ;
#37109 = CARTESIAN_POINT ( 'NONE',  ( 82.70745875113280476, -45.46473719772439637, -47.51979026979380194 ) ) ;
#37110 = ORIENTED_EDGE ( 'NONE', *, *, #29368, .F. ) ;
#37111 = ORIENTED_EDGE ( 'NONE', *, *, #33163, .F. ) ;
#37112 = AXIS2_PLACEMENT_3D ( 'NONE', #37039, #24955, #3333 ) ;
#37113 = VERTEX_POINT ( 'NONE', #31951 ) ;
#37114 = PLANE ( 'NONE',  #11915 ) ;
#37115 = FACE_OUTER_BOUND ( 'NONE', #30370, .T. ) ;
#37116 = AXIS2_PLACEMENT_3D ( 'NONE', #8551, #5145, #21099 ) ;
#37117 = CARTESIAN_POINT ( 'NONE',  ( 56.45053593251559931, -50.66578230959599694, -53.16922271350729545 ) ) ;
#37118 = AXIS2_PLACEMENT_3D ( 'NONE', #51307, #39762, #4110 ) ;
#37119 = ORIENTED_EDGE ( 'NONE', *, *, #10520, .F. ) ;
#37120 = ORIENTED_EDGE ( 'NONE', *, *, #20026, .T. ) ;
#37121 = CARTESIAN_POINT ( 'NONE',  ( 11.78282090895823053, 34.18901486863271799, -22.36199502296781816 ) ) ;
#37122 = EDGE_LOOP ( 'NONE', ( #5554, #1466, #14009, #20261, #33933, #41798, #44396, #34334 ) ) ;
#37123 = CARTESIAN_POINT ( 'NONE',  ( 56.76343336529819794, 19.30417086840829910, -53.08899915780749978 ) ) ;
#37124 = CARTESIAN_POINT ( 'NONE',  ( -8.713277369480067591, 14.44436079558252928, -42.72765124578886287 ) ) ;
#37125 = FACE_OUTER_BOUND ( 'NONE', #5235, .T. ) ;
#37126 = FACE_OUTER_BOUND ( 'NONE', #18417, .T. ) ;
#37127 = ORIENTED_EDGE ( 'NONE', *, *, #25525, .F. ) ;
#37128 = DIRECTION ( 'NONE',  ( 0.7071067811865475727, -0.7071067811865475727, 0.000000000000000000 ) ) ;
#37129 = CARTESIAN_POINT ( 'NONE',  ( 51.93051814572950065, -50.26010286414289396, -76.53037494222229498 ) ) ;
#37130 = CARTESIAN_POINT ( 'NONE',  ( 21.21558964501896938, -20.08614974262806285, -46.68245235485807854 ) ) ;
#37131 = CARTESIAN_POINT ( 'NONE',  ( 83.76204656032335549, -44.99353952466995565, -47.48603732813779033 ) ) ;
#37132 = EDGE_CURVE ( 'NONE', #26710, #13022, #32231, .T. ) ;
#37133 = CARTESIAN_POINT ( 'NONE',  ( 20.81968612761309956, -21.91146546216959834, -68.30882034609030029 ) ) ;
#37134 = EDGE_CURVE ( 'NONE', #26529, #45038, #44033, .T. ) ;
#37135 = CARTESIAN_POINT ( 'NONE',  ( 8.643872352928719138, 17.52418497763089889, -35.12503119152809461 ) ) ;
#37136 = AXIS2_PLACEMENT_3D ( 'NONE', #12812, #44768, #4932 ) ;
#37137 = CARTESIAN_POINT ( 'NONE',  ( 41.34377115688720750, 13.52348016558920030, -5.356934324971369676 ) ) ;
#37138 = CARTESIAN_POINT ( 'NONE',  ( 42.26864886252769793, -44.36179212852169940, -5.126484877156399556 ) ) ;
#37139 = EDGE_CURVE ( 'NONE', #14944, #2360, #28881, .T. ) ;
#37140 = CARTESIAN_POINT ( 'NONE',  ( -11.32734370190460105, 10.64934056395049922, -6.430561461456250072 ) ) ;
#37141 = DIRECTION ( 'NONE',  ( 1.000000000000000000, 0.000000000000000000, 0.000000000000000000 ) ) ;
#37142 =( BOUNDED_CURVE ( )  B_SPLINE_CURVE ( 3, ( #1241, #44225, #16978, #12263 ),
 .UNSPECIFIED., .F., .T. ) 
 B_SPLINE_CURVE_WITH_KNOTS ( ( 4, 4 ),
 ( 3.141592653589798445, 4.527609048992159657 ),
 .UNSPECIFIED. ) 
 CURVE ( )  GEOMETRIC_REPRESENTATION_ITEM ( )  RATIONAL_B_SPLINE_CURVE ( ( 1.000000000000000000, 0.8462184657327389559, 0.8462184657327389559, 1.000000000000000000 ) ) 
 REPRESENTATION_ITEM ( '' )  );
#37143 = CARTESIAN_POINT ( 'NONE',  ( 63.83267354985680697, 1.033012681683360023, -69.83402047387529876 ) ) ;
#37144 = CARTESIAN_POINT ( 'NONE',  ( 20.11812388789995154, -8.703698750585735056, -41.45899779116474804 ) ) ;
#37145 = CARTESIAN_POINT ( 'NONE',  ( 65.32710660623050103, 0.7917214628020530220, -17.54847713914429974 ) ) ;
#37146 = VERTEX_POINT ( 'NONE', #36941 ) ;
#37147 = CARTESIAN_POINT ( 'NONE',  ( 14.32991954030070048, -51.86173801737519540, -75.67066142420200947 ) ) ;
#37148 = CARTESIAN_POINT ( 'NONE',  ( 57.36123080758890325, 18.90300134970469870, -52.61896056700089730 ) ) ;
#37149 = LINE ( 'NONE', #37657, #24714 ) ;
#37150 = DIRECTION ( 'NONE',  ( 0.000000000000000000, 0.000000000000000000, -1.000000000000000000 ) ) ;
#37151 = CARTESIAN_POINT ( 'NONE',  ( 8.223600577592289795, -15.61621812327629932, -68.50766849176299900 ) ) ;
#37152 = CARTESIAN_POINT ( 'NONE',  ( 23.15196511571160087, -18.23446988725689977, -32.14999999999999858 ) ) ;
#37153 = FACE_OUTER_BOUND ( 'NONE', #12175, .T. ) ;
#37154 = ADVANCED_FACE ( 'NONE', ( #32720 ), #37982, .T. ) ;
#37155 = CARTESIAN_POINT ( 'NONE',  ( 11.51841290286379937, 34.14186997694120862, -17.84188021311150152 ) ) ;
#37157 = CARTESIAN_POINT ( 'NONE',  ( 23.83903610038404608, -17.68687214694392651, -51.87566247315886869 ) ) ;
#37156 = DIRECTION ( 'NONE',  ( 0.000000000000000000, 0.000000000000000000, 1.000000000000000000 ) ) ;
#37158 = CARTESIAN_POINT ( 'NONE',  ( 56.36581425992820726, 19.41514254598320122, -53.07180551597519980 ) ) ;
#37159 = APPLICATION_CONTEXT ( 'automotive_design' ) ;
#37160 = CARTESIAN_POINT ( 'NONE',  ( 48.85702442728319284, 22.78471410673780184, -55.29194429108009956 ) ) ;
#37161 = ORIENTED_EDGE ( 'NONE', *, *, #24467, .T. ) ;
#37162 = CARTESIAN_POINT ( 'NONE',  ( 22.79673239389820338, -13.30324233633820086, -58.74082357793209752 ) ) ;
#37163 = VERTEX_POINT ( 'NONE', #13873 ) ;
#37164 = DIRECTION ( 'NONE',  ( 0.000000000000000000, -0.7071067811865492381, -0.7071067811865457964 ) ) ;
#37165 = CARTESIAN_POINT ( 'NONE',  ( 11.63393739769600010, 10.38381105532060111, -35.14999999999999858 ) ) ;
#37166 = CARTESIAN_POINT ( 'NONE',  ( 14.16187783161720048, 19.11875810978959933, -20.85710678118659800 ) ) ;
#37168 = CARTESIAN_POINT ( 'NONE',  ( 54.89514228079339375, 15.99142857377610127, -25.88804800509620208 ) ) ;
#37167 = CARTESIAN_POINT ( 'NONE',  ( 83.82044569750020457, 13.55688828085889952, -47.35730118573349756 ) ) ;
#37169 = CARTESIAN_POINT ( 'NONE',  ( 22.71369373737119801, -18.15574898672049997, -62.57006952842979075 ) ) ;
#37170 = DIRECTION ( 'NONE',  ( 0.000000000000000000, -1.000000000000000000, 0.000000000000000000 ) ) ;
#37171 = CARTESIAN_POINT ( 'NONE',  ( 61.50409964636570237, 14.14168666559669951, -47.35437808293550432 ) ) ;
#37172 = LINE ( 'NONE', #9135, #38163 ) ;
#37173 = CIRCLE ( 'NONE', #45519, 5.500000000000000000 ) ;
#37174 = ORIENTED_EDGE ( 'NONE', *, *, #6646, .T. ) ;
#37175 = ORIENTED_EDGE ( 'NONE', *, *, #32926, .F. ) ;
#37176 = CARTESIAN_POINT ( 'NONE',  ( 11.93872965651020124, -65.19885638306720921, -16.76612700403689971 ) ) ;
#37177 = CARTESIAN_POINT ( 'NONE',  ( 11.91647380877470042, 33.89555377125369517, -46.05219393946750017 ) ) ;
#37178 = DIRECTION ( 'NONE',  ( 0.000000000000000000, 0.000000000000000000, -1.000000000000000000 ) ) ;
#37179 = CARTESIAN_POINT ( 'NONE',  ( 52.10268719324110265, -50.36005704266560201, -49.19170910618320391 ) ) ;
#37180 = CARTESIAN_POINT ( 'NONE',  ( 51.49832873845635817, 3.074675621640686973, -76.79134042563141804 ) ) ;
#37181 = ORIENTED_EDGE ( 'NONE', *, *, #51047, .F. ) ;
#37182 = CARTESIAN_POINT ( 'NONE',  ( -22.53234341801570295, -21.49586800030930078, -54.54381104595779561 ) ) ;
#37183 = CARTESIAN_POINT ( 'NONE',  ( 57.34776335324270491, 14.57942837581910034, -26.27178905609630277 ) ) ;
#37184 = CARTESIAN_POINT ( 'NONE',  ( 18.13393739769630031, 1.391621760993470014, -35.14999999999999858 ) ) ;
#37185 = VECTOR ( 'NONE', #26562, 1000.000000000000114 ) ;
#37186 = CARTESIAN_POINT ( 'NONE',  ( 50.45277833511170229, 21.36013689488169831, -53.06622874095319986 ) ) ;
#37187 = FACE_OUTER_BOUND ( 'NONE', #34649, .T. ) ;
#37188 = CARTESIAN_POINT ( 'NONE',  ( 63.43393739769620510, 1.383811055320669947, -62.79342862858290886 ) ) ;
#37189 = CARTESIAN_POINT ( 'NONE',  ( 9.221411471344291400, -19.60031560563376374, -44.34101869606306678 ) ) ;
#37190 = ORIENTED_EDGE ( 'NONE', *, *, #47809, .T. ) ;
#37191 = CARTESIAN_POINT ( 'NONE',  ( 22.90093741817085515, -14.73039762558461341, -68.41115124640887757 ) ) ;
#37192 = FACE_OUTER_BOUND ( 'NONE', #42159, .T. ) ;
#37193 = ORIENTED_EDGE ( 'NONE', *, *, #16308, .F. ) ;
#37194 = CARTESIAN_POINT ( 'NONE',  ( 12.51334871620187350, -55.45190834908655830, -75.31104306447832641 ) ) ;
#37195 = CARTESIAN_POINT ( 'NONE',  ( 72.83393739769620367, 1.883811055320669947, -65.65000000000000568 ) ) ;
#37196 = CARTESIAN_POINT ( 'NONE',  ( 8.334470150558480839, -16.48513208769189831, -32.97717709171600120 ) ) ;
#37197 = EDGE_CURVE ( 'NONE', #25307, #33390, #5752, .T. ) ;
#37198 = FACE_OUTER_BOUND ( 'NONE', #2755, .T. ) ;
#37199 = CARTESIAN_POINT ( 'NONE',  ( 22.90097009252848892, -15.61618913824531418, -68.84717732178738459 ) ) ;
#37200 = CARTESIAN_POINT ( 'NONE',  ( 46.42423052835359698, -53.00637862934869560, -76.14999999999999147 ) ) ;
#37201 = EDGE_LOOP ( 'NONE', ( #21828, #25762, #29049, #6929 ) ) ;
#37202 = CARTESIAN_POINT ( 'NONE',  ( 54.56504058078360231, 14.73772175096070036, -15.64073168106889788 ) ) ;
#37203 = CARTESIAN_POINT ( 'NONE',  ( 57.02020363348529486, -50.59809222457260347, -53.44649995476070359 ) ) ;
#37204 = CARTESIAN_POINT ( 'NONE',  ( 17.32262310423930174, -8.664240623128929286, -36.40108501799139873 ) ) ;
#37205 = DIRECTION ( 'NONE',  ( -0.000000000000000000, 1.000000000000000000, 0.000000000000000000 ) ) ;
#37206 = ORIENTED_EDGE ( 'NONE', *, *, #11171, .F. ) ;
#37207 = AXIS2_PLACEMENT_3D ( 'NONE', #34406, #7423, #11105 ) ;
#37208 = CARTESIAN_POINT ( 'NONE',  ( 47.02522487057739653, 22.84427288168209813, -75.65261601872900599 ) ) ;
#37209 = CARTESIAN_POINT ( 'NONE',  ( 65.17800597998859757, 1.373356196620459935, -60.86873524938349789 ) ) ;
#37210 = EDGE_CURVE ( 'NONE', #47819, #8620, #35595, .T. ) ;
#37211 = CARTESIAN_POINT ( 'NONE',  ( 41.26357389881030002, -45.58122989547749881, -6.211371138913489354 ) ) ;
#37212 = CARTESIAN_POINT ( 'NONE',  ( 12.36320305067610015, 33.31445045643330616, -15.76422791930239953 ) ) ;
#37213 = CARTESIAN_POINT ( 'NONE',  ( 12.41372322625400137, -22.97436356901700094, -80.15667222455330432 ) ) ;
#37214 = EDGE_CURVE ( 'NONE', #13573, #46163, #6316, .T. ) ;
#37215 = DIRECTION ( 'NONE',  ( 0.000000000000000000, -1.000000000000000000, 0.000000000000000000 ) ) ;
#37216 = DIRECTION ( 'NONE',  ( 0.000000000000000000, -1.000000000000000000, 0.000000000000000000 ) ) ;
#37218 = CARTESIAN_POINT ( 'NONE',  ( 44.27243015989088804, -40.08314457256550867, -64.90451195649632155 ) ) ;
#37217 = DIRECTION ( 'NONE',  ( 1.681987882033212302E-11, -1.000000000000000000, 0.000000000000000000 ) ) ;
#37219 = AXIS2_PLACEMENT_3D ( 'NONE', #3317, #30813, #18775 ) ;
#37220 = ADVANCED_FACE ( 'NONE', ( #8914 ), #38988, .F. ) ;
#37221 = DIRECTION ( 'NONE',  ( 0.3294064756441309472, 0.9441882088883087887, -3.053113317719179500E-16 ) ) ;
#37222 = CARTESIAN_POINT ( 'NONE',  ( -25.59424942068570275, -40.82387122898790466, -54.31183179444199993 ) ) ;
#37223 = CIRCLE ( 'NONE', #7821, 5.499999999999998224 ) ;
#37224 = ORIENTED_EDGE ( 'NONE', *, *, #24149, .T. ) ;
#37225 = CARTESIAN_POINT ( 'NONE',  ( 52.95585360091419602, -49.59527434762240006, -48.79473317602730020 ) ) ;
#37226 = CARTESIAN_POINT ( 'NONE',  ( 58.64502850088660324, -45.25097017255860266, -26.10756731467850145 ) ) ;
#37227 = FACE_OUTER_BOUND ( 'NONE', #893, .T. ) ;
#37228 = CARTESIAN_POINT ( 'NONE',  ( 13.45432746122430068, 19.59659184310620006, -21.59563733192320001 ) ) ;
#37229 = CARTESIAN_POINT ( 'NONE',  ( 56.93624918340190533, 14.63482917628590130, -26.22451992585920166 ) ) ;
#37230 = CARTESIAN_POINT ( 'NONE',  ( 8.713847312995159911, -16.28566013226560116, -81.20401221892029753 ) ) ;
#37231 = CARTESIAN_POINT ( 'NONE',  ( 50.12211799414349400, 17.52854795053300307, -76.14999999999999147 ) ) ;
#37232 = CARTESIAN_POINT ( 'NONE',  ( 52.82044782574460129, 18.44684647757109985, -48.83393253442750392 ) ) ;
#37233 = CARTESIAN_POINT ( 'NONE',  ( 71.17189893730710537, 1.387131204727280132, -70.29242575817399086 ) ) ;
#37234 = CARTESIAN_POINT ( 'NONE',  ( 41.03393739769609994, -15.61618894467929586, 8.449999999999974420 ) ) ;
#37235 = CARTESIAN_POINT ( 'NONE',  ( 75.49020191205489994, -43.37239104213820440, -13.40805175275450090 ) ) ;
#37236 = ORIENTED_EDGE ( 'NONE', *, *, #1757, .F. ) ;
#37237 = CARTESIAN_POINT ( 'NONE',  ( 12.98003058962980028, -8.866406267853768952, -72.42820476139830532 ) ) ;
#37238 = CARTESIAN_POINT ( 'NONE',  ( 73.04443511092439678, 0.9036513197889520788, -69.09785636402040154 ) ) ;
#37239 = CARTESIAN_POINT ( 'NONE',  ( 47.44496049464380150, -54.63145718528269867, -54.91866264090269567 ) ) ;
#37240 = CARTESIAN_POINT ( 'NONE',  ( -1.504259202252973493, -15.61618894397937751, 14.62639320225000006 ) ) ;
#37241 = DIRECTION ( 'NONE',  ( 0.000000000000000000, 0.000000000000000000, -1.000000000000000000 ) ) ;
#37242 = CARTESIAN_POINT ( 'NONE',  ( 58.91899206676210810, -28.48616099405090196, -15.64938374009210165 ) ) ;
#37243 = DIRECTION ( 'NONE',  ( 0.000000000000000000, -1.000000000000000000, 0.000000000000000000 ) ) ;
#37244 = DIRECTION ( 'NONE',  ( 0.000000000000000000, 0.000000000000000000, -1.000000000000000000 ) ) ;
#37245 = CARTESIAN_POINT ( 'NONE',  ( 71.65879992446289748, 1.379674774869709797, -61.09137707357210445 ) ) ;
#37246 = CARTESIAN_POINT ( 'NONE',  ( 64.43393739769619799, 10.88381105532070059, -68.84999999999999432 ) ) ;
#37247 = CARTESIAN_POINT ( 'NONE',  ( 64.92520290936280958, 0.8850831926798630178, -70.72000234600830026 ) ) ;
#37248 = ORIENTED_EDGE ( 'NONE', *, *, #28898, .F. ) ;
#37249 = AXIS2_PLACEMENT_3D ( 'NONE', #21898, #10651, #18502 ) ;
#37250 = CARTESIAN_POINT ( 'NONE',  ( 8.815605939025839888, -63.28267558187339148, -46.67186391138339729 ) ) ;
#37251 = FACE_OUTER_BOUND ( 'NONE', #35314, .T. ) ;
#37252 = VERTEX_POINT ( 'NONE', #48755 ) ;
#37253 = DIRECTION ( 'NONE',  ( 0.000000000000000000, -1.000000000000000000, 0.000000000000000000 ) ) ;
#37254 = CARTESIAN_POINT ( 'NONE',  ( 11.97526568333010033, -10.20486919016092564, -69.74448779737157622 ) ) ;
#37255 = DIRECTION ( 'NONE',  ( 1.224646799147353207E-16, 1.000000000000000000, -0.000000000000000000 ) ) ;
#37256 = CARTESIAN_POINT ( 'NONE',  ( 51.62415641043660486, 19.44432096110770303, -76.24933075980271724 ) ) ;
#37257 = VERTEX_POINT ( 'NONE', #49023 ) ;
#37258 = FACE_OUTER_BOUND ( 'NONE', #28453, .T. ) ;
#37259 = DIRECTION ( 'NONE',  ( -0.7089970498513415986, 0.7052114458104705719, -6.938893903906735340E-16 ) ) ;
#37260 = CARTESIAN_POINT ( 'NONE',  ( 11.73137203405252826, -41.76263555408610273, -34.79644660940672196 ) ) ;
#37261 = B_SPLINE_SURFACE_WITH_KNOTS ( 'NONE', 3, 3, ( 
 ( #28629, #44895, #32807, #17121, #45153, #32538, #48833, #17375, #36496, #49618, #33604 ),
 ( #1126, #44630, #5590, #16585, #48573, #9000, #25213, #12936, #24944, #13203, #24685 ),
 ( #17637, #37540, #40955, #1646, #49357, #21028, #49102, #12675, #41218, #37028, #40699 ),
 ( #29152, #21284, #4799, #20766, #5332, #29414, #33074, #37289, #1388, #33342, #13459 ),
 ( #45418, #9523, #6359, #14988, #22319, #38595, #25992, #37812, #42004, #26769, #2165 ),
 ( #18913, #22832, #33856, #27037, #50121, #34632, #34896, #46726, #46206, #2686, #10810 ),
 ( #42786, #2414, #50387, #6102, #13963, #50896, #10291, #30954, #22059, #46465, #6882 ),
 ( #11070, #46986, #38853, #38069, #42260, #18145, #29919, #5840, #26254, #21806, #34109 ),
 ( #2942, #1906, #17885, #49870, #45937, #14217, #38325, #10026, #30190, #18396, #34375 ),
 ( #14471, #30444, #10553, #26510, #42526, #22577, #6614, #18658, #50637, #14733, #30704 ),
 ( #27788, #7635, #31189, #3960, #15746, #27527, #35666, #23833, #43785, #11053, #19420 ),
 ( #39092, #11830, #2926, #3187, #23581, #51396, #23320, #51651, #39598, #27019, #11310 ),
 ( #15495, #43536, #14971, #47221, #47724, #44039, #31960, #47980, #19670, #35398, #43026 ),
 ( #18895, #34881, #27274, #7887, #19157, #51142, #47475, #7124, #39854, #30, #19920 ),
 ( #35913, #12082, #43284, #31447, #28036, #8143, #15239, #24088, #50880, #11568, #46969 ),
 ( #23074, #35137, #7373, #39347, #3447, #273, #45072, #16256, #9179, #16777, #24605 ),
 ( #49279, #4718, #20951, #8400, #20176, #24349, #25136, #36416, #28812, #1312, #5252 ),
 ( #9444, #32459, #17041, #17301, #29079, #28553, #36947, #41139, #21205, #37212, #36674 ) ),
 .UNSPECIFIED., .F., .F., .F.,
 ( 4, 2, 2, 2, 2, 2, 2, 2, 4 ),
 ( 4, 1, 1, 1, 1, 1, 1, 1, 4 ),
 ( -0.8717220151850350041, -0.8429723630856670313, -0.6591356692331089562, -0.5442377355752608947, -0.4350764559609309745, -0.3804958161537659866, -0.2931667924623029831, -0.1534403545559610005, 0.001568662496386999828 ),
 ( 0.000000000000000000, 0.1250000000000000000, 0.2500000000000000000, 0.3750000000000000000, 0.5000000000000000000, 0.6250000000000000000, 0.7500000000000000000, 0.8750000000000000000, 1.000000440766789955 ),
 .UNSPECIFIED. ) ;
#37262 = CARTESIAN_POINT ( 'NONE',  ( 16.71759420731690327, -7.391709338982750843, -57.31488281878699098 ) ) ;
#37263 = EDGE_CURVE ( 'NONE', #16348, #6096, #18979, .T. ) ;
#37264 = CARTESIAN_POINT ( 'NONE',  ( 9.560404261625569333, -13.76607691521293830, -55.53990993375253282 ) ) ;
#37265 = CARTESIAN_POINT ( 'NONE',  ( 42.25617998614456639, -37.66442862941680403, -79.03878004411602376 ) ) ;
#37266 = VERTEX_POINT ( 'NONE', #24608 ) ;
#37267 = CARTESIAN_POINT ( 'NONE',  ( 57.14590266161170007, -45.85825177618220039, -26.25338899624249933 ) ) ;
#37268 = CARTESIAN_POINT ( 'NONE',  ( 17.98718783828190126, -8.400084967489489074, -43.81267675689189645 ) ) ;
#37269 = CARTESIAN_POINT ( 'NONE',  ( 11.43117294225049996, -10.64118341557829872, -32.14999999999999858 ) ) ;
#37270 = CARTESIAN_POINT ( 'NONE',  ( 14.04674101893040117, 20.91311638024189890, -75.69337827730609547 ) ) ;
#37271 = CARTESIAN_POINT ( 'NONE',  ( 9.122145535666252414, -19.41028161033098343, -60.63421390308896264 ) ) ;
#37272 = LINE ( 'NONE', #8460, #22285 ) ;
#37273 = AXIS2_PLACEMENT_3D ( 'NONE', #50878, #7371, #15745 ) ;
#37274 = CARTESIAN_POINT ( 'NONE',  ( 24.06642615182659739, -13.36711294005660022, -49.41972697186898955 ) ) ;
#37275 = ORIENTED_EDGE ( 'NONE', *, *, #19142, .T. ) ;
#37276 = CARTESIAN_POINT ( 'NONE',  ( 53.78531600184879835, -48.57334919407480101, -26.63319078974290122 ) ) ;
#37277 = AXIS2_PLACEMENT_3D ( 'NONE', #50225, #14314, #30283 ) ;
#37278 = CARTESIAN_POINT ( 'NONE',  ( 54.71118390020190247, -51.11900467049459706, -75.31578149455251037 ) ) ;
#37279 = CARTESIAN_POINT ( 'NONE',  ( 10.61758738775479927, 33.59332580352769781, -18.17420787144230232 ) ) ;
#37281 = EDGE_CURVE ( 'NONE', #33328, #16351, #40622, .T. ) ;
#37280 = DIRECTION ( 'NONE',  ( 0.000000000000000000, 1.000000000000000000, 0.000000000000000000 ) ) ;
#37282 = CARTESIAN_POINT ( 'NONE',  ( -21.36606260230379917, 21.88381105532059934, 17.35000000000000142 ) ) ;
#37283 = ORIENTED_EDGE ( 'NONE', *, *, #45508, .F. ) ;
#37284 = CARTESIAN_POINT ( 'NONE',  ( -5.654166889186940992, -46.79365041531399783, -4.894927202041920111 ) ) ;
#37285 = CARTESIAN_POINT ( 'NONE',  ( 47.34904504271399617, 23.45336456905550193, -54.69724835834480103 ) ) ;
#37286 = CARTESIAN_POINT ( 'NONE',  ( 22.16915665782660128, 22.83973475445539947, -34.88336916441289759 ) ) ;
#37287 = CARTESIAN_POINT ( 'NONE',  ( 63.41538649190439969, 1.369535599030029971, -62.52785204568030508 ) ) ;
#37288 = CARTESIAN_POINT ( 'NONE',  ( 68.13393739769745139, -49.21324915460503036, -70.54648330188274485 ) ) ;
#37289 = CARTESIAN_POINT ( 'NONE',  ( 11.69717481575709961, 34.15430575971510052, -17.57872672726050212 ) ) ;
#37290 = DIRECTION ( 'NONE',  ( 1.000000000000000000, 0.000000000000000000, 0.000000000000000000 ) ) ;
#37291 = CARTESIAN_POINT ( 'NONE',  ( 46.63393739769619373, -36.11618894467930119, -34.64999999999999858 ) ) ;
#37292 = DIRECTION ( 'NONE',  ( 0.000000000000000000, 0.000000000000000000, 1.000000000000000000 ) ) ;
#37293 = AXIS2_PLACEMENT_3D ( 'NONE', #10656, #50740, #35526 ) ;
#37294 = CARTESIAN_POINT ( 'NONE',  ( 57.55922429997960421, -47.27898653534939655, -48.12542328384540724 ) ) ;
#37295 = CARTESIAN_POINT ( 'NONE',  ( 53.11476273806689363, 18.18247392671170104, -27.56271911843160183 ) ) ;
#37296 = CARTESIAN_POINT ( 'NONE',  ( 55.69529708736050111, 19.85053035562459911, -53.59729798802170109 ) ) ;
#37297 = CARTESIAN_POINT ( 'NONE',  ( 63.66395377270059441, 1.424118951467219896, -69.15359763556290318 ) ) ;
#37298 = CARTESIAN_POINT ( 'NONE',  ( 22.72481188910181515, -13.84494795670818057, -48.36948871484188572 ) ) ;
#37299 = ORIENTED_EDGE ( 'NONE', *, *, #40978, .T. ) ;
#37300 = CARTESIAN_POINT ( 'NONE',  ( 34.00893739769620083, -11.50256827670329862, -35.14999999999999858 ) ) ;
#37301 = CARTESIAN_POINT ( 'NONE',  ( 8.977322698627309805, 32.04338259973479808, -46.63353404011659364 ) ) ;
#37302 = CARTESIAN_POINT ( 'NONE',  ( 16.13393739769620083, -1.759782484128330049, -47.64999999999999858 ) ) ;
#37303 = AXIS2_PLACEMENT_3D ( 'NONE', #16470, #49239, #24308 ) ;
#37304 = CARTESIAN_POINT ( 'NONE',  ( 66.66721609728190856, -29.91978853676059913, -17.00551245635359976 ) ) ;
#37305 = CARTESIAN_POINT ( 'NONE',  ( 18.26164351804030161, 20.66741474030959935, -75.53710645103448940 ) ) ;
#37306 = ORIENTED_EDGE ( 'NONE', *, *, #46055, .T. ) ;
#37307 = ORIENTED_EDGE ( 'NONE', *, *, #16594, .F. ) ;
#37308 = DIRECTION ( 'NONE',  ( 0.2260571801428161443, -1.387778780781444751E-17, -0.9741140340359945027 ) ) ;
#37309 = ORIENTED_EDGE ( 'NONE', *, *, #48044, .T. ) ;
#37310 = CARTESIAN_POINT ( 'NONE',  ( 10.40650514412410033, -63.80199668435589189, -45.90516490080199929 ) ) ;
#37311 = CARTESIAN_POINT ( 'NONE',  ( 57.21078602787749645, -45.77107311845719551, -26.23711395555770309 ) ) ;
#37312 = CARTESIAN_POINT ( 'NONE',  ( 20.27230028841029963, -21.17689101966990251, -81.23899999999999011 ) ) ;
#37313 = CARTESIAN_POINT ( 'NONE',  ( 61.34620581403849826, 14.06250526994010031, -47.14190415927130573 ) ) ;
#37314 = CARTESIAN_POINT ( 'NONE',  ( 64.12726891144080810, 1.458412159422780130, -61.50690654180700534 ) ) ;
#37315 = ORIENTED_EDGE ( 'NONE', *, *, #33711, .F. ) ;
#37316 = DIRECTION ( 'NONE',  ( -1.000000000000000000, 0.000000000000000000, 0.000000000000000000 ) ) ;
#37317 = AXIS2_PLACEMENT_3D ( 'NONE', #41724, #5831, #37802 ) ;
#37318 = ORIENTED_EDGE ( 'NONE', *, *, #34664, .T. ) ;
#37319 = CARTESIAN_POINT ( 'NONE',  ( 47.04983409348690060, -45.11618894461270202, -8.541664432791959527 ) ) ;
#37320 = TOROIDAL_SURFACE ( 'NONE', #39825, 17.69999999999999929, 3.799999999999830180 ) ;
#37321 = ADVANCED_FACE ( 'NONE', ( #778 ), #16778, .T. ) ;
#37322 = CARTESIAN_POINT ( 'NONE',  ( 20.63393739769599833, 10.38381105532070059, -35.14999999999999858 ) ) ;
#37323 = DIRECTION ( 'NONE',  ( -0.1686178020941670463, 0.6660492713794461395, 0.7265992051412121233 ) ) ;
#37324 = EDGE_LOOP ( 'NONE', ( #47768, #996, #38432, #14812 ) ) ;
#37325 = ADVANCED_FACE ( 'NONE', ( #49280 ), #39785, .F. ) ;
#37326 = CARTESIAN_POINT ( 'NONE',  ( 73.13559359734860266, 0.8904513541338849869, -68.96413986139360475 ) ) ;
#37327 = CARTESIAN_POINT ( 'NONE',  ( 46.40189200261440305, -53.01982478580160318, -76.14999999999999147 ) ) ;
#37328 = CARTESIAN_POINT ( 'NONE',  ( 85.84022851002180232, 17.38381105532069881, -53.47585302082339354 ) ) ;
#37329 = EDGE_CURVE ( 'NONE', #16369, #40975, #10508, .T. ) ;
#37330 = CARTESIAN_POINT ( 'NONE',  ( 45.63703752229459809, 14.88915874026919894, -9.401572978158439398 ) ) ;
#37331 = CARTESIAN_POINT ( 'NONE',  ( 16.13393739769599833, 14.38381105532070059, -35.14999999999999858 ) ) ;
#37332 = DIRECTION ( 'NONE',  ( -0.1414213562373098920, 0.000000000000000000, -0.9899494936611664686 ) ) ;
#37334 = AXIS2_PLACEMENT_3D ( 'NONE', #9757, #21787, #34617 ) ;
#37333 = DIRECTION ( 'NONE',  ( 0.000000000000000000, 0.000000000000000000, -1.000000000000000000 ) ) ;
#37335 = EDGE_CURVE ( 'NONE', #27635, #2118, #45707, .T. ) ;
#37336 = CARTESIAN_POINT ( 'NONE',  ( 57.68156670551299925, 13.95962980738159942, -25.76772952340219902 ) ) ;
#37337 = CARTESIAN_POINT ( 'NONE',  ( 22.59532618109970059, -20.07008647076710162, -69.47961042150460287 ) ) ;
#37338 = EDGE_LOOP ( 'NONE', ( #44272, #33632, #40887, #15602, #48641 ) ) ;
#37339 = CARTESIAN_POINT ( 'NONE',  ( 58.49950606315620405, 15.48244237084779940, -47.77607446784710277 ) ) ;
#37340 = CARTESIAN_POINT ( 'NONE',  ( -11.08689484260690072, -41.65128607374619918, -5.028175088695070016 ) ) ;
#37341 = CARTESIAN_POINT ( 'NONE',  ( 75.67253118882268836, -42.26411609651090373, -13.31112060773330086 ) ) ;
#37343 = EDGE_CURVE ( 'NONE', #35847, #31353, #42964, .T. ) ;
#37342 = CARTESIAN_POINT ( 'NONE',  ( 72.74974170911090710, 1.318402576460560027, -69.23505850801080896 ) ) ;
#37344 = B_SPLINE_CURVE_WITH_KNOTS ( 'NONE', 3,
 ( #4528, #20500, #51722, #16582, #345, #35739, #35985, #12672, #12154, #7447, #3520, #16331, #32285, #8216, #51471, #15570, #16074, #11640 ),
 .UNSPECIFIED., .F., .F.,
 ( 4, 2, 2, 2, 2, 2, 2, 2, 4 ),
 ( 0.5000009992646622381, 0.5625008743565794722, 0.6250007494484968174, 0.6875006245404140515, 0.7500004996323312856, 0.8125003747242485197, 0.8750002498161656428, 0.9375001249080827659, 1.000000000000000000 ),
 .UNSPECIFIED. ) ;
#37345 = CARTESIAN_POINT ( 'NONE',  ( 12.26282170032640195, -64.61533680211610431, -15.83707920938230096 ) ) ;
#37346 = AXIS2_PLACEMENT_3D ( 'NONE', #6477, #38972, #15113 ) ;
#37347 = CARTESIAN_POINT ( 'NONE',  ( 82.35524870416759313, -45.10829932330300096, -46.40105680372339947 ) ) ;
#37348 = CARTESIAN_POINT ( 'NONE',  ( 9.366929721696807931, -16.50193097571266421, -79.41115341879661571 ) ) ;
#37349 = CARTESIAN_POINT ( 'NONE',  ( 48.99827939567540369, -53.83769105205929861, -54.60353251326420576 ) ) ;
#37350 = CARTESIAN_POINT ( 'NONE',  ( 24.04426633253695655, -15.72747050290504056, -33.51214286250507257 ) ) ;
#37351 = CARTESIAN_POINT ( 'NONE',  ( -3.429778956281600344, -15.61618894467929763, 7.849999999999999645 ) ) ;
#37352 = ORIENTED_EDGE ( 'NONE', *, *, #44738, .F. ) ;
#37353 = CARTESIAN_POINT ( 'NONE',  ( 18.30701343718470042, -22.74250881295229831, -39.47312943893279424 ) ) ;
#37354 = CARTESIAN_POINT ( 'NONE',  ( 64.36068579096159681, 0.9644290104359679594, -60.98409269229880181 ) ) ;
#37355 = ORIENTED_EDGE ( 'NONE', *, *, #408, .F. ) ;
#37356 = CARTESIAN_POINT ( 'NONE',  ( 16.13393739769620083, -15.61618894467929941, -6.721843382729280059 ) ) ;
#37357 = CARTESIAN_POINT ( 'NONE',  ( 60.87196862875009629, -45.65759271181720180, -47.67694403705610284 ) ) ;
#37358 = CYLINDRICAL_SURFACE ( 'NONE', #42123, 7.910999999999997812 ) ;
#37359 = CARTESIAN_POINT ( 'NONE',  ( 50.77827180918709615, 19.51522592562140090, -76.14999999999999147 ) ) ;
#37361 = DIRECTION ( 'NONE',  ( 0.000000000000000000, 0.000000000000000000, -1.000000000000000000 ) ) ;
#37360 = CARTESIAN_POINT ( 'NONE',  ( 44.34565080150579064, 8.750017722592588143, -64.98493568350201599 ) ) ;
#37362 = EDGE_CURVE ( 'NONE', #1900, #8620, #23011, .T. ) ;
#37363 = CARTESIAN_POINT ( 'NONE',  ( 52.71259601604019451, -51.43286903184419856, -75.79898490202970152 ) ) ;
#37364 = ORIENTED_EDGE ( 'NONE', *, *, #32524, .F. ) ;
#37365 = VECTOR ( 'NONE', #42832, 1000.000000000000000 ) ;
#37366 = VERTEX_POINT ( 'NONE', #22754 ) ;
#37367 = ORIENTED_EDGE ( 'NONE', *, *, #40516, .T. ) ;
#37368 = AXIS2_PLACEMENT_3D ( 'NONE', #36292, #12730, #13512 ) ;
#37369 = ORIENTED_EDGE ( 'NONE', *, *, #7474, .F. ) ;
#37370 = CARTESIAN_POINT ( 'NONE',  ( 61.61573738770560027, -45.13429482264220383, -46.61624098993680576 ) ) ;
#37371 = CARTESIAN_POINT ( 'NONE',  ( 24.04527307164895333, -15.61618901697373119, -57.79233174308600951 ) ) ;
#37372 = DIRECTION ( 'NONE',  ( 0.7071067811865510144, 0.000000000000000000, 0.7071067811865441310 ) ) ;
#37373 = AXIS2_PLACEMENT_3D ( 'NONE', #33524, #21978, #25650 ) ;
#37374 = ORIENTED_EDGE ( 'NONE', *, *, #14014, .T. ) ;
#37375 = ORIENTED_EDGE ( 'NONE', *, *, #36349, .F. ) ;
#37376 = ORIENTED_EDGE ( 'NONE', *, *, #34757, .F. ) ;
#37377 = CARTESIAN_POINT ( 'NONE',  ( 22.89142707005135691, -16.00359460448838789, -72.47105089344913154 ) ) ;
#37378 = CARTESIAN_POINT ( 'NONE',  ( 10.68011837214288029, -11.14422995437498543, -46.06579460775301271 ) ) ;
#37379 = DIRECTION ( 'NONE',  ( 0.000000000000000000, 0.000000000000000000, 1.000000000000000000 ) ) ;
#37380 = CARTESIAN_POINT ( 'NONE',  ( 22.90108808520262329, -15.61618901356150069, -52.45282226904397049 ) ) ;
#37381 = DIRECTION ( 'NONE',  ( 0.000000000000000000, -1.000000000000000000, 0.000000000000000000 ) ) ;
#37382 = VERTEX_POINT ( 'NONE', #7060 ) ;
#37383 = DIRECTION ( 'NONE',  ( -0.5516667872527503125, 0.8340645993220362486, -1.942890293094025918E-16 ) ) ;
#37384 = CARTESIAN_POINT ( 'NONE',  ( 52.61122377792880656, -50.99960881131569579, -76.13271377727109268 ) ) ;
#37385 = CARTESIAN_POINT ( 'NONE',  ( 38.67452568954060155, -15.61618894467929941, -81.65000000000000568 ) ) ;
#37386 = CARTESIAN_POINT ( 'NONE',  ( 83.91174613997148413, -44.80490681739117065, -47.46626505639375182 ) ) ;
#37387 = CIRCLE ( 'NONE', #30677, 1.999999999999997113 ) ;
#37388 = EDGE_CURVE ( 'NONE', #51495, #40473, #9945, .T. ) ;
#37389 = CARTESIAN_POINT ( 'NONE',  ( 8.927887674289250342, -18.72417784031090093, -66.88287958694499480 ) ) ;
#37390 = VECTOR ( 'NONE', #47874, 1000.000000000000000 ) ;
#37391 = CARTESIAN_POINT ( 'NONE',  ( 8.645706001916069638, 17.52774233096719669, -35.08633291502819418 ) ) ;
#37392 = CARTESIAN_POINT ( 'NONE',  ( 45.86660482663089766, 13.88490149991019962, -7.634519155851280381 ) ) ;
#37393 = CARTESIAN_POINT ( 'NONE',  ( 42.34652498500450690, -44.08694099878920269, -4.929786139639760201 ) ) ;
#37394 = CARTESIAN_POINT ( 'NONE',  ( 72.43519100933379207, 1.033013263524900083, -61.46596897695270201 ) ) ;
#37395 = CARTESIAN_POINT ( 'NONE',  ( -11.32734370190460105, 10.64934056395049922, -6.430192534648650593 ) ) ;
#37396 = CARTESIAN_POINT ( 'NONE',  ( 64.31741031388310148, 1.334515466074710055, -70.11420104233359041 ) ) ;
#37397 = CARTESIAN_POINT ( 'NONE',  ( 46.85203200633210230, 8.412936757578801661, -54.34706384622469244 ) ) ;
#37398 = CARTESIAN_POINT ( 'NONE',  ( 66.87130723771809926, 0.3340111767280660171, -17.65465185469040321 ) ) ;
#37399 = VERTEX_POINT ( 'NONE', #39031 ) ;
#37400 = CARTESIAN_POINT ( 'NONE',  ( 14.35743399087829886, -51.90926368007729508, -75.71157996061791096 ) ) ;
#37401 = B_SPLINE_CURVE_WITH_KNOTS ( 'NONE', 3,
 ( #1751, #26880, #6984, #10918, #6468, #42891, #22683, #22938 ),
 .UNSPECIFIED., .F., .F.,
 ( 4, 2, 2, 4 ),
 ( 0.4999999271596042849, 0.6249999999961461938, 0.8117231960810037394, 1.000000000000000000 ),
 .UNSPECIFIED. ) ;
#37402 = CARTESIAN_POINT ( 'NONE',  ( 47.21725345290060005, -54.78032235606750078, -54.61943838409560215 ) ) ;
#37403 = CARTESIAN_POINT ( 'NONE',  ( 46.30117189897522678, -40.10998932786493043, -55.49701588496500904 ) ) ;
#37404 = CARTESIAN_POINT ( 'NONE',  ( 30.13393739769619728, 7.383811055320659733, -72.14999999999999147 ) ) ;
#37405 = CIRCLE ( 'NONE', #34892, 32.00000000000000000 ) ;
#37406 = CARTESIAN_POINT ( 'NONE',  ( 23.09136781754329704, -18.42403774965039887, -32.14999999999999858 ) ) ;
#37407 = CARTESIAN_POINT ( 'NONE',  ( 14.34417029198830029, 20.88381105532299742, -23.15000000000000213 ) ) ;
#37408 = CARTESIAN_POINT ( 'NONE',  ( 11.78673863893369855, 34.19465826557939891, -17.91922926160039964 ) ) ;
#37410 = CARTESIAN_POINT ( 'NONE',  ( 23.04646567172652993, -19.60031090604470094, -51.95899602180234211 ) ) ;
#37409 = CARTESIAN_POINT ( 'NONE',  ( 14.29774505407299934, 19.88381105532299742, -22.54670831509739770 ) ) ;
#37411 = CARTESIAN_POINT ( 'NONE',  ( 48.19603879950989977, 23.00596188178739965, -54.83412089522879285 ) ) ;
#37412 = ORIENTED_EDGE ( 'NONE', *, *, #44721, .T. ) ;
#37413 = CARTESIAN_POINT ( 'NONE',  ( 22.75640274483500036, -18.04219634376060100, -60.95895364771359226 ) ) ;
#37414 = ORIENTED_EDGE ( 'NONE', *, *, #35627, .F. ) ;
#37415 = DIRECTION ( 'NONE',  ( -0.2260571801428161165, -2.775557561562891043E-17, 0.9741140340359943917 ) ) ;
#37416 = AXIS2_PLACEMENT_3D ( 'NONE', #30518, #3017, #22907 ) ;
#37417 = CARTESIAN_POINT ( 'NONE',  ( 53.59007904684525414, -49.40624020596621335, -49.22506784124646373 ) ) ;
#37418 = CARTESIAN_POINT ( 'NONE',  ( 14.02678725144350302, 19.07322791160352793, -20.88317649143827381 ) ) ;
#37420 = CARTESIAN_POINT ( 'NONE',  ( 54.11082558918479890, 16.90719386950179626, -26.08329795554909936 ) ) ;
#37419 = CARTESIAN_POINT ( 'NONE',  ( 84.22529662124048855, 12.91617031814629968, -47.36165834067109870 ) ) ;
#37421 = ADVANCED_FACE ( 'NONE', ( #6534 ), #29840, .T. ) ;
#37422 = CARTESIAN_POINT ( 'NONE',  ( 23.06275954296619801, -16.93299659040459915, -76.51260139562678830 ) ) ;
#37423 = CARTESIAN_POINT ( 'NONE',  ( 11.47551314107553289, 33.73997922480182154, -16.61573023121771087 ) ) ;
#37424 = CARTESIAN_POINT ( 'NONE',  ( 56.43578946174220334, -45.13008420189939329, -15.60617155886200003 ) ) ;
#37425 = DIRECTION ( 'NONE',  ( 0.000000000000000000, 0.000000000000000000, -1.000000000000000000 ) ) ;
#37426 = ADVANCED_FACE ( 'NONE', ( #49789 ), #34798, .F. ) ;
#37427 = ORIENTED_EDGE ( 'NONE', *, *, #9310, .F. ) ;
#37428 = ORIENTED_EDGE ( 'NONE', *, *, #14135, .F. ) ;
#37429 = ADVANCED_FACE ( 'NONE', ( #34557 ), #37320, .F. ) ;
#37430 = CARTESIAN_POINT ( 'NONE',  ( 11.68991505667689879, -64.90566085822540288, -16.36861125146140239 ) ) ;
#37431 = CARTESIAN_POINT ( 'NONE',  ( 11.83096648206709922, 33.93729815101410452, -46.65733685557199806 ) ) ;
#37432 = DIRECTION ( 'NONE',  ( 0.000000000000000000, 0.000000000000000000, 1.000000000000000000 ) ) ;
#37433 = CARTESIAN_POINT ( 'NONE',  ( 16.13393739769620083, -45.61618894467940066, -35.14999999999999858 ) ) ;
#37434 = DIRECTION ( 'NONE',  ( 0.06538141124691357331, -0.04750237581189067221, -0.9967290481146758863 ) ) ;
#37435 = ORIENTED_EDGE ( 'NONE', *, *, #14498, .T. ) ;
#37436 = CARTESIAN_POINT ( 'NONE',  ( -20.70080641011480083, -28.63484290321709835, -52.76718538126279867 ) ) ;
#37437 = DIRECTION ( 'NONE',  ( 1.000000000000000000, 0.000000000000000000, 0.000000000000000000 ) ) ;
#37438 = CARTESIAN_POINT ( 'NONE',  ( 20.99561100367103350, -21.94235771815155900, -59.79935458015073380 ) ) ;
#37439 = CARTESIAN_POINT ( 'NONE',  ( 62.50437461550328777, -1.750381705555160261, -16.13137864070830219 ) ) ;
#37440 = CARTESIAN_POINT ( 'NONE',  ( 50.65831133345510295, -49.27121936819580839, -76.22116164247820791 ) ) ;
#37441 = CARTESIAN_POINT ( 'NONE',  ( 11.27225585075783343, -21.94235148362552579, -44.21602647793709195 ) ) ;
#37442 =( BOUNDED_CURVE ( )  B_SPLINE_CURVE ( 3, ( #37260, #9493, #29635, #33824 ),
 .UNSPECIFIED., .F., .T. ) 
 B_SPLINE_CURVE_WITH_KNOTS ( ( 4, 4 ),
 ( 2.356194490192361712, 3.141592653589784234 ),
 .UNSPECIFIED. ) 
 CURVE ( )  GEOMETRIC_REPRESENTATION_ITEM ( )  RATIONAL_B_SPLINE_CURVE ( ( 1.000000000000000000, 0.9492530216741945637, 0.9492530216741945637, 1.000000000000000000 ) ) 
 REPRESENTATION_ITEM ( '' )  );
#37443 = VERTEX_POINT ( 'NONE', #50560 ) ;
#37444 = CARTESIAN_POINT ( 'NONE',  ( 53.09137791023449893, -49.29352759859440170, -26.91462423334489884 ) ) ;
#37445 = CARTESIAN_POINT ( 'NONE',  ( 20.63393739769599833, 10.38381105532070059, -35.14999999999999858 ) ) ;
#37446 = EDGE_LOOP ( 'NONE', ( #44147, #29345, #4543, #15646 ) ) ;
#37447 = CARTESIAN_POINT ( 'NONE',  ( 9.661801442696654973, -10.91390692633954451, -47.64999999999999858 ) ) ;
#37448 = CARTESIAN_POINT ( 'NONE',  ( 24.75751086271734280, -18.45471230805310370, -34.79644660940672907 ) ) ;
#37449 = ADVANCED_FACE ( 'NONE', ( #34291 ), #1333, .F. ) ;
#37450 = CARTESIAN_POINT ( 'NONE',  ( 12.28771955365369983, -22.90926077143079809, -80.44681068936390034 ) ) ;
#37451 = CARTESIAN_POINT ( 'NONE',  ( 13.93867182927249893, -51.20113036054549838, -22.80125035677469825 ) ) ;
#37452 = CARTESIAN_POINT ( 'NONE',  ( 55.04746246912909413, 19.47632002275969754, -75.94217828162659600 ) ) ;
#37453 = CARTESIAN_POINT ( 'NONE',  ( 47.14495913819240513, -54.17197317070149865, -75.51614565244940991 ) ) ;
#37454 = ORIENTED_EDGE ( 'NONE', *, *, #22407, .F. ) ;
#37455 = CARTESIAN_POINT ( 'NONE',  ( 55.27717382112350464, 14.24043577392810001, -15.58341969604579802 ) ) ;
#37456 = CARTESIAN_POINT ( 'NONE',  ( 57.22241558393270111, -50.57952226092219661, -53.44445692378550206 ) ) ;
#37457 = AXIS2_PLACEMENT_3D ( 'NONE', #40175, #40947, #4270 ) ;
#37458 = CARTESIAN_POINT ( 'NONE',  ( 9.093524979847760648, -15.19767719791919980, -33.86607922395559456 ) ) ;
#37459 = LINE ( 'NONE', #25643, #36874 ) ;
#37460 = EDGE_LOOP ( 'NONE', ( #38056, #51446, #3134, #28326 ) ) ;
#37461 = CARTESIAN_POINT ( 'NONE',  ( 47.21824388184999322, 23.05645682666510154, -75.35584192875380438 ) ) ;
#37462 = AXIS2_PLACEMENT_3D ( 'NONE', #14743, #38335, #6892 ) ;
#37463 = CARTESIAN_POINT ( 'NONE',  ( 64.92520290936280958, 0.8850831926798630178, -60.57999765399179637 ) ) ;
#37464 = B_SPLINE_CURVE_WITH_KNOTS ( 'NONE', 3,
 ( #48380, #417, #12746, #12476, #44446, #8552, #20838, #17192, #24495, #4601, #20576, #16936, #13011, #36569 ),
 .UNSPECIFIED., .F., .F.,
 ( 4, 2, 2, 2, 2, 2, 4 ),
 ( 0.000000000000000000, 0.1519567928777398325, 0.3055814807050730719, 0.4015969105971532449, 0.5936277703813197526, 0.9008771460359852323, 1.000000000000000000 ),
 .UNSPECIFIED. ) ;
#37465 = CARTESIAN_POINT ( 'NONE',  ( 37.13393739769620083, -49.46974233527257780, -34.79644660940672907 ) ) ;
#37466 = DIRECTION ( 'NONE',  ( -0.6643794812577336062, 0.7473954140103516997, 0.000000000000000000 ) ) ;
#37467 = CARTESIAN_POINT ( 'NONE',  ( 9.831796340808351076, -10.29963566149569942, -78.73073146540821199 ) ) ;
#37468 = B_SPLINE_CURVE_WITH_KNOTS ( 'NONE', 3,
 ( #4000, #12124, #19961, #35956, #32003, #36209, #48023, #28080, #44085, #1094 ),
 .UNSPECIFIED., .F., .F.,
 ( 4, 2, 2, 2, 4 ),
 ( -0.0004281134595752249749, 0.000000000000000000, 0.02012916873231600234, 0.03942875605144609968, 0.05028014561772611163 ),
 .UNSPECIFIED. ) ;
#37469 = FACE_OUTER_BOUND ( 'NONE', #8958, .T. ) ;
#37470 = CARTESIAN_POINT ( 'NONE',  ( 73.26121012496899709, 0.9212109678634080590, -68.76625967790960203 ) ) ;
#37472 = CARTESIAN_POINT ( 'NONE',  ( 47.18509805015050063, -39.34325223768411917, -54.67923127845079279 ) ) ;
#37471 = DIRECTION ( 'NONE',  ( 0.000000000000000000, 0.000000000000000000, -1.000000000000000000 ) ) ;
#37473 = CARTESIAN_POINT ( 'NONE',  ( 61.28346094977100478, 13.99940985045950015, -46.43278510584719498 ) ) ;
#37474 = DIRECTION ( 'NONE',  ( -0.5765530599821108160, 0.1342272854595029929, -0.8059588108975778153 ) ) ;
#37475 = CARTESIAN_POINT ( 'NONE',  ( -32.94143001319760344, -20.36928658016449845, -56.02216466475820056 ) ) ;
#37476 = EDGE_LOOP ( 'NONE', ( #5617, #46847, #39442, #31029 ) ) ;
#37477 = CARTESIAN_POINT ( 'NONE',  ( 52.91697748939440515, -49.61738182755579629, -48.80601310497799261 ) ) ;
#37478 = VERTEX_POINT ( 'NONE', #25908 ) ;
#37479 = CARTESIAN_POINT ( 'NONE',  ( 58.69147808494039964, -45.17395921270860271, -25.95218655891679660 ) ) ;
#37480 = CARTESIAN_POINT ( 'NONE',  ( 24.04037527269505503, -15.90671900147433782, -65.80402047898783735 ) ) ;
#37481 = CARTESIAN_POINT ( 'NONE',  ( 57.51163818235249892, 13.96175988552229974, -25.74441108106429965 ) ) ;
#37482 = CARTESIAN_POINT ( 'NONE',  ( 9.602139829674678495, -12.95570267495170036, -33.57594075914519749 ) ) ;
#37483 = CARTESIAN_POINT ( 'NONE',  ( 50.20000624151339963, 18.43678156217390196, -76.14999999999999147 ) ) ;
#37484 = CARTESIAN_POINT ( 'NONE',  ( 52.77791158333219812, 18.46457420104869840, -48.73086690438350388 ) ) ;
#37485 = CARTESIAN_POINT ( 'NONE',  ( 8.428876690002429228, -17.68701148082665497, -58.42433507561374029 ) ) ;
#37486 = CARTESIAN_POINT ( 'NONE',  ( 67.42785983160000285, -44.32276271297559589, -11.41916062409890031 ) ) ;
#37487 = EDGE_CURVE ( 'NONE', #15006, #30985, #28092, .T. ) ;
#37488 = ORIENTED_EDGE ( 'NONE', *, *, #836, .T. ) ;
#37489 = CARTESIAN_POINT ( 'NONE',  ( 12.39356905812690179, -22.05950633734969912, -69.73476110523529314 ) ) ;
#37490 = ADVANCED_FACE ( 'NONE', ( #30874 ), #26955, .T. ) ;
#37491 = CARTESIAN_POINT ( 'NONE',  ( 72.74776047649530142, 1.391252479931859964, -68.77264296518760034 ) ) ;
#37492 = CARTESIAN_POINT ( 'NONE',  ( 47.44225467880999503, -54.63206288700619950, -54.85722679016069492 ) ) ;
#37493 = CARTESIAN_POINT ( 'NONE',  ( 47.13393739769619373, -15.61618894467929941, -15.65000000000000036 ) ) ;
#37494 = CARTESIAN_POINT ( 'NONE',  ( 72.87639502376930523, 1.370118064600909902, -62.58950125921369789 ) ) ;
#37495 = CARTESIAN_POINT ( 'NONE',  ( 11.41644049895860036, -65.35642350271008638, -18.17421237901670139 ) ) ;
#37496 = CARTESIAN_POINT ( 'NONE',  ( 53.00700879704349688, 18.33567502363469970, -48.78176283131570301 ) ) ;
#37497 = CARTESIAN_POINT ( 'NONE',  ( 14.04007584740629788, -23.31488602239420516, -76.37656314211675124 ) ) ;
#37498 = CARTESIAN_POINT ( 'NONE',  ( 71.74419295952090181, 1.145379646617759928, -60.90832955879639599 ) ) ;
#37499 = CIRCLE ( 'NONE', #25723, 0.5000000000814214252 ) ;
#37500 = CARTESIAN_POINT ( 'NONE',  ( 19.36791954131713922, -22.86483927959923435, -45.87411009050862987 ) ) ;
#37501 = CARTESIAN_POINT ( 'NONE',  ( 64.81394005445639550, 0.9259537755896120048, -70.64777040355440363 ) ) ;
#37502 = VERTEX_POINT ( 'NONE', #45859 ) ;
#37503 = CARTESIAN_POINT ( 'NONE',  ( 9.297749548753010629, -63.28389869551808999, -46.53031453602530121 ) ) ;
#37504 = CARTESIAN_POINT ( 'NONE',  ( 0.1457841021255935343, -50.71887597443840434, -34.68167779225149161 ) ) ;
#37505 = VERTEX_POINT ( 'NONE', #41921 ) ;
#37506 = CARTESIAN_POINT ( 'NONE',  ( 13.13393739769619906, -49.61618894467939356, -83.01107220193038927 ) ) ;
#37507 = CARTESIAN_POINT ( 'NONE',  ( 22.90090927591486292, -15.61618926791037687, -70.45281771081829447 ) ) ;
#37508 = CARTESIAN_POINT ( 'NONE',  ( 8.428870326585922612, -17.68698834907383599, -70.42433541781397821 ) ) ;
#37509 = CARTESIAN_POINT ( 'NONE',  ( 52.31626064796109432, 19.70647560332339765, -76.18456440489789827 ) ) ;
#37510 = EDGE_LOOP ( 'NONE', ( #28588, #4106, #32676, #12900 ) ) ;
#37511 = DIRECTION ( 'NONE',  ( 0.000000000000000000, 1.000000000000000000, 0.000000000000000000 ) ) ;
#37512 = CARTESIAN_POINT ( 'NONE',  ( 52.10267382257649871, 1.883811055284760005, -77.60820171200670359 ) ) ;
#37513 = CARTESIAN_POINT ( 'NONE',  ( 71.33393739769628894, 11.38381105532070059, -68.84999999999999432 ) ) ;
#37514 = EDGE_CURVE ( 'NONE', #18363, #44083, #26408, .T. ) ;
#37515 = CARTESIAN_POINT ( 'NONE',  ( 18.85737764037289921, -23.39857889253620016, -50.18517902306130196 ) ) ;
#37516 = DIRECTION ( 'NONE',  ( 0.000000000000000000, 0.000000000000000000, -1.000000000000000000 ) ) ;
#37517 = CARTESIAN_POINT ( 'NONE',  ( 44.41215812983547551, -37.97064865278709078, -68.25889606298196099 ) ) ;
#37518 = ADVANCED_FACE ( 'NONE', ( #34033 ), #41509, .F. ) ;
#37519 = ORIENTED_EDGE ( 'NONE', *, *, #11470, .F. ) ;
#37520 = CARTESIAN_POINT ( 'NONE',  ( 18.86789271212754215, 20.55440457922848907, -74.33587756536769575 ) ) ;
#37521 = CARTESIAN_POINT ( 'NONE',  ( 22.85349008618740285, -12.39837828030880118, -48.09049903432739370 ) ) ;
#37522 = CARTESIAN_POINT ( 'NONE',  ( 68.13393739769618662, -0.5161889446793590519, -65.65000000000000568 ) ) ;
#37523 = CARTESIAN_POINT ( 'NONE',  ( 14.06610822376199899, 20.17488022308399920, -75.08736963500949457 ) ) ;
#37524 = CARTESIAN_POINT ( 'NONE',  ( 38.67452568954060155, 6.328436186825659782, -81.65000000000000568 ) ) ;
#37525 = CARTESIAN_POINT ( 'NONE',  ( 41.46798912450119445, -44.88968489520180327, -5.587157704053289820 ) ) ;
#37526 = CARTESIAN_POINT ( 'NONE',  ( 82.63159810076149370, -45.06836083909839630, -46.43844420537259765 ) ) ;
#37527 = CARTESIAN_POINT ( 'NONE',  ( 23.73155033226879951, -12.41322181943569980, -53.38067352504989316 ) ) ;
#37528 = ORIENTED_EDGE ( 'NONE', *, *, #43839, .F. ) ;
#37529 = CARTESIAN_POINT ( 'NONE',  ( 53.88942171400410786, -48.39633017241650492, -26.28222357612559890 ) ) ;
#37530 = CARTESIAN_POINT ( 'NONE',  ( 55.19366304728959705, -51.02473303371100144, -75.15423526130980747 ) ) ;
#37531 = CARTESIAN_POINT ( 'NONE',  ( 9.433581914129849366, 30.61547584016309997, -13.45314291414399932 ) ) ;
#37532 = CARTESIAN_POINT ( 'NONE',  ( 16.13393739769620083, -15.61618894467929941, 6.349999999999999645 ) ) ;
#37533 = CARTESIAN_POINT ( 'NONE',  ( 14.34417029198879945, -52.11618894467930119, -74.14999999999999147 ) ) ;
#37534 = VERTEX_POINT ( 'NONE', #42181 ) ;
#37535 = CARTESIAN_POINT ( 'NONE',  ( -3.981438317303439778, -47.92280625716200149, -4.793466068732310070 ) ) ;
#37536 = CARTESIAN_POINT ( 'NONE',  ( 47.51972458776440078, 23.33356625217060198, -54.65851536377620334 ) ) ;
#37537 = DIRECTION ( 'NONE',  ( 0.000000000000000000, 0.000000000000000000, 1.000000000000000000 ) ) ;
#37538 = CARTESIAN_POINT ( 'NONE',  ( 63.43166809737898859, 1.369719003397489976, -62.48691920258249155 ) ) ;
#37539 = CARTESIAN_POINT ( 'NONE',  ( 68.13393739769620083, -42.11618894467930119, -65.65000000000000568 ) ) ;
#37540 = CARTESIAN_POINT ( 'NONE',  ( 10.91696762329730142, 33.77617350747969738, -17.52451613595910374 ) ) ;
#37541 = CARTESIAN_POINT ( 'NONE',  ( 21.06894106338335604, -12.03069890569523714, -8.849999999999999645 ) ) ;
#37542 = CARTESIAN_POINT ( 'NONE',  ( 68.13393739769810509, 19.38381105532030091, -71.50000000000198952 ) ) ;
#37543 = CARTESIAN_POINT ( 'NONE',  ( 8.222339619445261150, -15.61627490117209938, -70.79233150823699816 ) ) ;
#37544 = CARTESIAN_POINT ( 'NONE',  ( 38.67452568954060155, -36.11618894467930119, -81.65000000000000568 ) ) ;
#37545 = CARTESIAN_POINT ( 'NONE',  ( 52.82976477458089448, 18.42853897965050081, -28.09161879090800085 ) ) ;
#37546 = EDGE_CURVE ( 'NONE', #42649, #1811, #47353, .T. ) ;
#37547 = CARTESIAN_POINT ( 'NONE',  ( 52.85039779125390424, 21.08368931838860050, -54.40094741851120119 ) ) ;
#37548 = CARTESIAN_POINT ( 'NONE',  ( 63.73255073857669828, 1.426104593066200188, -69.34551121535889706 ) ) ;
#37549 = CARTESIAN_POINT ( 'NONE',  ( 22.04685654012394735, -12.20821177133414892, -48.28615521496443108 ) ) ;
#37550 = ORIENTED_EDGE ( 'NONE', *, *, #46377, .T. ) ;
#37551 = CARTESIAN_POINT ( 'NONE',  ( 9.494855085389646732, -17.51523721219662022, -73.75786096057412067 ) ) ;
#37552 = CARTESIAN_POINT ( 'NONE',  ( 9.737523894043130568, 31.98622279338489349, -46.29791410543919739 ) ) ;
#37553 = DIRECTION ( 'NONE',  ( -0.5000000000000003331, -0.8660254037844384856, 0.000000000000000000 ) ) ;
#37554 = CARTESIAN_POINT ( 'NONE',  ( 13.53484056975250027, -8.242504967360991586, -81.23899999999999011 ) ) ;
#37555 = CARTESIAN_POINT ( 'NONE',  ( 22.90118952179220813, -15.61618876469732875, -46.84717865327674247 ) ) ;
#37556 = B_SPLINE_CURVE_WITH_KNOTS ( 'NONE', 3,
 ( #18119, #49332, #21522, #37785, #25446, #45911, #5566, #41707, #37520, #6075 ),
 .UNSPECIFIED., .F., .F.,
 ( 4, 2, 2, 2, 4 ),
 ( 0.4999999271656643818, 0.5624999999903476100, 0.6624999999924280347, 0.8224999999957559593, 1.000000000000000000 ),
 .UNSPECIFIED. ) ;
#37557 = ORIENTED_EDGE ( 'NONE', *, *, #9758, .T. ) ;
#37558 = ORIENTED_EDGE ( 'NONE', *, *, #19416, .T. ) ;
#37559 = CARTESIAN_POINT ( 'NONE',  ( 15.01109173769490113, 12.72875286183729848, -62.64999999999999858 ) ) ;
#37560 = ORIENTED_EDGE ( 'NONE', *, *, #29160, .F. ) ;
#37561 = CARTESIAN_POINT ( 'NONE',  ( 12.46092453159049995, -65.42383766440380555, -47.10609709158759983 ) ) ;
#37562 = CARTESIAN_POINT ( 'NONE',  ( 56.74397420296469363, -45.46880684231319947, -25.88716263708979781 ) ) ;
#37563 = B_SPLINE_CURVE_WITH_KNOTS ( 'NONE', 3,
 ( #12473, #23210, #7777, #15382, #31335, #31849, #11458, #27415 ),
 .UNSPECIFIED., .F., .F.,
 ( 4, 2, 2, 4 ),
 ( 0.000000000000000000, 0.1749999999961678876, 0.3749999999917854598, 0.4999999271656643818 ),
 .UNSPECIFIED. ) ;
#37564 = CARTESIAN_POINT ( 'NONE',  ( 24.04343812156989912, -15.78374718670210264, -77.51440025672197009 ) ) ;
#37565 = CARTESIAN_POINT ( 'NONE',  ( 61.72743783710129861, 13.88647446954439957, -46.49120720414349961 ) ) ;
#37566 = CARTESIAN_POINT ( 'NONE',  ( 64.93393739769599904, 1.396834109478129804, -61.06337307536569625 ) ) ;
#37567 = ORIENTED_EDGE ( 'NONE', *, *, #7339, .F. ) ;
#37568 = CIRCLE ( 'NONE', #29180, 20.00000000000001421 ) ;
#37569 = CARTESIAN_POINT ( 'NONE',  ( 46.95981438746490966, 7.013759907145603378, -55.52059116220966928 ) ) ;
#37570 = ORIENTED_EDGE ( 'NONE', *, *, #5899, .T. ) ;
#37571 = CARTESIAN_POINT ( 'NONE',  ( 52.51556228498769485, -45.11618894460669793, -12.38233830838520078 ) ) ;
#37572 = CARTESIAN_POINT ( 'NONE',  ( 24.04465409553882083, -15.68853894113726710, -33.79524008575338456 ) ) ;
#37573 = AXIS2_PLACEMENT_3D ( 'NONE', #27674, #48376, #44443 ) ;
#37574 = EDGE_CURVE ( 'NONE', #18792, #46486, #34669, .T. ) ;
#37575 = CARTESIAN_POINT ( 'NONE',  ( 22.90065299155850198, -15.61618013372109637, -50.45281880338879432 ) ) ;
#37576 = ORIENTED_EDGE ( 'NONE', *, *, #39346, .F. ) ;
#37577 = CYLINDRICAL_SURFACE ( 'NONE', #40079, 0.4999999999999985012 ) ;
#37578 = CARTESIAN_POINT ( 'NONE',  ( 46.55184893656709733, -53.32569582049830359, -76.10173089639540933 ) ) ;
#37579 = CARTESIAN_POINT ( 'NONE',  ( 75.40667024492320536, 13.07356525956230087, -13.67454515778790025 ) ) ;
#37580 = CARTESIAN_POINT ( 'NONE',  ( 48.37121793235419887, 13.88381105532070059, -9.155085387312430711 ) ) ;
#37581 = DIRECTION ( 'NONE',  ( 0.000000000000000000, 0.000000000000000000, -1.000000000000000000 ) ) ;
#37582 = DIRECTION ( 'NONE',  ( 8.462868000000000073E-18, -1.066343000000000058E-17, 1.000000000000000000 ) ) ;
#37583 = CARTESIAN_POINT ( 'NONE',  ( 61.35827264627630484, 13.96263723663859935, -28.15113330384149748 ) ) ;
#37584 = CARTESIAN_POINT ( 'NONE',  ( 16.60947325484960047, -7.782887352646469914, -72.80680552617660339 ) ) ;
#37585 = ORIENTED_EDGE ( 'NONE', *, *, #21719, .T. ) ;
#37586 = DIRECTION ( 'NONE',  ( 0.7071067811865475727, 0.000000000000000000, -0.7071067811865475727 ) ) ;
#37587 = CARTESIAN_POINT ( 'NONE',  ( -9.664157262737310461, -43.13799255771849772, -5.051889323743290028 ) ) ;
#37588 = CARTESIAN_POINT ( 'NONE',  ( 75.47851028940139884, -43.42898794502159632, -13.41230162649550017 ) ) ;
#37589 = CARTESIAN_POINT ( 'NONE',  ( 72.79388427887360535, 1.241979851175039951, -69.28847831928310086 ) ) ;
#37590 = CIRCLE ( 'NONE', #24174, 3.569999999999939444 ) ;
#37591 = CIRCLE ( 'NONE', #48488, 38.00000000000000711 ) ;
#37592 = CARTESIAN_POINT ( 'NONE',  ( 14.13393739769599833, 14.38381105532070059, -62.64999999999999858 ) ) ;
#37593 = CARTESIAN_POINT ( 'NONE',  ( 72.33393739769479680, 10.88381105532070059, -68.85000000000388809 ) ) ;
#37594 = AXIS2_PLACEMENT_3D ( 'NONE', #48936, #20860, #36863 ) ;
#37595 = CARTESIAN_POINT ( 'NONE',  ( -30.36606260230379917, 21.88381105532059934, 10.84999999999999964 ) ) ;
#37596 = CARTESIAN_POINT ( 'NONE',  ( 49.15407994174589845, -53.83453679569459638, -54.78253050193919904 ) ) ;
#37597 = CARTESIAN_POINT ( 'NONE',  ( 51.17843651765708302, -31.65766843421481624, -17.12041166110326174 ) ) ;
#37598 = EDGE_CURVE ( 'NONE', #19762, #29825, #15553, .T. ) ;
#37599 = VECTOR ( 'NONE', #42529, 1000.000000000000000 ) ;
#37600 = DIRECTION ( 'NONE',  ( 0.000000000000000000, 0.000000000000000000, 1.000000000000000000 ) ) ;
#37601 = CARTESIAN_POINT ( 'NONE',  ( 18.30650362895240235, -51.22777015963880132, -74.58518005234699899 ) ) ;
#37602 = CARTESIAN_POINT ( 'NONE',  ( 56.27102381480889903, -50.57721995146319927, -52.87265154067429762 ) ) ;
#37603 = ORIENTED_EDGE ( 'NONE', *, *, #18469, .F. ) ;
#37604 = EDGE_CURVE ( 'NONE', #49951, #27673, #31499, .T. ) ;
#37605 = CARTESIAN_POINT ( 'NONE',  ( 23.41830238215899840, -14.05262854882809975, -55.00003992740209924 ) ) ;
#37606 = B_SPLINE_CURVE_WITH_KNOTS ( 'NONE', 3,
 ( #36163, #19919, #36946, #32725, #28035, #29, #16509, #272, #36673, #9177 ),
 .UNSPECIFIED., .F., .F.,
 ( 4, 2, 2, 2, 4 ),
 ( -5.773159999999999959E-14, 2.783242270592499956, 5.292080373661850246, 6.860104188080190291, 7.840119072091650487 ),
 .UNSPECIFIED. ) ;
#37607 = ADVANCED_FACE ( 'NONE', ( #47415 ), #39791, .T. ) ;
#37608 = CARTESIAN_POINT ( 'NONE',  ( 64.45847733817470271, 1.439519383694989996, -61.26834731818230040 ) ) ;
#37609 = ORIENTED_EDGE ( 'NONE', *, *, #37598, .F. ) ;
#37610 = DIRECTION ( 'NONE',  ( -1.000000000000000000, 0.000000000000000000, 0.000000000000000000 ) ) ;
#37611 = CARTESIAN_POINT ( 'NONE',  ( 61.24499251173579495, -45.54248517078090686, -47.60670208486399702 ) ) ;
#37612 = DIRECTION ( 'NONE',  ( -1.000000000000000000, 0.000000000000000000, 0.000000000000000000 ) ) ;
#37613 = CARTESIAN_POINT ( 'NONE',  ( 68.13393739771808555, -29.66618894549150909, -49.15000000170420691 ) ) ;
#37615 = CARTESIAN_POINT ( 'NONE',  ( 9.367363532653184777, -14.62080165624493766, -53.89401576057853305 ) ) ;
#37614 = CARTESIAN_POINT ( 'NONE',  ( 44.78558282010767044, 8.783042718080674049, -62.85233582178556588 ) ) ;
#37616 = ADVANCED_FACE ( 'NONE', ( #39279 ), #44839, .F. ) ;
#37617 = CARTESIAN_POINT ( 'NONE',  ( 50.96213132486371933, -50.95760513581273443, -76.15000000000004832 ) ) ;
#37618 = CARTESIAN_POINT ( 'NONE',  ( 42.00758945880200201, -45.79790383927660002, -6.830514409016920752 ) ) ;
#37619 = ORIENTED_EDGE ( 'NONE', *, *, #51008, .F. ) ;
#37620 = VERTEX_POINT ( 'NONE', #19094 ) ;
#37621 = EDGE_LOOP ( 'NONE', ( #48327, #8561, #23084 ) ) ;
#37622 = ORIENTED_EDGE ( 'NONE', *, *, #19032, .F. ) ;
#37623 = CARTESIAN_POINT ( 'NONE',  ( 61.11135448844899543, -45.32462824983760186, -46.90702640965010062 ) ) ;
#37624 = CARTESIAN_POINT ( 'NONE',  ( 53.05499567186660670, -49.60096502583370182, -49.11111871955459662 ) ) ;
#37625 = CARTESIAN_POINT ( 'NONE',  ( 61.28085239525059791, 14.36939662108470017, -47.67834120296360112 ) ) ;
#37626 = FACE_OUTER_BOUND ( 'NONE', #38754, .T. ) ;
#37627 = EDGE_CURVE ( 'NONE', #7528, #43147, #3629, .T. ) ;
#37628 = ORIENTED_EDGE ( 'NONE', *, *, #36546, .F. ) ;
#37629 = EDGE_LOOP ( 'NONE', ( #40828, #26932, #25353, #44281 ) ) ;
#37630 = CARTESIAN_POINT ( 'NONE',  ( 24.04493067738190959, -15.60426386090046869, -77.50719664004228093 ) ) ;
#37631 = AXIS2_PLACEMENT_3D ( 'NONE', #41850, #2020, #30554 ) ;
#37632 = CARTESIAN_POINT ( 'NONE',  ( 56.09651439476719759, -50.93334530694360041, -53.89358350665009567 ) ) ;
#37633 = EDGE_CURVE ( 'NONE', #44858, #32800, #7175, .T. ) ;
#37634 = DIRECTION ( 'NONE',  ( 0.000000000000000000, 0.000000000000000000, 1.000000000000000000 ) ) ;
#37635 = TOROIDAL_SURFACE ( 'NONE', #26742, 16.60961179679779676, 0.5000000000000000000 ) ;
#37636 = VECTOR ( 'NONE', #11226, 1000.000000000000000 ) ;
#37637 = ORIENTED_EDGE ( 'NONE', *, *, #11062, .F. ) ;
#37638 = CARTESIAN_POINT ( 'NONE',  ( 0.3198710486850210311, -46.24968915917909840, -34.64999999999999858 ) ) ;
#37639 = CARTESIAN_POINT ( 'NONE',  ( 51.99242832958879745, -50.02583382361060416, -76.70333696065139861 ) ) ;
#37640 = VECTOR ( 'NONE', #26751, 1000.000000000000114 ) ;
#37641 = CARTESIAN_POINT ( 'NONE',  ( 14.17038268164659875, -32.57607267493840197, -34.95504743437659556 ) ) ;
#37642 = AXIS2_PLACEMENT_3D ( 'NONE', #46267, #29723, #5897 ) ;
#37643 = CARTESIAN_POINT ( 'NONE',  ( 18.13911242106300037, -8.028961472324999349, -59.59473792909199830 ) ) ;
#37644 = DIRECTION ( 'NONE',  ( 1.000000000000000000, 0.000000000000000000, 0.000000000000000000 ) ) ;
#37645 = CARTESIAN_POINT ( 'NONE',  ( 45.83940546124159710, 13.90408673295529773, -7.873659366785940250 ) ) ;
#37646 = CARTESIAN_POINT ( 'NONE',  ( 42.42176421416689891, -44.20760043642759740, -5.045468647411699870 ) ) ;
#37647 = CARTESIAN_POINT ( 'NONE',  ( 68.13393739769847457, -50.70395984888145335, -72.15645085170113759 ) ) ;
#37648 = CARTESIAN_POINT ( 'NONE',  ( 56.23669252666629603, 14.33142556199779882, -25.29918085107650327 ) ) ;
#37649 = EDGE_CURVE ( 'NONE', #19842, #25873, #16472, .T. ) ;
#37650 = CARTESIAN_POINT ( 'NONE',  ( 63.97355303201310051, 1.199411168077020085, -69.93688014721760737 ) ) ;
#37651 = FACE_OUTER_BOUND ( 'NONE', #45743, .T. ) ;
#37652 = CARTESIAN_POINT ( 'NONE',  ( 66.95999988526210700, 1.459641452089809999, -18.94776480168570032 ) ) ;
#37653 = ORIENTED_EDGE ( 'NONE', *, *, #32368, .F. ) ;
#37654 = CARTESIAN_POINT ( 'NONE',  ( 14.92989387051190064, -52.97186080988799972, -76.14999999999999147 ) ) ;
#37655 = CARTESIAN_POINT ( 'NONE',  ( 57.36404682476049999, 18.93586243731099827, -52.65764136420510511 ) ) ;
#37656 = B_SPLINE_CURVE_WITH_KNOTS ( 'NONE', 3,
 ( #27766, #11028, #7863, #51372, #23811, #39830, #31936, #26996, #15471, #11544, #39071, #3162, #19132, #31422, #51111, #15214, #23558, #31169, #47450, #27506, #39573, #3679, #35642, #4177, #20153, #36390, #248, #36146 ),
 .UNSPECIFIED., .F., .F.,
 ( 4, 2, 2, 2, 2, 2, 2, 2, 2, 2, 1, 1, 1, 1, 2, 4 ),
 ( 0.000000000000000000, 0.06250045316978908305, 0.1250009063395781661, 0.1875013595093672769, 0.2500018126791563322, 0.3125022658489454153, 0.3750027190187345538, 0.4375031721885235814, 0.4687533987734182062, 0.4843785120658654630, 0.4921910687120890637, 0.4960973470352010306, 0.4980504861967569585, 0.4990270557775348670, 0.4995153405679237379, 0.5000036253583125534 ),
 .UNSPECIFIED. ) ;
#37657 = CARTESIAN_POINT ( 'NONE',  ( 4.133937397696209715, -8.687985714403829718, -47.64999999999999858 ) ) ;
#37658 = CARTESIAN_POINT ( 'NONE',  ( 39.88393739769619373, 30.88381105532059934, 16.35000000000000142 ) ) ;
#37659 = CARTESIAN_POINT ( 'NONE',  ( 23.02572387508500285, -13.73427156000250093, -32.14999999999999858 ) ) ;
#37660 = CARTESIAN_POINT ( 'NONE',  ( 11.77545672747359973, 34.19368150675510520, -17.95294975582580221 ) ) ;
#37661 = DIRECTION ( 'NONE',  ( -0.2260571801428140071, 0.000000000000000000, 0.9741140340359949468 ) ) ;
#37662 = DIRECTION ( 'NONE',  ( -1.000000000000000000, 0.000000000000000000, 0.000000000000000000 ) ) ;
#37663 = CARTESIAN_POINT ( 'NONE',  ( 48.37262564244719698, 22.87082288443439992, -54.65898693694939681 ) ) ;
#37664 = VECTOR ( 'NONE', #9861, 1000.000000000000114 ) ;
#37665 = ORIENTED_EDGE ( 'NONE', *, *, #37878, .T. ) ;
#37666 = AXIS2_PLACEMENT_3D ( 'NONE', #27053, #3479, #47759 ) ;
#37667 = CARTESIAN_POINT ( 'NONE',  ( 14.22831053668800116, -22.40670773495260093, -61.43426723409519496 ) ) ;
#37668 = EDGE_CURVE ( 'NONE', #14308, #43415, #51589, .T. ) ;
#37669 = EDGE_LOOP ( 'NONE', ( #27694, #50540, #23190, #4 ) ) ;
#37670 = VECTOR ( 'NONE', #24958, 1000.000000000000000 ) ;
#37671 = CARTESIAN_POINT ( 'NONE',  ( 82.46534785695916980, 13.86080115390507750, -46.44243061472944589 ) ) ;
#37672 = CARTESIAN_POINT ( 'NONE',  ( 19.13393739769620083, -49.61618894467939356, -35.14999999999999858 ) ) ;
#37673 = CARTESIAN_POINT ( 'NONE',  ( 22.72481288133749899, -17.38742503737659106, -42.53615302188016045 ) ) ;
#37675 = CARTESIAN_POINT ( 'NONE',  ( 55.85842059416459904, 14.74773178907929960, -25.34033418961709927 ) ) ;
#37674 = CARTESIAN_POINT ( 'NONE',  ( 84.17895764879889953, 12.85061017212530032, -47.20739533566359825 ) ) ;
#37676 = AXIS2_PLACEMENT_3D ( 'NONE', #26063, #30257, #42334 ) ;
#37677 = CARTESIAN_POINT ( 'NONE',  ( 18.80263846160409713, -9.087744005176290329, -72.07634125606418252 ) ) ;
#37678 = CIRCLE ( 'NONE', #49447, 6.999999999999999112 ) ;
#37680 = EDGE_CURVE ( 'NONE', #21370, #19900, #39055, .T. ) ;
#37679 = DIRECTION ( 'NONE',  ( 0.000000000000000000, -1.000000000000000000, 0.000000000000000000 ) ) ;
#37681 = CARTESIAN_POINT ( 'NONE',  ( 56.67234887970509760, -45.11618894467940066, -15.60614885759789949 ) ) ;
#37682 = FACE_OUTER_BOUND ( 'NONE', #14465, .T. ) ;
#37683 = B_SPLINE_SURFACE_WITH_KNOTS ( 'NONE', 3, 3, ( 
 ( #48925, #5157, #44713, #20585, #40523, #8563, #9078, #1210 ),
 ( #5408, #1469, #36845, #17203, #8820, #49185, #41041, #32371 ),
 ( #13278, #12756, #21366, #29232, #24771, #45239, #951, #49439 ),
 ( #40780, #9349, #37370, #683, #25294, #41299, #24504, #36579 ),
 ( #32891, #13023, #17458, #33423, #13537, #45500, #40271, #4359 ),
 ( #429, #16414, #14558, #14299, #30526, #46550, #6445, #42344 ),
 ( #42608, #41555, #34190, #18485, #26591, #10637, #21619, #45760 ),
 ( #5920, #6704, #46024, #10114, #18739, #26074, #22402, #1987 ),
 ( #25552, #22661, #21886, #50207, #38682, #2768, #37623, #30781 ),
 ( #38409, #34717, #50467, #49952, #2505, #50720, #14819, #9598 ),
 ( #2248, #1729, #14041, #30001, #33935, #42081, #34460, #5672 ) ),
 .UNSPECIFIED., .F., .F., .F.,
 ( 4, 1, 1, 1, 1, 1, 1, 1, 4 ),
 ( 4, 2, 2, 4 ),
 ( -5.055087509999999899E-06, 0.1250000000000000000, 0.2500000000000000000, 0.3750000000000000000, 0.5000000000000000000, 0.6250000000000000000, 0.7500000000000000000, 0.8750000000000000000, 1.000052120045700210 ),
 ( -5.212004572900000261E-05, 0.2077504819954940074, 0.4451796042760580163, 0.5134866592470029856 ),
 .UNSPECIFIED. ) ;
#37684 = DIRECTION ( 'NONE',  ( -1.000000000000000000, 0.000000000000000000, 0.000000000000000000 ) ) ;
#37685 = EDGE_LOOP ( 'NONE', ( #2271, #6183, #15904, #5204, #27062, #12059, #42940, #2301, #21248, #39572 ) ) ;
#37686 = ORIENTED_EDGE ( 'NONE', *, *, #19775, .F. ) ;
#37687 = CARTESIAN_POINT ( 'NONE',  ( 11.57186432615189986, -64.94495217133389531, -16.50172565924879819 ) ) ;
#37688 = CARTESIAN_POINT ( 'NONE',  ( 11.92298585889120055, 33.98754786523329585, -46.74540749962589814 ) ) ;
#37689 = CARTESIAN_POINT ( 'NONE',  ( 23.79983412839517598, -13.61705418525005129, -39.42650676693061484 ) ) ;
#37690 = FACE_OUTER_BOUND ( 'NONE', #24194, .T. ) ;
#37691 = DIRECTION ( 'NONE',  ( 0.000000000000000000, 1.000000000000000000, 0.000000000000000000 ) ) ;
#37692 = VERTEX_POINT ( 'NONE', #28755 ) ;
#37693 = CARTESIAN_POINT ( 'NONE',  ( -10.12641005879179978, -44.73605830922169702, -43.60172970322699371 ) ) ;
#37694 = CARTESIAN_POINT ( 'NONE',  ( 16.13393739769620083, -15.61618894467929941, -5.966499999999999915 ) ) ;
#37695 = CARTESIAN_POINT ( 'NONE',  ( 53.02924607949410074, -49.59742459721449848, -49.05876173540320195 ) ) ;
#37696 = CARTESIAN_POINT ( 'NONE',  ( 47.18316543498789883, 23.57499020383020039, -54.61069134556619531 ) ) ;
#37697 = CARTESIAN_POINT ( 'NONE',  ( 61.51944663974359884, -1.517445158300650077, -16.03079937703390101 ) ) ;
#37698 = ADVANCED_FACE ( 'NONE', ( #989 ), #40307, .T. ) ;
#37699 = CARTESIAN_POINT ( 'NONE',  ( 51.07962911547610219, -49.63241203261180345, -76.32455169559919739 ) ) ;
#37700 = AXIS2_PLACEMENT_3D ( 'NONE', #40298, #711, #40809 ) ;
#37701 = CARTESIAN_POINT ( 'NONE',  ( 60.69770888843060419, -45.49484844471260203, -47.37007937758740184 ) ) ;
#37702 = ORIENTED_EDGE ( 'NONE', *, *, #14736, .F. ) ;
#37703 = CARTESIAN_POINT ( 'NONE',  ( 8.222914093092873244, -14.70876443408920231, -32.82885229014726036 ) ) ;
#37704 = CARTESIAN_POINT ( 'NONE',  ( 69.22748654599821805, 19.47158195952120963, -71.50000000000200373 ) ) ;
#37705 = ORIENTED_EDGE ( 'NONE', *, *, #45992, .T. ) ;
#37706 = CARTESIAN_POINT ( 'NONE',  ( 18.20470625429515366, -7.911114086817085500, -57.09100124538479548 ) ) ;
#37707 = CARTESIAN_POINT ( 'NONE',  ( 63.93393739769619089, 1.883811055320669947, -62.44999999999999574 ) ) ;
#37708 = CARTESIAN_POINT ( 'NONE',  ( 19.66219730728080251, -22.62604840133040085, -38.36406440404209661 ) ) ;
#37709 = CARTESIAN_POINT ( 'NONE',  ( 14.26103652196149874, -51.11779225937510063, -22.45545332540699945 ) ) ;
#37710 = CARTESIAN_POINT ( 'NONE',  ( 54.43019278679749817, 19.49833644664489896, -76.17363668804328825 ) ) ;
#37711 = CARTESIAN_POINT ( 'NONE',  ( 47.52149247108939534, -54.49734860518730528, -74.72520730820750146 ) ) ;
#37712 = EDGE_LOOP ( 'NONE', ( #36518, #43496, #46599, #16289, #37355, #25490 ) ) ;
#37713 = CIRCLE ( 'NONE', #18441, 1.000000000000000000 ) ;
#37714 = CARTESIAN_POINT ( 'NONE',  ( 55.42572184083550013, 14.71981156885540187, -16.50084453451690081 ) ) ;
#37715 = CARTESIAN_POINT ( 'NONE',  ( 10.77457706359389888, 32.17075419748780263, -45.20848294960729419 ) ) ;
#37716 = CARTESIAN_POINT ( 'NONE',  ( 57.07894516969589915, -50.21246463426640361, -52.67137581470450414 ) ) ;
#37718 = CARTESIAN_POINT ( 'NONE',  ( 52.84289957970359808, -49.69201392618609958, -48.97083559310770084 ) ) ;
#37717 = AXIS2_PLACEMENT_3D ( 'NONE', #32315, #39702, #48335 ) ;
#37719 = EDGE_CURVE ( 'NONE', #1476, #9581, #9116, .T. ) ;
#37720 = CARTESIAN_POINT ( 'NONE',  ( 11.57174743202489964, -10.23757062443000088, -32.12326274055600095 ) ) ;
#37721 = CARTESIAN_POINT ( 'NONE',  ( 13.10629489870523479, -49.56476373416713699, -34.89146800830128825 ) ) ;
#37722 = CIRCLE ( 'NONE', #44417, 0.5000000000000000000 ) ;
#37723 = ADVANCED_FACE ( 'NONE', ( #37153 ), #21148, .T. ) ;
#37724 = CARTESIAN_POINT ( 'NONE',  ( 47.55560966394020284, 23.31156186583769951, -74.50254675453470554 ) ) ;
#37725 = CARTESIAN_POINT ( 'NONE',  ( 19.90605753960891633, -54.76250717792285627, -18.14605458641800695 ) ) ;
#37726 = CARTESIAN_POINT ( 'NONE',  ( 60.89859637212024523, -45.70159618970223647, -47.74371479433301602 ) ) ;
#37727 = CARTESIAN_POINT ( 'NONE',  ( 68.13393739769598767, -2.032350560839250253, -102.2016796975539989 ) ) ;
#37728 = CARTESIAN_POINT ( 'NONE',  ( 33.32492040332130045, -15.61618894398128177, 14.34999999999999964 ) ) ;
#37729 = CARTESIAN_POINT ( 'NONE',  ( 16.63546379641747208, -49.61618961575661046, -83.24416995775972339 ) ) ;
#37730 = CARTESIAN_POINT ( 'NONE',  ( 60.23130391297029718, 14.55066440145539985, -47.24246919202519734 ) ) ;
#37731 = CARTESIAN_POINT ( 'NONE',  ( 73.26121012496899709, 0.8838110553206759423, -68.76625967790960203 ) ) ;
#37733 = CARTESIAN_POINT ( 'NONE',  ( 46.37986018651987052, -40.25936219620972167, -54.53427625130012757 ) ) ;
#37732 = LINE ( 'NONE', #17808, #24073 ) ;
#37734 = CARTESIAN_POINT ( 'NONE',  ( 61.28610485260839624, 13.99802463568589950, -46.40240378558789303 ) ) ;
#37735 = DIRECTION ( 'NONE',  ( -0.6653150774959307734, 0.7465626883635316791, 0.000000000000000000 ) ) ;
#37736 = CARTESIAN_POINT ( 'NONE',  ( -26.59371227466860077, 10.28970141081249778, -54.97277084359720334 ) ) ;
#37737 = ORIENTED_EDGE ( 'NONE', *, *, #41996, .F. ) ;
#37738 = EDGE_CURVE ( 'NONE', #16879, #18612, #33362, .T. ) ;
#37739 = CARTESIAN_POINT ( 'NONE',  ( 52.95762509366560522, -49.59632487776790555, -48.83320048153250070 ) ) ;
#37740 = VERTEX_POINT ( 'NONE', #45535 ) ;
#37741 = CARTESIAN_POINT ( 'NONE',  ( 42.18937197816117646, 8.603191575157895343, -75.20614456104748058 ) ) ;
#37742 = LINE ( 'NONE', #13893, #45313 ) ;
#37743 = CARTESIAN_POINT ( 'NONE',  ( 57.47357173634619443, 14.06667768184960110, -25.92429215579529966 ) ) ;
#37744 = CARTESIAN_POINT ( 'NONE',  ( 9.874923758134890761, -18.86692839231439933, -45.30034255656079978 ) ) ;
#37745 = CARTESIAN_POINT ( 'NONE',  ( 29.09106731080629871, -26.72413521581369977, -34.94555596725399482 ) ) ;
#37747 = EDGE_CURVE ( 'NONE', #48296, #121, #28924, .T. ) ;
#37746 = CARTESIAN_POINT ( 'NONE',  ( 53.53746104739140321, 18.13863166559730189, -49.11443482728900278 ) ) ;
#37748 = CARTESIAN_POINT ( 'NONE',  ( 64.95277593799399085, 1.369976237678190101, -60.95504431261769440 ) ) ;
#37749 = CARTESIAN_POINT ( 'NONE',  ( 60.63856430484059956, -45.56966716085530322, -47.11562948342380253 ) ) ;
#37750 = CARTESIAN_POINT ( 'NONE',  ( 16.32627796171218293, 19.85723994308319362, -15.67246579343190405 ) ) ;
#37751 = VERTEX_POINT ( 'NONE', #40561 ) ;
#37752 = CARTESIAN_POINT ( 'NONE',  ( 23.11151459842839984, -18.22772311948279977, -77.18134062521549765 ) ) ;
#37753 = CARTESIAN_POINT ( 'NONE',  ( 72.92486918121929307, 1.326324093417220240, -68.83951043167449768 ) ) ;
#37754 = CARTESIAN_POINT ( 'NONE',  ( 47.45327857978769970, -54.61763921174910053, -54.72404006642570096 ) ) ;
#37755 = CARTESIAN_POINT ( 'NONE',  ( 23.69469079014621116, -13.18663225633502911, -49.69345251610035064 ) ) ;
#37756 = CARTESIAN_POINT ( 'NONE',  ( 73.06112045927889653, 1.270877794983130027, -62.54449628245689752 ) ) ;
#37757 = AXIS2_PLACEMENT_3D ( 'NONE', #36627, #729, #48707 ) ;
#37758 =( BOUNDED_CURVE ( )  B_SPLINE_CURVE ( 2, ( #4123, #32131, #40288 ),
 .UNSPECIFIED., .F., .T. ) 
 B_SPLINE_CURVE_WITH_KNOTS ( ( 3, 3 ),
 ( 1.104980434577240045, 2.168627590050199672 ),
 .UNSPECIFIED. ) 
 CURVE ( )  GEOMETRIC_REPRESENTATION_ITEM ( )  RATIONAL_B_SPLINE_CURVE ( ( 1.323085463760209857, 1.425426480542939967, 1.425426480542939967 ) ) 
 REPRESENTATION_ITEM ( '' )  );
#37759 = CARTESIAN_POINT ( 'NONE',  ( 10.72320681400480069, -64.90816318788569106, -17.84617904804760258 ) ) ;
#37760 = CARTESIAN_POINT ( 'NONE',  ( 71.42907483962369497, 1.326134026835569912, -60.90937915352040477 ) ) ;
#37761 = CARTESIAN_POINT ( 'NONE',  ( 23.03994194550808672, -19.61239988445705862, -75.95950967876112259 ) ) ;
#37762 = CARTESIAN_POINT ( 'NONE',  ( 18.22483727046438773, -9.153516611488269561, -62.05237194099072440 ) ) ;
#37763 = AXIS2_PLACEMENT_3D ( 'NONE', #12697, #4821, #28651 ) ;
#37764 = AXIS2_PLACEMENT_3D ( 'NONE', #29627, #46681, #30140 ) ;
#37765 = CARTESIAN_POINT ( 'NONE',  ( 16.06492382637960858, -23.55873069923232777, -46.01057597322125048 ) ) ;
#37766 = CARTESIAN_POINT ( 'NONE',  ( 64.90488303983279650, 1.264791438333819906, -70.51396375885850887 ) ) ;
#37767 = ORIENTED_EDGE ( 'NONE', *, *, #4649, .T. ) ;
#37768 = B_SPLINE_CURVE_WITH_KNOTS ( 'NONE', 3,
 ( #23227, #22974, #26918, #14873, #19058, #35031, #43689, #51036, #15395, #34776, #46605, #30836, #3603, #46866, #3343, #47624, #27691, #31607 ),
 .UNSPECIFIED., .F., .F.,
 ( 4, 2, 2, 2, 2, 2, 2, 2, 4 ),
 ( 0.5000000029181979055, 0.5625000025534231396, 0.6250000021886483736, 0.6875000018238737187, 0.7500000014590989528, 0.8125000010943241868, 0.8750000007295495319, 0.9375000003647747659, 1.000000000000000000 ),
 .UNSPECIFIED. ) ;
#37769 = CARTESIAN_POINT ( 'NONE',  ( 8.978915886419921222, -63.28580153388660534, -46.63388789120410394 ) ) ;
#37770 = CARTESIAN_POINT ( 'NONE',  ( 9.367379825797401693, -15.61607429561870042, -45.84717978380999881 ) ) ;
#37771 = ORIENTED_EDGE ( 'NONE', *, *, #42141, .T. ) ;
#37772 = CARTESIAN_POINT ( 'NONE',  ( -2.366062599821302292, -15.61618894518879763, 4.350000001194220367 ) ) ;
#37773 = DIRECTION ( 'NONE',  ( 0.000000000000000000, 0.000000000000000000, -1.000000000000000000 ) ) ;
#37774 = FACE_OUTER_BOUND ( 'NONE', #14802, .T. ) ;
#37775 = CARTESIAN_POINT ( 'NONE',  ( 51.61768760743510143, 19.12657443447390193, -76.35064948391979556 ) ) ;
#37776 = B_SPLINE_CURVE_WITH_KNOTS ( 'NONE', 3,
 ( #40294, #12783, #36603, #15675 ),
 .UNSPECIFIED., .F., .F.,
 ( 4, 4 ),
 ( 0.000000000000000000, 1.000000000000000000 ),
 .UNSPECIFIED. ) ;
#37777 = ORIENTED_EDGE ( 'NONE', *, *, #37747, .F. ) ;
#37778 = CARTESIAN_POINT ( 'NONE',  ( 8.784728771177240603, -63.11543068614769680, -46.67204636144870022 ) ) ;
#37779 = LINE ( 'NONE', #9232, #49407 ) ;
#37780 = FACE_OUTER_BOUND ( 'NONE', #33789, .T. ) ;
#37781 = CARTESIAN_POINT ( 'NONE',  ( 8.189894513438611412, -13.40827076027780151, -52.87862267922429282 ) ) ;
#37782 = CARTESIAN_POINT ( 'NONE',  ( 9.366455112259469473, -15.61627688590920116, -55.45282021618999835 ) ) ;
#37783 = CARTESIAN_POINT ( 'NONE',  ( 43.72333004139270685, -37.88011359077987095, -71.70303684443479142 ) ) ;
#37784 = ORIENTED_EDGE ( 'NONE', *, *, #8054, .F. ) ;
#37785 = CARTESIAN_POINT ( 'NONE',  ( 18.54731091585823677, 20.81200738380825399, -75.33783710306417447 ) ) ;
#37786 = CARTESIAN_POINT ( 'NONE',  ( 10.27832463521709983, -20.22254248962530099, -43.02048744625579246 ) ) ;
#37787 = CARTESIAN_POINT ( 'NONE',  ( 52.74562315164479998, -49.73950520563579403, -48.86764759941510050 ) ) ;
#37788 = CARTESIAN_POINT ( 'NONE',  ( 8.894205530028397533, -15.14404388050549954, -32.14999999999999858 ) ) ;
#37789 = EDGE_CURVE ( 'NONE', #23557, #47819, #13865, .T. ) ;
#37790 = CARTESIAN_POINT ( 'NONE',  ( 13.72054943061259991, 20.81202934652590031, -75.33782839756391070 ) ) ;
#37791 = ADVANCED_FACE ( 'NONE', ( #16710 ), #45016, .T. ) ;
#37792 = FACE_OUTER_BOUND ( 'NONE', #44971, .T. ) ;
#37793 = CIRCLE ( 'NONE', #47021, 1.000000000000000888 ) ;
#37794 = CARTESIAN_POINT ( 'NONE',  ( 43.02887931165090407, -45.36581441162159933, -6.968331744212270529 ) ) ;
#37795 = CARTESIAN_POINT ( 'NONE',  ( 11.89147504607354655, -8.873838868181545436, -60.82910890462889597 ) ) ;
#37796 = AXIS2_PLACEMENT_3D ( 'NONE', #4532, #36497, #12676 ) ;
#37797 = CARTESIAN_POINT ( 'NONE',  ( 7.901851024471708840, -16.08038141849450042, -54.48973855994069737 ) ) ;
#37798 = VERTEX_POINT ( 'NONE', #49480 ) ;
#37799 = CARTESIAN_POINT ( 'NONE',  ( 52.72629826234909700, -49.69265837912299588, -27.60314321031239970 ) ) ;
#37800 = CARTESIAN_POINT ( 'NONE',  ( 16.60577464339360176, -51.11619062818909498, -20.14978695510610152 ) ) ;
#37802 = DIRECTION ( 'NONE',  ( -0.08481436951012806535, 0.9963967697281035374, 0.000000000000000000 ) ) ;
#37801 = CARTESIAN_POINT ( 'NONE',  ( 10.55533566658999867, 33.19687060618380059, -16.53455939563230004 ) ) ;
#37803 = CARTESIAN_POINT ( 'NONE',  ( 8.223340741289188571, -15.61635616670070092, -42.79233150823699816 ) ) ;
#37804 = CARTESIAN_POINT ( 'NONE',  ( 68.13393739769618662, -0.1661889446793529956, -65.65000000000000568 ) ) ;
#37805 = ORIENTED_EDGE ( 'NONE', *, *, #22992, .T. ) ;
#37806 = CARTESIAN_POINT ( 'NONE',  ( -3.303846065640429597, -48.27785255937200048, -4.380151423638459995 ) ) ;
#37807 = CARTESIAN_POINT ( 'NONE',  ( 47.50639103848880751, 23.34221793459570193, -54.65667269328779554 ) ) ;
#37808 = CARTESIAN_POINT ( 'NONE',  ( 56.52536539877740296, -50.75180572374080157, -53.84278118897309895 ) ) ;
#37809 = CARTESIAN_POINT ( 'NONE',  ( 63.25638208530150308, 1.265664290790580182, -62.44691083073610116 ) ) ;
#37810 = CARTESIAN_POINT ( 'NONE',  ( 12.86000844245529962, 19.41066285990589790, -21.34825237919379859 ) ) ;
#37811 = CARTESIAN_POINT ( 'NONE',  ( 61.14309862408159546, 14.08829758490710127, -46.99564608385690434 ) ) ;
#37812 = CARTESIAN_POINT ( 'NONE',  ( 11.74133914242139909, 34.13528131095510076, -17.40968318378989821 ) ) ;
#37813 = DIRECTION ( 'NONE',  ( -1.000000000000000000, 0.000000000000000000, 0.000000000000000000 ) ) ;
#37815 = EDGE_CURVE ( 'NONE', #16231, #49938, #25331, .T. ) ;
#37814 = CARTESIAN_POINT ( 'NONE',  ( 83.89200044194980421, 17.38381105532069881, -53.92796738110899923 ) ) ;
#37816 = DIRECTION ( 'NONE',  ( 1.000000000000000000, 0.000000000000000000, 0.000000000000000000 ) ) ;
#37817 = CARTESIAN_POINT ( 'NONE',  ( 55.20364026414679870, -48.56255352766319788, -48.76217699417520635 ) ) ;
#37818 = CARTESIAN_POINT ( 'NONE',  ( 65.13393739769620083, 1.383811055320669947, -65.65000000000000568 ) ) ;
#37819 = CARTESIAN_POINT ( 'NONE',  ( 52.01880079388769929, 21.21768078984590034, -53.65151492245650644 ) ) ;
#37820 = CARTESIAN_POINT ( 'NONE',  ( 63.75430343581950154, 1.400155262441499904, -69.47341233291868434 ) ) ;
#37821 = CARTESIAN_POINT ( 'NONE',  ( 11.98643060099639968, -65.41791523794120167, -17.50083490704260214 ) ) ;
#37822 = CARTESIAN_POINT ( 'NONE',  ( 68.13393739769630031, 1.530257664727401767, -69.99644660940670349 ) ) ;
#37823 = ORIENTED_EDGE ( 'NONE', *, *, #16122, .F. ) ;
#37824 = CARTESIAN_POINT ( 'NONE',  ( 71.25019707560579718, 0.8838110553206759423, -60.52272727272730179 ) ) ;
#37825 = CARTESIAN_POINT ( 'NONE',  ( 11.10544830731869936, 31.99586678468589795, -44.25060200236470109 ) ) ;
#37826 = CARTESIAN_POINT ( 'NONE',  ( 58.92073396209919878, -15.61618894467929941, -18.64999999999999858 ) ) ;
#37827 = CARTESIAN_POINT ( 'NONE',  ( 66.02283960027239118, -32.66876353588650517, -18.53621209913480072 ) ) ;
#37828 = CARTESIAN_POINT ( 'NONE',  ( 8.222918173831372357, -14.85904556795307485, -80.53814063808331980 ) ) ;
#37829 = ORIENTED_EDGE ( 'NONE', *, *, #41129, .T. ) ;
#37830 = ORIENTED_EDGE ( 'NONE', *, *, #48986, .T. ) ;
#37831 = FACE_OUTER_BOUND ( 'NONE', #22956, .T. ) ;
#37832 = CARTESIAN_POINT ( 'NONE',  ( 50.01965577494885906, -1.349691835600933087, -15.97243907347640679 ) ) ;
#37833 = ORIENTED_EDGE ( 'NONE', *, *, #40095, .F. ) ;
#37834 = CARTESIAN_POINT ( 'NONE',  ( 12.06186543847180026, -65.21351140459039186, -46.02873399224909434 ) ) ;
#37835 = CARTESIAN_POINT ( 'NONE',  ( 57.48932555802679900, -45.43918670114770464, -26.08426967047639877 ) ) ;
#37836 = CARTESIAN_POINT ( 'NONE',  ( 24.04493740255118439, -15.61827380739441118, -77.50775418025503427 ) ) ;
#37837 = VECTOR ( 'NONE', #18786, 1000.000000000000000 ) ;
#37838 = CARTESIAN_POINT ( 'NONE',  ( 27.13393739769620083, 7.383811055320659733, -84.65000000000000568 ) ) ;
#37839 = ORIENTED_EDGE ( 'NONE', *, *, #1473, .F. ) ;
#37840 = CIRCLE ( 'NONE', #6031, 6.049999999999999822 ) ;
#37841 = CARTESIAN_POINT ( 'NONE',  ( 46.11861065021020067, 6.933294690613563738, -59.72657760612104028 ) ) ;
#37842 = VERTEX_POINT ( 'NONE', #48696 ) ;
#37843 = CARTESIAN_POINT ( 'NONE',  ( 52.85262840411130014, -45.20798072659410138, -13.23787260301519986 ) ) ;
#37844 = CARTESIAN_POINT ( 'NONE',  ( 12.36442939451902667, -22.59821236439503522, -34.44981817989418715 ) ) ;
#37845 = CARTESIAN_POINT ( 'NONE',  ( 16.48362619534700002, 19.88018432961980153, -20.43421124880899953 ) ) ;
#37846 = B_SPLINE_CURVE_WITH_KNOTS ( 'NONE', 3,
 ( #4704, #49521, #20672, #13613, #21190, #29064, #45060, #1808, #9161, #25378 ),
 .UNSPECIFIED., .F., .F.,
 ( 4, 1, 1, 1, 1, 1, 1, 4 ),
 ( 0.4999989579104466841, 0.5363602085422365384, 0.6155791396058006848, 0.6947980706695208175, 0.7740170017330827434, 0.8532359327968050966, 0.9324548638603670225, 1.000000000000000000 ),
 .UNSPECIFIED. ) ;
#37847 = DIRECTION ( 'NONE',  ( -0.000000000000000000, -1.000000000000000000, -0.000000000000000000 ) ) ;
#37848 = ORIENTED_EDGE ( 'NONE', *, *, #40229, .F. ) ;
#37849 = DIRECTION ( 'NONE',  ( -1.000000000000000000, -0.000000000000000000, -0.000000000000000000 ) ) ;
#37850 = CARTESIAN_POINT ( 'NONE',  ( 47.20301019691079603, -54.79104926684230037, -74.19830160072660874 ) ) ;
#37851 = CARTESIAN_POINT ( 'NONE',  ( 56.54598780672240110, 13.11993018277919987, -8.486630820524080576 ) ) ;
#37852 = CARTESIAN_POINT ( 'NONE',  ( 50.23538084491709554, -49.77012050973750235, -76.14999999999999147 ) ) ;
#37853 = EDGE_CURVE ( 'NONE', #9596, #19643, #13568, .T. ) ;
#37854 = CARTESIAN_POINT ( 'NONE',  ( 54.22654478441499748, 20.21700441338549936, -53.14607073534880044 ) ) ;
#37855 = PRODUCT_DEFINITION_SHAPE ( 'NONE', 'NONE',  #51873 ) ;
#37856 = DIRECTION ( 'NONE',  ( -1.000000000000000000, 0.000000000000000000, 0.000000000000000000 ) ) ;
#37857 = CARTESIAN_POINT ( 'NONE',  ( 61.51104789187949962, 13.91173340009640036, -28.09355830686730116 ) ) ;
#37858 = CARTESIAN_POINT ( 'NONE',  ( 23.81821264185619924, -14.02287097416230033, -71.22242690490419648 ) ) ;
#37859 = VERTEX_POINT ( 'NONE', #44754 ) ;
#37860 = DIRECTION ( 'NONE',  ( 0.000000000000000000, 0.000000000000000000, 1.000000000000000000 ) ) ;
#37861 = B_SPLINE_CURVE_WITH_KNOTS ( 'NONE', 3,
 ( #18731, #50967, #3275, #15330, #43373, #26851, #39440, #34710, #31033, #30774, #10888, #47059, #46797, #38400, #30260, #18217, #46281, #10367 ),
 .UNSPECIFIED., .F., .F.,
 ( 4, 2, 2, 2, 2, 2, 2, 2, 4 ),
 ( 0.000000000000000000, 0.06250000073800097977, 0.1250000014760019595, 0.1875000022140029254, 0.2500000029520039191, 0.3125000036900049127, 0.3750000044280058509, 0.4375000051660068445, 0.5000000059040078382 ),
 .UNSPECIFIED. ) ;
#37862 = CARTESIAN_POINT ( 'NONE',  ( 2.277530937145189949, -15.61618894467929941, -32.14999999999999858 ) ) ;
#37863 = CARTESIAN_POINT ( 'NONE',  ( 84.13393739769618662, -30.49118894467929763, -65.65000000000000568 ) ) ;
#37864 = CARTESIAN_POINT ( 'NONE',  ( 72.69256032412449997, 1.379674774869650067, -69.17486252676589231 ) ) ;
#37865 = CARTESIAN_POINT ( 'NONE',  ( 71.47612964547799663, 0.8925687589132609290, -60.66703147076970737 ) ) ;
#37866 = EDGE_CURVE ( 'NONE', #17310, #24832, #14624, .T. ) ;
#37867 = AXIS2_PLACEMENT_3D ( 'NONE', #50410, #17399, #41758 ) ;
#37868 = VECTOR ( 'NONE', #25629, 1000.000000000000114 ) ;
#37869 = CARTESIAN_POINT ( 'NONE',  ( 16.13393739769620083, -15.61618894467929941, -69.65000000000000568 ) ) ;
#37870 = CARTESIAN_POINT ( 'NONE',  ( 12.14972608106025120, -8.703710964786449011, -42.84096575448170086 ) ) ;
#37871 = CARTESIAN_POINT ( 'NONE',  ( 12.69301297134110129, 19.09118037685809810, -21.19712480391079978 ) ) ;
#37873 = ADVANCED_FACE ( 'NONE', ( #3254 ), #2472, .T. ) ;
#37872 = CARTESIAN_POINT ( 'NONE',  ( 12.14970654918197823, -8.703721948391146768, -59.12570771485219012 ) ) ;
#37874 = CARTESIAN_POINT ( 'NONE',  ( 70.99050876911339003, 1.383811055320669947, -60.94999999999999574 ) ) ;
#37875 = CARTESIAN_POINT ( 'NONE',  ( 41.53147706019129970, -44.71252858122500129, -5.331435815133920286 ) ) ;
#37876 = CARTESIAN_POINT ( 'NONE',  ( -1.365754458141149819, 11.26366790782569893, -20.15000000000000213 ) ) ;
#37877 = CARTESIAN_POINT ( 'NONE',  ( 18.84530080626689852, -51.72201830638929465, -74.14993436883820266 ) ) ;
#37878 = EDGE_CURVE ( 'NONE', #48268, #9595, #21398, .T. ) ;
#37879 = VERTEX_POINT ( 'NONE', #23394 ) ;
#37880 = CARTESIAN_POINT ( 'NONE',  ( 10.64020559113360065, -20.64864412837480145, -51.83128268485729961 ) ) ;
#37881 = CARTESIAN_POINT ( 'NONE',  ( 63.75818144730860126, 1.026088617261689873, -61.54425306709249810 ) ) ;
#37882 = ORIENTED_EDGE ( 'NONE', *, *, #29086, .T. ) ;
#37883 = CARTESIAN_POINT ( 'NONE',  ( 11.97533377483439487, -21.02756021161885158, -69.16115284857546897 ) ) ;
#37884 = DIRECTION ( 'NONE',  ( 0.000000000000000000, 0.7071067811865492381, 0.7071067811865457964 ) ) ;
#37885 = CARTESIAN_POINT ( 'NONE',  ( 51.13393739769620083, 19.38381105532069881, 16.85000000000000142 ) ) ;
#37886 = FACE_OUTER_BOUND ( 'NONE', #5422, .T. ) ;
#37888 = DIRECTION ( 'NONE',  ( 0.000000000000000000, 0.000000000000000000, 1.000000000000000000 ) ) ;
#37887 = CARTESIAN_POINT ( 'NONE',  ( 44.39456236031976033, 8.753821728143037717, -64.74790854932149387 ) ) ;
#37889 = CARTESIAN_POINT ( 'NONE',  ( 24.04518460902906085, -15.61618869790763675, -47.79232989768991757 ) ) ;
#37890 = CARTESIAN_POINT ( 'NONE',  ( 44.92052329722529436, -46.01048457530889380, -8.851553140290988608 ) ) ;
#37891 = ORIENTED_EDGE ( 'NONE', *, *, #14, .F. ) ;
#37892 = ORIENTED_EDGE ( 'NONE', *, *, #13735, .T. ) ;
#37893 = EDGE_LOOP ( 'NONE', ( #15070, #28645, #26072, #44973 ) ) ;
#37894 = CARTESIAN_POINT ( 'NONE',  ( -22.79177331775788673, -17.86816468640815003, -54.71780484469083206 ) ) ;
#37895 = CARTESIAN_POINT ( 'NONE',  ( 53.42104377997379316, -49.46540347068880550, -49.21624230352519902 ) ) ;
#37896 = CARTESIAN_POINT ( 'NONE',  ( 52.56522529778620623, -49.86179102641759897, -48.47379134784809906 ) ) ;
#37897 = CARTESIAN_POINT ( 'NONE',  ( 54.99091206896520134, -51.40428974184509769, -54.03945093368859887 ) ) ;
#37898 = ORIENTED_EDGE ( 'NONE', *, *, #15949, .F. ) ;
#37899 = ORIENTED_EDGE ( 'NONE', *, *, #39796, .F. ) ;
#37900 = DIRECTION ( 'NONE',  ( -1.000000000000000000, 0.000000000000000000, 0.000000000000000000 ) ) ;
#37901 = CARTESIAN_POINT ( 'NONE',  ( 28.13393739769619728, -8.687985714403851034, -35.14999999999999858 ) ) ;
#37902 = CARTESIAN_POINT ( 'NONE',  ( 16.13393739769620083, -29.53197612349504553, -34.89146800830128825 ) ) ;
#37903 = VERTEX_POINT ( 'NONE', #34688 ) ;
#37904 = CARTESIAN_POINT ( 'NONE',  ( 24.01027070323695867, -16.38076406562427678, -49.53846147474892092 ) ) ;
#37906 = CARTESIAN_POINT ( 'NONE',  ( 53.23404681179649600, -50.62188124027260017, -76.66833019152879558 ) ) ;
#37905 = CIRCLE ( 'NONE', #40433, 28.31678667024650409 ) ;
#37907 = CARTESIAN_POINT ( 'NONE',  ( 60.74039577305779858, 14.35309089330909949, -47.45735349090180222 ) ) ;
#37908 = CARTESIAN_POINT ( 'NONE',  ( 9.901417542572799491, -10.84728510343080110, -73.22039407203469352 ) ) ;
#37909 = CYLINDRICAL_SURFACE ( 'NONE', #31345, 1.000000000000029976 ) ;
#37910 = CARTESIAN_POINT ( 'NONE',  ( 41.43650635183630015, 13.58022812337069851, -5.462486971552510617 ) ) ;
#37911 = ADVANCED_FACE ( 'NONE', ( #7188 ), #18713, .T. ) ;
#37912 = CARTESIAN_POINT ( 'NONE',  ( 41.88234443079220171, -43.67296333914980266, -3.969549610420470387 ) ) ;
#37913 = CARTESIAN_POINT ( 'NONE',  ( 72.49279582477669237, 1.028300555801499927, -61.52602141601349928 ) ) ;
#37914 = CARTESIAN_POINT ( 'NONE',  ( -7.625877374285919608, 14.22289747138790084, -5.682500641286110543 ) ) ;
#37915 = CARTESIAN_POINT ( 'NONE',  ( 64.57873039904879420, 0.9579170000946040098, -70.48345851730660172 ) ) ;
#37916 = CARTESIAN_POINT ( 'NONE',  ( 46.47536507427530239, 8.886826513564159313, -54.64999999999999858 ) ) ;
#37917 = CARTESIAN_POINT ( 'NONE',  ( 65.62515792676039439, 0.5188969770332930720, -17.33365040072970231 ) ) ;
#37918 = ORIENTED_EDGE ( 'NONE', *, *, #22299, .T. ) ;
#37919 = CARTESIAN_POINT ( 'NONE',  ( 15.05440318628160057, -53.11618894467930119, -76.14999999999999147 ) ) ;
#37920 = CIRCLE ( 'NONE', #15337, 0.5000000000000004441 ) ;
#37921 = CARTESIAN_POINT ( 'NONE',  ( 47.21101641624719747, -54.78526367574990275, -54.63499203783069902 ) ) ;
#37922 = DIRECTION ( 'NONE',  ( -0.8090169943749453418, 0.5877852522924759127, 0.000000000000000000 ) ) ;
#37923 = DIRECTION ( 'NONE',  ( 0.000000000000000000, 0.000000000000000000, -1.000000000000000000 ) ) ;
#37924 = DIRECTION ( 'NONE',  ( 0.000000000000000000, 0.000000000000000000, 1.000000000000000000 ) ) ;
#37925 = CARTESIAN_POINT ( 'NONE',  ( 63.13228119804391270, 0.8904513541338849869, -68.96413986139360475 ) ) ;
#37926 = CARTESIAN_POINT ( 'NONE',  ( 48.00591971102450373, -54.35791002652510429, -54.98714547078049719 ) ) ;
#37927 = CARTESIAN_POINT ( 'NONE',  ( 19.13393739769620083, -49.61618894467939356, -34.64999999999999858 ) ) ;
#37928 = CARTESIAN_POINT ( 'NONE',  ( -8.116933555512177989, -44.87420182799904467, -5.094470741909731260 ) ) ;
#37929 = CARTESIAN_POINT ( 'NONE',  ( 9.221370973493520751, -19.60024637595736863, -46.62569193087001906 ) ) ;
#37930 = EDGE_CURVE ( 'NONE', #4326, #34714, #24718, .T. ) ;
#37931 = CARTESIAN_POINT ( 'NONE',  ( 47.90090429088169799, 23.17274928892609864, -54.97513107683430889 ) ) ;
#37932 = ORIENTED_EDGE ( 'NONE', *, *, #27466, .T. ) ;
#37933 = CIRCLE ( 'NONE', #30356, 2.999999999999999112 ) ;
#37934 = CARTESIAN_POINT ( 'NONE',  ( 23.03988594485150188, -14.18425534339259997, -70.78210109960220109 ) ) ;
#37935 = CIRCLE ( 'NONE', #38818, 33.00000000000000000 ) ;
#37936 = ORIENTED_EDGE ( 'NONE', *, *, #19027, .T. ) ;
#37937 = FACE_OUTER_BOUND ( 'NONE', #46068, .T. ) ;
#37938 = CARTESIAN_POINT ( 'NONE',  ( 24.04493739769619864, -15.61618894467929941, -32.14999999999999858 ) ) ;
#37939 = DIRECTION ( 'NONE',  ( 0.000000000000000000, -1.000000000000000000, 0.000000000000000000 ) ) ;
#37941 = CARTESIAN_POINT ( 'NONE',  ( 55.63848436370919615, 15.03490499964270022, -25.39977966304109813 ) ) ;
#37940 = CARTESIAN_POINT ( 'NONE',  ( 83.91322170983950457, 13.24675980165680045, -47.13452068490819613 ) ) ;
#37942 = CARTESIAN_POINT ( 'NONE',  ( 23.18677759228159729, -15.61816030595169913, -74.45290918797279289 ) ) ;
#37943 = DIRECTION ( 'NONE',  ( 1.000000000000000000, 0.000000000000000000, 0.000000000000000000 ) ) ;
#37944 = CARTESIAN_POINT ( 'NONE',  ( 56.36758570843819882, -45.11618894467940066, -15.20758541532019947 ) ) ;
#37945 = CARTESIAN_POINT ( 'NONE',  ( 33.13393739769620083, -38.61618894467930119, -59.64999999999999147 ) ) ;
#37946 = VERTEX_POINT ( 'NONE', #46521 ) ;
#37947 = FACE_OUTER_BOUND ( 'NONE', #3941, .T. ) ;
#37948 = ORIENTED_EDGE ( 'NONE', *, *, #12856, .T. ) ;
#37949 = ORIENTED_EDGE ( 'NONE', *, *, #1477, .T. ) ;
#37950 = CARTESIAN_POINT ( 'NONE',  ( 12.00693377042660082, -64.79851766967649951, -16.09314495739829809 ) ) ;
#37951 = CARTESIAN_POINT ( 'NONE',  ( 24.00787544518242100, -14.82575727831162382, -39.47583133721960991 ) ) ;
#37952 = CARTESIAN_POINT ( 'NONE',  ( -29.90025726814942431, 4.910446297966914564, -56.90830752171230245 ) ) ;
#37953 = CARTESIAN_POINT ( 'NONE',  ( 50.99272666193287051, 4.001659728125646964, -76.39686140629422084 ) ) ;
#37954 = ORIENTED_EDGE ( 'NONE', *, *, #42900, .F. ) ;
#37955 = VERTEX_POINT ( 'NONE', #30498 ) ;
#37956 = CARTESIAN_POINT ( 'NONE',  ( -13.78940531703979921, -41.12028084088070301, -46.90119366654699462 ) ) ;
#37957 = CARTESIAN_POINT ( 'NONE',  ( 64.93393739769749118, 11.38381105532110205, -69.85000000000074749 ) ) ;
#37959 = CIRCLE ( 'NONE', #7883, 0.9999999999999986677 ) ;
#37958 = CARTESIAN_POINT ( 'NONE',  ( 52.63649943311990143, -49.80150522235119581, -48.66853994086150692 ) ) ;
#37960 = CARTESIAN_POINT ( 'NONE',  ( 51.92180556447119955, 19.59192512143929932, -50.64576713626780702 ) ) ;
#37961 = CARTESIAN_POINT ( 'NONE',  ( 63.15143557569741262, -1.746388215850740000, -16.22393059072330246 ) ) ;
#37962 = CARTESIAN_POINT ( 'NONE',  ( 51.40462280232890180, -50.54840350189540032, -76.23573550552210065 ) ) ;
#37963 = CARTESIAN_POINT ( 'NONE',  ( 57.50557710143229428, -49.31997340228490145, -51.53210862891840094 ) ) ;
#37964 = ORIENTED_EDGE ( 'NONE', *, *, #5581, .T. ) ;
#37965 = CARTESIAN_POINT ( 'NONE',  ( 8.222903922732800908, -15.61639209420869889, -32.79233150823699816 ) ) ;
#37966 = CARTESIAN_POINT ( 'NONE',  ( 9.221497967028252418, -19.60046347223059726, -48.62566517465766935 ) ) ;
#37967 = ORIENTED_EDGE ( 'NONE', *, *, #15071, .T. ) ;
#37968 = CARTESIAN_POINT ( 'NONE',  ( 8.222930384839667539, -14.58069280931489153, -52.83399830599484659 ) ) ;
#37969 = CARTESIAN_POINT ( 'NONE',  ( 47.78347825172009777, -46.15534745134900163, -10.88057999588169977 ) ) ;
#37970 = CARTESIAN_POINT ( 'NONE',  ( 17.30631058744340223, -7.454800704868429939, -79.33774565447329508 ) ) ;
#37971 = CARTESIAN_POINT ( 'NONE',  ( 13.64404399975630078, -50.99724096237619619, -21.86438480750510038 ) ) ;
#37972 = CARTESIAN_POINT ( 'NONE',  ( 57.06611319472220600, 19.38619040980010055, -74.64592700447491325 ) ) ;
#37973 = EDGE_CURVE ( 'NONE', #43880, #19145, #29001, .T. ) ;
#37974 = CARTESIAN_POINT ( 'NONE',  ( 47.57154850773469690, -54.56571258662719970, -74.17405913703889553 ) ) ;
#37975 = VERTEX_POINT ( 'NONE', #39160 ) ;
#37976 = CARTESIAN_POINT ( 'NONE',  ( 55.96166294374940264, 14.18843861383079918, -16.30655967985860144 ) ) ;
#37977 = CARTESIAN_POINT ( 'NONE',  ( 9.299128317299539148, 32.06192745982850312, -46.53057822423220102 ) ) ;
#37978 = AXIS2_PLACEMENT_3D ( 'NONE', #36306, #41029, #41288 ) ;
#37979 = ADVANCED_FACE ( 'NONE', ( #31524 ), #45659, .F. ) ;
#37980 = CARTESIAN_POINT ( 'NONE',  ( 56.96124597811810020, -50.60744642191669840, -53.44837636084510279 ) ) ;
#37981 = VECTOR ( 'NONE', #22660, 1000.000000000000114 ) ;
#37982 = CYLINDRICAL_SURFACE ( 'NONE', #16364, 16.00000000000000000 ) ;
#37983 = CARTESIAN_POINT ( 'NONE',  ( 61.28189545210631195, 14.37036762458959238, -47.67949669966547077 ) ) ;
#37984 = EDGE_CURVE ( 'NONE', #15596, #45466, #13058, .T. ) ;
#37985 = CARTESIAN_POINT ( 'NONE',  ( 47.64143408597180240, 23.30250929682300409, -74.17387245455559253 ) ) ;
#37986 = CARTESIAN_POINT ( 'NONE',  ( 65.07262241358380095, 1.198183261254770038, -60.61312937625270081 ) ) ;
#37987 = CARTESIAN_POINT ( 'NONE',  ( 75.47966807050509885, -43.37310274687460065, -13.40512917118210012 ) ) ;
#37988 = CARTESIAN_POINT ( 'NONE',  ( 20.99566025495300536, -9.290059480944934833, -57.50066464107244713 ) ) ;
#37989 = DIRECTION ( 'NONE',  ( 1.000000000000000000, 0.000000000000000000, 0.000000000000000000 ) ) ;
#37990 = CARTESIAN_POINT ( 'NONE',  ( 29.63393739769619728, -15.61618894467929941, -2.149999999999999911 ) ) ;
#37991 = VECTOR ( 'NONE', #44930, 1000.000000000000000 ) ;
#37992 = CARTESIAN_POINT ( 'NONE',  ( -15.80024602150229640, 6.819013759894939852, -48.50583260171929822 ) ) ;
#37994 = CARTESIAN_POINT ( 'NONE',  ( 46.26053575279389918, -39.27325360143171196, -59.27255113039620937 ) ) ;
#37993 = CARTESIAN_POINT ( 'NONE',  ( 64.85894149894409111, 0.8879664753683469414, -60.62259972594610247 ) ) ;
#37995 = CARTESIAN_POINT ( 'NONE',  ( 7.820074255002050556, -9.575813799495708878, -18.58999999999999986 ) ) ;
#37996 = EDGE_CURVE ( 'NONE', #5090, #46086, #29646, .T. ) ;
#37997 = CARTESIAN_POINT ( 'NONE',  ( 6.300025116805320735, 33.86872402518860525, -48.92608059699399803 ) ) ;
#37998 = EDGE_LOOP ( 'NONE', ( #43851, #21065, #14287, #21841, #1869 ) ) ;
#37999 = CARTESIAN_POINT ( 'NONE',  ( 53.22411023516859530, -49.46633164296870433, -48.94726693978910248 ) ) ;
#38000 = VERTEX_POINT ( 'NONE', #10865 ) ;
#38001 = CARTESIAN_POINT ( 'NONE',  ( 47.45189513940888304, 8.060285789217719099, -53.60622457599794899 ) ) ;
#38002 = DIRECTION ( 'NONE',  ( -0.2260571801428161165, 7.216449660063443557E-16, 0.9741140340359943917 ) ) ;
#38003 = CARTESIAN_POINT ( 'NONE',  ( 55.95312836925540267, 14.62053896309619994, -25.39030107927520064 ) ) ;
#38004 = CARTESIAN_POINT ( 'NONE',  ( 9.620888334170560441, -12.91013081656500106, -49.57816483399619756 ) ) ;
#38005 = CARTESIAN_POINT ( 'NONE',  ( 50.85760623216560106, 19.45375030590959753, -76.14999999999999147 ) ) ;
#38006 = CARTESIAN_POINT ( 'NONE',  ( 52.96692102286459658, 18.37433252106210091, -48.95117868485719725 ) ) ;
#38007 = CARTESIAN_POINT ( 'NONE',  ( 64.67849076041288470, 1.005545696829380109, -60.75297091621269630 ) ) ;
#38008 = CARTESIAN_POINT ( 'NONE',  ( 60.55542095703709293, -45.61322829028730297, -47.18108258831090041 ) ) ;
#38009 = CARTESIAN_POINT ( 'NONE',  ( 16.26108084590278935, 19.84491886401188054, -15.67129894889461994 ) ) ;
#38010 = ORIENTED_EDGE ( 'NONE', *, *, #48280, .F. ) ;
#38011 = CARTESIAN_POINT ( 'NONE',  ( 20.08119151113339740, -9.297496097080600208, -72.74508048565279239 ) ) ;
#38013 = CARTESIAN_POINT ( 'NONE',  ( 16.13393739769620083, -15.61618894467929941, -49.12910085600329779 ) ) ;
#38012 = VECTOR ( 'NONE', #1190, 1000.000000000000000 ) ;
#38014 = CARTESIAN_POINT ( 'NONE',  ( 23.15473124193005461, -11.90455973904859732, -49.63748291447825522 ) ) ;
#38015 = CARTESIAN_POINT ( 'NONE',  ( 73.15615143370008866, 1.097085799869290224, -62.44531798733959960 ) ) ;
#38016 = CARTESIAN_POINT ( 'NONE',  ( 56.98397975609619692, 19.46089624346329927, -53.23409293251930308 ) ) ;
#38017 = CARTESIAN_POINT ( 'NONE',  ( 52.90855285609569592, 18.38725884964449975, -48.71990423803699599 ) ) ;
#38018 = CARTESIAN_POINT ( 'NONE',  ( 9.797968754430565141, -20.46465235352011192, -76.58461035990077903 ) ) ;
#38019 = CARTESIAN_POINT ( 'NONE',  ( 21.26777047317277081, -11.15835231960324414, -62.22513457443928786 ) ) ;
#38020 = ADVANCED_FACE ( 'NONE', ( #15568 ), #14786, .T. ) ;
#38021 = CARTESIAN_POINT ( 'NONE',  ( 10.86351723737203123, -21.58463999176102277, -46.23780422378855093 ) ) ;
#38022 = EDGE_LOOP ( 'NONE', ( #37306, #36519, #14046, #30673, #22213 ) ) ;
#38023 = CARTESIAN_POINT ( 'NONE',  ( 64.81933968820119674, 1.186515949276290227, -70.54416184698391135 ) ) ;
#38024 = VERTEX_POINT ( 'NONE', #22890 ) ;
#38025 = CARTESIAN_POINT ( 'NONE',  ( 8.951579501146909479, -63.12553281437028829, -46.63485218348429839 ) ) ;
#38026 = CARTESIAN_POINT ( 'NONE',  ( 63.93393739769619089, 1.383811055320669947, -62.44999999999999574 ) ) ;
#38027 = B_SPLINE_CURVE_WITH_KNOTS ( 'NONE', 3,
 ( #45960, #37836, #41499, #18169, #49894, #10054, #26016, #29437, #42027, #9545, #25497, #5613, #37564, #34136, #46229, #1672, #6383, #2440, #18423, #17660, #11350, #27315, #23621, #35707, #31738, #43576, #7676, #47009, #50663, #26798, #7163, #22856, #51183, #35442, #43828, #18683, #38877, #11608, #51691, #47767, #15278, #27827, #42810, #19716, #27569, #30982, #23360, #31234, #19195, #7926, #3224, #3487, #2965, #47260, #23876, #39640, #18939, #35180, #47512, #34656 ),
 .UNSPECIFIED., .F., .F.,
 ( 4, 2, 1, 1, 1, 1, 1, 2, 2, 2, 2, 2, 2, 2, 2, 1, 1, 1, 1, 1, 1, 2, 2, 2, 2, 2, 2, 1, 1, 1, 1, 1, 2, 2, 2, 2, 2, 4 ),
 ( 0.5000034598518116047, 0.5001255293196273932, 0.5002475987874431818, 0.5004917377230646558, 0.5009800155943028299, 0.5019565713367789561, 0.5039096828217313195, 0.5078159057916349362, 0.5156283517314436127, 0.5312532436110607437, 0.5625030273702946726, 0.5937528111295286015, 0.6093777030091455105, 0.6250025948887624194, 0.6251246643565719907, 0.6252467338243815620, 0.6254908727600008156, 0.6259791506312393228, 0.6269557063737165592, 0.6289088178586710320, 0.6328150408285799777, 0.6406274867683978691, 0.6562523786480337629, 0.6875021624073054394, 0.7187519461665772269, 0.7500017299258489034, 0.7502458688614681570, 0.7504900077970874106, 0.7509782856683260288, 0.7519548414108030432, 0.7539079528957572940, 0.7578141758656659066, 0.7656266218054831318, 0.7812515136851174713, 0.8125012974443863722, 0.8750008649629243962, 0.9375004324814621981, 1.000000000000000000 ),
 .UNSPECIFIED. ) ;
#38028 = ORIENTED_EDGE ( 'NONE', *, *, #38165, .F. ) ;
#38029 = CARTESIAN_POINT ( 'NONE',  ( -11.80944000494479873, 2.826328597561450273, -45.03554556751399929 ) ) ;
#38030 = CARTESIAN_POINT ( 'NONE',  ( 57.04000889551539899, 19.39440449634280128, -53.73354994110280103 ) ) ;
#38031 = CARTESIAN_POINT ( 'NONE',  ( 24.04497561966918440, -15.61618908881887080, -69.50766602643473391 ) ) ;
#38032 = CARTESIAN_POINT ( 'NONE',  ( 53.31396975641249725, 19.22903114769359689, -77.17790062668180440 ) ) ;
#38033 = ORIENTED_EDGE ( 'NONE', *, *, #11718, .F. ) ;
#38034 = LINE ( 'NONE', #29882, #35004 ) ;
#38035 = CARTESIAN_POINT ( 'NONE',  ( 16.13393739769620083, -15.61618894467929941, 5.729250452415290518 ) ) ;
#38036 = CARTESIAN_POINT ( 'NONE',  ( 0.08961746015897857631, -26.87852304757121402, -34.70268271585498354 ) ) ;
#38037 = CARTESIAN_POINT ( 'NONE',  ( 11.23390675766243518, -21.85624464617543694, -66.21956934538100370 ) ) ;
#38038 = CARTESIAN_POINT ( 'NONE',  ( 10.20798635145410138, -9.883316693052110580, -53.03706054135160031 ) ) ;
#38039 = B_SPLINE_CURVE_WITH_KNOTS ( 'NONE', 3,
 ( #39310, #19888, #43252, #19121, #39060, #18860, #31159, #31668, #11536, #35364, #34845, #51101, #35879, #15201, #12615, #51618, #7340, #51363 ),
 .UNSPECIFIED., .F., .F.,
 ( 4, 2, 2, 2, 2, 2, 2, 2, 4 ),
 ( 0.000000000000000000, 0.06250000036477473819, 0.1250000007295494764, 0.1875000010943242146, 0.2500000014590989528, 0.3125000018238737187, 0.3750000021886484292, 0.4375000025534231396, 0.5000000029181979055 ),
 .UNSPECIFIED. ) ;
#38040 = VECTOR ( 'NONE', #15791, 1000.000000000000000 ) ;
#38041 = DIRECTION ( 'NONE',  ( 0.000000000000000000, -1.000000000000000000, 0.000000000000000000 ) ) ;
#38042 = CARTESIAN_POINT ( 'NONE',  ( 45.92519079177113639, -38.14579169924610369, -60.69370282983792464 ) ) ;
#38043 = ORIENTED_EDGE ( 'NONE', *, *, #21679, .T. ) ;
#38044 = EDGE_CURVE ( 'NONE', #48450, #14522, #2997, .T. ) ;
#38045 = CARTESIAN_POINT ( 'NONE',  ( 88.13393739769620083, -15.61618894467929941, -65.65000000000000568 ) ) ;
#38046 = CARTESIAN_POINT ( 'NONE',  ( 22.48979959896199787, -19.50330992088589710, -48.40737475858179550 ) ) ;
#38047 = CARTESIAN_POINT ( 'NONE',  ( 52.84346301666479917, -49.69122173838940881, -48.96941052353699320 ) ) ;
#38048 = CARTESIAN_POINT ( 'NONE',  ( 9.780793637630969428, -12.57087751220609917, -32.14999999999999858 ) ) ;
#38049 = EDGE_CURVE ( 'NONE', #14401, #12539, #31012, .T. ) ;
#38050 = VECTOR ( 'NONE', #7130, 1000.000000000000114 ) ;
#38051 = CARTESIAN_POINT ( 'NONE',  ( 14.34420549403320067, 19.88381105676229765, -74.14994299942661371 ) ) ;
#38052 = DIRECTION ( 'NONE',  ( 1.000000000000000000, 0.000000000000000000, 0.000000000000000000 ) ) ;
#38053 = CARTESIAN_POINT ( 'NONE',  ( 41.00663092279180688, -45.00381178176490238, -5.555598286907029504 ) ) ;
#38054 = CARTESIAN_POINT ( 'NONE',  ( 15.84222111805427424, -7.629322965617999053, -60.99577838100516658 ) ) ;
#38055 = CARTESIAN_POINT ( 'NONE',  ( 22.07021184574940165, -9.894006984415741002, -65.26351318459300899 ) ) ;
#38056 = ORIENTED_EDGE ( 'NONE', *, *, #3385, .F. ) ;
#38057 = CARTESIAN_POINT ( 'NONE',  ( 53.19504529726539488, -49.21163053193929926, -27.08660439529860042 ) ) ;
#38058 = CARTESIAN_POINT ( 'NONE',  ( 53.90939472220419759, -50.74970086946049719, -76.32822664810839797 ) ) ;
#38060 = CARTESIAN_POINT ( 'NONE',  ( 41.91337957294418004, -39.75513214800343320, -76.74976791096347029 ) ) ;
#38059 = CARTESIAN_POINT ( 'NONE',  ( 2.774641425251900273, 25.39332573679260108, -11.69510809164579968 ) ) ;
#38061 = CARTESIAN_POINT ( 'NONE',  ( 8.133937397696209715, 31.88305279702909800, -43.74348518090240390 ) ) ;
#38062 = ORIENTED_EDGE ( 'NONE', *, *, #41819, .T. ) ;
#38063 =( BOUNDED_CURVE ( )  B_SPLINE_CURVE ( 2, ( #8738, #5075, #13206 ),
 .UNSPECIFIED., .F., .T. ) 
 B_SPLINE_CURVE_WITH_KNOTS ( ( 3, 3 ),
 ( 0.09013492862022640106, 2.097321517346030006 ),
 .UNSPECIFIED. ) 
 CURVE ( )  GEOMETRIC_REPRESENTATION_ITEM ( )  RATIONAL_B_SPLINE_CURVE ( ( 1.000760683868189949, 1.008873536167329998, 1.001092624574940082 ) ) 
 REPRESENTATION_ITEM ( '' )  );
#38064 = CARTESIAN_POINT ( 'NONE',  ( -3.974232546700849689, -47.86947640837310303, -4.409288521898479196 ) ) ;
#38065 = CARTESIAN_POINT ( 'NONE',  ( 47.56368033297190578, 23.31135455392519873, -54.70077872531200569 ) ) ;
#38066 = CARTESIAN_POINT ( 'NONE',  ( 17.92370450342619748, 19.88381105532299742, -15.67980087199299888 ) ) ;
#38067 = CARTESIAN_POINT ( 'NONE',  ( 63.19469565515579745, 1.000225705806889964, -62.25573873525459589 ) ) ;
#38068 = CARTESIAN_POINT ( 'NONE',  ( 61.04011654556379796, 14.12690480185519881, -46.86308378909100014 ) ) ;
#38069 = CARTESIAN_POINT ( 'NONE',  ( 11.57222021527569922, 33.85198765799319887, -16.73996640652449841 ) ) ;
#38070 = CARTESIAN_POINT ( 'NONE',  ( 51.62358001281780417, 17.38380888595600027, -76.93789421597429623 ) ) ;
#38071 = CARTESIAN_POINT ( 'NONE',  ( 53.39111139338680090, 18.13443291158960236, -48.76214190021520523 ) ) ;
#38072 = CARTESIAN_POINT ( 'NONE',  ( 19.53299984191638927, 24.23912880602019726, -75.56421462368636810 ) ) ;
#38073 = CARTESIAN_POINT ( 'NONE',  ( 57.08416941684100010, -47.57703361919330121, -48.31006120114819424 ) ) ;
#38074 = CARTESIAN_POINT ( 'NONE',  ( 54.06609827824310344, 17.30031468964149965, -26.91176089519509773 ) ) ;
#38075 = CARTESIAN_POINT ( 'NONE',  ( 56.10252019742019769, 19.69840917465210239, -53.89291062504800323 ) ) ;
#38076 = CARTESIAN_POINT ( 'NONE',  ( 63.47791868668480220, 1.368314977562110180, -68.96521306187010225 ) ) ;
#38077 = DIRECTION ( 'NONE',  ( 0.6911981449639433839, -0.7226652920947592706, -1.665334536937735550E-16 ) ) ;
#38078 = DIRECTION ( 'NONE',  ( 0.000000000000000000, 0.000000000000000000, 1.000000000000000000 ) ) ;
#38079 = CARTESIAN_POINT ( 'NONE',  ( 19.21228758657862912, 21.54155451009319933, -16.16996892446439205 ) ) ;
#38080 = CARTESIAN_POINT ( 'NONE',  ( 11.10535879386450198, 31.92573324508259702, -44.25018954536789551 ) ) ;
#38081 = CARTESIAN_POINT ( 'NONE',  ( 72.76912858252920557, 1.370387345318210048, -62.28683037558460001 ) ) ;
#38082 = ADVANCED_FACE ( 'NONE', ( #12152 ), #31777, .T. ) ;
#38083 = CARTESIAN_POINT ( 'NONE',  ( 66.48974184299869705, -31.33002686145149696, -17.32440450352510197 ) ) ;
#38084 = CARTESIAN_POINT ( 'NONE',  ( 19.76827833599991990, -21.66053548658283034, -47.17485964264358955 ) ) ;
#38085 = ORIENTED_EDGE ( 'NONE', *, *, #30435, .T. ) ;
#38086 = EDGE_CURVE ( 'NONE', #49444, #37399, #19731, .T. ) ;
#38087 = ORIENTED_EDGE ( 'NONE', *, *, #24917, .F. ) ;
#38088 = CARTESIAN_POINT ( 'NONE',  ( 8.428888757039553425, -17.68705536023493607, -80.42433531602081587 ) ) ;
#38089 = CARTESIAN_POINT ( 'NONE',  ( 76.49475450406279720, -3.230546176492170130, -13.20481461287775460 ) ) ;
#38090 = VERTEX_POINT ( 'NONE', #44113 ) ;
#38091 = CARTESIAN_POINT ( 'NONE',  ( 12.88931624166749934, -65.50825287758750903, -47.54166358398200032 ) ) ;
#38092 = CARTESIAN_POINT ( 'NONE',  ( 57.05606732091469979, -45.81799886118620435, -26.22800298916919814 ) ) ;
#38093 = DIRECTION ( 'NONE',  ( 0.000000000000000000, -1.000000000000000000, 0.000000000000000000 ) ) ;
#38094 = ADVANCED_FACE ( 'NONE', ( #32282 ), #15132, .T. ) ;
#38095 = CARTESIAN_POINT ( 'NONE',  ( 20.99564406849854237, -9.290046565741832296, -63.21600299103990750 ) ) ;
#38096 = CARTESIAN_POINT ( 'NONE',  ( 16.97276188636949712, 12.56821928479469896, -59.64999999999999147 ) ) ;
#38097 = EDGE_LOOP ( 'NONE', ( #34156, #46285 ) ) ;
#38098 = DIRECTION ( 'NONE',  ( -1.000000000000000000, 0.000000000000000000, 0.000000000000000000 ) ) ;
#38099 = B_SPLINE_CURVE_WITH_KNOTS ( 'NONE', 3,
 ( #2047, #17770, #33740, #30060, #45560, #38210, #25359, #46090, #26388, #49755, #41361, #2571, #1532, #13846, #5476, #50272, #6502, #29803 ),
 .UNSPECIFIED., .F., .F.,
 ( 4, 2, 2, 2, 2, 2, 2, 2, 4 ),
 ( 0.5000015730941113068, 0.5625013764573473241, 0.6250011798205833413, 0.6875009831838194696, 0.7500007865470554869, 0.8125005899102915041, 0.8750003932735277434, 0.9375001966367638717, 1.000000000000000000 ),
 .UNSPECIFIED. ) ;
#38101 = CARTESIAN_POINT ( 'NONE',  ( 45.54888968018341444, 6.872726959284684689, -62.57519952278095587 ) ) ;
#38100 = AXIS2_PLACEMENT_3D ( 'NONE', #2628, #50327, #18600 ) ;
#38102 = ORIENTED_EDGE ( 'NONE', *, *, #874, .F. ) ;
#38103 = CARTESIAN_POINT ( 'NONE',  ( 54.53726787685040023, -46.02702818155930231, -15.67786106914689803 ) ) ;
#38104 = CARTESIAN_POINT ( 'NONE',  ( 12.90691782988471559, -22.86298708769336585, -34.42568375498250788 ) ) ;
#38105 = CARTESIAN_POINT ( 'NONE',  ( 14.72196958650020093, 19.87258839401659927, -22.05098504493599876 ) ) ;
#38106 = DIRECTION ( 'NONE',  ( -0.8732394366197193669, -0.4872913772396092469, 0.000000000000000000 ) ) ;
#38107 = CARTESIAN_POINT ( 'NONE',  ( 66.70013194292150160, -1.463538230407920082, -17.02746303015019791 ) ) ;
#38108 = CARTESIAN_POINT ( 'NONE',  ( 47.18324198357279897, -54.80726809202429450, -74.14999999999999147 ) ) ;
#38109 = CARTESIAN_POINT ( 'NONE',  ( 41.51080288407340646, 13.17508010173299837, -4.911631759730330060 ) ) ;
#38110 = EDGE_CURVE ( 'NONE', #16597, #24679, #8406, .T. ) ;
#38111 = CARTESIAN_POINT ( 'NONE',  ( 7.853097003783780394, -60.52042854835909935, -20.86915960608759946 ) ) ;
#38112 = VECTOR ( 'NONE', #47717, 1000.000000000000000 ) ;
#38113 = CARTESIAN_POINT ( 'NONE',  ( 14.18536260820854800, 10.43523626583284347, -34.89146800830132378 ) ) ;
#38114 = CARTESIAN_POINT ( 'NONE',  ( 53.43416147895619872, 19.95816927601739721, -75.78314185115898738 ) ) ;
#38115 = CARTESIAN_POINT ( 'NONE',  ( 59.18929318893719937, 14.08236763960739957, -26.39549450433730371 ) ) ;
#38116 = CARTESIAN_POINT ( 'NONE',  ( 13.52842820780809951, -23.01876079806860176, -67.89523180023219595 ) ) ;
#38117 = B_SPLINE_SURFACE_WITH_KNOTS ( 'NONE', 3, 3, ( 
 ( #38866, #34645, #14230, #6895, #45950, #21818, #18157, #18925, #15000 ),
 ( #46738, #18411, #50908, #17897, #26784, #45688, #6370, #38608, #46219 ),
 ( #30456, #1920, #38081, #10565, #10306, #42799, #6627, #22332, #50399 ),
 ( #33870, #18672, #26005, #38338, #2698, #49881, #13976, #2427, #14486 ),
 ( #29933, #30716, #42015, #6117, #26522, #16034, #19447, #31729, #3734 ),
 ( #35432, #31224, #15525, #19705, #30968, #15775, #12109, #51681, #31477 ),
 ( #40137, #15268, #39888, #51174, #47250, #47501, #47755, #11862, #35697 ),
 ( #24117, #28066, #7151, #35167, #43566, #11340, #3215, #27817, #3476 ),
 ( #7667, #46999, #27304, #27051, #11083, #43055, #44070, #11599, #43817 ),
 ( #43312, #7916, #27558, #31990, #39631, #7404, #23351, #23866, #23610 ),
 ( #35939, #3987, #48011, #39375, #23103, #4233, #19186, #51429, #39121 ),
 ( #20207, #19950, #8173, #36194, #60, #305, #36708, #49052, #1078 ),
 ( #44584, #17077, #24640, #49312, #29108, #40653, #20983, #48784, #41426 ),
 ( #32759, #33027, #13407, #8689, #25166, #41173, #553, #20457, #5020 ),
 ( #8955, #40394, #1343, #29366, #17333, #4751, #33296, #45107, #20718 ),
 ( #21235, #36981, #37245, #45371, #13158, #9213, #5284, #9476, #48263 ),
 ( #25423, #5543, #21498, #28322, #16539, #37498, #12624, #810, #16286 ),
 ( #32240, #16810, #12358, #32492, #44850, #44323, #8433, #48519, #12892 ),
 ( #24379, #4489, #28847, #24897, #40910, #36447, #28584, #23486, #18548 ),
 ( #3351, #38474, #19325, #34525, #30590, #42930, #10697, #6771, #39249 ) ),
 .UNSPECIFIED., .F., .F., .F.,
 ( 4, 2, 2, 2, 2, 2, 2, 2, 2, 4 ),
 ( 4, 1, 1, 1, 1, 1, 4 ),
 ( -1.826192301619909975, -1.664708266391559999, -1.413116924483460046, -1.141370188512440098, -0.9130961508099539881, -0.7989591319587090457, -0.6163399017967190474, -0.3681920442862079978, -0.1161770321749559937, 0.000000000000000000 ),
 ( 0.000000000000000000, 0.1666666666666670182, 0.3333333333333329818, 0.5000000000000000000, 0.6666666666666670737, 0.8333333333333330373, 1.000000000000000000 ),
 .UNSPECIFIED. ) ;
#38118 = ORIENTED_EDGE ( 'NONE', *, *, #26717, .F. ) ;
#38119 = CARTESIAN_POINT ( 'NONE',  ( 18.11900864776900022, 1.362847559348050019, -35.02873218748179340 ) ) ;
#38120 = AXIS2_PLACEMENT_3D ( 'NONE', #23139, #7439, #11896 ) ;
#38121 = CARTESIAN_POINT ( 'NONE',  ( -3.382504787385450129, -49.25282957014520235, -5.960458118589759380 ) ) ;
#38122 = DIRECTION ( 'NONE',  ( 0.000000000000000000, 0.000000000000000000, 1.000000000000000000 ) ) ;
#38123 = CARTESIAN_POINT ( 'NONE',  ( 72.89119224076110015, 1.045341414532760194, -69.29500968820069318 ) ) ;
#38124 = CARTESIAN_POINT ( 'NONE',  ( 61.14249685063511208, -45.50505420239858978, -47.52526588987043255 ) ) ;
#38125 = CARTESIAN_POINT ( 'NONE',  ( 3.892469389394927148, -22.68380379454831086, -34.70142521051216988 ) ) ;
#38126 = CARTESIAN_POINT ( 'NONE',  ( 23.46945290812993079, -12.58981197008611375, -65.38307690060923960 ) ) ;
#38127 = CARTESIAN_POINT ( 'NONE',  ( 40.87221884731469856, 13.29834217954369890, -4.420649500702079848 ) ) ;
#38128 = CARTESIAN_POINT ( 'NONE',  ( 9.543049929519856533, -17.38738464657387794, -79.36948662140328281 ) ) ;
#38129 = DIRECTION ( 'NONE',  ( 0.000000000000000000, 1.000000000000000000, 0.000000000000000000 ) ) ;
#38130 = CARTESIAN_POINT ( 'NONE',  ( 20.99557285898455206, -21.94238817380684026, -56.08401504527179782 ) ) ;
#38131 = CARTESIAN_POINT ( 'NONE',  ( 8.784728771152170879, -54.93525725209899235, -46.67204636145419983 ) ) ;
#38132 = CARTESIAN_POINT ( 'NONE',  ( -18.86606260230390220, 13.88381105532060289, 16.85000000000000142 ) ) ;
#38133 = ORIENTED_EDGE ( 'NONE', *, *, #27334, .T. ) ;
#38134 = CARTESIAN_POINT ( 'NONE',  ( 15.13944710363159984, -8.232579841174930024, -54.52472634102049653 ) ) ;
#38135 = CARTESIAN_POINT ( 'NONE',  ( 63.76776162078119370, 1.195685806282509978, -61.57371279390859797 ) ) ;
#38136 = VERTEX_POINT ( 'NONE', #50890 ) ;
#38137 = CARTESIAN_POINT ( 'NONE',  ( 21.54529026121558744, -19.77481651483016023, -68.66115164695051476 ) ) ;
#38138 = CARTESIAN_POINT ( 'NONE',  ( 60.91959772890210445, -45.69583638042100660, -47.74153617882520706 ) ) ;
#38139 = DIRECTION ( 'NONE',  ( 1.000000000000000000, 0.000000000000000000, 0.000000000000000000 ) ) ;
#38140 = CARTESIAN_POINT ( 'NONE',  ( 16.52003647484010429, -23.51837224676972582, -61.99213453326030532 ) ) ;
#38142 = CARTESIAN_POINT ( 'NONE',  ( 22.90067702240739322, -15.61618873416334807, -54.84718332859007006 ) ) ;
#38141 = CARTESIAN_POINT ( 'NONE',  ( 43.19653520511483435, 8.652243319877685579, -70.54837756005113647 ) ) ;
#38143 = CIRCLE ( 'NONE', #21359, 2.576499999999998902 ) ;
#38144 = CARTESIAN_POINT ( 'NONE',  ( 10.46343333517600094, -19.39436818664529838, -81.23899999999999011 ) ) ;
#38145 = CARTESIAN_POINT ( 'NONE',  ( 52.10267382257649871, -33.11618894464340457, -77.60820171200670359 ) ) ;
#38146 = ORIENTED_EDGE ( 'NONE', *, *, #14710, .F. ) ;
#38147 = AXIS2_PLACEMENT_3D ( 'NONE', #47796, #32029, #28106 ) ;
#38148 = ADVANCED_FACE ( 'NONE', ( #2408 ), #46720, .T. ) ;
#38149 = EDGE_LOOP ( 'NONE', ( #28440, #2772, #46804, #14824 ) ) ;
#38150 = VERTEX_POINT ( 'NONE', #50116 ) ;
#38151 = CARTESIAN_POINT ( 'NONE',  ( -22.70962239977677299, -19.05578711724787411, -54.67894118608715104 ) ) ;
#38152 = EDGE_CURVE ( 'NONE', #45666, #8993, #12130, .T. ) ;
#38153 = DIRECTION ( 'NONE',  ( 1.000000000000000000, 0.000000000000000000, 0.000000000000000000 ) ) ;
#38154 = ORIENTED_EDGE ( 'NONE', *, *, #27139, .F. ) ;
#38155 = EDGE_LOOP ( 'NONE', ( #32323, #17207, #29873, #6223 ) ) ;
#38156 = CARTESIAN_POINT ( 'NONE',  ( 22.81411286000173888, -16.71917825895734921, -72.50489804183278864 ) ) ;
#38157 = CARTESIAN_POINT ( 'NONE',  ( 17.01975655319769487, -22.38318595458896709, -52.91115215000503014 ) ) ;
#38158 = CARTESIAN_POINT ( 'NONE',  ( 17.01971462380884859, -8.849185945517076490, -53.99448858704194976 ) ) ;
#38159 = ORIENTED_EDGE ( 'NONE', *, *, #13028, .F. ) ;
#38160 = CARTESIAN_POINT ( 'NONE',  ( 24.04493704540187693, -15.61897246368578429, -49.50777781568486091 ) ) ;
#38161 = CARTESIAN_POINT ( 'NONE',  ( 52.63691518385540036, -50.41536572445579623, -76.75103203777939598 ) ) ;
#38162 = CARTESIAN_POINT ( 'NONE',  ( 60.90589200473370113, 14.20139306651049971, -47.09719146388230371 ) ) ;
#38163 = VECTOR ( 'NONE', #29294, 1000.000000000000000 ) ;
#38164 = CARTESIAN_POINT ( 'NONE',  ( 21.17919601613330016, -9.605189604746890097, -69.73476110523539262 ) ) ;
#38165 = EDGE_CURVE ( 'NONE', #10985, #12115, #26764, .T. ) ;
#38166 = AXIS2_PLACEMENT_3D ( 'NONE', #13953, #14981, #10283 ) ;
#38167 = CYLINDRICAL_SURFACE ( 'NONE', #34750, 0.4999999999999994449 ) ;
#38168 = CARTESIAN_POINT ( 'NONE',  ( 45.18671004937630187, 13.88808930430720068, -7.327102700430730309 ) ) ;
#38169 = EDGE_CURVE ( 'NONE', #51178, #44797, #48411, .T. ) ;
#38170 = CARTESIAN_POINT ( 'NONE',  ( 42.65512910181180217, -42.85913616512119972, -3.541891443463950129 ) ) ;
#38171 = CARTESIAN_POINT ( 'NONE',  ( 68.13393739769618662, 0.9838110553206419473, -65.65000000000000568 ) ) ;
#38172 = CARTESIAN_POINT ( 'NONE',  ( 29.52882095054619782, 20.46959749294990161, -75.56421356237308373 ) ) ;
#38173 = CARTESIAN_POINT ( 'NONE',  ( 64.52268999588739007, 1.145495783610749996, -70.39094822078129710 ) ) ;
#38174 = AXIS2_PLACEMENT_3D ( 'NONE', #1316, #17048, #4464 ) ;
#38175 = CARTESIAN_POINT ( 'NONE',  ( 46.78220155478780384, 8.502076674257970978, -54.45081220080809459 ) ) ;
#38176 = CARTESIAN_POINT ( 'NONE',  ( 16.13393739769620083, -3.616188944679339823, -22.14999999999999858 ) ) ;
#38177 = ORIENTED_EDGE ( 'NONE', *, *, #30685, .F. ) ;
#38178 = AXIS2_PLACEMENT_3D ( 'NONE', #50956, #11133, #3263 ) ;
#38179 = SURFACE_STYLE_FILL_AREA ( #34216 ) ;
#38180 = CARTESIAN_POINT ( 'NONE',  ( 47.18324198357289845, -54.80726809202429450, -54.61058319554170026 ) ) ;
#38181 = DIRECTION ( 'NONE',  ( 0.000000000000000000, 0.000000000000000000, -1.000000000000000000 ) ) ;
#38182 = DIRECTION ( 'NONE',  ( 0.000000000000000000, -1.000000000000000000, 0.000000000000000000 ) ) ;
#38183 = CARTESIAN_POINT ( 'NONE',  ( 0.3209249304026170480, -15.61618894467929941, -35.14999999999999858 ) ) ;
#38184 = CARTESIAN_POINT ( 'NONE',  ( 63.33772283987339335, 1.326578174762039986, -68.82808305222700085 ) ) ;
#38185 = CARTESIAN_POINT ( 'NONE',  ( 48.01492169973680291, -54.34163064677210286, -54.91800274540270266 ) ) ;
#38186 = CARTESIAN_POINT ( 'NONE',  ( 12.30690527417384494, -8.626895769526717217, -44.84843753875242811 ) ) ;
#38187 = MECHANICAL_DESIGN_GEOMETRIC_PRESENTATION_REPRESENTATION (  '', ( #33969 ), #49089 ) ;
#38188 = CARTESIAN_POINT ( 'NONE',  ( -10.44076364992884187, -42.78597905896825182, -5.977015743028451844 ) ) ;
#38189 = CARTESIAN_POINT ( 'NONE',  ( 47.98988913041800686, 23.14896199218459927, -55.12692082525529713 ) ) ;
#38190 = VERTEX_POINT ( 'NONE', #22571 ) ;
#38191 = CARTESIAN_POINT ( 'NONE',  ( 23.11815408353849577, -14.63472246044799796, -76.80273986043728485 ) ) ;
#38192 = ORIENTED_EDGE ( 'NONE', *, *, #50275, .T. ) ;
#38193 = CARTESIAN_POINT ( 'NONE',  ( 71.20900144662560649, 1.388715606738730068, -70.28003120372629553 ) ) ;
#38194 = CARTESIAN_POINT ( 'NONE',  ( 53.59003930803689997, -49.40628012469949937, -49.22510501142529904 ) ) ;
#38195 = DIRECTION ( 'NONE',  ( 1.000000000000000000, 0.000000000000000000, 0.000000000000000000 ) ) ;
#38196 = CARTESIAN_POINT ( 'NONE',  ( 14.70129771474999103, 19.30056145025122660, -20.74427287069836723 ) ) ;
#38198 = CARTESIAN_POINT ( 'NONE',  ( 55.06229968142930176, 15.76352112526989835, -25.67610890140170454 ) ) ;
#38197 = CARTESIAN_POINT ( 'NONE',  ( 84.27240597999899308, 12.65244516160949928, -47.25334685439979410 ) ) ;
#38199 = CARTESIAN_POINT ( 'NONE',  ( 13.25502815134339940, -22.05470121444239595, -75.08666063648169597 ) ) ;
#38200 = CARTESIAN_POINT ( 'NONE',  ( 68.13393739771727553, -29.66618894467940137, -49.64999999999999858 ) ) ;
#38201 = CARTESIAN_POINT ( 'NONE',  ( 71.42462519098069151, 0.8888742037077599356, -70.66714310028369539 ) ) ;
#38202 = CARTESIAN_POINT ( 'NONE',  ( 55.95579871441826469, -45.88748562638757988, -25.57470094210382427 ) ) ;
#38203 = ORIENTED_EDGE ( 'NONE', *, *, #21166, .T. ) ;
#38204 = CARTESIAN_POINT ( 'NONE',  ( 51.81838445030630425, -33.69149598205980567, -77.22003196546970116 ) ) ;
#38205 = ORIENTED_EDGE ( 'NONE', *, *, #19728, .T. ) ;
#38206 = ADVANCED_FACE ( 'NONE', ( #18653 ), #23059, .T. ) ;
#38207 = EDGE_LOOP ( 'NONE', ( #47885, #31651, #13534, #36711, #46346 ) ) ;
#38208 = CARTESIAN_POINT ( 'NONE',  ( 12.36320305068320025, -64.54682834576858852, -15.76422791927960176 ) ) ;
#38209 = CARTESIAN_POINT ( 'NONE',  ( 24.04493527958818078, -15.61020189840042427, -39.50743058786228801 ) ) ;
#38210 = CARTESIAN_POINT ( 'NONE',  ( 20.29259522008245042, -21.02751836791847495, -54.74448911140668628 ) ) ;
#38211 = CARTESIAN_POINT ( 'NONE',  ( 50.96898030287184156, 4.043820165196742700, -76.38408506549473032 ) ) ;
#38212 = ORIENTED_EDGE ( 'NONE', *, *, #41621, .F. ) ;
#38213 = ORIENTED_EDGE ( 'NONE', *, *, #11675, .F. ) ;
#38214 = CARTESIAN_POINT ( 'NONE',  ( 0.8822469062514919358, -51.51059052437120300, -34.40037443414259144 ) ) ;
#38215 = B_SPLINE_CURVE_WITH_KNOTS ( 'NONE', 3,
 ( #47281, #47027, #35722, #35969, #38897, #3508, #27845, #27335 ),
 .UNSPECIFIED., .F., .F.,
 ( 4, 2, 2, 4 ),
 ( 0.000000000000000000, 0.2515559781046747823, 0.3773339671570129505, 0.5031119562093512299 ),
 .UNSPECIFIED. ) ;
#38216 = FACE_OUTER_BOUND ( 'NONE', #38767, .T. ) ;
#38217 = CARTESIAN_POINT ( 'NONE',  ( 9.366383648607859769, -15.61614502978449970, -45.45282021618989177 ) ) ;
#38218 = CARTESIAN_POINT ( 'NONE',  ( 64.45807172334708923, -1.442643869120930011, -16.41040740274739917 ) ) ;
#38219 = B_SPLINE_CURVE_WITH_KNOTS ( 'NONE', 3,
 ( #34126, #37828, #46741, #41492, #41750, #50136, #14234, #1663, #21560, #6374 ),
 .UNSPECIFIED., .F., .F.,
 ( 4, 2, 2, 2, 4 ),
 ( 0.000000000000000000, 0.1250000005901855116, 0.2500000011803710231, 0.3750000017705565347, 0.5000000023607420463 ),
 .UNSPECIFIED. ) ;
#38220 = CARTESIAN_POINT ( 'NONE',  ( 51.18091049923690150, -50.74726768130989996, -76.16568857009508520 ) ) ;
#38221 = CARTESIAN_POINT ( 'NONE',  ( 58.58470796083329191, -48.16305383058679723, -50.30464788415889643 ) ) ;
#38222 = B_SPLINE_CURVE_WITH_KNOTS ( 'NONE', 3,
 ( #49626, #4808, #45683, #21553, #37821, #17646, #33612, #1914, #40711, #46475, #10818, #50130, #10036, #14226, #50904, #26263, #18667, #43051 ),
 .UNSPECIFIED., .F., .F.,
 ( 4, 2, 2, 2, 2, 2, 2, 2, 4 ),
 ( 0.000000000000000000, 0.03292124886954176516, 0.2434314436876863774, 0.3750003154490272328, 0.5000002523592219639, 0.5625002208143193849, 0.6625001703424752142, 0.8225000895875238527, 1.000000000000000000 ),
 .UNSPECIFIED. ) ;
#38223 = ORIENTED_EDGE ( 'NONE', *, *, #9627, .F. ) ;
#38224 = CARTESIAN_POINT ( 'NONE',  ( 72.38393739883420608, 11.88381105532070414, -61.44999999999999574 ) ) ;
#38225 = CARTESIAN_POINT ( 'NONE',  ( 65.43042069958036677, 17.98087126525108914, -68.79648330188406646 ) ) ;
#38226 = ORIENTED_EDGE ( 'NONE', *, *, #43795, .F. ) ;
#38227 = CARTESIAN_POINT ( 'NONE',  ( 53.70552627772385534, -51.31509389902640095, -75.56421117895261830 ) ) ;
#38228 = CARTESIAN_POINT ( 'NONE',  ( 48.26658354477700641, -45.11618894467940066, -9.084211283567670492 ) ) ;
#38229 = CARTESIAN_POINT ( 'NONE',  ( 20.49355919092259981, -22.14155831442439748, -42.32501095722299311 ) ) ;
#38230 = CARTESIAN_POINT ( 'NONE',  ( 13.09773310522899870, -50.91350717092480238, -21.58185367788340159 ) ) ;
#38231 = AXIS2_PLACEMENT_3D ( 'NONE', #30241, #46262, #10348 ) ;
#38232 = CARTESIAN_POINT ( 'NONE',  ( 54.08446768638849989, 19.51091414381249578, -76.27847822918199938 ) ) ;
#38233 = EDGE_CURVE ( 'NONE', #33614, #25343, #47572, .T. ) ;
#38234 = CARTESIAN_POINT ( 'NONE',  ( 47.27618702399809791, -54.10032693455720221, -75.52157719890121257 ) ) ;
#38235 = CARTESIAN_POINT ( 'NONE',  ( 55.91593866523759715, 14.67229690674569831, -17.93020249829309876 ) ) ;
#38236 = CARTESIAN_POINT ( 'NONE',  ( 68.13393739769620083, 1.383811055320669947, -60.14999999999999858 ) ) ;
#38237 = CARTESIAN_POINT ( 'NONE',  ( 56.53399784783299964, -50.44739419118339896, -52.81205167950179913 ) ) ;
#38238 = CARTESIAN_POINT ( 'NONE',  ( 14.27580295341549999, -22.41985674678640095, -45.43204315924410253 ) ) ;
#38239 = FACE_OUTER_BOUND ( 'NONE', #23723, .T. ) ;
#38240 = ORIENTED_EDGE ( 'NONE', *, *, #21437, .T. ) ;
#38241 = CARTESIAN_POINT ( 'NONE',  ( 46.35275103504439898, 21.67755452994670406, -76.14999999999999147 ) ) ;
#38242 = CARTESIAN_POINT ( 'NONE',  ( 64.97847163984020824, 0.9947083095259759977, -60.55634004142090276 ) ) ;
#38243 = DIRECTION ( 'NONE',  ( 1.000000000000000000, 2.460964292799963328E-14, 0.000000000000000000 ) ) ;
#38244 = CARTESIAN_POINT ( 'NONE',  ( 68.13393739769658453, -28.80002732851960445, -29.09832030244560741 ) ) ;
#38245 = DIRECTION ( 'NONE',  ( 0.000000000000000000, -0.7371541403039566509, 0.6757246284047478957 ) ) ;
#38246 = CIRCLE ( 'NONE', #9790, 17.70000000000000284 ) ;
#38247 = CARTESIAN_POINT ( 'NONE',  ( 16.13393739769309931, -15.61618894467859953, -3.187564294432039702 ) ) ;
#38248 = CARTESIAN_POINT ( 'NONE',  ( 82.55668469584230706, 14.40343100263957865, -47.71685812434790108 ) ) ;
#38249 = CARTESIAN_POINT ( 'NONE',  ( -15.91219141626359956, 7.039674273257229942, -48.73593760451629464 ) ) ;
#38251 = CARTESIAN_POINT ( 'NONE',  ( 41.63730079839010045, -38.78348554106982249, -82.15224707392265202 ) ) ;
#38250 = CARTESIAN_POINT ( 'NONE',  ( 8.133937397696215044, 28.62669279778661036, -21.14999999999999858 ) ) ;
#38252 = CARTESIAN_POINT ( 'NONE',  ( 10.83871905795021284, -21.53117133270660943, -32.52469633233020119 ) ) ;
#38253 = PRODUCT_DEFINITION ( 'UNKNOWN', '', #12651, #48890 ) ;
#38254 = CARTESIAN_POINT ( 'NONE',  ( -32.24202920327260102, -6.110563815214810290, -55.86711240520629929 ) ) ;
#38255 = EDGE_LOOP ( 'NONE', ( #19782, #38531, #47169, #9549, #2617, #50799, #5291 ) ) ;
#38256 = CARTESIAN_POINT ( 'NONE',  ( 53.14225961112249763, -49.51472671965699845, -48.98057208336989987 ) ) ;
#38257 = ORIENTED_EDGE ( 'NONE', *, *, #43141, .F. ) ;
#38258 = LINE ( 'NONE', #26968, #12807 ) ;
#38259 = CARTESIAN_POINT ( 'NONE',  ( 9.366959348133711671, -14.73023002513620128, -41.49448685887290367 ) ) ;
#38260 = CARTESIAN_POINT ( 'NONE',  ( 14.01770721255530106, 19.93736976191020105, -22.72048054942820272 ) ) ;
#38261 = CARTESIAN_POINT ( 'NONE',  ( 55.85837259913330399, 14.77764870892549887, -25.54560217317060022 ) ) ;
#38262 = CARTESIAN_POINT ( 'NONE',  ( 23.04447129454539933, -14.20655070842010126, -40.38876883061639234 ) ) ;
#38263 = CYLINDRICAL_SURFACE ( 'NONE', #14870, 0.9999999999999976685 ) ;
#38264 = CARTESIAN_POINT ( 'NONE',  ( 53.03054970849530037, 18.35345454141090116, -49.02174585020699737 ) ) ;
#38265 = CARTESIAN_POINT ( 'NONE',  ( 55.81704914353240099, -45.86755745118960448, -17.13878629476699800 ) ) ;
#38266 = DIRECTION ( 'NONE',  ( 0.000000000000000000, 0.000000000000000000, -1.000000000000000000 ) ) ;
#38267 = ORIENTED_EDGE ( 'NONE', *, *, #5975, .F. ) ;
#38268 = EDGE_CURVE ( 'NONE', #17159, #15981, #28951, .T. ) ;
#38269 = CARTESIAN_POINT ( 'NONE',  ( 9.489348988027188625, -19.79185572368299972, -38.10891372031139213 ) ) ;
#38270 = EDGE_CURVE ( 'NONE', #1146, #22337, #9750, .T. ) ;
#38271 = CARTESIAN_POINT ( 'NONE',  ( 73.01625195241490474, 1.007912009470880221, -69.12629645913949616 ) ) ;
#38272 = CARTESIAN_POINT ( 'NONE',  ( 24.04491681007057480, -15.59668230724852300, -49.79154587196198634 ) ) ;
#38273 = CARTESIAN_POINT ( 'NONE',  ( 73.16133767175010405, 0.8879664753683469414, -62.37500410124779648 ) ) ;
#38274 = CARTESIAN_POINT ( 'NONE',  ( 11.93174526809839975, -65.43929183185349530, -17.93019253464870033 ) ) ;
#38275 = B_SPLINE_CURVE_WITH_KNOTS ( 'NONE', 3,
 ( #5595, #21811, #29158, #17126, #29923 ),
 .UNSPECIFIED., .F., .F.,
 ( 4, 1, 4 ),
 ( 0.5000152864445784884, 0.6666870483743799758, 1.000000000000000000 ),
 .UNSPECIFIED. ) ;
#38277 = EDGE_CURVE ( 'NONE', #48161, #24229, #48236, .T. ) ;
#38276 = CARTESIAN_POINT ( 'NONE',  ( 52.74562315164475734, -49.73950520563583666, -48.86764759941514313 ) ) ;
#38278 = CYLINDRICAL_SURFACE ( 'NONE', #41719, 1.999999999999995115 ) ;
#38279 = CARTESIAN_POINT ( 'NONE',  ( 22.90093587091927319, -15.61081685778595762, -62.45257565318340909 ) ) ;
#38280 = CARTESIAN_POINT ( 'NONE',  ( 20.29261247985267502, -10.20487329796221054, -58.16115334902455203 ) ) ;
#38281 = EDGE_CURVE ( 'NONE', #15666, #40171, #6395, .T. ) ;
#38282 = CARTESIAN_POINT ( 'NONE',  ( 64.79174514991450451, 0.8925687589132640376, -70.63296852923039637 ) ) ;
#38283 = ORIENTED_EDGE ( 'NONE', *, *, #8638, .T. ) ;
#38284 = CARTESIAN_POINT ( 'NONE',  ( 10.76970654631240087, -63.14946393425128690, -45.20602416875770047 ) ) ;
#38285 = CARTESIAN_POINT ( 'NONE',  ( 20.11809584606473678, -8.703681988134835734, -47.45899950725307548 ) ) ;
#38286 = ORIENTED_EDGE ( 'NONE', *, *, #23589, .T. ) ;
#38287 = CARTESIAN_POINT ( 'NONE',  ( 16.13393739769620083, -15.61618894467929941, -34.64999999999999858 ) ) ;
#38288 = CARTESIAN_POINT ( 'NONE',  ( 56.94695452114130063, 19.24930104416129950, -53.05466020597059895 ) ) ;
#38289 = CARTESIAN_POINT ( 'NONE',  ( 52.84793103446079954, 19.11984488519809844, -76.98160984307151011 ) ) ;
#38290 = ORIENTED_EDGE ( 'NONE', *, *, #10118, .F. ) ;
#38291 = DIRECTION ( 'NONE',  ( 1.000000000000000000, 0.000000000000000000, 0.000000000000000000 ) ) ;
#38292 = CARTESIAN_POINT ( 'NONE',  ( 23.06214062797170072, -3.616188944679339823, -32.14999999999999858 ) ) ;
#38293 = CARTESIAN_POINT ( 'NONE',  ( 22.89127052530449546, -15.22560942949823470, -72.43445116809684237 ) ) ;
#38294 = CIRCLE ( 'NONE', #41644, 0.5000000000000004441 ) ;
#38295 = CARTESIAN_POINT ( 'NONE',  ( 8.643744238043529649, 17.52287609088129727, -35.14999999999999858 ) ) ;
#38296 = CARTESIAN_POINT ( 'NONE',  ( 12.29178504908659875, -8.320944919562059283, -67.13803027067569928 ) ) ;
#38297 = DIRECTION ( 'NONE',  ( 0.000000000000000000, 0.000000000000000000, -1.000000000000000000 ) ) ;
#38298 = CARTESIAN_POINT ( 'NONE',  ( 43.48544627107390426, -37.84702645128613341, -72.89241229296673907 ) ) ;
#38299 = ADVANCED_FACE ( 'NONE', ( #46808 ), #48334, .T. ) ;
#38300 = ORIENTED_EDGE ( 'NONE', *, *, #51108, .F. ) ;
#38301 = CARTESIAN_POINT ( 'NONE',  ( 56.68830530524120093, -46.09563615325990327, -26.25268044571639692 ) ) ;
#38302 = CARTESIAN_POINT ( 'NONE',  ( 21.83716472214950244, -10.82245429508140155, -40.01016806583820085 ) ) ;
#38303 = CARTESIAN_POINT ( 'NONE',  ( 8.886432599889248607, -17.14058911653749817, -32.14999999999999858 ) ) ;
#38304 = CARTESIAN_POINT ( 'NONE',  ( 24.04493739769619864, -15.61618894467929941, -32.14999999999999858 ) ) ;
#38305 = CARTESIAN_POINT ( 'NONE',  ( 13.44492653017840134, 20.50885532556510071, -74.53071772762450564 ) ) ;
#38306 = DIRECTION ( 'NONE',  ( 0.000000000000000000, 0.7371541402007432131, -0.6757246285173443834 ) ) ;
#38307 = CARTESIAN_POINT ( 'NONE',  ( 41.11636499574930070, -44.91157709887249894, -5.497152887732390525 ) ) ;
#38308 = PLANE ( 'NONE',  #9736 ) ;
#38309 = EDGE_CURVE ( 'NONE', #7609, #32627, #44401, .T. ) ;
#38310 = CARTESIAN_POINT ( 'NONE',  ( 20.89934259796100235, -8.887620450098559388, -63.20382097693880041 ) ) ;
#38311 = VERTEX_POINT ( 'NONE', #36783 ) ;
#38312 = CARTESIAN_POINT ( 'NONE',  ( 55.92359621412080628, -45.89461707380959865, -25.40852082268940038 ) ) ;
#38313 = B_SPLINE_CURVE_WITH_KNOTS ( 'NONE', 3,
 ( #42613, #22920, #38686, #6707, #18746, #23690, #23174, #43384, #11418, #47578, #15079, #3808, #51502, #7742, #30785, #39192, #42872, #15603 ),
 .UNSPECIFIED., .F., .F.,
 ( 4, 2, 2, 2, 2, 2, 2, 2, 4 ),
 ( 0.000000000000000000, 0.06249962094764476006, 0.1249992418952895201, 0.1874988628429342663, 0.2499984837905790402, 0.3124981047382238142, 0.3749977256858685326, 0.4374973466335133065, 0.4999969675811580805 ),
 .UNSPECIFIED. ) ;
#38314 = CARTESIAN_POINT ( 'NONE',  ( 56.61426160987299738, -50.70378515394530439, -74.49626132433751025 ) ) ;
#38316 = CARTESIAN_POINT ( 'NONE',  ( 41.47164856782293185, -39.70574416324859612, -78.88105259561210403 ) ) ;
#38315 = CARTESIAN_POINT ( 'NONE',  ( 65.03253056770502383, 12.18167892300241206, -10.43310554112815325 ) ) ;
#38317 = CARTESIAN_POINT ( 'NONE',  ( 47.46364465723310389, -54.60385569402070161, -54.65913311076389647 ) ) ;
#38318 = CARTESIAN_POINT ( 'NONE',  ( 25.03312433582057750, -22.08182671989646906, -84.65000000000000568 ) ) ;
#38319 = EDGE_LOOP ( 'NONE', ( #13164, #7017, #49274, #50108 ) ) ;
#38320 = CARTESIAN_POINT ( 'NONE',  ( 18.81513785123362936, -8.134968765430629745, -81.11711141586931717 ) ) ;
#38321 = CARTESIAN_POINT ( 'NONE',  ( 47.43221812499459844, 23.40624208892269920, -54.88095735414919574 ) ) ;
#38322 = CARTESIAN_POINT ( 'NONE',  ( 12.75708233038401751, -8.434022097740552226, -65.15251670430993158 ) ) ;
#38323 = CARTESIAN_POINT ( 'NONE',  ( 63.46279604660929863, 1.371509258145880095, -62.41110185547420031 ) ) ;
#38324 = CARTESIAN_POINT ( 'NONE',  ( 60.76016881783269952, 14.27357726001389970, -47.06493626314229317 ) ) ;
#38325 = CARTESIAN_POINT ( 'NONE',  ( 11.85902006005049891, 33.93748487951390302, -16.73665430628790318 ) ) ;
#38326 = CARTESIAN_POINT ( 'NONE',  ( 40.57649240635721100, -37.56081407618430035, -83.97002642401369599 ) ) ;
#38327 = CARTESIAN_POINT ( 'NONE',  ( 53.01963653383530328, 18.32905899852440257, -48.79855609391960058 ) ) ;
#38328 = FACE_OUTER_BOUND ( 'NONE', #24137, .T. ) ;
#38329 = CARTESIAN_POINT ( 'NONE',  ( 57.59186919487559919, -47.31111691810159670, -48.20254613966260138 ) ) ;
#38330 = CARTESIAN_POINT ( 'NONE',  ( 53.79192597912830109, 17.55350234038469992, -27.04907804900940249 ) ) ;
#38331 = VECTOR ( 'NONE', #29156, 1000.000000000000000 ) ;
#38332 = CARTESIAN_POINT ( 'NONE',  ( 51.58686502407429941, 21.60049488496320080, -54.30991078205589417 ) ) ;
#38333 = CARTESIAN_POINT ( 'NONE',  ( 63.64098798152370762, 1.412341182043239884, -69.17505041201758331 ) ) ;
#38334 = CARTESIAN_POINT ( 'NONE',  ( 52.90434486281380799, 18.43107897257790029, -49.01850765170799917 ) ) ;
#38335 = DIRECTION ( 'NONE',  ( 0.9146474252872274224, -0.000000000000000000, 0.4042525045258791860 ) ) ;
#38336 = CARTESIAN_POINT ( 'NONE',  ( 19.80165575756416985, 23.23087915573190543, -17.67623750364432311 ) ) ;
#38337 = CARTESIAN_POINT ( 'NONE',  ( 10.49236770985929823, 32.06433946733989870, -45.62571961304500689 ) ) ;
#38338 = CARTESIAN_POINT ( 'NONE',  ( 72.77037870541830955, 1.316034553466219892, -62.10038360666850110 ) ) ;
#38339 = DIRECTION ( 'NONE',  ( -0.3294064756442134922, -0.9441882088882800339, 8.551492847173810438E-14 ) ) ;
#38340 = EDGE_CURVE ( 'NONE', #40450, #5413, #45915, .T. ) ;
#38341 = EDGE_LOOP ( 'NONE', ( #25951, #23108, #4563, #31290, #49123 ) ) ;
#38342 = CARTESIAN_POINT ( 'NONE',  ( 10.38933687974308384, -19.70790301870552241, -47.65017322902551911 ) ) ;
#38343 = ORIENTED_EDGE ( 'NONE', *, *, #23800, .F. ) ;
#38344 = VERTEX_POINT ( 'NONE', #41244 ) ;
#38345 = CARTESIAN_POINT ( 'NONE',  ( 14.13393739769640156, 6.292713355527309815, -54.64999999999999858 ) ) ;
#38346 = CARTESIAN_POINT ( 'NONE',  ( 76.49467596410896419, -3.235303301204498272, -13.20447617252744621 ) ) ;
#38347 = ORIENTED_EDGE ( 'NONE', *, *, #39474, .T. ) ;
#38348 = CARTESIAN_POINT ( 'NONE',  ( 11.04919440717550039, -64.12845758586969680, -45.19200995724910541 ) ) ;
#38349 = CARTESIAN_POINT ( 'NONE',  ( 56.76310125540409501, -45.25731884260100202, -25.36477901628050091 ) ) ;
#38350 = CARTESIAN_POINT ( 'NONE',  ( 14.36266436798912771, -22.20705554833075013, -45.03617451210310918 ) ) ;
#38351 = CARTESIAN_POINT ( 'NONE',  ( 63.46757340380580814, 1.384887413063060180, -68.61455525072810246 ) ) ;
#38352 = EDGE_LOOP ( 'NONE', ( #24556, #12451, #47343, #33812 ) ) ;
#38353 = CARTESIAN_POINT ( 'NONE',  ( 44.13393739769620083, 4.883811055320659733, -35.14999999999999858 ) ) ;
#38354 = CARTESIAN_POINT ( 'NONE',  ( 46.55606098839130880, 6.976707678039790750, -57.53936765601046233 ) ) ;
#38355 = CARTESIAN_POINT ( 'NONE',  ( -17.22968739472086241, 4.597376488843254450, -50.03813090013385079 ) ) ;
#38356 = ORIENTED_EDGE ( 'NONE', *, *, #35559, .F. ) ;
#38357 = CARTESIAN_POINT ( 'NONE',  ( 21.79569638026020328, -9.937173318903379737, -31.54232391275619563 ) ) ;
#38358 = DIRECTION ( 'NONE',  ( 0.000000000000000000, 0.000000000000000000, -1.000000000000000000 ) ) ;
#38359 = CARTESIAN_POINT ( 'NONE',  ( 16.62868081655389929, 19.88381105408159755, -20.46561682067460097 ) ) ;
#38360 = CARTESIAN_POINT ( 'NONE',  ( 22.87052914506156398, -16.27176351700221346, -50.48368888301278901 ) ) ;
#38361 = EDGE_CURVE ( 'NONE', #30947, #29939, #25237, .T. ) ;
#38362 = CARTESIAN_POINT ( 'NONE',  ( 16.13734155123387026, -22.38318897308463917, -46.95266346626168286 ) ) ;
#38363 = DIRECTION ( 'NONE',  ( 0.3805321250008310008, 0.000000000000000000, -0.9247677015566404535 ) ) ;
#38364 = CARTESIAN_POINT ( 'NONE',  ( 47.22839619843820458, -54.42900472606909545, -75.17099345517469544 ) ) ;
#38365 = CARTESIAN_POINT ( 'NONE',  ( 60.78498736401110136, 13.10757611403960077, -9.606534188251758977 ) ) ;
#38366 = TOROIDAL_SURFACE ( 'NONE', #19932, 10.49999999968949815, 0.4999999999856510335 ) ;
#38367 = DIRECTION ( 'NONE',  ( 0.000000000000000000, -1.000000000000000000, 0.000000000000000000 ) ) ;
#38368 =( BOUNDED_CURVE ( )  B_SPLINE_CURVE ( 2, ( #5548, #36453, #12632 ),
 .UNSPECIFIED., .F., .T. ) 
 B_SPLINE_CURVE_WITH_KNOTS ( ( 3, 3 ),
 ( -0.06696923885014899325, 0.06696923885011449307 ),
 .UNSPECIFIED. ) 
 CURVE ( )  GEOMETRIC_REPRESENTATION_ITEM ( )  RATIONAL_B_SPLINE_CURVE ( ( 1.000000000000000000, 0.9977583984878120038, 1.000000000000000000 ) ) 
 REPRESENTATION_ITEM ( '' )  );
#38369 = CARTESIAN_POINT ( 'NONE',  ( 52.25623527804339830, 20.09621345565349770, -75.95837141101100087 ) ) ;
#38370 = CARTESIAN_POINT ( 'NONE',  ( 57.24929578595760660, -52.61618894467940066, -63.99406948319280275 ) ) ;
#38371 = ADVANCED_FACE ( 'NONE', ( #49385 ), #13481, .T. ) ;
#38372 = CARTESIAN_POINT ( 'NONE',  ( 24.34134549961779825, -14.82804368003519890, -35.47719510467199910 ) ) ;
#38373 = ORIENTED_EDGE ( 'NONE', *, *, #30807, .T. ) ;
#38375 = EDGE_CURVE ( 'NONE', #40090, #8235, #48468, .T. ) ;
#38374 = DIRECTION ( 'NONE',  ( -1.000000000000000000, 0.000000000000000000, 0.000000000000000000 ) ) ;
#38376 = CARTESIAN_POINT ( 'NONE',  ( 9.595232318844979957, -63.69675525222269385, -16.46787902471350051 ) ) ;
#38377 = CARTESIAN_POINT ( 'NONE',  ( 76.21567127096270156, -5.958767942511509652, -12.35740042236670000 ) ) ;
#38378 = CARTESIAN_POINT ( 'NONE',  ( 75.12459293833639151, 13.75682883240243370, -14.63710905661170081 ) ) ;
#38379 = CARTESIAN_POINT ( 'NONE',  ( 44.89330862275510725, -33.71195016353239993, -35.14497980672799571 ) ) ;
#38380 = CARTESIAN_POINT ( 'NONE',  ( 12.81875897587595503, -55.47848908301230608, -75.64152464218183525 ) ) ;
#38381 = DIRECTION ( 'NONE',  ( 0.000000000000000000, 1.000000000000000000, 0.000000000000000000 ) ) ;
#38382 = CARTESIAN_POINT ( 'NONE',  ( 61.75019796695539753, -45.11618894467940066, -28.15000000000000213 ) ) ;
#38383 = CARTESIAN_POINT ( 'NONE',  ( 16.13393739769620083, -15.61618894467929941, -22.14999999999999858 ) ) ;
#38384 = CARTESIAN_POINT ( 'NONE',  ( 40.75026669549949787, 13.34597472761970138, -4.220911263362750354 ) ) ;
#38385 = CARTESIAN_POINT ( 'NONE',  ( 11.96660005458869946, 10.88381105532060111, -34.64999999999999858 ) ) ;
#38386 = CARTESIAN_POINT ( 'NONE',  ( 7.492845759203685674, -61.18022026567161475, -20.13893727953967172 ) ) ;
#38387 = CARTESIAN_POINT ( 'NONE',  ( 66.23540447448809232, -49.95860450174330225, -73.25000000000169109 ) ) ;
#38388 = CARTESIAN_POINT ( 'NONE',  ( 76.39354817796227337, -43.26297082301523034, -13.95540116459575586 ) ) ;
#38389 = CARTESIAN_POINT ( 'NONE',  ( 16.13393739769620083, -1.590680505402594314, -34.79644660940672196 ) ) ;
#38390 = ORIENTED_EDGE ( 'NONE', *, *, #32427, .F. ) ;
#38391 = EDGE_CURVE ( 'NONE', #18174, #9837, #40677, .T. ) ;
#38392 = CARTESIAN_POINT ( 'NONE',  ( 19.61755955990300038, -9.030517303204650403, -50.72221764996669435 ) ) ;
#38393 = CARTESIAN_POINT ( 'NONE',  ( 63.53675997960419863, 1.374525224581449878, -62.20330014729499624 ) ) ;
#38394 = ORIENTED_EDGE ( 'NONE', *, *, #32206, .F. ) ;
#38395 = CARTESIAN_POINT ( 'NONE',  ( 10.61754762155600140, 33.59328422689429772, -18.17417937929459981 ) ) ;
#38396 = CARTESIAN_POINT ( 'NONE',  ( 60.97391253512209630, -45.68106840025299675, -47.73524043326649746 ) ) ;
#38397 = CARTESIAN_POINT ( 'NONE',  ( 8.643744238043529649, 17.52287609088129727, -35.14999999999999858 ) ) ;
#38398 = VECTOR ( 'NONE', #51759, 1000.000000000000000 ) ;
#38399 = CARTESIAN_POINT ( 'NONE',  ( 24.04481203031673076, -15.61619115162449312, -61.50767625960597229 ) ) ;
#38400 = CARTESIAN_POINT ( 'NONE',  ( 21.54530244994622379, -11.45757809935890137, -74.24448689220467656 ) ) ;
#38401 = CONICAL_SURFACE ( 'NONE', #12553, 36.50000000000000000, 0.1651486774146265213 ) ;
#38402 = CARTESIAN_POINT ( 'NONE',  ( 4.403190979259558269, -24.13907510292004233, -6.928362978644219794 ) ) ;
#38403 = CARTESIAN_POINT ( 'NONE',  ( 60.60294763170050203, -45.58832773382454207, -47.14361286069857471 ) ) ;
#38404 = ADVANCED_FACE ( 'NONE', ( #42287 ), #46752, .T. ) ;
#38405 = ORIENTED_EDGE ( 'NONE', *, *, #34876, .T. ) ;
#38406 = VERTEX_POINT ( 'NONE', #2709 ) ;
#38407 = ORIENTED_EDGE ( 'NONE', *, *, #50096, .F. ) ;
#38408 = CARTESIAN_POINT ( 'NONE',  ( 18.86789271228509790, -51.78678246903520233, -76.14999999999999147 ) ) ;
#38409 = CARTESIAN_POINT ( 'NONE',  ( 61.30390548032649889, -45.22107570635780860, -46.37197824241119548 ) ) ;
#38410 = DIRECTION ( 'NONE',  ( 0.000000000000000000, 1.000000000000000000, 0.000000000000000000 ) ) ;
#38411 = ORIENTED_EDGE ( 'NONE', *, *, #21980, .T. ) ;
#38412 = EDGE_LOOP ( 'NONE', ( #47331, #20282, #28253, #5214, #247, #31603 ) ) ;
#38413 = FACE_OUTER_BOUND ( 'NONE', #16852, .T. ) ;
#38414 = DIRECTION ( 'NONE',  ( 0.000000000000000000, 0.000000000000000000, -1.000000000000000000 ) ) ;
#38415 = ORIENTED_EDGE ( 'NONE', *, *, #7470, .T. ) ;
#38416 = B_SPLINE_CURVE_WITH_KNOTS ( 'NONE', 3,
 ( #31629, #43711, #200, #19851, #11754 ),
 .UNSPECIFIED., .F., .F.,
 ( 4, 1, 4 ),
 ( 0.000000000000000000, 0.3333267645415212144, 0.4999950733969018013 ),
 .UNSPECIFIED. ) ;
#38417 = CARTESIAN_POINT ( 'NONE',  ( 18.81810784640891399, -23.12961269479223603, -49.89815809426819015 ) ) ;
#38418 = CARTESIAN_POINT ( 'NONE',  ( 52.19402250454749748, -50.90613807397439672, -76.20338398719890449 ) ) ;
#38419 = CARTESIAN_POINT ( 'NONE',  ( 60.31836632494100314, 14.50504996450150053, -47.25075699645550742 ) ) ;
#38420 = CARTESIAN_POINT ( 'NONE',  ( 10.52882599906690153, -21.10886349454530375, -78.76571924648798984 ) ) ;
#38421 = CARTESIAN_POINT ( 'NONE',  ( 16.13393739769620083, -30.04994567442000175, -34.64999999999999858 ) ) ;
#38422 = CARTESIAN_POINT ( 'NONE',  ( 40.91145569068659427, 13.87671759085050027, -5.616194440429819856 ) ) ;
#38423 = CARTESIAN_POINT ( 'NONE',  ( 42.80229243920160087, -42.71639462152419497, -3.540423289868949830 ) ) ;
#38424 = CARTESIAN_POINT ( 'NONE',  ( 24.04493742325405137, -16.65172786793846882, -79.54933697072902987 ) ) ;
#38425 = FACE_OUTER_BOUND ( 'NONE', #37998, .T. ) ;
#38426 = CIRCLE ( 'NONE', #40108, 2.999999999999999112 ) ;
#38427 = CARTESIAN_POINT ( 'NONE',  ( 64.69570918563078976, 1.132579237369299996, -70.50812303354531707 ) ) ;
#38428 = CARTESIAN_POINT ( 'NONE',  ( 46.83318063571350365, 8.437011769841980424, -54.37544270859390139 ) ) ;
#38429 = AXIS2_PLACEMENT_3D ( 'NONE', #38287, #34330, #41693 ) ;
#38430 = SPHERICAL_SURFACE ( 'NONE', #29244, 2.000000000000000000 ) ;
#38431 = CARTESIAN_POINT ( 'NONE',  ( 8.537791930192160095, -13.64506687344660030, -52.36832131176279859 ) ) ;
#38432 = ORIENTED_EDGE ( 'NONE', *, *, #14892, .T. ) ;
#38434 = ADVANCED_FACE ( 'NONE', ( #22345 ), #15014, .T. ) ;
#38433 =( LENGTH_UNIT ( ) NAMED_UNIT ( * ) SI_UNIT ( .MILLI., .METRE. ) );
#38435 = CARTESIAN_POINT ( 'NONE',  ( 43.50059062573970436, 14.79387737681599901, -7.939643042942710061 ) ) ;
#38436 = CARTESIAN_POINT ( 'NONE',  ( 72.00712697859638922, 1.176186365484889862, -70.19198721960910348 ) ) ;
#38437 = EDGE_CURVE ( 'NONE', #17140, #41357, #43322, .T. ) ;
#38438 = CARTESIAN_POINT ( 'NONE',  ( 44.37302628842170549, -39.98451940133276850, -64.85227893969756963 ) ) ;
#38439 = DIRECTION ( 'NONE',  ( 0.6911981449639439390, -0.7226652920947588266, 0.000000000000000000 ) ) ;
#38440 = CARTESIAN_POINT ( 'NONE',  ( 22.00297652178539920, -11.84456943261250039, -32.14999999999999858 ) ) ;
#38441 = CARTESIAN_POINT ( 'NONE',  ( 63.21507766202849865, 1.186856010528209993, -68.92285061280580294 ) ) ;
#38442 = CARTESIAN_POINT ( 'NONE',  ( 47.82694498829380336, -54.45586656085379929, -55.20630169768750051 ) ) ;
#38443 = CARTESIAN_POINT ( 'NONE',  ( 24.04491913310489082, -15.59780088466810710, -45.50693619046535332 ) ) ;
#38444 = DIRECTION ( 'NONE',  ( -1.000000000000000000, 0.000000000000000000, 0.000000000000000000 ) ) ;
#38445 = CARTESIAN_POINT ( 'NONE',  ( 48.05894033739649984, 23.11179829524310136, -55.06192549311779771 ) ) ;
#38446 = VERTEX_POINT ( 'NONE', #38619 ) ;
#38447 = CARTESIAN_POINT ( 'NONE',  ( 22.48516629158629954, -12.54952123915529860, -78.70399420596410778 ) ) ;
#38448 = VERTEX_POINT ( 'NONE', #34657 ) ;
#38449 = CARTESIAN_POINT ( 'NONE',  ( 71.17905174416029013, 1.387412027389909985, -70.29005197907430613 ) ) ;
#38450 = CARTESIAN_POINT ( 'NONE',  ( 82.54525856212266888, 13.91914240249079171, -46.85691352100786844 ) ) ;
#38451 = FACE_OUTER_BOUND ( 'NONE', #45006, .T. ) ;
#38452 = DIRECTION ( 'NONE',  ( 1.000000000000000000, 0.000000000000000000, 0.000000000000000000 ) ) ;
#38454 = CARTESIAN_POINT ( 'NONE',  ( 55.89496596761120628, 14.69986299189930001, -25.41538446139790253 ) ) ;
#38453 = CARTESIAN_POINT ( 'NONE',  ( 60.14258128935630054, 13.88381105532070059, -25.78020575349050958 ) ) ;
#38455 = CARTESIAN_POINT ( 'NONE',  ( 9.166073574391180756, -14.52466137448119987, -73.50228201520940274 ) ) ;
#38456 = CARTESIAN_POINT ( 'NONE',  ( 19.68346084944639784, -21.71073103174810015, -79.17930779234599470 ) ) ;
#38457 = CARTESIAN_POINT ( 'NONE',  ( 15.09849273411411197, -7.705176520340744517, -67.25066374008305559 ) ) ;
#38458 = CARTESIAN_POINT ( 'NONE',  ( 20.63393739769620083, -41.61618894467930119, -35.14999999999999858 ) ) ;
#38459 = ADVANCED_FACE ( 'NONE', ( #18940 ), #495, .T. ) ;
#38460 = VERTEX_POINT ( 'NONE', #24843 ) ;
#38461 = LINE ( 'NONE', #22714, #33976 ) ;
#38462 = ORIENTED_EDGE ( 'NONE', *, *, #12422, .T. ) ;
#38463 = ADVANCED_FACE ( 'NONE', ( #4952 ), #5481, .T. ) ;
#38464 = VERTEX_POINT ( 'NONE', #45306 ) ;
#38465 = CARTESIAN_POINT ( 'NONE',  ( 12.05049839502609998, -64.90519735259998413, -16.21910226669200128 ) ) ;
#38466 = CARTESIAN_POINT ( 'NONE',  ( 24.04493137009028558, -15.60562024842286633, -39.50724629200023941 ) ) ;
#38467 = DIRECTION ( 'NONE',  ( -1.000000000000000000, 0.000000000000000000, 0.000000000000000000 ) ) ;
#38468 = DIRECTION ( 'NONE',  ( 1.000000000000000000, 0.000000000000000000, 0.000000000000000000 ) ) ;
#38469 = AXIS2_PLACEMENT_3D ( 'NONE', #12589, #40104, #40877 ) ;
#38470 = ORIENTED_EDGE ( 'NONE', *, *, #23615, .T. ) ;
#38471 = CIRCLE ( 'NONE', #16692, 4.000000000000058620 ) ;
#38472 = AXIS2_PLACEMENT_3D ( 'NONE', #44896, #51726, #31785 ) ;
#38473 = ORIENTED_EDGE ( 'NONE', *, *, #50529, .F. ) ;
#38474 = CARTESIAN_POINT ( 'NONE',  ( 71.35671708621339349, 1.389801772588449946, -61.03316673290180461 ) ) ;
#38475 = DIRECTION ( 'NONE',  ( 1.000000000000000000, 0.000000000000000000, 0.000000000000000000 ) ) ;
#38476 = AXIS2_PLACEMENT_3D ( 'NONE', #37356, #40510, #24757 ) ;
#38477 = CARTESIAN_POINT ( 'NONE',  ( 53.55414459173979935, 18.14307244785399931, -49.14835486563159606 ) ) ;
#38478 = CARTESIAN_POINT ( 'NONE',  ( 61.18464984179839661, -1.879430190305400039, -15.94894231725639955 ) ) ;
#38479 = CARTESIAN_POINT ( 'NONE',  ( 51.13984108499739989, -50.70264635719080104, -76.16554330276399298 ) ) ;
#38480 = CARTESIAN_POINT ( 'NONE',  ( 60.44324472221690314, -46.04849446251390077, -48.06791170149890036 ) ) ;
#38481 = ORIENTED_EDGE ( 'NONE', *, *, #18469, .T. ) ;
#38482 = CARTESIAN_POINT ( 'NONE',  ( 52.56521993351449851, -49.86179673305679927, -28.06704019101890069 ) ) ;
#38483 = CARTESIAN_POINT ( 'NONE',  ( 66.23540447448930024, 18.72622661238738573, -69.60146707679315625 ) ) ;
#38484 = VERTEX_POINT ( 'NONE', #1023 ) ;
#38485 = CARTESIAN_POINT ( 'NONE',  ( 15.24822371850887670, -8.849178727619387175, -51.91115236531553734 ) ) ;
#38486 = CARTESIAN_POINT ( 'NONE',  ( 58.76768575440100051, -46.69271212826609485, -47.97336379875430623 ) ) ;
#38487 = CARTESIAN_POINT ( 'NONE',  ( 9.835386274950829844, -10.93484284064630074, -41.21594592233229548 ) ) ;
#38488 = CARTESIAN_POINT ( 'NONE',  ( 13.95210466151750062, -50.80799586102129695, -21.48689998016109826 ) ) ;
#38489 = CARTESIAN_POINT ( 'NONE',  ( 54.18608382124189404, 19.84132336588830015, -75.62481673555129191 ) ) ;
#38490 = CARTESIAN_POINT ( 'NONE',  ( 46.42685859020519956, -53.00479672858950408, -76.14999999999999147 ) ) ;
#38491 = CARTESIAN_POINT ( 'NONE',  ( 56.80155790502700341, 13.89662352512740107, -16.18051027641230277 ) ) ;
#38492 = CARTESIAN_POINT ( 'NONE',  ( 20.25033824699210072, -9.889252315854481168, -78.54555634383710583 ) ) ;
#38493 = CARTESIAN_POINT ( 'NONE',  ( 56.48517904004920354, -50.54035073133489675, -52.93690031806480079 ) ) ;
#38494 = CARTESIAN_POINT ( 'NONE',  ( 9.421037744642760003, -13.45296509530860085, -41.94641019244480162 ) ) ;
#38495 = CARTESIAN_POINT ( 'NONE',  ( 9.366937397696199596, -15.61618894467949836, -28.45282021618999835 ) ) ;
#38496 = ORIENTED_EDGE ( 'NONE', *, *, #9854, .F. ) ;
#38498 = EDGE_CURVE ( 'NONE', #40171, #43323, #19683, .T. ) ;
#38497 = CARTESIAN_POINT ( 'NONE',  ( 47.60140394363290284, 23.29083994314989781, -74.50357325149190046 ) ) ;
#38499 = AXIS2_PLACEMENT_3D ( 'NONE', #34493, #38439, #5699 ) ;
#38500 = CARTESIAN_POINT ( 'NONE',  ( 64.81199447428090821, 0.8910129994591549085, -60.65352295474710331 ) ) ;
#38501 = VECTOR ( 'NONE', #6387, 1000.000000000000000 ) ;
#38502 = FACE_OUTER_BOUND ( 'NONE', #7838, .T. ) ;
#38503 = CARTESIAN_POINT ( 'NONE',  ( 11.84855223979754335, -65.05575864949535969, -23.81153761973788363 ) ) ;
#38504 = AXIS2_PLACEMENT_3D ( 'NONE', #23947, #39712, #8774 ) ;
#38505 = CARTESIAN_POINT ( 'NONE',  ( 45.92997521403570715, -45.11618897614619783, -7.538598176229350578 ) ) ;
#38506 = CARTESIAN_POINT ( 'NONE',  ( 61.75019796695546859, -45.11618894467940066, -26.84765976650484376 ) ) ;
#38507 = AXIS2_PLACEMENT_3D ( 'NONE', #20322, #43683, #47367 ) ;
#38508 = CIRCLE ( 'NONE', #35986, 23.00000000000000000 ) ;
#38509 = DIRECTION ( 'NONE',  ( 3.556943099846429769E-14, -1.469246684736110336E-14, 1.000000000000000000 ) ) ;
#38510 = CARTESIAN_POINT ( 'NONE',  ( 82.64668144475160716, 14.08996193411520004, -47.29313766171369338 ) ) ;
#38511 = DIRECTION ( 'NONE',  ( 0.8090169943749490056, 0.5877852522924709167, 0.000000000000000000 ) ) ;
#38513 = CARTESIAN_POINT ( 'NONE',  ( 47.17216055865273461, -39.34257126785092140, -54.74311960827047585 ) ) ;
#38512 = CARTESIAN_POINT ( 'NONE',  ( 65.03603135454920903, 1.015437840524759938, -17.83403478221330118 ) ) ;
#38514 = CARTESIAN_POINT ( 'NONE',  ( 24.02557101327613154, -15.05142125834110089, -71.48493766499311164 ) ) ;
#38515 = CARTESIAN_POINT ( 'NONE',  ( 6.211423689675569904, 33.74952992075439795, -48.42816009187949788 ) ) ;
#38516 = EDGE_CURVE ( 'NONE', #39196, #46682, #32967, .T. ) ;
#38517 = EDGE_LOOP ( 'NONE', ( #40581, #9414, #11088, #39814, #49592, #19463 ) ) ;
#38518 =( BOUNDED_CURVE ( )  B_SPLINE_CURVE ( 3, ( #27639, #18749, #7483, #15606 ),
 .UNSPECIFIED., .F., .T. ) 
 B_SPLINE_CURVE_WITH_KNOTS ( ( 4, 4 ),
 ( 0.000000000000000000, 0.7973345187655109800 ),
 .UNSPECIFIED. ) 
 CURVE ( )  GEOMETRIC_REPRESENTATION_ITEM ( )  RATIONAL_B_SPLINE_CURVE ( ( 1.000000000000000000, 0.9477194463320799400, 0.9477194463320799400, 1.000000000000000000 ) ) 
 REPRESENTATION_ITEM ( '' )  );
#38519 = CARTESIAN_POINT ( 'NONE',  ( 52.98105876229369926, -49.58786226930830310, -48.88375727566869955 ) ) ;
#38520 = ORIENTED_EDGE ( 'NONE', *, *, #29160, .T. ) ;
#38521 = CARTESIAN_POINT ( 'NONE',  ( 46.39291221988571579, 9.013049155818599445, -54.53239148715100271 ) ) ;
#38522 = CARTESIAN_POINT ( 'NONE',  ( 22.88346836455789557, -14.35432754477256090, -40.78781185829218003 ) ) ;
#38523 = CARTESIAN_POINT ( 'NONE',  ( 14.08288962360609986, 19.91677594646370153, -22.65087057678250204 ) ) ;
#38524 = CARTESIAN_POINT ( 'NONE',  ( 57.23260717840510381, 13.90933895519079933, -25.52124253973569878 ) ) ;
#38525 = CARTESIAN_POINT ( 'NONE',  ( 18.07474544453310017, -22.39673632833200045, -40.86408241699809452 ) ) ;
#38526 = CARTESIAN_POINT ( 'NONE',  ( 29.00424600244190287, -26.69196671705950052, -34.81403640487199880 ) ) ;
#38527 = CARTESIAN_POINT ( 'NONE',  ( 52.91963044591119569, 18.40471342935619958, -48.95754072428230330 ) ) ;
#38528 = CARTESIAN_POINT ( 'NONE',  ( 55.13867673449530571, -45.86707377957979759, -16.04494662851070075 ) ) ;
#38529 = ADVANCED_FACE ( 'NONE', ( #21438 ), #1538, .T. ) ;
#38530 = DIRECTION ( 'NONE',  ( 0.6339889056055360017, 0.000000000000000000, -0.7733421413379041320 ) ) ;
#38531 = ORIENTED_EDGE ( 'NONE', *, *, #37210, .T. ) ;
#38532 = CARTESIAN_POINT ( 'NONE',  ( 18.42293784796460088, -23.12266782108029872, -39.69329234158379194 ) ) ;
#38533 = EDGE_CURVE ( 'NONE', #50841, #25812, #25010, .T. ) ;
#38534 = CIRCLE ( 'NONE', #40314, 1.999999999999998224 ) ;
#38535 = CARTESIAN_POINT ( 'NONE',  ( 11.09248976069099868, -65.15264557193228256, -17.64371789480989960 ) ) ;
#38536 = CARTESIAN_POINT ( 'NONE',  ( 12.26578330975819853, 34.20340090639090391, -47.53372884124510023 ) ) ;
#38537 = CARTESIAN_POINT ( 'NONE',  ( 73.23379646625190276, 0.8840451408750739093, -62.48896739026430680 ) ) ;
#38538 = CARTESIAN_POINT ( 'NONE',  ( 11.89539497636140020, -65.43621263634180707, -18.11027658854760247 ) ) ;
#38539 = CARTESIAN_POINT ( 'NONE',  ( 53.27382404857081610, -49.51603170232991857, -49.18478183594817921 ) ) ;
#38540 = CARTESIAN_POINT ( 'NONE',  ( 22.45032208304290577, -20.49099972680067339, -76.00127256676395859 ) ) ;
#38541 = CARTESIAN_POINT ( 'NONE',  ( 22.75694797707483374, -14.18238632346227845, -62.38495220962165888 ) ) ;
#38542 = DIRECTION ( 'NONE',  ( 0.000000000000000000, 0.000000000000000000, -1.000000000000000000 ) ) ;
#38543 = VERTEX_POINT ( 'NONE', #51224 ) ;
#38544 = CARTESIAN_POINT ( 'NONE',  ( 64.97448143965360146, 1.327097482837290121, -70.45474866971780159 ) ) ;
#38545 = VERTEX_POINT ( 'NONE', #39169 ) ;
#38546 = CARTESIAN_POINT ( 'NONE',  ( 10.97995962411470039, -63.42200521575770722, -44.74774816381809472 ) ) ;
#38547 = CARTESIAN_POINT ( 'NONE',  ( 24.04493737206227877, -14.58064542962933352, -47.75066675682263906 ) ) ;
#38548 = ORIENTED_EDGE ( 'NONE', *, *, #21330, .F. ) ;
#38549 = DIRECTION ( 'NONE',  ( 0.000000000000000000, 0.000000000000000000, -1.000000000000000000 ) ) ;
#38550 = CARTESIAN_POINT ( 'NONE',  ( 57.02020359077309308, 19.36571434131419878, -53.44649995584460100 ) ) ;
#38551 = CARTESIAN_POINT ( 'NONE',  ( 52.66506589159119756, 18.87069406197509736, -77.26054838684399328 ) ) ;
#38552 = AXIS2_PLACEMENT_3D ( 'NONE', #32652, #44740, #45001 ) ;
#38553 = ORIENTED_EDGE ( 'NONE', *, *, #12009, .F. ) ;
#38554 = CARTESIAN_POINT ( 'NONE',  ( 13.00893739761190027, -65.51843714052189682, -47.75434321210310173 ) ) ;
#38555 = CARTESIAN_POINT ( 'NONE',  ( 57.50723796702470025, 15.88381105532069704, -31.98003398807230369 ) ) ;
#38556 = VECTOR ( 'NONE', #42610, 1000.000000000000000 ) ;
#38557 = CYLINDRICAL_SURFACE ( 'NONE', #31822, 38.00000000000000711 ) ;
#38558 = CARTESIAN_POINT ( 'NONE',  ( 17.87670698131359970, -32.37825826146760733, -34.70985242058469566 ) ) ;
#38559 = VECTOR ( 'NONE', #4442, 1000.000000000000000 ) ;
#38560 = B_SPLINE_SURFACE_WITH_KNOTS ( 'NONE', 3, 3, ( 
 ( #14503, #2971, #38882, #34925, #47266, #11612, #42555, #50924, #27320, #10585 ),
 ( #6647, #2715, #15021, #18688, #30732, #11354, #35447, #39389, #23366, #15284 ),
 ( #31238, #7420, #3493, #46758, #46495, #15540, #51444, #3229, #50668, #14764 ),
 ( #43580, #19720, #7681, #30474, #26541, #42816, #18946, #6912, #38624, #22861 ) ),
 .UNSPECIFIED., .F., .F., .F.,
 ( 4, 4 ),
 ( 4, 1, 1, 1, 1, 1, 1, 4 ),
 ( 1.485879941667409998, 1.508490955196220007 ),
 ( -1.052722112000000057E-06, 0.1428571428571430157, 0.2857142857142860315, 0.4285714285714289917, 0.5714285714285709528, 0.7142857142857139685, 0.8571428571428569843, 1.000000000000000000 ),
 .UNSPECIFIED. ) ;
#38561 = CARTESIAN_POINT ( 'NONE',  ( 18.80293497738039932, -23.41741782066900157, -66.18740309791239440 ) ) ;
#38562 = CARTESIAN_POINT ( 'NONE',  ( 9.221499647708412795, -19.60046634496452356, -48.34100205621588486 ) ) ;
#38563 = CARTESIAN_POINT ( 'NONE',  ( 44.94746977831004386, -38.03605091149837136, -65.58232186645768991 ) ) ;
#38564 = EDGE_LOOP ( 'NONE', ( #42425, #20989 ) ) ;
#38565 = DIRECTION ( 'NONE',  ( 0.000000000000000000, 0.000000000000000000, -1.000000000000000000 ) ) ;
#38566 = CARTESIAN_POINT ( 'NONE',  ( 17.24066946489620022, -22.98380985896210049, -52.68519703601729987 ) ) ;
#38567 = CARTESIAN_POINT ( 'NONE',  ( 53.16274104891699892, -49.55751115293769971, -49.15255090718000019 ) ) ;
#38568 = CARTESIAN_POINT ( 'NONE',  ( 9.036293696460461433, -17.93112585678219872, -32.14999999999999858 ) ) ;
#38569 = B_SPLINE_CURVE_WITH_KNOTS ( 'NONE', 3,
 ( #20065, #39493, #19821, #7263, #3591, #7010 ),
 .UNSPECIFIED., .F., .F.,
 ( 4, 2, 4 ),
 ( -0.0003214729304729410479, 0.000000000000000000, 0.01784182840660334182 ),
 .UNSPECIFIED. ) ;
#38571 = EDGE_CURVE ( 'NONE', #13264, #13283, #49900, .T. ) ;
#38570 = CYLINDRICAL_SURFACE ( 'NONE', #8313, 1.999999999999999556 ) ;
#38572 = CARTESIAN_POINT ( 'NONE',  ( 13.60549620763140233, 20.19926697308349972, -74.35527526576591129 ) ) ;
#38573 = ADVANCED_FACE ( 'NONE', ( #6682 ), #7454, .F. ) ;
#38574 = CARTESIAN_POINT ( 'NONE',  ( 9.221490736555526979, -11.63192677752850024, -50.95899774428340834 ) ) ;
#38575 = CARTESIAN_POINT ( 'NONE',  ( 45.83940545869849359, -45.13646462238730095, -7.873659365571991309 ) ) ;
#38576 = CARTESIAN_POINT ( 'NONE',  ( 19.78512659345921421, -8.570954873263845641, -61.15985033246573011 ) ) ;
#38577 = CARTESIAN_POINT ( 'NONE',  ( 23.03293134511480034, -11.10103632018729947, -67.32320539224708966 ) ) ;
#38578 = EDGE_LOOP ( 'NONE', ( #21754, #33111, #15637, #29170 ) ) ;
#38579 = CARTESIAN_POINT ( 'NONE',  ( 20.11790897856640115, -22.39793288440460017, -32.14999999999999858 ) ) ;
#38580 = CARTESIAN_POINT ( 'NONE',  ( 56.08336180637530788, -50.80210678062450569, -74.87709413289790916 ) ) ;
#38582 = CARTESIAN_POINT ( 'NONE',  ( 41.17180578240099464, -39.67071095666287306, -80.32671525995388606 ) ) ;
#38581 = CARTESIAN_POINT ( 'NONE',  ( -1.485984422640509894, 19.61345480293289967, -6.464765694581079636 ) ) ;
#38583 = CARTESIAN_POINT ( 'NONE',  ( 20.30127474080329719, 10.88381105532070059, -34.64999999999999858 ) ) ;
#38584 = DIRECTION ( 'NONE',  ( 0.9741140340359943917, 0.000000000000000000, 0.2260571801428161165 ) ) ;
#38585 =( GEOMETRIC_REPRESENTATION_CONTEXT ( 3 ) GLOBAL_UNCERTAINTY_ASSIGNED_CONTEXT ( ( #22688 ) ) GLOBAL_UNIT_ASSIGNED_CONTEXT ( ( #24338, #15735, #20414 ) ) REPRESENTATION_CONTEXT ( 'NONE', 'WORKASPACE' ) );
#38586 = VERTEX_POINT ( 'NONE', #31021 ) ;
#38587 = AXIS2_PLACEMENT_3D ( 'NONE', #40374, #286, #16270 ) ;
#38588 = CARTESIAN_POINT ( 'NONE',  ( 16.58613412942849408, -7.681895695860129436, -81.02569497777129470 ) ) ;
#38589 = AXIS2_PLACEMENT_3D ( 'NONE', #25071, #5454, #44760 ) ;
#38590 = CARTESIAN_POINT ( 'NONE',  ( 47.50173433525049660, 23.36124847523640113, -54.80342700628099806 ) ) ;
#38591 = CARTESIAN_POINT ( 'NONE',  ( 24.04493737206098203, -15.04802456787528619, -65.76947574710013100 ) ) ;
#38592 = CARTESIAN_POINT ( 'NONE',  ( 63.47112272702528912, 1.372372808637209785, -62.39142423721519748 ) ) ;
#38593 = CARTESIAN_POINT ( 'NONE',  ( 56.61928438282120624, 14.09173444410579989, -25.29356196242219923 ) ) ;
#38594 = VECTOR ( 'NONE', #44025, 1000.000000000000000 ) ;
#38595 = CARTESIAN_POINT ( 'NONE',  ( 11.50351859489629902, 34.04974385669249415, -17.32566793788090109 ) ) ;
#38596 = LINE ( 'NONE', #30191, #46696 ) ;
#38597 = CARTESIAN_POINT ( 'NONE',  ( 52.82947172221679466, 18.42909589620090216, -48.64743982913490328 ) ) ;
#38598 = PLANE ( 'NONE',  #33377 ) ;
#38599 = SPHERICAL_SURFACE ( 'NONE', #2475, 3.000000000000000000 ) ;
#38600 = CARTESIAN_POINT ( 'NONE',  ( 52.77132786495689487, 18.46083226933780352, -28.08595485654360147 ) ) ;
#38601 = CARTESIAN_POINT ( 'NONE',  ( 50.51123532868781041, 4.833585210846805147, -76.20873194682746998 ) ) ;
#38602 = EDGE_CURVE ( 'NONE', #43797, #12820, #7213, .T. ) ;
#38603 = CARTESIAN_POINT ( 'NONE',  ( 52.82976000643810011, -49.66091852057420652, -28.05436868014771079 ) ) ;
#38604 = CARTESIAN_POINT ( 'NONE',  ( 53.12218290940240450, 18.34074958227849805, -49.13784296393349393 ) ) ;
#38605 = CARTESIAN_POINT ( 'NONE',  ( 53.10211901724390060, -45.11618894467940066, -9.306651317679861535 ) ) ;
#38606 = CARTESIAN_POINT ( 'NONE',  ( 71.13364007206789097, 1.371651820402770117, -60.88469507784019896 ) ) ;
#38607 = CARTESIAN_POINT ( 'NONE',  ( 11.10559214712420051, 32.11323242349129714, -44.25388736977730275 ) ) ;
#38608 = CARTESIAN_POINT ( 'NONE',  ( 72.98330304380999678, 0.9543424661151610477, -62.11630250819479926 ) ) ;
#38609 = CARTESIAN_POINT ( 'NONE',  ( 65.32710667846340868, -32.02409943616269317, -17.54847724138329923 ) ) ;
#38610 = CARTESIAN_POINT ( 'NONE',  ( 18.78670704276689918, 20.36472114263469990, -74.14993923597710079 ) ) ;
#38611 = ORIENTED_EDGE ( 'NONE', *, *, #24833, .F. ) ;
#38612 = EDGE_LOOP ( 'NONE', ( #2449, #41943 ) ) ;
#38613 = CARTESIAN_POINT ( 'NONE',  ( 63.25402410758490390, 0.9098571636355720083, -62.15909090909049439 ) ) ;
#38614 = CARTESIAN_POINT ( 'NONE',  ( 76.49478695177366205, -3.228580831157734199, -13.20495443489320131 ) ) ;
#38615 = ORIENTED_EDGE ( 'NONE', *, *, #4646, .T. ) ;
#38616 = CARTESIAN_POINT ( 'NONE',  ( 11.79375100434000068, -65.01330894899159318, -45.51098474479470468 ) ) ;
#38617 = CARTESIAN_POINT ( 'NONE',  ( 56.92167681130780466, -45.21777262807209752, -25.50865813986290220 ) ) ;
#38618 = CYLINDRICAL_SURFACE ( 'NONE', #37867, 10.00000000000000711 ) ;
#38619 = CARTESIAN_POINT ( 'NONE',  ( 28.28038400710289935, -8.603434725040973063, -34.79644660940672907 ) ) ;
#38620 = CARTESIAN_POINT ( 'NONE',  ( 13.58893910384336046, -51.93861847144918187, -75.09855816271630147 ) ) ;
#38621 = ORIENTED_EDGE ( 'NONE', *, *, #44068, .F. ) ;
#38622 = CARTESIAN_POINT ( 'NONE',  ( 61.51122975691189509, 13.91278366405479616, -37.26101630944549470 ) ) ;
#38623 = CARTESIAN_POINT ( 'NONE',  ( 43.34994082412796956, 6.595960187102031469, -73.56991816002565088 ) ) ;
#38624 = CARTESIAN_POINT ( 'NONE',  ( 11.72646946156880077, 32.43593556876640349, -24.74253206387260207 ) ) ;
#38625 = VERTEX_POINT ( 'NONE', #10618 ) ;
#38626 = CARTESIAN_POINT ( 'NONE',  ( 8.497902144169069416, -12.50593227557700082, -32.91545205119220441 ) ) ;
#38627 = DIRECTION ( 'NONE',  ( 0.000000000000000000, -1.000000000000000000, 0.000000000000000000 ) ) ;
#38628 = CARTESIAN_POINT ( 'NONE',  ( 14.30960224998139907, 19.88381748068809785, -22.40439468542579604 ) ) ;
#38629 = CARTESIAN_POINT ( 'NONE',  ( 17.53270220351207698, -22.29603902678120519, -50.88730431063954995 ) ) ;
#38630 = CARTESIAN_POINT ( 'NONE',  ( 10.22098660000356318, -19.02411275232799781, -47.28612486470034781 ) ) ;
#38631 = TOROIDAL_SURFACE ( 'NONE', #13520, 30.50439988982899564, 1.000000000000000000 ) ;
#38632 = CARTESIAN_POINT ( 'NONE',  ( 63.10653712364229762, 0.8879664753683499390, -62.37500410124779648 ) ) ;
#38633 = CARTESIAN_POINT ( 'NONE',  ( 46.47231003491339862, -53.11747274052710566, -76.13961530627510399 ) ) ;
#38634 = CIRCLE ( 'NONE', #1760, 9.999999999999998224 ) ;
#38635 = CARTESIAN_POINT ( 'NONE',  ( 58.16220902598259812, 13.11504794394689988, -8.909165776004030590 ) ) ;
#38636 = AXIS2_PLACEMENT_3D ( 'NONE', #39069, #24063, #36144 ) ;
#38637 = EDGE_CURVE ( 'NONE', #21295, #13019, #43106, .T. ) ;
#38638 = CARTESIAN_POINT ( 'NONE',  ( -0.4410626023037830246, -8.356009309619699010, -35.14999999999999858 ) ) ;
#38639 = EDGE_CURVE ( 'NONE', #46452, #9063, #23151, .T. ) ;
#38640 = EDGE_CURVE ( 'NONE', #16604, #32526, #26451, .T. ) ;
#38641 = CARTESIAN_POINT ( 'NONE',  ( 52.32303876295770095, 20.18503163261420141, -75.90202713928280787 ) ) ;
#38642 = CARTESIAN_POINT ( 'NONE',  ( 61.51122975691189509, -45.14516155341349446, -37.26101630944549470 ) ) ;
#38643 = ADVANCED_FACE ( 'NONE', ( #19239 ), #35765, .F. ) ;
#38644 = CARTESIAN_POINT ( 'NONE',  ( 11.24524132308850000, -22.25571999044219851, -34.20969220765409347 ) ) ;
#38645 = ORIENTED_EDGE ( 'NONE', *, *, #8917, .T. ) ;
#38646 = CARTESIAN_POINT ( 'NONE',  ( 54.35976913619879980, -48.30693508310460516, -26.83861054538819957 ) ) ;
#38647 = CARTESIAN_POINT ( 'NONE',  ( 1.127313977364120090, -53.29995640468419538, -7.495105548070389645 ) ) ;
#38648 = CARTESIAN_POINT ( 'NONE',  ( 75.79457347663668543, -29.99145320232659984, -12.10716626236989946 ) ) ;
#38649 = CARTESIAN_POINT ( 'NONE',  ( 74.93037820153030282, 13.88381105528979909, -15.31096251095349992 ) ) ;
#38650 = CARTESIAN_POINT ( 'NONE',  ( 51.13393739769659874, -50.61618894467899565, 11.97999999999999865 ) ) ;
#38651 = CARTESIAN_POINT ( 'NONE',  ( 14.23931515459926089, 1.282173023328767369, -34.84133294386911217 ) ) ;
#38652 = B_SPLINE_CURVE_WITH_KNOTS ( 'NONE', 3,
 ( #28205, #20090, #8572, #4892, #32906, #20859, #25038, #9089, #40534, #36591, #692, #32641, #16682, #17213, #33173, #29242 ),
 .UNSPECIFIED., .F., .F.,
 ( 4, 2, 2, 2, 2, 2, 2, 4 ),
 ( 0.000000000000000000, 0.1774999999999995748, 0.3374999999999991340, 0.4375000000000007772, 0.4999999999999992228, 0.6250000000000014433, 0.8249999999999997335, 1.000000000000000000 ),
 .UNSPECIFIED. ) ;
#38653 = CARTESIAN_POINT ( 'NONE',  ( 74.93037048120270072, -45.11618894467940066, -15.31097009269700138 ) ) ;
#38654 = EDGE_CURVE ( 'NONE', #6764, #20524, #7965, .T. ) ;
#38655 = CARTESIAN_POINT ( 'NONE',  ( 82.51402289001910617, -45.11865457252260114, -46.70332443011600532 ) ) ;
#38656 = DIRECTION ( 'NONE',  ( 0.000000000000000000, 0.000000000000000000, 1.000000000000000000 ) ) ;
#38657 = CARTESIAN_POINT ( 'NONE',  ( 42.16710579538349890, 12.08965825037509845, -3.592545294286160207 ) ) ;
#38658 = CARTESIAN_POINT ( 'NONE',  ( -2.366062601062550730, -15.61618894523020629, 9.350000000582056714 ) ) ;
#38659 = CARTESIAN_POINT ( 'NONE',  ( 19.58096105366284334, 24.23501488104968260, -75.51638835764758539 ) ) ;
#38660 = CARTESIAN_POINT ( 'NONE',  ( 70.83393739769717001, -48.11618894467018492, -75.95000000000109708 ) ) ;
#38661 = CARTESIAN_POINT ( 'NONE',  ( 21.54527684569834989, -19.77483519589170058, -62.66115525799357044 ) ) ;
#38662 = CARTESIAN_POINT ( 'NONE',  ( 18.30489236469509962, -52.23921076650779582, -75.65449215554859563 ) ) ;
#38664 = ADVANCED_FACE ( 'NONE', ( #24690 ), #355, .T. ) ;
#38663 = CARTESIAN_POINT ( 'NONE',  ( 53.17454399592740089, -51.89736142002809771, -53.32454619227790005 ) ) ;
#38665 = ORIENTED_EDGE ( 'NONE', *, *, #27742, .T. ) ;
#38666 = CIRCLE ( 'NONE', #42854, 25.10000000000000142 ) ;
#38667 = CARTESIAN_POINT ( 'NONE',  ( 18.71541599555600044, -22.60494152200909923, -49.45471475294879582 ) ) ;
#38668 = CARTESIAN_POINT ( 'NONE',  ( 63.43387347518848429, 0.9897451961579500912, -61.91936536276160297 ) ) ;
#38669 = ORIENTED_EDGE ( 'NONE', *, *, #31813, .T. ) ;
#38670 = CARTESIAN_POINT ( 'NONE',  ( 12.72598263503342686, -21.52912116282474742, -69.11948608177338826 ) ) ;
#38671 = CIRCLE ( 'NONE', #16056, 0.4999999999096970127 ) ;
#38672 = CARTESIAN_POINT ( 'NONE',  ( 61.00705302608989911, -45.67218455906219532, -47.73074504205549573 ) ) ;
#38673 = CARTESIAN_POINT ( 'NONE',  ( 73.22759735627541033, 0.9947083095259801055, -68.80546575785609775 ) ) ;
#38674 = CARTESIAN_POINT ( 'NONE',  ( 45.49455817588943773, 8.831023168557877057, -59.41298158052058653 ) ) ;
#38675 = AXIS2_PLACEMENT_3D ( 'NONE', #40700, #24945, #13460 ) ;
#38676 = CARTESIAN_POINT ( 'NONE',  ( 8.133937397696209715, 23.57564693985150228, -21.14999999999999858 ) ) ;
#38677 = CARTESIAN_POINT ( 'NONE',  ( 41.26311261641770045, -45.40138146105840633, -6.071159984357790584 ) ) ;
#38678 = ORIENTED_EDGE ( 'NONE', *, *, #27334, .F. ) ;
#38679 = ORIENTED_EDGE ( 'NONE', *, *, #16012, .T. ) ;
#38680 = ORIENTED_EDGE ( 'NONE', *, *, #3093, .F. ) ;
#38681 = DIRECTION ( 'NONE',  ( 1.000000000000000000, 0.000000000000000000, 0.000000000000000000 ) ) ;
#38682 = CARTESIAN_POINT ( 'NONE',  ( 61.21704192275100098, -45.26864704484780333, -46.77873930917139944 ) ) ;
#38683 = CARTESIAN_POINT ( 'NONE',  ( -22.60072279458010058, -20.15755767129849829, -54.65015892017029842 ) ) ;
#38684 = EDGE_CURVE ( 'NONE', #37751, #13264, #35767, .T. ) ;
#38685 = EDGE_LOOP ( 'NONE', ( #29302, #1417, #25412, #41692 ) ) ;
#38686 = CARTESIAN_POINT ( 'NONE',  ( 9.507079698477085117, -14.03414070217627341, -79.52724392247833407 ) ) ;
#38687 = ORIENTED_EDGE ( 'NONE', *, *, #44093, .T. ) ;
#38688 = CARTESIAN_POINT ( 'NONE',  ( 16.13393739769639623, 7.383811055320659733, -59.64999999999999147 ) ) ;
#38689 = CARTESIAN_POINT ( 'NONE',  ( 45.17583307331749864, -33.37024725518060109, -34.90149097438519732 ) ) ;
#38690 = VERTEX_POINT ( 'NONE', #12680 ) ;
#38691 = CARTESIAN_POINT ( 'NONE',  ( 2.404741263826560171, -25.85214510508460251, -35.14999999999999858 ) ) ;
#38692 = CARTESIAN_POINT ( 'NONE',  ( 52.19959688358610350, -51.15283330212230339, -76.05470842491450867 ) ) ;
#38693 = CARTESIAN_POINT ( 'NONE',  ( 60.24866557976239534, 14.54998834221819948, -47.36885438232269507 ) ) ;
#38694 = CARTESIAN_POINT ( 'NONE',  ( 71.33393739769628894, 1.883811055320669947, -68.84999999999999432 ) ) ;
#38695 = CARTESIAN_POINT ( 'NONE',  ( 41.72814281503579537, -43.80724058770579887, -4.012820145101700042 ) ) ;
#38696 = CARTESIAN_POINT ( 'NONE',  ( -10.42699089400579915, 11.57162609797640052, -6.107075065358959165 ) ) ;
#38697 = EDGE_CURVE ( 'NONE', #23033, #37842, #37065, .T. ) ;
#38698 = VECTOR ( 'NONE', #7273, 1000.000000000000000 ) ;
#38699 = AXIS2_PLACEMENT_3D ( 'NONE', #20199, #48002, #28059 ) ;
#38700 = CARTESIAN_POINT ( 'NONE',  ( 64.64722926691230498, 0.9479899806831150189, -70.53291850127419593 ) ) ;
#38701 = LINE ( 'NONE', #31314, #25519 ) ;
#38702 = CARTESIAN_POINT ( 'NONE',  ( 56.39270784227079503, -50.52750194671250483, -52.86271187454359932 ) ) ;
#38703 = EDGE_CURVE ( 'NONE', #1308, #31549, #38275, .T. ) ;
#38704 = CARTESIAN_POINT ( 'NONE',  ( 9.460335462710569132, -19.74532752270490121, -54.11113779516249878 ) ) ;
#38705 = ORIENTED_EDGE ( 'NONE', *, *, #6759, .F. ) ;
#38706 = CARTESIAN_POINT ( 'NONE',  ( 14.30198883284579914, -52.24360429457480137, -75.86497326479759806 ) ) ;
#38707 = CARTESIAN_POINT ( 'NONE',  ( 44.98357806667660697, 14.87857081572859919, -8.963106682104738709 ) ) ;
#38708 = CARTESIAN_POINT ( 'NONE',  ( 71.82945924946500327, 1.426105412860660060, -70.05138037415009933 ) ) ;
#38709 = CARTESIAN_POINT ( 'NONE',  ( 45.43114679010229651, -40.05928987699603283, -59.72086155090411097 ) ) ;
#38710 = CARTESIAN_POINT ( 'NONE',  ( 15.10819245920639986, 19.52950791741820069, -20.77789291003839978 ) ) ;
#38711 = CARTESIAN_POINT ( 'NONE',  ( 21.39116947223989840, -11.14063841565600121, -32.14999999999999858 ) ) ;
#38712 = CARTESIAN_POINT ( 'NONE',  ( 63.25402410758490390, 0.9098571636355680115, -69.14090909090950277 ) ) ;
#38713 = CARTESIAN_POINT ( 'NONE',  ( 47.85552020099460435, -54.43926621290979995, -55.10000200886270250 ) ) ;
#38714 = CARTESIAN_POINT ( 'NONE',  ( 18.86789271228509790, -51.78678246903520233, -74.14999999999999147 ) ) ;
#38715 = CARTESIAN_POINT ( 'NONE',  ( 9.367498100245670756, -15.05912955991499658, -35.87337699974327165 ) ) ;
#38716 = CARTESIAN_POINT ( 'NONE',  ( 47.86297059184269642, 23.17976950889599763, -54.90440623528039765 ) ) ;
#38717 = ORIENTED_EDGE ( 'NONE', *, *, #6985, .T. ) ;
#38718 = CARTESIAN_POINT ( 'NONE',  ( 9.185203505404999191, -16.82352339236760130, -73.79242048001970034 ) ) ;
#38719 = ORIENTED_EDGE ( 'NONE', *, *, #27312, .F. ) ;
#38721 = CARTESIAN_POINT ( 'NONE',  ( 71.43836573789060651, 0.9955677559369568996, -70.64918477200470193 ) ) ;
#38720 = B_SPLINE_SURFACE_WITH_KNOTS ( 'NONE', 3, 3, ( 
 ( #37279, #45926, #5830, #25715, #49860, #42515, #17625, #17365 ),
 ( #6604, #29406, #18134, #46455, #6092, #21793, #22046, #10543 ),
 ( #46196, #5579, #21534, #37801, #1896, #2401, #33333, #1378 ),
 ( #13949, #45661, #34096, #17873, #18385, #30430, #37531, #26499 ),
 ( #10016, #49348, #33595, #13447, #45406, #9511, #34360, #33844 ),
 ( #38059, #42250, #9764, #50377, #10280, #25458, #41463, #29908 ),
 ( #26242, #41992, #13696, #1636, #50111, #2154, #14206, #6349 ),
 ( #22307, #49609, #29656, #41723, #35141, #34885, #47729, #51656 ),
 ( #35672, #46715, #15501, #23585, #11315, #31454, #43790, #23327 ),
 ( #51400, #50626, #10800, #30943, #30693, #3191, #38581, #43031 ),
 ( #11834, #7128, #23080, #39098, #27534, #18648, #38842, #2675 ),
 ( #27280, #11057, #14977, #2930, #19164, #51146, #31704, #15244 ),
 ( #31194, #27024, #47225, #27794, #18901, #34622, #43289, #22565 ),
 ( #3451, #14723, #7378, #39352, #19424, #26759, #6872, #47480 ),
 ( #42772, #35404, #11572, #39603, #22821, #50885, #46974, #43540 ),
 ( #7640, #3706, #19674, #15750, #28039, #33001, #24611, #32462 ) ),
 .UNSPECIFIED., .F., .F., .F.,
 ( 4, 2, 2, 2, 2, 2, 2, 4 ),
 ( 4, 1, 1, 1, 1, 4 ),
 ( 12.41737348417879971, 14.15001006772950021, 23.85327782795560125, 28.70491170806869974, 32.58621881215919558, 36.46752591624959905, 42.67761728279440092, 46.65092557583719923 ),
 ( -1.202762707400000043E-05, 0.2000000000000000111, 0.4000000000000000222, 0.5999999999999999778, 0.8000000000000000444, 1.000241744799150068 ),
 .UNSPECIFIED. ) ;
#38722 = CARTESIAN_POINT ( 'NONE',  ( 82.48407818766771982, 13.86596467738130833, -46.54738304680805783 ) ) ;
#38723 = LINE ( 'NONE', #2819, #37837 ) ;
#38725 = DIRECTION ( 'NONE',  ( 1.000000000000000000, 2.460964292799963328E-14, 0.000000000000000000 ) ) ;
#38724 = CARTESIAN_POINT ( 'NONE',  ( 17.21347160910390173, -53.11618894467930119, -76.14999999999999147 ) ) ;
#38726 = CARTESIAN_POINT ( 'NONE',  ( 13.89842162571510009, -9.131180857971619602, -81.84667608724390675 ) ) ;
#38727 = CARTESIAN_POINT ( 'NONE',  ( 16.13393739769620083, -15.61618894467929941, -14.88746750000000141 ) ) ;
#38728 = CARTESIAN_POINT ( 'NONE',  ( 12.14988920053796306, -22.52875919624318257, -42.17433473518147480 ) ) ;
#38729 = CARTESIAN_POINT ( 'NONE',  ( 21.54526587704876661, -19.77485033222403743, -40.66111538846325146 ) ) ;
#38730 = ORIENTED_EDGE ( 'NONE', *, *, #50149, .F. ) ;
#38731 = CARTESIAN_POINT ( 'NONE',  ( 68.13393739769618662, -30.66618894467940137, -65.65000000000000568 ) ) ;
#38732 = VERTEX_POINT ( 'NONE', #45942 ) ;
#38733 = ORIENTED_EDGE ( 'NONE', *, *, #48676, .T. ) ;
#38734 = CARTESIAN_POINT ( 'NONE',  ( 12.36320305068320025, -64.54682834576858852, -15.76422791927960176 ) ) ;
#38735 = CARTESIAN_POINT ( 'NONE',  ( 41.61626771661330082, -36.11618894467930119, -82.23834840541459812 ) ) ;
#38736 = AXIS2_PLACEMENT_3D ( 'NONE', #12766, #25304, #960 ) ;
#38737 = CARTESIAN_POINT ( 'NONE',  ( 16.96763219941080081, -8.612796041803930436, -62.38489440685859222 ) ) ;
#38738 = CARTESIAN_POINT ( 'NONE',  ( 13.00893739769619906, -65.51843714052719747, -47.75434321273180416 ) ) ;
#38739 = AXIS2_PLACEMENT_3D ( 'NONE', #30855, #46884, #50801 ) ;
#38740 = ORIENTED_EDGE ( 'NONE', *, *, #3366, .F. ) ;
#38741 = ADVANCED_FACE ( 'NONE', ( #33080 ), #29419, .T. ) ;
#38742 = ORIENTED_EDGE ( 'NONE', *, *, #20746, .T. ) ;
#38743 = CARTESIAN_POINT ( 'NONE',  ( 54.45614327494340046, 20.39970296835689823, -54.11881936521780290 ) ) ;
#38744 = CARTESIAN_POINT ( 'NONE',  ( 50.95939809116894992, -35.29322421015848477, -76.37898009206955408 ) ) ;
#38745 = EDGE_CURVE ( 'NONE', #26084, #6962, #12255, .T. ) ;
#38746 = CARTESIAN_POINT ( 'NONE',  ( 52.58363548700440049, -49.84283414857759453, -48.51251314324170494 ) ) ;
#38747 = CARTESIAN_POINT ( 'NONE',  ( 22.89955372608299555, -15.46837744865813313, -46.44587548950233469 ) ) ;
#38748 = CARTESIAN_POINT ( 'NONE',  ( 61.93068749498159775, -0.2735828025601050317, -16.53651274250989545 ) ) ;
#38749 = EDGE_CURVE ( 'NONE', #39228, #49183, #39052, .T. ) ;
#38750 = CARTESIAN_POINT ( 'NONE',  ( 57.57487205268949992, -49.96950191258749641, -52.44452323771800195 ) ) ;
#38751 = EDGE_LOOP ( 'NONE', ( #44106, #32220, #49904, #6569 ) ) ;
#38752 = CARTESIAN_POINT ( 'NONE',  ( 24.04493740047237083, -15.60197482040396721, -33.79175808096959344 ) ) ;
#38753 = CARTESIAN_POINT ( 'NONE',  ( 76.13592501344869845, 12.07790803439914029, -13.68765646776531320 ) ) ;
#38754 = EDGE_LOOP ( 'NONE', ( #39455, #24435, #46343, #27879 ) ) ;
#38755 = CARTESIAN_POINT ( 'NONE',  ( 16.13393739769620083, -1.182432214938700099, -34.64999999999999858 ) ) ;
#38756 = CARTESIAN_POINT ( 'NONE',  ( 54.36584921719999386, -48.99915756198799954, -48.99053282728779379 ) ) ;
#38757 = CARTESIAN_POINT ( 'NONE',  ( 22.45595482960829870, -10.96658216752249970, -45.81064392402229402 ) ) ;
#38758 = CARTESIAN_POINT ( 'NONE',  ( 13.93396757539989927, -51.17250542873200203, -22.49579876130530209 ) ) ;
#38759 = FACE_OUTER_BOUND ( 'NONE', #37049, .T. ) ;
#38760 = CARTESIAN_POINT ( 'NONE',  ( 56.52130130765199567, 13.95454412478370010, -16.23639984573850015 ) ) ;
#38761 = CARTESIAN_POINT ( 'NONE',  ( 10.22105663364766848, -12.20814506941904831, -77.61948635994986034 ) ) ;
#38762 = CARTESIAN_POINT ( 'NONE',  ( 71.07527734533519492, 1.384447124000270035, -70.32375107525380997 ) ) ;
#38763 = CARTESIAN_POINT ( 'NONE',  ( 16.91867857995320179, -8.607141901655479543, -46.38267033200749978 ) ) ;
#38764 = CARTESIAN_POINT ( 'NONE',  ( 21.54526522592269444, -11.45752699557874088, -44.24446278245023478 ) ) ;
#38765 = B_SPLINE_CURVE_WITH_KNOTS ( 'NONE', 3,
 ( #42318, #45993, #6670, #23143, #11122, #6415 ),
 .UNSPECIFIED., .F., .F.,
 ( 4, 1, 1, 4 ),
 ( 0.000000000000000000, 0.3333336742575975231, 0.6666673485151961565, 1.000000000000000000 ),
 .UNSPECIFIED. ) ;
#38766 = EDGE_CURVE ( 'NONE', #30137, #31815, #15802, .T. ) ;
#38767 = EDGE_LOOP ( 'NONE', ( #43857, #23447, #31863, #27505, #4815 ) ) ;
#38768 = CARTESIAN_POINT ( 'NONE',  ( 46.37807361908240011, 21.71172191342840208, -76.14999999999999147 ) ) ;
#38769 = CARTESIAN_POINT ( 'NONE',  ( 65.07649219403889163, 1.383767307422960169, -60.97855929785719553 ) ) ;
#38770 = CARTESIAN_POINT ( 'NONE',  ( 43.83352794118219720, -46.05657771629909547, -8.175079556547590443 ) ) ;
#38771 = AXIS2_PLACEMENT_3D ( 'NONE', #5418, #1481, #8829 ) ;
#38772 = CARTESIAN_POINT ( 'NONE',  ( 30.68460988201149320, -15.41618894467931611, -103.0993275156849762 ) ) ;
#38773 = AXIS2_PLACEMENT_3D ( 'NONE', #38953, #6979, #30540 ) ;
#38774 = DIRECTION ( 'NONE',  ( 0.000000000000000000, 4.336808689941963009E-16, -1.000000000000000000 ) ) ;
#38775 = DIRECTION ( 'NONE',  ( -8.592609827796581962E-15, 1.919972818367709724E-16, -1.000000000000000000 ) ) ;
#38776 = B_SPLINE_CURVE_WITH_KNOTS ( 'NONE', 3,
 ( #50263, #2562, #39236, #30829, #30317, #2824, #15130, #22450, #31087, #42917, #47115, #38728, #14349, #11204, #46341, #51028, #3334, #42396 ),
 .UNSPECIFIED., .F., .F.,
 ( 4, 2, 2, 2, 2, 2, 2, 2, 4 ),
 ( 0.4999993651278294982, 0.5624994444868508525, 0.6249995238458720959, 0.6874996032048934502, 0.7499996825639148046, 0.8124997619229360479, 0.8749998412819574023, 0.9374999206409786456, 1.000000000000000000 ),
 .UNSPECIFIED. ) ;
#38777 = CARTESIAN_POINT ( 'NONE',  ( 82.48253024579470605, 14.11464642499709932, -47.31939374336590021 ) ) ;
#38778 = CARTESIAN_POINT ( 'NONE',  ( -21.99499352544900077, -6.866245975711579241, -54.13127606174950301 ) ) ;
#38780 = CARTESIAN_POINT ( 'NONE',  ( 24.04527307164895333, -15.61618901697373119, -57.79233174308600951 ) ) ;
#38779 = CARTESIAN_POINT ( 'NONE',  ( 52.27429626352468262, 18.55921403040872875, -77.19751344877612098 ) ) ;
#38781 = CARTESIAN_POINT ( 'NONE',  ( 14.35738282767117902, -23.35377304929353315, -32.36411522678612585 ) ) ;
#38782 = CARTESIAN_POINT ( 'NONE',  ( -25.78889119571919863, 9.715729424517359547, -54.35424806255070251 ) ) ;
#38783 = ORIENTED_EDGE ( 'NONE', *, *, #47093, .F. ) ;
#38784 = CARTESIAN_POINT ( 'NONE',  ( 52.73034409711829795, -49.72355465471469671, -48.63395058221750133 ) ) ;
#38785 = ORIENTED_EDGE ( 'NONE', *, *, #11718, .T. ) ;
#38786 = CARTESIAN_POINT ( 'NONE',  ( 47.23718928093980196, 8.041435364245701933, -54.67975386834223883 ) ) ;
#38787 = CARTESIAN_POINT ( 'NONE',  ( 21.54530377845328815, -11.45757991958564048, -42.24448642716485125 ) ) ;
#38788 = CARTESIAN_POINT ( 'NONE',  ( 13.89738755828549976, 19.98851976734169966, -22.99807275174740084 ) ) ;
#38789 = DIRECTION ( 'NONE',  ( -0.8090169943749462300, -0.5877852522924749135, 0.000000000000000000 ) ) ;
#38790 = CARTESIAN_POINT ( 'NONE',  ( 21.81560882561450043, -11.43753264368949907, -46.25096972932429651 ) ) ;
#38791 = CARTESIAN_POINT ( 'NONE',  ( 53.16045451627860530, 18.32047277855539846, -49.13860146820209707 ) ) ;
#38792 = CARTESIAN_POINT ( 'NONE',  ( 55.62727650224960740, -45.90849497969049509, -16.78013324446749976 ) ) ;
#38793 = CARTESIAN_POINT ( 'NONE',  ( 24.04493739769619864, -15.61618894467929941, -32.14999999999999858 ) ) ;
#38794 = AXIS2_PLACEMENT_3D ( 'NONE', #19504, #37939, #31538 ) ;
#38795 = ORIENTED_EDGE ( 'NONE', *, *, #39936, .F. ) ;
#38796 = CARTESIAN_POINT ( 'NONE',  ( 21.66969093749800024, -20.60263879829989619, -81.30072504052380111 ) ) ;
#38797 = ORIENTED_EDGE ( 'NONE', *, *, #39305, .F. ) ;
#38798 = DIRECTION ( 'NONE',  ( 1.000000000000000000, 0.000000000000000000, 0.000000000000000000 ) ) ;
#38799 = CARTESIAN_POINT ( 'NONE',  ( 12.91569276135830080, 34.28022004553969992, -47.73039263113269470 ) ) ;
#38800 = CARTESIAN_POINT ( 'NONE',  ( 72.80507874878320251, 1.371509258145880095, -62.41110185547420031 ) ) ;
#38801 = LINE ( 'NONE', #2895, #46119 ) ;
#38802 = CARTESIAN_POINT ( 'NONE',  ( 52.69474619017665873, -49.76773528829182425, -48.79529908194032117 ) ) ;
#38803 = CARTESIAN_POINT ( 'NONE',  ( -33.86606260230286125, -15.61618894467806484, -57.75434458024869855 ) ) ;
#38804 = CARTESIAN_POINT ( 'NONE',  ( 50.09664746341090336, -53.48905984871790054, -54.90216016554420264 ) ) ;
#38805 = ORIENTED_EDGE ( 'NONE', *, *, #40805, .T. ) ;
#38806 = CARTESIAN_POINT ( 'NONE',  ( 68.13393739769618662, -30.66618894467940137, -65.65000000000000568 ) ) ;
#38807 = ORIENTED_EDGE ( 'NONE', *, *, #45351, .F. ) ;
#38808 = CARTESIAN_POINT ( 'NONE',  ( 9.736265806055229177, -63.20621787679230152, -46.29822409738210354 ) ) ;
#38809 = ADVANCED_FACE ( 'NONE', ( #5077 ), #51126, .T. ) ;
#38810 = CARTESIAN_POINT ( 'NONE',  ( 15.09844379329638819, -7.705182437209532331, -47.25066575756055443 ) ) ;
#38811 = VERTEX_POINT ( 'NONE', #45810 ) ;
#38812 = DIRECTION ( 'NONE',  ( 1.000000000000000000, 0.000000000000000000, 0.000000000000000000 ) ) ;
#38813 = CARTESIAN_POINT ( 'NONE',  ( 57.35590716991889337, 18.90417298847060223, -52.61987026654610133 ) ) ;
#38814 = EDGE_CURVE ( 'NONE', #12694, #43570, #20563, .T. ) ;
#38815 = CARTESIAN_POINT ( 'NONE',  ( 53.27342892381020079, 19.23708225937859595, -77.09451959761469197 ) ) ;
#38816 = AXIS2_PLACEMENT_3D ( 'NONE', #26582, #49430, #42598 ) ;
#38817 = VERTEX_POINT ( 'NONE', #5972 ) ;
#38818 = AXIS2_PLACEMENT_3D ( 'NONE', #30463, #42804, #10573 ) ;
#38819 = CARTESIAN_POINT ( 'NONE',  ( 9.897519174578837564, -64.60056534141453710, -46.94956808238860191 ) ) ;
#38820 = CARTESIAN_POINT ( 'NONE',  ( 53.63393739769619373, -62.11618894467930119, 10.84999999999999964 ) ) ;
#38821 = CYLINDRICAL_SURFACE ( 'NONE', #16770, 7.910999999999997812 ) ;
#38822 = CARTESIAN_POINT ( 'NONE',  ( 57.28991729228579288, -50.57887465766769708, -53.44461810997250240 ) ) ;
#38823 = CARTESIAN_POINT ( 'NONE',  ( 13.26310097102749985, -23.34542035971960061, -68.40553316769378966 ) ) ;
#38824 = CARTESIAN_POINT ( 'NONE',  ( 14.06336589401369430, -23.32131682797999161, -48.09100240289522077 ) ) ;
#38825 = CARTESIAN_POINT ( 'NONE',  ( 47.05500271796362455, -38.25475083058559989, -55.04467339866013731 ) ) ;
#38826 = ORIENTED_EDGE ( 'NONE', *, *, #46040, .F. ) ;
#38827 = ORIENTED_EDGE ( 'NONE', *, *, #19397, .F. ) ;
#38828 = CARTESIAN_POINT ( 'NONE',  ( -22.76700179775898292, -12.96293114564705284, -54.70490354874866767 ) ) ;
#38829 = CARTESIAN_POINT ( 'NONE',  ( 9.907410570274159056, -11.52509404568959894, -51.41769413899928765 ) ) ;
#38830 = CARTESIAN_POINT ( 'NONE',  ( 52.57361112802249892, -49.85323755487960540, -48.51313449024529234 ) ) ;
#38831 = CARTESIAN_POINT ( 'NONE',  ( 9.011357356587289757, -17.82701623712219785, -32.14999999999999858 ) ) ;
#38832 = EDGE_CURVE ( 'NONE', #41343, #26710, #21929, .T. ) ;
#38833 = CARTESIAN_POINT ( 'NONE',  ( 9.366908763506170743, -15.61636271700460021, -33.45282021618999835 ) ) ;
#38834 = EDGE_CURVE ( 'NONE', #43823, #26115, #5312, .T. ) ;
#38835 = DIRECTION ( 'NONE',  ( 0.000000000000000000, -1.000000000000000000, 0.000000000000000000 ) ) ;
#38836 = CYLINDRICAL_SURFACE ( 'NONE', #43968, 50.00000000000000000 ) ;
#38837 =( BOUNDED_CURVE ( )  B_SPLINE_CURVE ( 3, ( #32363, #32620, #48382, #44448 ),
 .UNSPECIFIED., .F., .T. ) 
 B_SPLINE_CURVE_WITH_KNOTS ( ( 4, 4 ),
 ( 4.712388980384684345, 5.070260775219124660 ),
 .UNSPECIFIED. ) 
 CURVE ( )  GEOMETRIC_REPRESENTATION_ITEM ( )  RATIONAL_B_SPLINE_CURVE ( ( 1.000000000000000000, 0.9893557610490359977, 0.9893557610490359977, 1.000000000000000000 ) ) 
 REPRESENTATION_ITEM ( '' )  );
#38838 = CARTESIAN_POINT ( 'NONE',  ( 21.33354701331730752, -9.619326380292379852, -61.23501538585083637 ) ) ;
#38839 = CARTESIAN_POINT ( 'NONE',  ( 21.68697980347609899, -9.521400946021341127, -59.24287442375779733 ) ) ;
#38840 = CARTESIAN_POINT ( 'NONE',  ( 52.56521993351449851, -49.86179673305689874, -28.15000000000000213 ) ) ;
#38841 = CARTESIAN_POINT ( 'NONE',  ( 54.59220245897340362, -50.90304460341570092, -75.70160923548360188 ) ) ;
#38843 = CARTESIAN_POINT ( 'NONE',  ( 16.13393739769620083, -15.61618894467929941, -76.14999999999999147 ) ) ;
#38842 = CARTESIAN_POINT ( 'NONE',  ( -2.400008891863520066, 18.68547184855179921, -6.077313690069900076 ) ) ;
#38844 = CARTESIAN_POINT ( 'NONE',  ( 47.73667124825149699, -54.43832146008400485, -54.70375119057089819 ) ) ;
#38845 = CARTESIAN_POINT ( 'NONE',  ( 18.38973105523400164, -21.99613282959019500, -81.23899999999999011 ) ) ;
#38846 = AXIS2_PLACEMENT_3D ( 'NONE', #23526, #7067, #3647 ) ;
#38847 = ORIENTED_EDGE ( 'NONE', *, *, #24406, .T. ) ;
#38848 = CARTESIAN_POINT ( 'NONE',  ( -6.554330340120890774, -46.10323663931790605, -4.693995879374440072 ) ) ;
#38849 = CARTESIAN_POINT ( 'NONE',  ( 47.55845087153019790, 23.33810426020020046, -54.95948882862809626 ) ) ;
#38850 = CARTESIAN_POINT ( 'NONE',  ( -1.566062602304203022, -15.61618894467939889, -10.44999999999964757 ) ) ;
#38851 = DIRECTION ( 'NONE',  ( 1.000000000000000000, 2.460964292799963328E-14, 0.000000000000000000 ) ) ;
#38852 = CARTESIAN_POINT ( 'NONE',  ( 61.47032571389799926, 14.17707786984260032, -47.41712456996229719 ) ) ;
#38853 = CARTESIAN_POINT ( 'NONE',  ( 11.49145838457179991, 33.80527165212970431, -16.71591419048260008 ) ) ;
#38854 = CARTESIAN_POINT ( 'NONE',  ( 51.81471494547309931, 18.30023427017130189, -76.85964192801058914 ) ) ;
#38855 = CARTESIAN_POINT ( 'NONE',  ( 52.80356173049369772, 18.44276956637660092, -48.56462661435369910 ) ) ;
#38856 = DIRECTION ( 'NONE',  ( 0.8090169943749464521, -0.5877852522924744694, 0.000000000000000000 ) ) ;
#38857 = CARTESIAN_POINT ( 'NONE',  ( -0.04495657159227190586, -45.64487445774500429, -34.80555997329428664 ) ) ;
#38858 = CARTESIAN_POINT ( 'NONE',  ( 54.80579272659560530, 16.60235534783570088, -26.62706727043990185 ) ) ;
#38859 = CARTESIAN_POINT ( 'NONE',  ( 29.46622902366960162, 1.883811055320659955, -54.64999999999999858 ) ) ;
#38860 = APPLICATION_CONTEXT ( 'automotive_design' ) ;
#38861 = FACE_OUTER_BOUND ( 'NONE', #33302, .T. ) ;
#38862 = DIRECTION ( 'NONE',  ( 0.000000000000000000, 0.000000000000000000, -1.000000000000000000 ) ) ;
#38863 = DIRECTION ( 'NONE',  ( 0.000000000000000000, 0.000000000000000000, -1.000000000000000000 ) ) ;
#38864 = CARTESIAN_POINT ( 'NONE',  ( 71.00993340901570150, 1.383811055320669947, -60.91804007473620430 ) ) ;
#38865 = CARTESIAN_POINT ( 'NONE',  ( 11.13393739769619906, 32.09617326967790518, -43.91648406538870120 ) ) ;
#38866 = CARTESIAN_POINT ( 'NONE',  ( 72.72056432233058842, 1.396834109478129804, -62.44999999999999574 ) ) ;
#38867 = CARTESIAN_POINT ( 'NONE',  ( 66.13977606332380788, -31.03571436735869682, -17.02376530829800316 ) ) ;
#38868 = EDGE_LOOP ( 'NONE', ( #44854, #30926, #14620, #41240 ) ) ;
#38869 = EDGE_LOOP ( 'NONE', ( #32110, #27873, #47065, #45191, #42777, #161, #16236, #50979, #21868, #39490, #25694, #24441, #30925, #50765, #14235, #45685, #20014, #28678, #18097, #27761, #18994, #36269, #46547, #40371, #29660, #46697, #16320, #49437, #8114, #25292, #13274, #42857, #34193, #29502, #28693, #9824, #45759, #4864, #44888, #23435, #14556, #33684, #115, #50115, #28870, #6256, #20753, #2051, #19203, #25242, #26137, #26164 ) ) ;
#38870 = CIRCLE ( 'NONE', #35522, 17.19098300562509962 ) ;
#38871 = CARTESIAN_POINT ( 'NONE',  ( 41.36298005976649961, 12.80050257910570011, -3.553636961524439641 ) ) ;
#38872 = ADVANCED_FACE ( 'NONE', ( #42133 ), #15387, .T. ) ;
#38873 = CARTESIAN_POINT ( 'NONE',  ( 49.45810426794375303, -2.188232918999916343, -15.73681870539564365 ) ) ;
#38874 = ORIENTED_EDGE ( 'NONE', *, *, #35321, .F. ) ;
#38875 = CARTESIAN_POINT ( 'NONE',  ( 10.95435945972059955, -63.78130685611410655, -44.98684614314139907 ) ) ;
#38876 = CARTESIAN_POINT ( 'NONE',  ( 56.43568955072729665, -45.44241490114089999, -25.50436399627979966 ) ) ;
#38877 = CARTESIAN_POINT ( 'NONE',  ( 18.16485855442270392, -23.27956588526017256, -77.92524956637772959 ) ) ;
#38878 = DIRECTION ( 'NONE',  ( 0.8090169943749475623, 0.5877852522924730261, 0.000000000000000000 ) ) ;
#38879 = ORIENTED_EDGE ( 'NONE', *, *, #35559, .T. ) ;
#38880 = DIRECTION ( 'NONE',  ( 1.062456999999999985E-16, -7.719205000000000365E-17, 1.000000000000000000 ) ) ;
#38881 = CARTESIAN_POINT ( 'NONE',  ( 44.46199409210488085, 6.744907085701958849, -68.00970624157608313 ) ) ;
#38882 = CARTESIAN_POINT ( 'NONE',  ( 11.59229195909269983, 34.14674705323289317, -22.55625370316070288 ) ) ;
#38883 = ORIENTED_EDGE ( 'NONE', *, *, #46274, .F. ) ;
#38884 = CARTESIAN_POINT ( 'NONE',  ( 52.65940447408669911, -45.11618894467940066, -12.18415347133140081 ) ) ;
#38885 = B_SPLINE_CURVE_WITH_KNOTS ( 'NONE', 3,
 ( #34198, #5936, #9611, #34469 ),
 .UNSPECIFIED., .F., .F.,
 ( 4, 4 ),
 ( 0.4987209838069229795, 1.000000000000000000 ),
 .UNSPECIFIED. ) ;
#38886 = CARTESIAN_POINT ( 'NONE',  ( 68.13393739771808555, -29.66618894502720138, -65.65000000100739896 ) ) ;
#38887 = AXIS2_PLACEMENT_3D ( 'NONE', #23142, #46776, #31260 ) ;
#38888 = CARTESIAN_POINT ( 'NONE',  ( 16.08016673438230271, 19.80150180430160134, -20.14986617604239783 ) ) ;
#38889 = CARTESIAN_POINT ( 'NONE',  ( 21.13657264101065181, -20.24127860378771615, -50.69013539568535975 ) ) ;
#38890 = B_SPLINE_CURVE_WITH_KNOTS ( 'NONE', 3,
 ( #43569, #31992, #51176, #35700, #43314, #48013, #15527, #15271 ),
 .UNSPECIFIED., .F., .F.,
 ( 4, 2, 2, 4 ),
 ( 0.3562431257904284942, 0.5954397627775694923, 0.8830025937151522175, 1.000000000000000000 ),
 .UNSPECIFIED. ) ;
#38891 = CARTESIAN_POINT ( 'NONE',  ( 60.74065736930379700, -29.42750435924840247, -15.90652919026539891 ) ) ;
#38892 = CARTESIAN_POINT ( 'NONE',  ( 11.97534086647365825, -10.20481231275635459, -63.74448752987081690 ) ) ;
#38893 = CARTESIAN_POINT ( 'NONE',  ( 46.35275103504449845, -52.90993241930539881, -76.14999999999999147 ) ) ;
#38894 = CARTESIAN_POINT ( 'NONE',  ( 43.03640022808939847, 13.88381105527780157, -6.890438909537429879 ) ) ;
#38895 = EDGE_CURVE ( 'NONE', #13523, #5090, #1425, .T. ) ;
#38896 = EDGE_CURVE ( 'NONE', #26692, #6571, #27681, .T. ) ;
#38897 = CARTESIAN_POINT ( 'NONE',  ( 10.00991122538783173, 23.91216740073585001, -46.09048026812309473 ) ) ;
#38898 = CARTESIAN_POINT ( 'NONE',  ( 58.53216149070850349, 13.88381120887479980, -25.55155896066500176 ) ) ;
#38899 = CARTESIAN_POINT ( 'NONE',  ( 15.00846012470890045, -23.78417636420700276, -34.05125434552689967 ) ) ;
#38900 = ORIENTED_EDGE ( 'NONE', *, *, #10767, .F. ) ;
#38901 = CARTESIAN_POINT ( 'NONE',  ( 29.52882095054619782, 21.88381105532300097, -74.14999999999999147 ) ) ;
#38902 = AXIS2_PLACEMENT_3D ( 'NONE', #13295, #49203, #16695 ) ;
#38903 = CARTESIAN_POINT ( 'NONE',  ( -5.957774818403610340, -47.45617016592679960, -6.636813055207410272 ) ) ;
#38904 = CARTESIAN_POINT ( 'NONE',  ( 76.56166476258249531, 9.631681111976121201, -13.86454137039240031 ) ) ;
#38905 = CARTESIAN_POINT ( 'NONE',  ( 75.38195435473652140, 13.04593086575056127, -13.74600147056045607 ) ) ;
#38906 = CARTESIAN_POINT ( 'NONE',  ( 20.13393739768959634, -55.41568642894479524, -74.14999999999999147 ) ) ;
#38907 = CARTESIAN_POINT ( 'NONE',  ( 12.77676462293392134, -55.47504473345251341, -75.60405384314019273 ) ) ;
#38908 = FACE_OUTER_BOUND ( 'NONE', #12425, .T. ) ;
#38909 = CARTESIAN_POINT ( 'NONE',  ( 82.46545078568199472, -45.09314778790560041, -46.44237448698110171 ) ) ;
#38910 = CARTESIAN_POINT ( 'NONE',  ( 57.36488636042089695, -50.16807177143650165, -52.65750501476470191 ) ) ;
#38911 = CARTESIAN_POINT ( 'NONE',  ( 41.02005863531599772, 13.11595598970779974, -4.033360981351730601 ) ) ;
#38912 = DIRECTION ( 'NONE',  ( 0.000000000000000000, 0.000000000000000000, -1.000000000000000000 ) ) ;
#38913 = CARTESIAN_POINT ( 'NONE',  ( 2.633937397696199945, -15.61618894467929763, -8.655000000000001137 ) ) ;
#38914 = DIRECTION ( 'NONE',  ( 1.000000000000000000, 0.000000000000000000, 0.000000000000000000 ) ) ;
#38915 = CARTESIAN_POINT ( 'NONE',  ( 16.13393739769620083, -15.61618894467929941, -35.02873218748179340 ) ) ;
#38916 = CARTESIAN_POINT ( 'NONE',  ( 75.99395259271645386, -43.32339650468484393, -13.62990582981167620 ) ) ;
#38917 = CARTESIAN_POINT ( 'NONE',  ( 18.04837480293360130, -52.31213937195320085, -75.84958893011570069 ) ) ;
#38918 = CARTESIAN_POINT ( 'NONE',  ( 45.25256250357250565, -43.53500084062090281, -5.388698120161880212 ) ) ;
#38919 = CARTESIAN_POINT ( 'NONE',  ( 8.891688449396310645, -17.36448082797300074, -67.99194462183578480 ) ) ;
#38920 = CARTESIAN_POINT ( 'NONE',  ( 63.99198253403570646, 1.457833794292699992, -61.64494777836840456 ) ) ;
#38921 = ORIENTED_EDGE ( 'NONE', *, *, #43818, .F. ) ;
#38922 = CARTESIAN_POINT ( 'NONE',  ( 7.712470290556179719, 30.55595177311299793, -15.52620908427480018 ) ) ;
#38923 = DIRECTION ( 'NONE',  ( 0.000000000000000000, 0.000000000000000000, -1.000000000000000000 ) ) ;
#38924 = CARTESIAN_POINT ( 'NONE',  ( 72.83834671619840151, 1.382830464309369844, -68.61079447352989291 ) ) ;
#38925 = CARTESIAN_POINT ( 'NONE',  ( 45.38228619634400474, 8.823823693349686081, -59.95777824142523116 ) ) ;
#38926 = CARTESIAN_POINT ( 'NONE',  ( -0.007164427059776000244, -4.186223695871990280, -34.77269723891829756 ) ) ;
#38927 = CARTESIAN_POINT ( 'NONE',  ( 42.89815834353850477, -45.52996223267120257, -7.114957886879119897 ) ) ;
#38928 = VERTEX_POINT ( 'NONE', #43682 ) ;
#38929 = ORIENTED_EDGE ( 'NONE', *, *, #26161, .T. ) ;
#38930 = ORIENTED_EDGE ( 'NONE', *, *, #25238, .F. ) ;
#38931 = EDGE_CURVE ( 'NONE', #46311, #38817, #19047, .T. ) ;
#38932 = ORIENTED_EDGE ( 'NONE', *, *, #26608, .T. ) ;
#38933 = FACE_OUTER_BOUND ( 'NONE', #4365, .T. ) ;
#38934 = CARTESIAN_POINT ( 'NONE',  ( 22.84324496511920088, -11.76751259666689897, -81.23899999999999011 ) ) ;
#38935 = EDGE_CURVE ( 'NONE', #38545, #2764, #47616, .T. ) ;
#38936 = CARTESIAN_POINT ( 'NONE',  ( 16.13393739769620083, -15.61618894467929941, 36.77166666666649775 ) ) ;
#38937 = ADVANCED_FACE ( 'NONE', ( #11464 ), #22260, .T. ) ;
#38938 = VERTEX_POINT ( 'NONE', #31085 ) ;
#38939 = EDGE_CURVE ( 'NONE', #21117, #17335, #39857, .T. ) ;
#38940 = CARTESIAN_POINT ( 'NONE',  ( 64.93393739769619799, 1.883811055320669947, -70.34999999999999432 ) ) ;
#38941 = ORIENTED_EDGE ( 'NONE', *, *, #36951, .T. ) ;
#38942 = DIRECTION ( 'NONE',  ( 0.2993038002561358990, -0.8275125542569267134, 0.4750160078349067727 ) ) ;
#38943 = VECTOR ( 'NONE', #36676, 1000.000000000000000 ) ;
#38944 = DIRECTION ( 'NONE',  ( 0.000000000000000000, 0.000000000000000000, 1.000000000000000000 ) ) ;
#38945 = ORIENTED_EDGE ( 'NONE', *, *, #13327, .T. ) ;
#38946 = CARTESIAN_POINT ( 'NONE',  ( 61.28610861176739633, 13.99802266614350010, -28.15000000000000213 ) ) ;
#38947 = CARTESIAN_POINT ( 'NONE',  ( 52.25623532178450148, -51.32859135100709835, -75.95837140036390167 ) ) ;
#38948 = CARTESIAN_POINT ( 'NONE',  ( 60.66089622436710016, 14.32868137727570002, -47.20375295697429863 ) ) ;
#38949 = EDGE_CURVE ( 'NONE', #17454, #16042, #8279, .T. ) ;
#38950 = CARTESIAN_POINT ( 'NONE',  ( 21.75904242978619507, -11.76187703652407279, -40.26184854905846322 ) ) ;
#38951 = EDGE_CURVE ( 'NONE', #35735, #17152, #23931, .T. ) ;
#38952 = CARTESIAN_POINT ( 'NONE',  ( 41.36297991754150161, -44.03288059546810018, -3.553637027260359904 ) ) ;
#38953 = CARTESIAN_POINT ( 'NONE',  ( 16.13393739769620083, -15.61618894467929941, -81.65000000000000568 ) ) ;
#38954 = CARTESIAN_POINT ( 'NONE',  ( -10.88693382329749859, 11.10980032629789882, -6.245353000315719605 ) ) ;
#38955 = DIRECTION ( 'NONE',  ( 0.000000000000000000, 0.000000000000000000, 1.000000000000000000 ) ) ;
#38956 = DIRECTION ( 'NONE',  ( 0.2260571801428170324, 2.970872000000000522E-15, -0.9741140340359940586 ) ) ;
#38957 = PLANE ( 'NONE',  #22663 ) ;
#38958 = CARTESIAN_POINT ( 'NONE',  ( 16.55472973932799974, -7.779755955850329308, -56.80458145132549674 ) ) ;
#38959 = ORIENTED_EDGE ( 'NONE', *, *, #37362, .F. ) ;
#38960 = CARTESIAN_POINT ( 'NONE',  ( 8.815605938792600682, 32.05029769220720226, -46.67186391141279955 ) ) ;
#38961 = CARTESIAN_POINT ( 'NONE',  ( 57.55751162087899786, 19.32515479037619954, -53.43780795140229856 ) ) ;
#38962 = CARTESIAN_POINT ( 'NONE',  ( 71.60705152684150221, 1.024253516290730026, -70.53167046690928998 ) ) ;
#38963 = CARTESIAN_POINT ( 'NONE',  ( 45.06222871821497478, -40.03483142178188814, -61.51087723771117055 ) ) ;
#38964 = CARTESIAN_POINT ( 'NONE',  ( 13.73505343097469833, 18.97478628885919960, -20.93075220000899961 ) ) ;
#38966 = EDGE_CURVE ( 'NONE', #33975, #12711, #8065, .T. ) ;
#38965 = CARTESIAN_POINT ( 'NONE',  ( 20.06281976506910070, -10.10654536788180025, -32.14999999999999858 ) ) ;
#38967 = AXIS2_PLACEMENT_3D ( 'NONE', #33268, #278, #44559 ) ;
#38968 = CARTESIAN_POINT ( 'NONE',  ( 8.738424198519890496, -18.52118839557869023, -32.38844566117526824 ) ) ;
#38969 = CARTESIAN_POINT ( 'NONE',  ( 63.22343968446819673, 0.9036513197889520788, -69.09785636402040154 ) ) ;
#38970 = CARTESIAN_POINT ( 'NONE',  ( 47.81064057165269787, -54.45306024599980077, -55.02164417520120310 ) ) ;
#38971 = AXIS2_PLACEMENT_3D ( 'NONE', #21970, #49016, #12852 ) ;
#38972 = DIRECTION ( 'NONE',  ( 0.000000000000000000, 0.000000000000000000, -1.000000000000000000 ) ) ;
#38973 = CARTESIAN_POINT ( 'NONE',  ( -7.471208905559357127, -45.39622512240971730, -4.913224500014766960 ) ) ;
#38974 = CARTESIAN_POINT ( 'NONE',  ( 24.04493741069041235, -16.65172996398426264, -37.54933800668455035 ) ) ;
#38975 = CARTESIAN_POINT ( 'NONE',  ( 47.68932896513950226, 23.27841431174140041, -55.03972088634769477 ) ) ;
#38976 = ORIENTED_EDGE ( 'NONE', *, *, #50867, .T. ) ;
#38977 = CARTESIAN_POINT ( 'NONE',  ( 22.38708172792839690, -18.87820445042670059, -73.00023116938359635 ) ) ;
#38978 = ORIENTED_EDGE ( 'NONE', *, *, #38745, .T. ) ;
#38979 = CARTESIAN_POINT ( 'NONE',  ( 71.51817256006181367, 0.9307121176571799825, -70.60454574395809857 ) ) ;
#38980 = CARTESIAN_POINT ( 'NONE',  ( 60.89998638923569985, -45.43270080629340413, -46.98170749212690822 ) ) ;
#38981 = DIRECTION ( 'NONE',  ( 0.6801873868961743064, 0.000000000000000000, -0.7330382791555664079 ) ) ;
#38982 = DIRECTION ( 'NONE',  ( 0.000000000000000000, 0.000000000000000000, -1.000000000000000000 ) ) ;
#38984 = DIRECTION ( 'NONE',  ( 0.000000000000000000, -1.000000000000000000, 0.000000000000000000 ) ) ;
#38983 = DIRECTION ( 'NONE',  ( 1.000000000000000000, 5.245810363639075036E-26, 1.180619220495489865E-10 ) ) ;
#38985 = CARTESIAN_POINT ( 'NONE',  ( 22.87259979537421728, -16.95485826009387864, -78.91015894931038588 ) ) ;
#38986 = LINE ( 'NONE', #46080, #35128 ) ;
#38987 = DIRECTION ( 'NONE',  ( 0.000000000000000000, 0.000000000000000000, -1.000000000000000000 ) ) ;
#38988 = B_SPLINE_SURFACE_WITH_KNOTS ( 'NONE', 3, 3, ( 
 ( #24862, #21709, #9170, #40873, #4975, #37720, #1815, #20945, #17545, #1042, #17036, #32988, #25642, #49530, #13119, #33255, #37458, #29072, #21459, #41386, #45066, #25128, #41645, #25385, #41134, #33517, #9936, #5245, #21199, #17294, #33770, #9682, #37204, #29831, #49781, #41911, #1304, #49272, #5503, #13365, #29330, #45331, #9436, #13621, #29583, #14386, #6272, #7050, #23000, #3117, #42952, #47148, #19084, #22488, #2858, #50033, #30864, #30091, #42173, #10719, #35060, #18057, #18822, #34023, #26946, #14126, #2597, #38494, #18570, #39021, #46117, #18305, #10202, #51065, #46893, #26162, #22230, #14643, #34276, #50809, #7302, #15165, #2078, #26674, #34547, #42437, #30611, #23254, #50299, #38238, #22745, #2331, #30350, #34806, #11238, #38763, #50551, #14899, #27198, #46378, #10982, #10463, #26418, #46634, #42696, #31123, #6526, #6792, #43211, #51835, #47652, #20107, #3888, #20358, #16443, #32397, #47908, #4389, #40297, #39269, #19603, #35328, #3373, #51327, #36345, #19854, #40041, #8072, #44224, #11758, #455, #48158, #48418, #27457, #35844, #39530, #12262, #43967, #15678, #12519, #204, #12011, #36099, #8590, #32142, #24277, #8325, #24017, #16182, #15934, #51580, #28486, #35592, #4131, #27964, #3631, #31377, #28223, #44485, #19345, #15426, #31633, #47404, #11500, #43460, #7561, #23509, #31891, #27715, #43716, #7817, #23770, #39782, #37162, #32677, #997, #21661, #29282, #28762, #1259, #13574, #20900, #29538, #41342, #5459, #13075, #33210, #37413, #45542, #21412, #37667, #1515, #16996, #17500, #32944, #1771, #33469, #9637, #49487, #24555, #17246, #48971, #4928, #44764, #29028, #45025, #17752, #9124, #45284, #48704, #44503, #12808, #25593, #8867, #49228, #41598, #5706, #33722, #25077, #12538, #28505, #8605, #40568, #41092, #9393, #4664, #20637, #36624, #21155, #726, #5203, #25341, #13322, #16721, #24820, #40829, #36897, #13826, #26901, #46848, #34758, #30042, #42385, #34501, #50763, #6224, #46067, #7005, #19039, #37934, #14339, #26113, #14857, #14597, #22181, #50507, #2286, #30566, #18260, #46327, #10155, #29783, #34229, #38977, #2813, #42124, #45802, #21923, #38718, #18782, #49736, #46587, #3070, #9891, #33974, #6746, #10675, #41861, #30308, #18528, #30820, #42908, #22955, #6482, #10935, #25847, #5965, #38191, #2029, #18009, #49988, #14081, #10416, #26631, #42648, #50251, #26369, #22440, #22702, #38447, #2549, #31587, #35284, #8023, #39739, #11455, #36052, #47866, #7774, #15890, #4344, #27924, #20060, #39997, #3842, #11969, #47608 ),
 ( #43926, #35015, #32097, #23973, #44179, #48116, #43164, #23724, #3324, #40252, #51282, #31333, #4086, #39488, #47359, #39227, #162, #16137, #12215, #28177, #8278, #24227, #3586, #35803, #31078, #51019, #11194, #23207, #43674, #15119, #47105, #51787, #27156, #7258, #19301, #35548, #19558, #51538, #15379, #27413, #43416, #7517, #23465, #15635, #11708, #27671, #19815, #31845, #17186, #25536, #37353, #20312, #28959, #40764, #8801, #32874, #41540, #665, #411, #41024, #36301, #12470, #1194, #29478, #5140, #4865, #21094, #45484, #4595, #29217, #40506, #20570, #20832, #36830, #21349, #16398, #32354, #44440, #48907, #28694, #33143, #933, #9582, #45224, #1452, #25279, #48373, #9061, #24754, #12740, #16655, #16930, #13005, #28438, #44959, #49169, #36563, #8546, #32612, #41283, #48639, #25009, #33407, #13521, #17440, #37097, #49425, #13262, #24490, #9332, #5393, #44697, #10623, #38667, #42593, #14285, #22648, #10098, #22388, #26057, #50193, #38392, #42066, #25790, #21603, #34704, #2753, #6689, #37880, #30252, #42329, #18725, #14026, #1972, #14803, #26845, #45744, #22127, #33919, #50704, #2491, #29985, #6429, #6168, #18471, #38134, #2234, #17951, #37605, #18210, #46790, #26577, #49936, #1713, #29728, #46535, #30768, #5656, #34444, #10882, #17695, #41799, #14543, #50453, #49681, #34174, #26321, #46008, #10359, #46273, #5905, #13774, #30512, #33665, #9838, #21869, #19243, #39685, #32750, #20709, #4742, #31537, #23412, #19759, #31027, #35225, #3532, #36700, #15583, #11137, #31276, #801, #7724, #7201, #47555, #43872, #51231, #7970, #35750, #51732, #43366, #11651, #15827, #23920, #31792, #16802, #47810, #47309, #11916, #11397, #39943, #27870, #3010, #27616, #27359, #15323, #23156, #7458, #39433, #48777, #19503, #23668, #27107, #22902, #43110, #12881, #39173, #43622, #42855, #6951, #38919, #35493, #18982, #34963, #50960, #15059, #51483, #3790, #47052, #3268, #13904, #37489, #45882, #33286, #45615, #49304, #21490, #9714, #13399, #49042, #44842, #6045, #25930, #29861, #9204, #1590, #13651, #9969, #37237, #25156, #38011, #50063, #17066, #45363, #5275, #41944, #25674, #1335, #29612, #29357, #41676, #9467, #25414, #41162, #8947, #41416, #18085, #33801, #21225, #24889, #1068, #17828, #49811, #28838, #5783, #34054, #40901, #13149, #37752, #21744, #20972, #5535, #49565, #17324, #33547, #17578, #29099, #36972, #1849, #22002, #5011, #33018, #2107, #45097, #3408, #43245, #27229, #2889, #46667, #42987, #2361, #42468, #26709, #7334, #38796, #34316, #2630 ),
 ( #14674, #34840, #39054, #15194, #23032, #23282, #3148, #18602, #19115, #34579, #39304, #35095, #19375, #31154, #14159, #22776, #50584, #30643, #42728, #35358, #46409, #46147, #50839, #30127, #6303, #46924, #10236, #14931, #10750, #30896, #26195, #50329, #51095, #14416, #30385, #6823, #18855, #47181, #42205, #22262, #38269, #11009, #22522, #26978, #7082, #11269, #18338, #10496, #26453, #6556, #38532, #51358, #35626, #47436, #15457, #11530, #48190, #3922, #27997, #47942, #36129, #11790, #28254, #4163, #32174, #23541, #19883, #51613, #20139, #12044, #31662, #12295, #24051, #15967, #8106, #31408, #234, #44253, #8361, #40070, #16217, #31921, #27749, #24310, #43747, #27488, #43495, #3664, #39559, #51869, #7595, #19635, #15706, #47686, #7849, #23798, #39813, #44002, #35874, #14580, #51519, #46571, #42631, #39205, #50742, #6728, #50490, #51265, #15360, #47342, #35266, #39469, #11438, #14840, #47087, #42368, #23189, #22425, #34484, #3050, #27397, #10399, #11176, #26353, #19284, #6469, #46831, #30802, #10919, #31316, #38431, #10658, #2533, #43398, #3305, #18511, #30546, #6986, #26616, #43146, #22684, #38704, #7241, #35529, #23446, #7497, #34996, #26881, #3571, #2792, #18764, #22939, #19538, #19020, #34737, #42892, #15619, #27143, #38958, #51001, #46310, #15100, #31061, #8525, #24473, #32080, #394, #4577, #32592, #40485, #40748, #20550, #20041, #36545, #142, #4847, #651, #48622, #16634, #43656, #20295, #36034, #23956, #11950, #16119, #48098, #20814, #12197, #12450, #51769, #11691, #15873, #12722, #27905, #36283, #44679, #24733, #28677, #28158, #8782, #36808, #914, #31572, #44162, #28420, #47592, #27653, #7758, #40235, #23706, #8258, #48356, #24211, #4325, #44424, #16378, #31828, #39720, #3824, #19797, #35786, #43909, #32336, #47844, #8003, #39978, #4072, #26037, #38116, #5122, #33389, #45205, #17931, #33647, #41266, #17679, #21331, #49666, #37337, #13504, #49151, #48884, #1438, #6150, #21851, #9316, #12988, #41010, #5887, #37858, #16909, #1695, #22105, #32855, #1175, #25774, #13754, #9044, #49408, #37584, #13247, #21586, #41522, #17170, #24990, #41781, #25516, #28939, #29711, #17423, #29460, #29197, #44943, #45465, #21075, #1954, #25260, #37078, #33122, #33902, #49914, #5375, #45722, #9564, #5640, #9823, #14008, #29968, #45986, #10078, #42047, #34421, #6928, #26823, #2463, #46251, #27085, #10856, #23385, #14267, #30489, #50939, #43344, #31255, #15300, #42833, #34680, #31004, #42308, #46512, #14779, #47286, #22882, #22367, #42571, #11376, #18960 ),
 ( #43088, #3247, #11116, #27340, #7180, #6663, #23137, #22628, #7437, #39151, #19219, #35205, #30234, #38899, #38644, #10601, #50432, #2732, #18705, #2212, #50681, #34940, #38372, #34155, #18451, #51207, #14521, #2987, #18190, #50170, #10340, #30747, #26298, #47031, #6408, #26557, #46770, #15035, #44359, #20489, #24411, #48043, #4516, #43850, #4265, #7946, #32019, #20235, #23896, #7701, #3511, #16570, #36479, #40423, #19735, #12142, #24150, #585, #47786, #35728, #48553, #8721, #27591, #4017, #15805, #32525, #36224, #11894, #40170, #39921, #43599, #8464, #12661, #28614, #28354, #44615, #39410, #19978, #335, #35469, #16318, #15561, #23645, #28097, #19478, #51461, #32273, #31515, #12391, #47533, #35972, #91, #16062, #11630, #39661, #3767, #51711, #31766, #48295, #27848, #44105, #8204, #40943, #21530, #29904, #41718, #24669, #33327, #45139, #13189, #37274, #45921, #5054, #4783, #45402, #40684, #16843, #5574, #33840, #9507, #9250, #25454, #49855, #8985, #33590, #44880, #24930, #25199, #41205, #25711, #20752, #36739, #48815, #1374, #33060, #37527, #5314, #5825, #1891, #17869, #49344, #21788, #37797, #846, #21014, #32792, #12923, #28878, #13945, #21270, #41458, #1630, #29652, #49085, #37012, #49605, #1111, #17107, #17361, #29139, #13692, #29402, #13442, #17621, #45656, #9759, #42769, #31190, #2927, #46971, #14973, #30688, #38839, #22561, #22303, #30940, #2397, #46711, #39093, #22041, #41986, #10537, #11054, #18896, #10012, #7125, #34882, #19159, #23076, #18129, #50621, #30172, #15241, #10275, #6344, #50881, #14457, #38310, #27020, #25973, #3188, #43028, #35138, #51143, #34092, #14718, #46192, #6088, #26238, #18381, #38055, #30425, #34356, #14202, #2149, #50106, #42245, #50373, #46451, #26494, #42511, #10796, #6599, #38577, #2671, #18643, #34618, #26756, #6869, #22817, #27276, #20177, #11311, #47725, #31700, #11831, #274, #43285, #11569, #7374, #48235, #40109, #19421, #23323, #7888, #27529, #44041, #525, #12330, #47222, #3961, #15747, #35668, #23834, #16511, #43537, #39348, #16004, #3448, #35400, #28037, #4459, #31961, #27790, #47981, #20430, #31449, #4205, #15497, #47477, #43786, #39856, #28290, #51397, #7636, #23582, #19921, #3703, #8144, #35914, #44293, #24350, #40364, #31, #8401, #36417, #39599, #19671, #51652, #12083, #24089, #36166, #16257, #32212, #1313, #37467, #4987, #45595, #41394, #49539, #20686, #29080, #32727, #5511, #37213, #8924, #33525, #45339, #5253, #13376, #1825, #25392, #17557, #1566, #17303, #9445, #45073 ) ),
 .UNSPECIFIED., .F., .F., .F.,
 ( 4, 4 ),
 ( 4, 1, 1, 1, 1, 1, 1, 1, 1, 1, 1, 1, 1, 1, 1, 1, 1, 1, 1, 1, 1, 1, 1, 1, 1, 1, 1, 1, 1, 1, 1, 1, 1, 1, 1, 1, 1, 1, 1, 1, 1, 1, 1, 1, 1, 1, 1, 1, 1, 1, 1, 1, 1, 1, 1, 1, 1, 1, 1, 1, 1, 1, 1, 1, 1, 1, 1, 1, 1, 1, 1, 1, 1, 1, 1, 1, 1, 1, 1, 1, 1, 1, 1, 1, 1, 1, 1, 1, 1, 1, 1, 1, 1, 1, 1, 1, 1, 1, 1, 1, 1, 1, 1, 1, 1, 1, 1, 1, 1, 1, 1, 1, 1, 1, 1, 1, 1, 1, 1, 1, 1, 1, 1, 1, 1, 1, 1, 1, 1, 1, 1, 1, 1, 1, 1, 1, 1, 1, 1, 1, 1, 1, 1, 1, 1, 1, 1, 1, 1, 1, 1, 1, 1, 1, 1, 1, 1, 1, 1, 1, 1, 1, 1, 1, 1, 1, 1, 1, 1, 1, 1, 1, 1, 1, 1, 1, 1, 1, 1, 1, 1, 1, 1, 1, 1, 1, 1, 1, 1, 1, 1, 1, 1, 1, 1, 1, 1, 1, 1, 1, 1, 1, 1, 1, 1, 1, 1, 1, 1, 1, 1, 1, 1, 1, 1, 1, 1, 1, 1, 1, 1, 1, 1, 1, 1, 1, 1, 1, 1, 1, 1, 1, 1, 1, 1, 1, 1, 1, 1, 1, 1, 1, 1, 1, 1, 1, 1, 1, 1, 1, 1, 1, 1, 1, 1, 1, 1, 1, 1, 1, 1, 1, 1, 1, 1, 1, 1, 1, 1, 1, 1, 1, 1, 1, 1, 1, 1, 1, 1, 1, 1, 1, 1, 1, 1, 1, 1, 1, 1, 1, 1, 1, 1, 1, 1, 1, 1, 1, 1, 1, 1, 1, 1, 1, 1, 1, 1, 1, 1, 1, 1, 1, 1, 1, 4 ),
 ( 0.000000000000000000, 0.1320977415905860153 ),
 ( 8.301129254626310683, 8.798876478335710516, 9.296623702045119231, 9.794370925754529722, 10.29211814946389936, 10.78986537317329919, 11.28761259688270080, 11.78535982059210063, 12.28310704430160172, 12.78085426801099977, 13.27860149172039961, 13.77634871542980122, 14.27409593913919927, 14.77184316284859911, 15.26959038655800072, 15.76733761026740055, 16.26508483397680038, 16.76283205768620022, 17.26057928139560005, 17.75832650510499988, 18.25607372881439971, 18.75382095252380310, 19.25156817623319938, 19.74931539994259921, 20.24706262365200260, 20.74480984736149836, 21.24255707107090174, 21.74030429478030157, 22.23805151848970141, 22.73579874219910124, 23.23354596590850107, 23.73129318961789735, 24.22904041332729719, 24.72678763703670057, 25.22453486074610041, 25.72228208445550024, 26.22002930816490007, 26.71777653187429991, 27.21552375558369974, 27.71327097929309957, 28.21101820300250296, 28.70876542671189924, 29.20651265042139855, 29.70425987413079838, 30.20200709784019821, 30.69975432154959805, 31.19750154525900143, 31.69524876896840127, 32.19299599267780110, 32.69074321638719738, 33.18849044009660076, 33.68623766380599704, 34.18398488751540043, 34.68173211122479671, 35.17947933493420010, 35.67722655864360348, 36.17497378235299976, 36.67272100606240315, 37.17046822977179943, 37.66821545348130229, 38.16596267719069857, 38.66370990090010196, 39.16145712460949824, 39.65920434831890162, 40.15695157202829790, 40.65469879573769418, 41.15244601944709757, 41.65019324315649385, 42.14794046686590434, 42.64568769057530062, 43.14343491428470401, 43.64118213799410029, 44.13892936170350367, 44.63667658541289995, 45.13442380912230334, 45.63217103283169962, 46.12991825654119538, 46.62766548025059876, 47.12541270395999504, 47.62315992766939843, 48.12090715137879471, 48.61865437508820520, 49.11640159879760148, 49.61414882250700487, 50.11189604621640115, 50.60964326992579743, 51.10739049363520081, 51.60513771734459709, 52.10288494105400048, 52.60063216476339676, 53.09837938847280014, 53.59612661218219642, 54.09387383589159981, 54.59162105960110267, 55.08936828331050606, 55.58711550701990234, 56.08486273072930572, 56.58260995443870200, 57.08035717814809828, 57.57810440185750167, 58.07585162556689795, 58.57359884927630134, 59.07134607298569762, 59.56909329669510100, 60.06684052040449728, 60.56458774411389356, 61.06233496782330405, 61.56008219153270034, 62.05782941524210372, 62.55557663895150000, 63.05332386266090339, 63.55107108637029967, 64.04881831007979542, 64.54656553378920592, 65.04431275749860220, 65.54205998120799848, 66.03980720491739476, 66.53755442862680525, 67.03530165233620153, 67.53304887604559781, 68.03079609975499409, 68.52854332346439037, 69.02629054717380086, 69.52403777088319714, 70.02178499459259342, 70.51953221830200391, 71.01727944201140019, 71.51502666572079647, 72.01277388943020696, 72.51052111313960324, 73.00826833684909900, 73.50601556055850949, 74.00376278426789156, 74.50151000797730205, 74.99925723168669833, 75.49700445539609461, 75.99475167910550510, 76.49249890281490138, 76.99024612652429767, 77.48799335023369395, 77.98574057394310444, 78.48348779765250072, 78.98123502136189700, 79.47898224507130749, 79.97672946878068956, 80.47447669249010005, 80.97222391619961002, 81.46997113990889261, 81.96771836361840258, 82.46546558732779886, 82.96321281103719514, 83.46096003474660563, 83.95870725845600191, 84.45645448216539819, 84.95420170587479447, 85.45194892958420496, 85.94969615329360124, 86.44744337700299752, 86.94519060071240801, 87.44293782442179008, 87.94068504813120057, 88.43843227184059685, 88.93617949555000735, 89.43392671925940363, 89.93167394296891359, 90.42942116667829566, 90.92716839038770615, 91.42491561409710243, 91.92266283780649871, 92.42041006151590921, 92.91815728522529128, 93.41590450893470177, 93.91365173264409805, 94.41139895635349433, 94.90914618006290482, 95.40689340377230110, 95.90464062748169738, 96.40238785119109366, 96.90013507490050415, 97.39788229860990043, 97.89562952231929671, 98.39337674602870720, 98.89112396973820296, 99.38887119344759924, 99.88661841715700973, 100.3843656408659939, 100.8821128645760012, 101.3798600882849996, 101.8776073119949928, 102.3753545357040053, 102.8731017594130037, 103.3708489831229969, 103.8685962068319952, 104.3663434305420026, 104.8640906542510010, 105.3618378779599993, 105.8595851016700067, 106.3573323253789908, 106.8550795490889982, 107.3528267727979966, 107.8505739965069949, 108.3483212202170023, 108.8460684439259865, 109.3438156676359938, 109.8415628913450064, 110.3393101150540048, 110.8370573387639979, 111.3348045624730105, 111.8325517861829894, 112.3302990098920020, 112.8280462336020094, 113.3257934573109935, 113.8235406810200061, 114.3212879047299992, 114.8190351284389976, 115.3167823521490050, 115.8145295758580033, 116.3122767995670017, 116.8100240232769949, 117.3077712469860074, 117.8055184706960006, 118.3032656944049990, 118.8010129181139973, 119.2987601418239905, 119.7965073655330031, 120.2942545892429962, 120.7920018129519946, 121.2897490366610072, 121.7874962603710003, 122.2852434840799987, 122.7829907077900060, 123.2807379314990044, 123.7784851552080028, 124.2762323789180101, 124.7739796026270085, 125.2717268263370016, 125.7694740500460000, 126.2672212737549984, 126.7649684974650057, 127.2627157211740041, 127.7604629448839972, 128.2582101685930240, 128.7559573923030030, 129.2537046160119871, 129.7514518397209997, 130.2491990634310071, 130.7469462871399912, 131.2446935108499986, 131.7424407345590112, 132.2401879582679953, 132.7379351819779743, 133.2356824056870153, 133.7334296293969942, 134.2311768531059784, 134.7289240768150194, 135.2266713005249983, 135.7244185242340109, 136.2221657479440182, 136.7199129716530024, 137.2176601953619866, 137.7154074190719939, 138.2131546427810065, 138.7109018664909854, 139.2086490901999980, 139.7063963139089822, 140.2041435376189895, 140.7018907613280021, 141.1996379850380094, 141.6973852087470220, 142.1951324324560062, 142.6928796561659851, 143.1906268798749977, 143.6883741035850051, 144.1861213272939892, 144.6838685510039966, 145.1816157747130092, 145.6793629984219933, 146.1771102221320007, 146.6748574458410133, 147.1726046695509922, 147.6703518932600048, 148.1680991169690174, 148.6658463406789963, 149.1635935643879805, 149.6613407880980162, 150.1590880118070004, 150.6568352355159846, 151.1545824592260203, 151.6523296829350045, 152.1500769066449834, 152.6478241303539960, 153.1455713540630086, 153.6433185777729875, 154.1410658014820001, 154.6388130251920074, 155.1365602489009916, 155.6343074726100042, 156.1320546963200115, 156.6298019200289957, 157.1275491437390031, 157.6252963674480156, 158.1230435911569998, 158.6207908148670072, 159.1185380385759913, 159.6162852622859987, 160.1140324859950113, 160.6117797097039954, 161.1095269334140028, 161.6072741571230154, 162.1050213808329943, 162.6027686045419784, 163.1005158282520142, 163.5982630519609984, 164.0960102756699825, 164.5937574993799899 ),
 .UNSPECIFIED. ) ;
#38989 = ORIENTED_EDGE ( 'NONE', *, *, #12133, .T. ) ;
#38990 = DIRECTION ( 'NONE',  ( 1.000000000000000000, 0.000000000000000000, 0.000000000000000000 ) ) ;
#38991 = EDGE_LOOP ( 'NONE', ( #28664, #32678, #7748, #22441 ) ) ;
#38992 = EDGE_LOOP ( 'NONE', ( #11870, #34756, #18245, #18750, #36406 ) ) ;
#38993 = DIRECTION ( 'NONE',  ( 1.000000000000000000, 0.000000000000000000, 0.000000000000000000 ) ) ;
#38994 = CARTESIAN_POINT ( 'NONE',  ( -2.927979189508790103, -49.19984425798019601, -5.740620115512199639 ) ) ;
#38995 = CARTESIAN_POINT ( 'NONE',  ( 20.21022320103229930, -9.860630481422070659, -62.54333226898589260 ) ) ;
#38996 = CARTESIAN_POINT ( 'NONE',  ( 9.514507235804281038, -64.16384161684520393, -46.74925938990359953 ) ) ;
#38997 = ORIENTED_EDGE ( 'NONE', *, *, #51250, .T. ) ;
#38998 = ORIENTED_EDGE ( 'NONE', *, *, #5097, .F. ) ;
#38999 = ADVANCED_FACE ( 'NONE', ( #22709 ), #7265, .T. ) ;
#39000 = CARTESIAN_POINT ( 'NONE',  ( 23.79191500766741996, -17.66738227821284113, -55.59098426646090729 ) ) ;
#39001 = AXIS2_PLACEMENT_3D ( 'NONE', #22049, #22825, #33847 ) ;
#39002 = CARTESIAN_POINT ( 'NONE',  ( 66.70013194292150160, -1.463538230407920082, -17.02746303015019791 ) ) ;
#39003 = DIRECTION ( 'NONE',  ( -0.8660254037844384856, 0.5000000000000003331, 0.000000000000000000 ) ) ;
#39004 = DIRECTION ( 'NONE',  ( 0.3619651935900872752, 0.9321916104692696825, -3.469446951953614978E-15 ) ) ;
#39005 = CARTESIAN_POINT ( 'NONE',  ( 58.93930182096060122, -2.761714617466529909, -15.64944026956619894 ) ) ;
#39006 = CARTESIAN_POINT ( 'NONE',  ( 52.13018415749819923, -49.87691714427380418, -76.92945436144250948 ) ) ;
#39007 = CARTESIAN_POINT ( 'NONE',  ( 9.124981245646200279, 17.63186422973200251, -35.14566343974350104 ) ) ;
#39008 = ORIENTED_EDGE ( 'NONE', *, *, #15915, .F. ) ;
#39009 = CARTESIAN_POINT ( 'NONE',  ( 14.13393739769599833, 14.38381105532070059, -49.33749999999999858 ) ) ;
#39010 = CARTESIAN_POINT ( 'NONE',  ( 20.11812491441067152, -22.52867852696467210, -48.12566617391976109 ) ) ;
#39011 = LINE ( 'NONE', #38755, #30189 ) ;
#39012 = CARTESIAN_POINT ( 'NONE',  ( 52.65940447374160271, -45.11618894467940066, -12.18415347180710029 ) ) ;
#39013 = CIRCLE ( 'NONE', #39855, 3.076499999999999346 ) ;
#39014 = CARTESIAN_POINT ( 'NONE',  ( 8.779189791706480506, -18.35378556284099716, -40.89907019807789368 ) ) ;
#39015 = CARTESIAN_POINT ( 'NONE',  ( 13.57020051470579958, -51.02066577404819725, -21.88590882852059849 ) ) ;
#39016 = EDGE_CURVE ( 'NONE', #29117, #3105, #756, .T. ) ;
#39017 = CARTESIAN_POINT ( 'NONE',  ( -3.366062602303800055, -15.61618894467929763, -15.18999999999999950 ) ) ;
#39018 = CARTESIAN_POINT ( 'NONE',  ( 55.48947357315069695, 13.88381105532070059, -14.40594736128640108 ) ) ;
#39019 = CARTESIAN_POINT ( 'NONE',  ( 61.16413136812519724, -45.33305036688479817, -47.10581894728210273 ) ) ;
#39020 = CARTESIAN_POINT ( 'NONE',  ( 56.52536539877740296, -50.75180572374080157, -53.84278118897309895 ) ) ;
#39021 = CARTESIAN_POINT ( 'NONE',  ( 14.29653415316120046, -8.806893203457351049, -42.26328591669919632 ) ) ;
#39022 = CARTESIAN_POINT ( 'NONE',  ( 46.63300573313630082, -39.92275617562160051, -54.59612248810249469 ) ) ;
#39023 = ORIENTED_EDGE ( 'NONE', *, *, #41450, .T. ) ;
#39024 = DIRECTION ( 'NONE',  ( -1.000000000000000000, 0.000000000000000000, 0.000000000000000000 ) ) ;
#39025 = AXIS2_PLACEMENT_3D ( 'NONE', #23198, #15627, #51272 ) ;
#39026 = CARTESIAN_POINT ( 'NONE',  ( 64.94442696602180831, 1.326324093417220240, -60.85906821647699871 ) ) ;
#39027 = CARTESIAN_POINT ( 'NONE',  ( 23.62342291817629913, 17.52530927293010166, -35.10565360069929852 ) ) ;
#39028 = CARTESIAN_POINT ( 'NONE',  ( 64.93393739769599904, 1.396834109478129804, -61.06337307536569625 ) ) ;
#39029 = CARTESIAN_POINT ( 'NONE',  ( 18.20467892795669229, -7.911106368036362468, -47.09100263401473541 ) ) ;
#39030 = EDGE_CURVE ( 'NONE', #2811, #19647, #46611, .T. ) ;
#39031 = CARTESIAN_POINT ( 'NONE',  ( 13.64499661450167878, -17.42451027335708602, -22.14999999999999858 ) ) ;
#39032 = VECTOR ( 'NONE', #19113, 1000.000000000000000 ) ;
#39034 = EDGE_CURVE ( 'NONE', #34773, #14662, #419, .T. ) ;
#39033 = CARTESIAN_POINT ( 'NONE',  ( 82.71799697060619394, 14.26033053130370121, -47.55443180484209620 ) ) ;
#39035 = CARTESIAN_POINT ( 'NONE',  ( 14.38779660597143462, -7.866279551837843442, -64.93722419047314531 ) ) ;
#39036 = DIRECTION ( 'NONE',  ( 0.8204012560548797905, 0.5717882292104092823, 0.000000000000000000 ) ) ;
#39037 = CARTESIAN_POINT ( 'NONE',  ( 11.82116268612174359, -8.893085577089458127, -70.82645228965780859 ) ) ;
#39038 = CARTESIAN_POINT ( 'NONE',  ( 49.54883067255690321, 22.47422963147529984, -54.90668699459310176 ) ) ;
#39039 = EDGE_CURVE ( 'NONE', #39828, #13190, #10667, .T. ) ;
#39040 = ORIENTED_EDGE ( 'NONE', *, *, #51530, .T. ) ;
#39041 = CARTESIAN_POINT ( 'NONE',  ( 52.87494885159379976, -49.64620920156320238, -48.84793719265900336 ) ) ;
#39042 = ORIENTED_EDGE ( 'NONE', *, *, #19728, .F. ) ;
#39043 = CARTESIAN_POINT ( 'NONE',  ( 47.12471753871997748, 6.751739564498508095, -54.63036517340856335 ) ) ;
#39044 = VECTOR ( 'NONE', #38656, 1000.000000000000000 ) ;
#39045 = CARTESIAN_POINT ( 'NONE',  ( 22.22400857603370028, -12.05900013647219993, -40.67890729542689598 ) ) ;
#39046 = CARTESIAN_POINT ( 'NONE',  ( 13.90167036883489970, 19.71647169284459977, -21.77341558205650074 ) ) ;
#39047 = CARTESIAN_POINT ( 'NONE',  ( 51.88872915794820528, -49.34590157055340143, -77.07840658455160110 ) ) ;
#39048 = CARTESIAN_POINT ( 'NONE',  ( 9.809908155058138846, -12.49381599532109988, -55.59880359483129553 ) ) ;
#39049 = CARTESIAN_POINT ( 'NONE',  ( 52.91162664118279935, 18.41734443179310077, -48.98817407849419681 ) ) ;
#39050 = CARTESIAN_POINT ( 'NONE',  ( 55.90886914330630475, -45.57186394744790192, -16.63621152108130019 ) ) ;
#39051 = CARTESIAN_POINT ( 'NONE',  ( 54.39509416807689490, 16.57266139559970242, -25.91861715551300094 ) ) ;
#39052 = CIRCLE ( 'NONE', #2200, 15.11955878774480233 ) ;
#39053 = ORIENTED_EDGE ( 'NONE', *, *, #47117, .T. ) ;
#39054 = CARTESIAN_POINT ( 'NONE',  ( 9.773944590104200358, -20.21402263050010006, -32.08827495947629416 ) ) ;
#39055 = B_SPLINE_CURVE_WITH_KNOTS ( 'NONE', 3,
 ( #41335, #29272, #33458, #5448, #8859, #41083, #36356, #17239, #16454, #28496, #48962, #21405, #4400, #5195, #20369, #13314 ),
 .UNSPECIFIED., .F., .F.,
 ( 4, 2, 2, 2, 2, 2, 2, 4 ),
 ( 0.000000000000000000, 0.1775017698726158166, 0.3375008917962792343, 0.4375003429985697689, 0.4999999999999995559, 0.6249993140028615723, 0.8249982164074401991, 1.000000000000000000 ),
 .UNSPECIFIED. ) ;
#39056 = ORIENTED_EDGE ( 'NONE', *, *, #38832, .T. ) ;
#39057 = CARTESIAN_POINT ( 'NONE',  ( 58.58074692517319448, 15.55817703255979900, -48.00570932831679727 ) ) ;
#39058 = CARTESIAN_POINT ( 'NONE',  ( 11.33121657942630023, 33.96965385299019857, -47.25760506163170049 ) ) ;
#39059 = CARTESIAN_POINT ( 'NONE',  ( 72.86479754607628934, 1.326666718054990035, -62.33513496753349870 ) ) ;
#39060 = CARTESIAN_POINT ( 'NONE',  ( 9.807676903462912321, -20.47774473141403817, -40.58400665967682386 ) ) ;
#39061 = CARTESIAN_POINT ( 'NONE',  ( 52.95065152567730138, -49.64318942350852382, -49.05053742289103980 ) ) ;
#39062 = DIRECTION ( 'NONE',  ( 1.000000000000000000, 0.000000000000000000, 0.000000000000000000 ) ) ;
#39063 = CARTESIAN_POINT ( 'NONE',  ( 52.85072064880949938, -52.31592968273889710, -54.40017261481339972 ) ) ;
#39064 = EDGE_LOOP ( 'NONE', ( #14644, #10997, #21015, #40598 ) ) ;
#39065 = EDGE_CURVE ( 'NONE', #51621, #18232, #31141, .T. ) ;
#39066 = FACE_OUTER_BOUND ( 'NONE', #2193, .T. ) ;
#39067 = ORIENTED_EDGE ( 'NONE', *, *, #26887, .T. ) ;
#39068 = CARTESIAN_POINT ( 'NONE',  ( 10.77331230356430147, -63.33365191942790062, -45.20581385033180055 ) ) ;
#39069 = CARTESIAN_POINT ( 'NONE',  ( 16.13393739769620083, -15.61618894467929941, -28.45282021618999835 ) ) ;
#39070 = VERTEX_POINT ( 'NONE', #942 ) ;
#39071 = CARTESIAN_POINT ( 'NONE',  ( 17.48820068928834459, -23.48304697401851016, -44.23826555476666300 ) ) ;
#39072 = CARTESIAN_POINT ( 'NONE',  ( 56.96373068998019562, 19.10405578956169848, -52.80952918204310720 ) ) ;
#39073 = CARTESIAN_POINT ( 'NONE',  ( 53.48387700974569725, 19.28793721532720085, -77.13966347312370431 ) ) ;
#39074 = ORIENTED_EDGE ( 'NONE', *, *, #13162, .T. ) ;
#39075 = CARTESIAN_POINT ( 'NONE',  ( 16.13393739769620083, -15.61618894467919816, -82.14319696191608955 ) ) ;
#39076 = CARTESIAN_POINT ( 'NONE',  ( 50.95182575631829991, 19.71852405838109945, -76.14999999999999147 ) ) ;
#39078 = DIRECTION ( 'NONE',  ( 0.000000000000000000, -1.000000000000000000, 0.000000000000000000 ) ) ;
#39077 = CIRCLE ( 'NONE', #2251, 2.000000000000001776 ) ;
#39079 = CARTESIAN_POINT ( 'NONE',  ( 41.13393739769610136, -15.61618894467929586, 7.920000000000036344 ) ) ;
#39080 = CARTESIAN_POINT ( 'NONE',  ( 22.55256813713110020, -20.79150531053719675, -60.00832647494999605 ) ) ;
#39081 = CARTESIAN_POINT ( 'NONE',  ( 61.51122975691189509, 13.91278366405479616, -28.15000000000000213 ) ) ;
#39082 = ORIENTED_EDGE ( 'NONE', *, *, #45689, .T. ) ;
#39083 = ORIENTED_EDGE ( 'NONE', *, *, #42745, .F. ) ;
#39084 = B_SPLINE_CURVE_WITH_KNOTS ( 'NONE', 3,
 ( #8705, #16555, #4001, #20473, #12641, #48536, #16048, #43832, #829, #44600, #24395, #19962, #35957, #24914, #24657, #5038 ),
 .UNSPECIFIED., .F., .F.,
 ( 4, 2, 2, 2, 2, 2, 2, 4 ),
 ( 0.07080984669201570436, 0.1402455969909039979, 0.3005262792662219962, 0.4007017056882959949, 0.4507894188993329943, 0.5309297600369918824, 0.6591543058572471026, 0.8014033947008442071 ),
 .UNSPECIFIED. ) ;
#39085 = CARTESIAN_POINT ( 'NONE',  ( 13.13393739769619906, -49.61618894467939356, -35.14999999999999858 ) ) ;
#39086 = CARTESIAN_POINT ( 'NONE',  ( 18.90477078506000197, -8.700324852274359699, -55.85395427856209949 ) ) ;
#39087 = CARTESIAN_POINT ( 'NONE',  ( 52.62788022554430256, -49.80985595739589655, -48.67187667633960046 ) ) ;
#39088 = CIRCLE ( 'NONE', #2261, 3.000000000000005773 ) ;
#39089 = CARTESIAN_POINT ( 'NONE',  ( 47.13393657218789912, 8.048130458325550407, -53.76789950451890121 ) ) ;
#39090 = CARTESIAN_POINT ( 'NONE',  ( 8.222937397696199469, -15.61618894467929941, -32.14999999999999858 ) ) ;
#39091 = CYLINDRICAL_SURFACE ( 'NONE', #21718, 9.999999999999998224 ) ;
#39092 = CARTESIAN_POINT ( 'NONE',  ( 11.68991505668609854, 33.67328296886339700, -16.36861125145140150 ) ) ;
#39093 = CARTESIAN_POINT ( 'NONE',  ( 11.58913342612299857, -22.49568584263250415, -60.19350159652129406 ) ) ;
#39094 = CARTESIAN_POINT ( 'NONE',  ( 21.52056153400079808, -21.16699044271719998, -32.14999999999999858 ) ) ;
#39095 = ADVANCED_FACE ( 'NONE', ( #24762, #25018 ), #8810, .T. ) ;
#39096 = VECTOR ( 'NONE', #21902, 1000.000000000000000 ) ;
#39097 = CARTESIAN_POINT ( 'NONE',  ( 53.68378902630690419, -51.14674281437299896, -75.73832380907369100 ) ) ;
#39099 = DIRECTION ( 'NONE',  ( -0.05023550054955997629, 0.000000000000000000, 0.9987374001630935361 ) ) ;
#39098 = CARTESIAN_POINT ( 'NONE',  ( -3.157173927189479645, 18.96160609307260003, -7.169295440220589732 ) ) ;
#39100 = CARTESIAN_POINT ( 'NONE',  ( 14.14886614762350092, -32.59522544870679894, -35.02873218748179340 ) ) ;
#39101 = DIRECTION ( 'NONE',  ( 1.000000000000000000, 0.000000000000000000, 0.000000000000000000 ) ) ;
#39102 = EDGE_CURVE ( 'NONE', #7036, #24695, #38837, .T. ) ;
#39103 = ORIENTED_EDGE ( 'NONE', *, *, #11943, .T. ) ;
#39104 = CARTESIAN_POINT ( 'NONE',  ( -10.43833443274229822, -42.78838519611409907, -5.987488507031909712 ) ) ;
#39105 = CARTESIAN_POINT ( 'NONE',  ( 47.62304984032139998, 23.30770537504639961, -55.01447731861150459 ) ) ;
#39106 = CARTESIAN_POINT ( 'NONE',  ( 20.69249140832376810, -9.085681294808187758, -65.48617898402430626 ) ) ;
#39107 = CARTESIAN_POINT ( 'NONE',  ( 63.53329261246669546, 1.393731187554809958, -62.48946499964799983 ) ) ;
#39108 = CARTESIAN_POINT ( 'NONE',  ( 61.18512861914399537, 14.25518643980569955, -47.51727820143830172 ) ) ;
#39109 = CARTESIAN_POINT ( 'NONE',  ( 23.52846977382590055, -14.70647209751679974, -78.19369283850278407 ) ) ;
#39110 = CARTESIAN_POINT ( 'NONE',  ( 51.86152320295530416, 18.16617469022599707, -77.00280388411249533 ) ) ;
#39111 = CARTESIAN_POINT ( 'NONE',  ( 52.85276752197869854, 18.41685827962099609, -48.69281274069099652 ) ) ;
#39112 = CARTESIAN_POINT ( 'NONE',  ( 16.13393739769620083, -15.61618894467929941, 6.789625226207629538 ) ) ;
#39113 = DIRECTION ( 'NONE',  ( 0.000000000000000000, 1.000000000000000000, 0.000000000000000000 ) ) ;
#39114 = CARTESIAN_POINT ( 'NONE',  ( 52.86922557812509638, 18.38647850950570017, -27.84988300371350078 ) ) ;
#39115 = DIRECTION ( 'NONE',  ( 0.7071067811865510144, 0.000000000000000000, 0.7071067811865441310 ) ) ;
#39116 = CARTESIAN_POINT ( 'NONE',  ( 10.77457706359389888, -63.40313208684650448, -45.20848294960729419 ) ) ;
#39117 = CARTESIAN_POINT ( 'NONE',  ( 52.59025554715780260, 18.60560742025969816, -48.57067451951849790 ) ) ;
#39118 = CARTESIAN_POINT ( 'NONE',  ( 65.19670345645570819, -31.70240288822050090, -17.22254538528369849 ) ) ;
#39119 = CARTESIAN_POINT ( 'NONE',  ( 71.21626143364200345, 1.196343736543249880, -60.62426770491639871 ) ) ;
#39120 = CARTESIAN_POINT ( 'NONE',  ( 39.04269904001555602, 1.028000652403628701, 6.072546842075589701 ) ) ;
#39121 = CARTESIAN_POINT ( 'NONE',  ( 72.31745269033768864, 1.031856533264720266, -61.34884692546020091 ) ) ;
#39122 =( GEOMETRIC_REPRESENTATION_CONTEXT ( 3 ) GLOBAL_UNCERTAINTY_ASSIGNED_CONTEXT ( ( #8531 ) ) GLOBAL_UNIT_ASSIGNED_CONTEXT ( ( #23837, #1053, #47986 ) ) REPRESENTATION_CONTEXT ( 'NONE', 'WORKASPACE' ) );
#39123 = LINE ( 'NONE', #19187, #28460 ) ;
#39124 = EDGE_CURVE ( 'NONE', #10051, #13019, #25163, .T. ) ;
#39125 = CARTESIAN_POINT ( 'NONE',  ( 17.65201533994627070, -8.962439695671685413, -66.02401901343213808 ) ) ;
#39126 = VERTEX_POINT ( 'NONE', #21102 ) ;
#39127 = ORIENTED_EDGE ( 'NONE', *, *, #9563, .T. ) ;
#39128 = CARTESIAN_POINT ( 'NONE',  ( 42.11778985390380114, 12.11280974652049913, -3.278435070539889917 ) ) ;
#39129 = EDGE_CURVE ( 'NONE', #7977, #15209, #28876, .T. ) ;
#39130 = FACE_BOUND ( 'NONE', #19409, .T. ) ;
#39131 = EDGE_LOOP ( 'NONE', ( #32945, #5123, #5188, #49424 ) ) ;
#39132 = CARTESIAN_POINT ( 'NONE',  ( 56.26582864981669729, -45.64151070618309802, -25.71051917747889703 ) ) ;
#39133 = LINE ( 'NONE', #28076, #1048 ) ;
#39134 = ORIENTED_EDGE ( 'NONE', *, *, #27044, .T. ) ;
#39135 = CARTESIAN_POINT ( 'NONE',  ( 22.91193804342860574, -14.92565144664893850, -80.42032930067895791 ) ) ;
#39136 = CARTESIAN_POINT ( 'NONE',  ( 44.85897114471773506, 6.793334218869983232, -66.02479074488660160 ) ) ;
#39137 = DIRECTION ( 'NONE',  ( 1.000000000000000000, 0.000000000000000000, -0.000000000000000000 ) ) ;
#39138 = ORIENTED_EDGE ( 'NONE', *, *, #48371, .F. ) ;
#39139 = CARTESIAN_POINT ( 'NONE',  ( 48.77938445352399555, -45.11618894467940066, -9.436603585181519094 ) ) ;
#39140 = CARTESIAN_POINT ( 'NONE',  ( 51.17461318815491467, 0.4193470954621815738, -17.11446460828111427 ) ) ;
#39141 = CARTESIAN_POINT ( 'NONE',  ( 16.65784958574153407, -23.52864899547403610, -50.27127475680247670 ) ) ;
#39142 = CARTESIAN_POINT ( 'NONE',  ( 59.89126922325319669, -28.73587617226999669, -15.75816652841679755 ) ) ;
#39143 =( BOUNDED_CURVE ( )  B_SPLINE_CURVE ( 3, ( #37166, #37418, #5970, #36901 ),
 .UNSPECIFIED., .F., .T. ) 
 B_SPLINE_CURVE_WITH_KNOTS ( ( 4, 4 ),
 ( 0.7853981633974950194, 0.8959462480754279978 ),
 .UNSPECIFIED. ) 
 CURVE ( )  GEOMETRIC_REPRESENTATION_ITEM ( )  RATIONAL_B_SPLINE_CURVE ( ( 1.000000000000000000, 0.9989818526760920747, 0.9989818526760920747, 1.000000000000000000 ) ) 
 REPRESENTATION_ITEM ( '' )  );
#39144 = DIRECTION ( 'NONE',  ( -1.000000000000000000, 0.000000000000000000, 0.000000000000000000 ) ) ;
#39145 = CARTESIAN_POINT ( 'NONE',  ( 47.24351674907580190, -54.76020115456520188, -74.19815949659729881 ) ) ;
#39146 = CARTESIAN_POINT ( 'NONE',  ( 9.367501421782780113, -15.61622054991689978, -37.45282021618999835 ) ) ;
#39147 = CARTESIAN_POINT ( 'NONE',  ( 14.93164752284620178, 21.74151571116259873, -76.14999999999999147 ) ) ;
#39148 = CARTESIAN_POINT ( 'NONE',  ( 83.56294434887010425, -44.67980675742190044, -46.81484486652620092 ) ) ;
#39149 = CIRCLE ( 'NONE', #11551, 2.500000000000000444 ) ;
#39150 = CARTESIAN_POINT ( 'NONE',  ( 65.05986636033101433, -32.17013944165564965, -17.72012440155577195 ) ) ;
#39151 = CARTESIAN_POINT ( 'NONE',  ( 24.05051738721850185, -13.31173972757300028, -33.41750289701789711 ) ) ;
#39152 = VERTEX_POINT ( 'NONE', #25544 ) ;
#39153 = DIRECTION ( 'NONE',  ( 1.000000000000000000, 0.000000000000000000, 0.000000000000000000 ) ) ;
#39154 = EDGE_CURVE ( 'NONE', #21117, #8299, #43242, .T. ) ;
#39155 = CARTESIAN_POINT ( 'NONE',  ( 3.311002740984799964, -55.48809801447850276, -8.795318458723610178 ) ) ;
#39156 = CARTESIAN_POINT ( 'NONE',  ( 76.45066347563938791, -5.998607385428130101, -13.01482868083799893 ) ) ;
#39157 = AXIS2_PLACEMENT_3D ( 'NONE', #3534, #51233, #19505 ) ;
#39158 = CARTESIAN_POINT ( 'NONE',  ( 75.12321108456825414, 13.75868864148215209, -14.64191154256811522 ) ) ;
#39159 = CARTESIAN_POINT ( 'NONE',  ( 16.13393739769620083, -15.61618894467929941, -28.02168704970069868 ) ) ;
#39160 = CARTESIAN_POINT ( 'NONE',  ( 45.14919548887390022, -33.29386571476810275, -35.12503119152809461 ) ) ;
#39161 = CARTESIAN_POINT ( 'NONE',  ( 47.18324198357279897, 23.57489020266570279, -54.61058319554400242 ) ) ;
#39162 = CARTESIAN_POINT ( 'NONE',  ( 82.74206167245459653, -45.55975176208480093, -47.63388670989679952 ) ) ;
#39163 = CARTESIAN_POINT ( 'NONE',  ( 13.13413232964760091, 19.09465183653970044, -21.17378716131170080 ) ) ;
#39164 = CARTESIAN_POINT ( 'NONE',  ( 57.42034897354250234, -50.39122232172000082, -52.99919040445719531 ) ) ;
#39165 = CARTESIAN_POINT ( 'NONE',  ( 41.98583911138710079, 12.34957473716399967, -3.946145644750030268 ) ) ;
#39166 = CYLINDRICAL_SURFACE ( 'NONE', #20008, 0.5000000000000154321 ) ;
#39167 = CARTESIAN_POINT ( 'NONE',  ( 63.75818144730860126, 1.026088617261689873, -61.54425306709249810 ) ) ;
#39168 = FACE_OUTER_BOUND ( 'NONE', #43928, .T. ) ;
#39169 = CARTESIAN_POINT ( 'NONE',  ( 16.13393739769620083, -1.759782484128330049, -47.64999999999999858 ) ) ;
#39170 = CARTESIAN_POINT ( 'NONE',  ( 67.36987268233460213, -1.219418600938930064, -17.47395685963029877 ) ) ;
#39171 = CARTESIAN_POINT ( 'NONE',  ( 18.27764122236090216, -52.20804236601910020, -75.66803551354809088 ) ) ;
#39172 = DIRECTION ( 'NONE',  ( 1.000000000000000000, 0.000000000000000000, 0.000000000000000000 ) ) ;
#39173 = CARTESIAN_POINT ( 'NONE',  ( 20.68452214731360428, -21.51524588413079897, -67.35819317332679645 ) ) ;
#39174 = CARTESIAN_POINT ( 'NONE',  ( 63.38185292195529286, 1.308647200627810259, -62.31695083504749988 ) ) ;
#39175 = ORIENTED_EDGE ( 'NONE', *, *, #230, .F. ) ;
#39176 = CARTESIAN_POINT ( 'NONE',  ( 8.801404170410069838, 31.97031994814190270, -46.67014817202279886 ) ) ;
#39177 = CARTESIAN_POINT ( 'NONE',  ( 85.26960572018150231, 18.79802461769378397, -53.60827425107920874 ) ) ;
#39178 = CARTESIAN_POINT ( 'NONE',  ( 73.20393974370449541, 0.8850831926798630178, -68.85873448833339694 ) ) ;
#39179 = CARTESIAN_POINT ( 'NONE',  ( 45.75084721212736838, 8.846752882301483822, -58.16900694336454336 ) ) ;
#39180 = CARTESIAN_POINT ( 'NONE',  ( 9.077368987888030816, -13.86164298377170034, -81.23899999999999011 ) ) ;
#39181 = CARTESIAN_POINT ( 'NONE',  ( 42.10988702888519697, -45.61410618971950726, -6.748864943960410478 ) ) ;
#39182 = VERTEX_POINT ( 'NONE', #1721 ) ;
#39183 = CARTESIAN_POINT ( 'NONE',  ( 17.65712708557559907, 21.25914908875220277, -76.03975947796440948 ) ) ;
#39184 = ORIENTED_EDGE ( 'NONE', *, *, #3375, .T. ) ;
#39185 = EDGE_CURVE ( 'NONE', #42670, #6855, #1404, .T. ) ;
#39186 = ORIENTED_EDGE ( 'NONE', *, *, #43095, .T. ) ;
#39187 = DIRECTION ( 'NONE',  ( 0.000000000000000000, 0.000000000000000000, -1.000000000000000000 ) ) ;
#39188 = CARTESIAN_POINT ( 'NONE',  ( 21.96651055732200319, -10.35688966336140027, -81.23899999999999011 ) ) ;
#39189 = FACE_OUTER_BOUND ( 'NONE', #18630, .T. ) ;
#39190 = STYLED_ITEM ( 'NONE', ( #35896 ), #44821 ) ;
#39191 = ORIENTED_EDGE ( 'NONE', *, *, #16786, .F. ) ;
#39192 = CARTESIAN_POINT ( 'NONE',  ( 21.86911740259973413, -11.93844100352546000, -80.27148098536147813 ) ) ;
#39193 = ORIENTED_EDGE ( 'NONE', *, *, #30644, .F. ) ;
#39194 = FACE_BOUND ( 'NONE', #44587, .T. ) ;
#39195 = DIRECTION ( 'NONE',  ( -0.8660254037844472563, -0.4999999999999851785, 0.000000000000000000 ) ) ;
#39196 = VERTEX_POINT ( 'NONE', #33151 ) ;
#39197 = CARTESIAN_POINT ( 'NONE',  ( 68.13393739769620083, -42.11618894467930119, -59.64999999999999858 ) ) ;
#39198 = CARTESIAN_POINT ( 'NONE',  ( 51.19516171219699885, -51.09621740586149485, -76.13919816896859061 ) ) ;
#39199 = CARTESIAN_POINT ( 'NONE',  ( 60.34509757308260447, 14.55242050680869959, -47.56040643802499801 ) ) ;
#39200 = DIRECTION ( 'NONE',  ( 1.000000000000000000, 0.000000000000000000, 0.000000000000000000 ) ) ;
#39201 = CARTESIAN_POINT ( 'NONE',  ( 41.52331217152200082, -43.88959755902970272, -3.580227202335870551 ) ) ;
#39202 = CARTESIAN_POINT ( 'NONE',  ( -2.760456474399689775, 17.67254785648750115, -5.324092234737729967 ) ) ;
#39203 = CARTESIAN_POINT ( 'NONE',  ( 46.97440434159817357, 23.10210195763378138, -75.47461153636835718 ) ) ;
#39204 = LINE ( 'NONE', #2790, #34772 ) ;
#39205 = CARTESIAN_POINT ( 'NONE',  ( 9.741898527687681053, -20.16905477484420217, -48.09049903432729423 ) ) ;
#39206 = EDGE_LOOP ( 'NONE', ( #14248, #9795, #46654, #19051, #34985, #22217 ) ) ;
#39207 = CYLINDRICAL_SURFACE ( 'NONE', #49793, 1.000000000000001110 ) ;
#39208 = EDGE_CURVE ( 'NONE', #6375, #12691, #11440, .T. ) ;
#39209 = CARTESIAN_POINT ( 'NONE',  ( 57.49142314647060203, 19.07070453755489936, -52.84932360955439634 ) ) ;
#39210 = CARTESIAN_POINT ( 'NONE',  ( 71.51343005691549592, 1.309114013480880079, -70.37891650423269141 ) ) ;
#39211 = CARTESIAN_POINT ( 'NONE',  ( 45.06511394444972041, -40.03503324105221850, -61.49686747805221643 ) ) ;
#39212 = EDGE_CURVE ( 'NONE', #37478, #17894, #37105, .T. ) ;
#39213 = CARTESIAN_POINT ( 'NONE',  ( 14.09495638489210201, 19.44551819299880080, -21.23638623580700013 ) ) ;
#39214 = EDGE_CURVE ( 'NONE', #43185, #28919, #20606, .T. ) ;
#39215 = AXIS2_PLACEMENT_3D ( 'NONE', #45771, #14569, #45514 ) ;
#39216 = DIRECTION ( 'NONE',  ( 1.000000000000000000, 2.460964292799963328E-14, 0.000000000000000000 ) ) ;
#39217 = DIRECTION ( 'NONE',  ( 0.000000000000000000, 0.000000000000000000, -1.000000000000000000 ) ) ;
#39218 = EDGE_CURVE ( 'NONE', #38090, #13535, #11456, .T. ) ;
#39219 = AXIS2_PLACEMENT_3D ( 'NONE', #48197, #12562, #16479 ) ;
#39220 = CARTESIAN_POINT ( 'NONE',  ( 63.25409997666370288, 1.100585178972010025, -69.07860007646949896 ) ) ;
#39221 = CARTESIAN_POINT ( 'NONE',  ( 48.50283979947599988, -54.16647448328220094, -55.22557313126660006 ) ) ;
#39222 = CARTESIAN_POINT ( 'NONE',  ( -33.86606260230286125, -15.61618894467806484, -57.75434458024869855 ) ) ;
#39223 = AXIS2_PLACEMENT_3D ( 'NONE', #40703, #32291, #8482 ) ;
#39224 = CARTESIAN_POINT ( 'NONE',  ( 63.41196002899329898, 0.9486721756287899154, -69.35284629089680664 ) ) ;
#39225 = CARTESIAN_POINT ( 'NONE',  ( 8.222339619445261150, -15.61627490117209938, -70.79233150823699816 ) ) ;
#39226 = ORIENTED_EDGE ( 'NONE', *, *, #4646, .F. ) ;
#39227 = CARTESIAN_POINT ( 'NONE',  ( 9.388128293077700803, -18.77858577391589989, -33.92780426447939846 ) ) ;
#39228 = VERTEX_POINT ( 'NONE', #45492 ) ;
#39229 = CARTESIAN_POINT ( 'NONE',  ( 71.58293006479010501, 1.102139304147779830, -70.51608385812031088 ) ) ;
#39230 = DIRECTION ( 'NONE',  ( 0.000000000000000000, 0.000000000000000000, 1.000000000000000000 ) ) ;
#39231 = CARTESIAN_POINT ( 'NONE',  ( 59.82327988359549664, -45.99681751185720202, -47.29966340866579344 ) ) ;
#39232 = CARTESIAN_POINT ( 'NONE',  ( 52.13393739769618662, -29.66618894467940137, -65.65000000000000568 ) ) ;
#39234 = CARTESIAN_POINT ( 'NONE',  ( 16.13393739769620083, -15.61618894467929941, -28.45282021618999835 ) ) ;
#39233 = CARTESIAN_POINT ( 'NONE',  ( 83.91175033285890095, 13.57253447764839827, -47.46627397093730139 ) ) ;
#39235 = CARTESIAN_POINT ( 'NONE',  ( 24.04508668034977248, -15.61618904219531778, -35.79233368253564862 ) ) ;
#39236 = CARTESIAN_POINT ( 'NONE',  ( 23.83903754356633797, -17.68686498457494238, -41.59100066116396732 ) ) ;
#39237 = CARTESIAN_POINT ( 'NONE',  ( 68.13393739769620083, 17.38381105532069881, -65.65000000000000568 ) ) ;
#39238 = ORIENTED_EDGE ( 'NONE', *, *, #3918, .T. ) ;
#39239 = CARTESIAN_POINT ( 'NONE',  ( 18.13393739769620439, -34.76920587681881614, -43.67210485825550847 ) ) ;
#39240 = ORIENTED_EDGE ( 'NONE', *, *, #50000, .F. ) ;
#39241 = ADVANCED_FACE ( 'NONE', ( #1202 ), #41574, .T. ) ;
#39242 = ORIENTED_EDGE ( 'NONE', *, *, #30931, .F. ) ;
#39243 = DIRECTION ( 'NONE',  ( 0.000000000000000000, 1.000000000000000000, 0.000000000000000000 ) ) ;
#39244 = DIRECTION ( 'NONE',  ( 0.000000000000000000, 0.000000000000000000, -1.000000000000000000 ) ) ;
#39245 = DIRECTION ( 'NONE',  ( 0.000000000000000000, 0.000000000000000000, 1.000000000000000000 ) ) ;
#39246 = CARTESIAN_POINT ( 'NONE',  ( 11.53802652246220006, -65.15112864915029434, -46.97774799415349634 ) ) ;
#39247 = VERTEX_POINT ( 'NONE', #13270 ) ;
#39248 = ORIENTED_EDGE ( 'NONE', *, *, #33265, .F. ) ;
#39249 = CARTESIAN_POINT ( 'NONE',  ( 71.62484648860579739, 0.9098571636355720083, -60.77008670988870165 ) ) ;
#39250 = CARTESIAN_POINT ( 'NONE',  ( 21.14288210468432183, -10.65101126812107957, -32.59857632693771734 ) ) ;
#39251 = CARTESIAN_POINT ( 'NONE',  ( 56.52536539877759481, -50.75180572374069499, -53.84278118897309895 ) ) ;
#39252 = DIRECTION ( 'NONE',  ( -1.000000000000000000, 0.000000000000000000, 0.000000000000000000 ) ) ;
#39253 = CARTESIAN_POINT ( 'NONE',  ( 60.83673909420080150, -0.6553940542465449548, -16.28925331010010069 ) ) ;
#39254 = CARTESIAN_POINT ( 'NONE',  ( 51.75737835881179905, -49.21100704886299582, -76.97426712213069777 ) ) ;
#39255 = CARTESIAN_POINT ( 'NONE',  ( 19.13393739769600188, 18.38381105532069881, -83.01107220193038927 ) ) ;
#39256 = VERTEX_POINT ( 'NONE', #9590 ) ;
#39257 = CARTESIAN_POINT ( 'NONE',  ( 63.93393739769591377, 11.38381105532030801, -61.44999999999966178 ) ) ;
#39258 = CARTESIAN_POINT ( 'NONE',  ( 76.79908580335488466, 11.93597894565887430, -14.51620736842078863 ) ) ;
#39259 = CARTESIAN_POINT ( 'NONE',  ( 29.12893361417140525, -26.73813571787616539, -35.06842082984513098 ) ) ;
#39260 = DIRECTION ( 'NONE',  ( -1.000000000000000000, 0.000000000000000000, 0.000000000000000000 ) ) ;
#39261 = EDGE_CURVE ( 'NONE', #50083, #36534, #4722, .T. ) ;
#39262 = AXIS2_PLACEMENT_3D ( 'NONE', #37772, #42220, #26469 ) ;
#39263 = CARTESIAN_POINT ( 'NONE',  ( 8.328589087560620996, -16.43061226767880001, -48.97940116656710074 ) ) ;
#39264 = CARTESIAN_POINT ( 'NONE',  ( 13.29196628380899980, -50.07647854234220119, -21.00283603054380066 ) ) ;
#39265 = DIRECTION ( 'NONE',  ( -1.000000000000000000, 0.000000000000000000, 0.000000000000000000 ) ) ;
#39266 = CARTESIAN_POINT ( 'NONE',  ( 56.33352089224590031, 13.89801324381519976, -15.47337191694060010 ) ) ;
#39267 = CARTESIAN_POINT ( 'NONE',  ( 61.19909444736899928, -45.31215391586800223, -47.06069671806489652 ) ) ;
#39268 = CARTESIAN_POINT ( 'NONE',  ( 45.63393739769620083, 19.38381105532069881, 16.85000000000000142 ) ) ;
#39269 = CARTESIAN_POINT ( 'NONE',  ( 12.69742525569020053, -9.457216345917659694, -50.18517902306119538 ) ) ;
#39270 = DIRECTION ( 'NONE',  ( 0.000000000000000000, 0.000000000000000000, 1.000000000000000000 ) ) ;
#39271 = ORIENTED_EDGE ( 'NONE', *, *, #23754, .T. ) ;
#39272 = CARTESIAN_POINT ( 'NONE',  ( 13.42257398911860022, -51.72201830638929465, -74.14993436883828792 ) ) ;
#39273 = CARTESIAN_POINT ( 'NONE',  ( 64.89987712417480736, 0.8859637708054489691, -60.59611492242089525 ) ) ;
#39274 = CARTESIAN_POINT ( 'NONE',  ( 43.44329010622809761, -46.02041590603030130, -7.898785361262961047 ) ) ;
#39275 = ADVANCED_FACE ( 'NONE', ( #1460 ), #45752, .T. ) ;
#39276 = CARTESIAN_POINT ( 'NONE',  ( 55.53661300022847769, -47.20923717753896653, -26.46481881287708759 ) ) ;
#39277 = EDGE_CURVE ( 'NONE', #38344, #4837, #45137, .T. ) ;
#39278 = CARTESIAN_POINT ( 'NONE',  ( 8.223454620794861114, -15.61605491354059971, -46.50766849176290663 ) ) ;
#39279 = FACE_OUTER_BOUND ( 'NONE', #8178, .T. ) ;
#39280 = EDGE_CURVE ( 'NONE', #10844, #32800, #30679, .T. ) ;
#39281 = CARTESIAN_POINT ( 'NONE',  ( 82.34888464648300044, 14.41279304669810024, -47.72707126332089445 ) ) ;
#39282 = CYLINDRICAL_SURFACE ( 'NONE', #24246, 2.999999999999999556 ) ;
#39284 = CARTESIAN_POINT ( 'NONE',  ( 47.67266003423409870, -38.15547488882079818, -51.93650398367349652 ) ) ;
#39283 = CARTESIAN_POINT ( 'NONE',  ( 27.13393739769620083, -15.61618894467929941, -19.83999999999999986 ) ) ;
#39285 = CARTESIAN_POINT ( 'NONE',  ( 17.01354725415873759, -23.50622319154220818, -32.25706115642341842 ) ) ;
#39286 = CARTESIAN_POINT ( 'NONE',  ( 49.20613926322570109, 22.63364074929049607, -55.12403394422909741 ) ) ;
#39287 = ORIENTED_EDGE ( 'NONE', *, *, #23115, .T. ) ;
#39288 = AXIS2_PLACEMENT_3D ( 'NONE', #3685, #12067, #19902 ) ;
#39289 = CARTESIAN_POINT ( 'NONE',  ( 53.14599526630189530, -49.52280220221379636, -49.02433929921330247 ) ) ;
#39290 = ORIENTED_EDGE ( 'NONE', *, *, #25931, .F. ) ;
#39291 = VECTOR ( 'NONE', #45459, 1000.000000000000000 ) ;
#39292 = B_SPLINE_CURVE_WITH_KNOTS ( 'NONE', 3,
 ( #20514, #610, #49627, #32549, #49112, #41227, #25222, #29422, #5341, #12685, #28638, #32817, #37037, #1135, #37549, #37298, #33613, #9531 ),
 .UNSPECIFIED., .F., .F.,
 ( 4, 2, 2, 2, 2, 2, 2, 2, 4 ),
 ( 0.000000000000000000, 0.06250012490808277976, 0.1250002498161655595, 0.1875003747242483532, 0.2500004996323311190, 0.3125006245404138849, 0.3750007494484967063, 0.4375008743565794722, 0.5000009992646622381 ),
 .UNSPECIFIED. ) ;
#39293 = CARTESIAN_POINT ( 'NONE',  ( 44.59253762482858718, 6.549697931826371722, -67.31859651280061030 ) ) ;
#39294 = CARTESIAN_POINT ( 'NONE',  ( 13.67284627086910120, 19.93818776675360027, -22.23398155374439966 ) ) ;
#39295 = CARTESIAN_POINT ( 'NONE',  ( 46.99731062513887281, -39.23427468941395801, -34.80647497723114725 ) ) ;
#39296 = AXIS2_PLACEMENT_3D ( 'NONE', #3015, #46278, #37884 ) ;
#39297 = CARTESIAN_POINT ( 'NONE',  ( 21.56449732505549832, -11.11601366231700005, -56.23255504334029098 ) ) ;
#39298 = AXIS2_PLACEMENT_3D ( 'NONE', #31404, #43489, #43743 ) ;
#39299 = CARTESIAN_POINT ( 'NONE',  ( 52.60258329861409976, 18.59156606793389699, -48.51134384244380016 ) ) ;
#39300 = CARTESIAN_POINT ( 'NONE',  ( 55.66436213888189855, -45.60096027170479971, -16.29539555431340148 ) ) ;
#39301 = CARTESIAN_POINT ( 'NONE',  ( 54.18967173931659431, 16.81490735217030164, -26.03594187494229928 ) ) ;
#39302 = ORIENTED_EDGE ( 'NONE', *, *, #16144, .T. ) ;
#39303 = CIRCLE ( 'NONE', #38476, 15.11955878774480233 ) ;
#39304 = CARTESIAN_POINT ( 'NONE',  ( 23.80184081761380099, -17.28652279287269877, -33.35577785649419980 ) ) ;
#39305 = EDGE_CURVE ( 'NONE', #8243, #29849, #12139, .T. ) ;
#39306 = ORIENTED_EDGE ( 'NONE', *, *, #14140, .T. ) ;
#39307 = CARTESIAN_POINT ( 'NONE',  ( 10.87995450790350205, -64.97548900853969656, -17.51161086048150040 ) ) ;
#39308 = CARTESIAN_POINT ( 'NONE',  ( 9.188454688195358600, 32.78433166906430074, -46.76666145987389456 ) ) ;
#39309 = CARTESIAN_POINT ( 'NONE',  ( 72.75396425272869294, 1.390208944942419755, -62.54542373973200142 ) ) ;
#39310 = CARTESIAN_POINT ( 'NONE',  ( 8.223148984577919762, -15.61599292915740023, -40.79233150823699816 ) ) ;
#39311 = CARTESIAN_POINT ( 'NONE',  ( 68.13393739769618662, -28.66618894467939782, -65.65000000000000568 ) ) ;
#39312 = FACE_OUTER_BOUND ( 'NONE', #18706, .T. ) ;
#39313 = ORIENTED_EDGE ( 'NONE', *, *, #21227, .F. ) ;
#39314 = DIRECTION ( 'NONE',  ( 0.9990957361526741076, 0.000000000000000000, -0.04251717301921900671 ) ) ;
#39315 = CARTESIAN_POINT ( 'NONE',  ( 10.77136036876739844, -63.23172379110331320, -45.20469033881160215 ) ) ;
#39316 = CYLINDRICAL_SURFACE ( 'NONE', #22694, 6.766999999999998572 ) ;
#39317 = ORIENTED_EDGE ( 'NONE', *, *, #6440, .T. ) ;
#39318 = CARTESIAN_POINT ( 'NONE',  ( 68.36163517248512278, -30.78936114711470751, -18.19591817807315692 ) ) ;
#39319 = CARTESIAN_POINT ( 'NONE',  ( 56.70659705232079517, 19.32440130277539936, -53.10139024778879957 ) ) ;
#39320 = CARTESIAN_POINT ( 'NONE',  ( 47.26610112325450075, 22.82567072896360116, -75.56421356201970241 ) ) ;
#39321 = EDGE_LOOP ( 'NONE', ( #27892, #7929 ) ) ;
#39322 = DIRECTION ( 'NONE',  ( 0.000000000000000000, 0.000000000000000000, -1.000000000000000000 ) ) ;
#39323 = DIRECTION ( 'NONE',  ( 1.000000000000000000, 2.460964292799963328E-14, 0.000000000000000000 ) ) ;
#39324 = CARTESIAN_POINT ( 'NONE',  ( 83.09574697842404589, -44.89486775114661299, -46.39646040884239397 ) ) ;
#39325 = CARTESIAN_POINT ( 'NONE',  ( 18.20459673516950261, -7.911083136343404654, -69.37566667060073655 ) ) ;
#39326 = EDGE_CURVE ( 'NONE', #24020, #29481, #27031, .T. ) ;
#39327 = CARTESIAN_POINT ( 'NONE',  ( 8.790427394441779896, -19.36526628291030150, -60.64207792345899151 ) ) ;
#39328 = ADVANCED_FACE ( 'NONE', ( #44878 ), #15621, .F. ) ;
#39329 = DIRECTION ( 'NONE',  ( 0.000000000000000000, 0.000000000000000000, -1.000000000000000000 ) ) ;
#39330 = CARTESIAN_POINT ( 'NONE',  ( 61.20224358684065891, -45.27433979179907197, -46.71246603851685819 ) ) ;
#39332 = ORIENTED_EDGE ( 'NONE', *, *, #51515, .T. ) ;
#39331 = B_SPLINE_CURVE_WITH_KNOTS ( 'NONE', 3,
 ( #17713, #33680, #49695, #13788, #29746, #17967, #37894, #9851, #25807, #41814, #6184, #22141, #38151, #18224, #26334, #30268, #46286 ),
 .UNSPECIFIED., .F., .F.,
 ( 4, 2, 2, 2, 2, 1, 2, 2, 4 ),
 ( 0.4766446636200218356, 0.5420640806675175449, 0.6074834977150133097, 0.7383223318100058385, 0.7546771860718798353, 0.7710320403337540540, 0.8037417488575033797, 0.8691611659050022531, 1.000000000000000000 ),
 .UNSPECIFIED. ) ;
#39333 = ORIENTED_EDGE ( 'NONE', *, *, #33201, .F. ) ;
#39334 = AXIS2_PLACEMENT_3D ( 'NONE', #30470, #18941, #12062 ) ;
#39335 = VECTOR ( 'NONE', #51575, 1000.000000000000000 ) ;
#39336 = CARTESIAN_POINT ( 'NONE',  ( 12.06284766121009966, -63.44323389162830296, -46.39999999999999858 ) ) ;
#39337 = CARTESIAN_POINT ( 'NONE',  ( 19.73032284921290369, -9.091412665812349303, -51.89300772538119588 ) ) ;
#39338 = AXIS2_PLACEMENT_3D ( 'NONE', #46768, #27077, #6923 ) ;
#39339 = CARTESIAN_POINT ( 'NONE',  ( 52.45428892279399946, 13.97507276140040133, -12.94524249092279966 ) ) ;
#39340 = VECTOR ( 'NONE', #51556, 1000.000000000000000 ) ;
#39341 = CARTESIAN_POINT ( 'NONE',  ( 9.539384564179858472, -19.34381366239919942, -32.14999999999999858 ) ) ;
#39342 = CARTESIAN_POINT ( 'NONE',  ( 47.30600330445400203, 23.48391298978570063, -74.19742682671839873 ) ) ;
#39343 = CONICAL_SURFACE ( 'NONE', #16736, 12.92820323027549989, 0.7481802937784480800 ) ;
#39344 = CARTESIAN_POINT ( 'NONE',  ( 49.75282653525520260, -57.95720799465139805, -54.55458065461419892 ) ) ;
#39345 = CARTESIAN_POINT ( 'NONE',  ( 68.13393739769620083, 11.88381105532070059, -71.50000000000000000 ) ) ;
#39346 = EDGE_CURVE ( 'NONE', #1287, #1526, #20804, .T. ) ;
#39347 = CARTESIAN_POINT ( 'NONE',  ( 12.19720189296489998, 33.46095046226900394, -15.92873818749999870 ) ) ;
#39348 = CARTESIAN_POINT ( 'NONE',  ( 7.967372319093019684, -14.48043565900760044, -72.55165484244589891 ) ) ;
#39349 = EDGE_CURVE ( 'NONE', #10310, #1136, #36394, .T. ) ;
#39350 = CARTESIAN_POINT ( 'NONE',  ( 20.82227175848069933, -21.85412434938530168, -32.14999999999999858 ) ) ;
#39351 = CARTESIAN_POINT ( 'NONE',  ( 54.46179591467679870, -50.62549687492020212, -76.64268959045750762 ) ) ;
#39353 = CARTESIAN_POINT ( 'NONE',  ( 30.95441726489424283, -35.72841810710970378, -84.62495954532434439 ) ) ;
#39352 = CARTESIAN_POINT ( 'NONE',  ( -9.343064548044289097, 12.51679987183899811, -5.546829476069820686 ) ) ;
#39354 = CARTESIAN_POINT ( 'NONE',  ( 63.45006824032990522, 1.383161449028130097, -68.67155289007729380 ) ) ;
#39355 = CYLINDRICAL_SURFACE ( 'NONE', #24735, 0.5000000000000049960 ) ;
#39356 = ORIENTED_EDGE ( 'NONE', *, *, #28990, .T. ) ;
#39357 = CARTESIAN_POINT ( 'NONE',  ( 14.27930865506306013, 21.26098553221025611, -75.92929758211228375 ) ) ;
#39358 = CARTESIAN_POINT ( 'NONE',  ( 47.54404738341980163, 23.34326443908900117, -54.90429578540580025 ) ) ;
#39359 = CARTESIAN_POINT ( 'NONE',  ( 61.12509698999170382, -45.25425853416980004, -27.63408038702889868 ) ) ;
#39360 = DIRECTION ( 'NONE',  ( 0.000000000000000000, 0.000000000000000000, -1.000000000000000000 ) ) ;
#39361 = DIRECTION ( 'NONE',  ( 1.000000000000000000, 0.000000000000000000, 0.000000000000000000 ) ) ;
#39362 = CARTESIAN_POINT ( 'NONE',  ( 23.22922891231669951, -13.34384827310289978, -76.13400063084860392 ) ) ;
#39363 = CARTESIAN_POINT ( 'NONE',  ( 51.43588672793779892, 18.51358431124270254, -76.47300566802010735 ) ) ;
#39364 = CARTESIAN_POINT ( 'NONE',  ( 52.82975622904280755, 18.42854261028849905, -48.47378032971769812 ) ) ;
#39365 = DIRECTION ( 'NONE',  ( 0.2260571801428149230, 0.000000000000000000, -0.9741140340359946137 ) ) ;
#39366 = CARTESIAN_POINT ( 'NONE',  ( 52.83236148840860125, -49.65955553127109567, -48.53481065559509489 ) ) ;
#39367 = CARTESIAN_POINT ( 'NONE',  ( 49.81362442766570098, 22.09256562639079746, -54.04987025831400160 ) ) ;
#39368 = CONICAL_SURFACE ( 'NONE', #19267, 1.942499999999999227, 0.8266833912447979493 ) ;
#39369 = CARTESIAN_POINT ( 'NONE',  ( 17.80236287562073016, -23.36212981481903483, -61.94013304973208278 ) ) ;
#39370 = CARTESIAN_POINT ( 'NONE',  ( 85.38000601716228743, -48.61618894467930119, -60.34000486924599471 ) ) ;
#39371 = CIRCLE ( 'NONE', #34333, 21.19999999999999929 ) ;
#39372 = CARTESIAN_POINT ( 'NONE',  ( 60.45235380029059513, -30.32562723922359993, -16.15944822728640062 ) ) ;
#39373 = CARTESIAN_POINT ( 'NONE',  ( 71.24781132387310834, 1.101170701158060039, -60.57405794295090118 ) ) ;
#39374 = CARTESIAN_POINT ( 'NONE',  ( 11.13393739769619906, 31.98148447116350113, -43.74438458204450342 ) ) ;
#39375 = CARTESIAN_POINT ( 'NONE',  ( 72.23215937178071044, 1.347758125946160179, -61.41854848478109830 ) ) ;
#39376 = CIRCLE ( 'NONE', #5886, 1.999999999999998224 ) ;
#39377 = LINE ( 'NONE', #51430, #49404 ) ;
#39378 = DIRECTION ( 'NONE',  ( 1.000000000000000000, 0.000000000000000000, 0.000000000000000000 ) ) ;
#39379 = VERTEX_POINT ( 'NONE', #25452 ) ;
#39380 = ORIENTED_EDGE ( 'NONE', *, *, #44946, .T. ) ;
#39381 = CARTESIAN_POINT ( 'NONE',  ( 12.67868222463649808, -21.76466606210399846, -37.51015005288219584 ) ) ;
#39382 = CARTESIAN_POINT ( 'NONE',  ( 14.36277553031169596, -22.20708433113889058, -59.03615343158287487 ) ) ;
#39383 = ORIENTED_EDGE ( 'NONE', *, *, #32241, .T. ) ;
#39384 = CARTESIAN_POINT ( 'NONE',  ( 57.14705973144530304, -45.14741832947689915, -25.37809429576289943 ) ) ;
#39385 = DIRECTION ( 'NONE',  ( 0.000000000000000000, 0.000000000000000000, -1.000000000000000000 ) ) ;
#39386 = VERTEX_POINT ( 'NONE', #9754 ) ;
#39387 = CARTESIAN_POINT ( 'NONE',  ( 10.99717798698634752, 33.61421173664781037, -23.19667442668940893 ) ) ;
#39388 = CARTESIAN_POINT ( 'NONE',  ( 45.06955000105763531, 6.818482170417528465, -64.97193686384484579 ) ) ;
#39389 = CARTESIAN_POINT ( 'NONE',  ( 11.01453361030839950, 32.67406340009490151, -23.98619660447929647 ) ) ;
#39390 = ADVANCED_FACE ( 'NONE', ( #29899 ), #1887, .T. ) ;
#39391 = ORIENTED_EDGE ( 'NONE', *, *, #408, .T. ) ;
#39392 = CARTESIAN_POINT ( 'NONE',  ( 24.15879671053109945, -17.50942769270979937, -33.86607922395569403 ) ) ;
#39393 = EDGE_CURVE ( 'NONE', #42024, #15377, #40721, .T. ) ;
#39394 = CARTESIAN_POINT ( 'NONE',  ( 50.62425669123998517, 19.01350634637644532, 11.97999999999999865 ) ) ;
#39395 = CARTESIAN_POINT ( 'NONE',  ( 24.03634747343981104, -15.99279584001448917, -49.80748426219081182 ) ) ;
#39396 = EDGE_CURVE ( 'NONE', #42606, #5918, #15162, .T. ) ;
#39397 = CIRCLE ( 'NONE', #26810, 16.60961179679778965 ) ;
#39398 = CARTESIAN_POINT ( 'NONE',  ( 62.97929662215530300, -29.57076698415579941, -16.19920473766450186 ) ) ;
#39399 = CARTESIAN_POINT ( 'NONE',  ( 17.90521437699635854, -9.025324052677705211, -64.03615484355167098 ) ) ;
#39400 = CARTESIAN_POINT ( 'NONE',  ( 46.97454301875460203, -53.98875319215230206, -75.73879140141839628 ) ) ;
#39401 = CARTESIAN_POINT ( 'NONE',  ( 23.03046715727910154, -11.87124236738749872, -73.85414552054359660 ) ) ;
#39402 = DIRECTION ( 'NONE',  ( 0.000000000000000000, 0.7371541402007423249, 0.6757246285173452716 ) ) ;
#39403 = CARTESIAN_POINT ( 'NONE',  ( 41.23776877753270753, 13.84931952467590044, -5.742138678026360132 ) ) ;
#39404 = FACE_OUTER_BOUND ( 'NONE', #38207, .T. ) ;
#39405 = CIRCLE ( 'NONE', #26818, 20.00000000000000355 ) ;
#39406 = CARTESIAN_POINT ( 'NONE',  ( 82.53147610877059037, -45.13461238702009837, -46.79182873648620244 ) ) ;
#39407 = CARTESIAN_POINT ( 'NONE',  ( 65.10753665118122058, -31.99864820310045133, -17.50331349256994073 ) ) ;
#39408 = AXIS2_PLACEMENT_3D ( 'NONE', #7854, #35632, #42992 ) ;
#39409 = B_SPLINE_CURVE_WITH_KNOTS ( 'NONE', 3,
 ( #27855, #19985, #16327, #15308, #7953, #28104, #36232, #24157, #31261, #40178, #47293, #4272, #47794, #3775, #19741, #28361 ),
 .UNSPECIFIED., .F., .F.,
 ( 4, 2, 2, 2, 2, 2, 2, 4 ),
 ( -1.047176999999999937E-15, 0.4421363464883489858, 0.9474350281893189063, 1.263246704252430019, 1.421152542283979914, 1.673801883134459878, 2.076007908835539872, 2.526493408504850269 ),
 .UNSPECIFIED. ) ;
#39410 = CARTESIAN_POINT ( 'NONE',  ( 15.48260933934249906, -23.83558627473800229, -44.03283965954289414 ) ) ;
#39411 = EDGE_CURVE ( 'NONE', #47621, #43823, #49602, .T. ) ;
#39412 = ORIENTED_EDGE ( 'NONE', *, *, #35368, .F. ) ;
#39413 = CARTESIAN_POINT ( 'NONE',  ( 55.53662353292170195, -47.20924349302610068, -26.46482561396789990 ) ) ;
#39414 = CARTESIAN_POINT ( 'NONE',  ( 16.05644225716720186, -51.03148892433259931, -20.34167354763580349 ) ) ;
#39415 = CARTESIAN_POINT ( 'NONE',  ( 76.37043116117959585, -8.469752128233089650, -12.66764180611509971 ) ) ;
#39416 = DIRECTION ( 'NONE',  ( -1.000000000000000000, 0.000000000000000000, 0.000000000000000000 ) ) ;
#39417 = CYLINDRICAL_SURFACE ( 'NONE', #34022, 0.9999999999999407141 ) ;
#39418 = CARTESIAN_POINT ( 'NONE',  ( 13.04629919360907309, 18.51631118994176362, -82.73668660645843431 ) ) ;
#39419 = CARTESIAN_POINT ( 'NONE',  ( 47.18324198357279897, 23.57489020266570279, -54.61058319554400242 ) ) ;
#39420 = CARTESIAN_POINT ( 'NONE',  ( 18.65820481519197926, 18.38381105532056736, -83.09320499157193751 ) ) ;
#39421 = CARTESIAN_POINT ( 'NONE',  ( 82.39374053741410364, -45.13655374397700371, -46.71923274431809858 ) ) ;
#39422 = CARTESIAN_POINT ( 'NONE',  ( 57.48533814307809564, -50.45530859044179550, -53.13639308838089903 ) ) ;
#39423 = CARTESIAN_POINT ( 'NONE',  ( 43.68128689219040695, 12.31476791676119831, -5.037759820107959641 ) ) ;
#39424 = CARTESIAN_POINT ( 'NONE',  ( 47.62441104666342540, -54.51319350588585877, -74.50474471046057090 ) ) ;
#39425 = CARTESIAN_POINT ( 'NONE',  ( 63.83278432315639606, 1.031856533264730258, -61.46648470735859604 ) ) ;
#39426 = CARTESIAN_POINT ( 'NONE',  ( 56.94228693352650339, -47.50625043831589522, -47.82842110489030318 ) ) ;
#39427 = CARTESIAN_POINT ( 'NONE',  ( 65.43042069957887463, -49.21324915460706961, -70.54648330188271643 ) ) ;
#39428 = CARTESIAN_POINT ( 'NONE',  ( 105.5832649133809156, -15.41618894467769962, -103.0993275156849762 ) ) ;
#39429 = CARTESIAN_POINT ( 'NONE',  ( 17.81969638158939873, -51.79813798162680172, -75.64877291256318870 ) ) ;
#39430 = B_SPLINE_CURVE_WITH_KNOTS ( 'NONE', 3,
 ( #49490, #12542, #13577, #4931, #28509, #41345, #20903, #41095, #1518, #1262, #17503, #44506, #5462, #8609, #4667, #20641 ),
 .UNSPECIFIED., .F., .F.,
 ( 4, 2, 2, 2, 2, 2, 2, 4 ),
 ( -4.528785000000000087E-15, 0.07216186899280399580, 0.1546325764131560032, 0.2061767685508759940, 0.2319488646197360171, 0.2731842183299119653, 0.3391607842661930050, 0.4123535371017559847 ),
 .UNSPECIFIED. ) ;
#39431 = CARTESIAN_POINT ( 'NONE',  ( 45.23836003753899604, -43.83063101194750288, -5.450403507060779695 ) ) ;
#39432 = B_SPLINE_CURVE_WITH_KNOTS ( 'NONE', 3,
 ( #13467, #8746, #25481, #24694, #40712, #28902, #12946, #44904, #41485, #9010 ),
 .UNSPECIFIED., .F., .F.,
 ( 4, 1, 1, 1, 1, 1, 1, 4 ),
 ( 0.5000038607551413605, 0.5558869319517651952, 0.6351058630153233464, 0.7143247940790398154, 0.7935437251426000760, 0.8727626562061583382, 0.9519815872698746961, 1.000000000000000000 ),
 .UNSPECIFIED. ) ;
#39433 = CARTESIAN_POINT ( 'NONE',  ( 8.703688250329728149, -15.07021097222849981, -66.09069027630890503 ) ) ;
#39434 = DIRECTION ( 'NONE',  ( 0.000000000000000000, 0.000000000000000000, 1.000000000000000000 ) ) ;
#39435 = CARTESIAN_POINT ( 'NONE',  ( 63.45871665573360332, 1.367045641526529964, -62.38166218803879559 ) ) ;
#39436 = ORIENTED_EDGE ( 'NONE', *, *, #1565, .T. ) ;
#39437 = CARTESIAN_POINT ( 'NONE',  ( 16.13393739769620083, -29.64169738395614218, -34.79644660940672907 ) ) ;
#39438 = CARTESIAN_POINT ( 'NONE',  ( 11.61470965350185125, -20.68213784063762972, -35.18459255138716912 ) ) ;
#39439 = CARTESIAN_POINT ( 'NONE',  ( 72.95172982307090592, 1.328073773609210084, -68.78070348185231353 ) ) ;
#39440 = CARTESIAN_POINT ( 'NONE',  ( 12.72603970786425975, -9.703224440543703366, -73.78615355345934290 ) ) ;
#39441 = CARTESIAN_POINT ( 'NONE',  ( 8.975894543716849583, -15.11915247762119918, -81.23899999999999011 ) ) ;
#39442 = ORIENTED_EDGE ( 'NONE', *, *, #9715, .T. ) ;
#39443 = CARTESIAN_POINT ( 'NONE',  ( 17.50704397559620062, 21.63336578114690312, -76.12563501418109979 ) ) ;
#39444 = EDGE_LOOP ( 'NONE', ( #14431, #23943, #24383, #38192 ) ) ;
#39445 = ORIENTED_EDGE ( 'NONE', *, *, #42677, .T. ) ;
#39446 = CARTESIAN_POINT ( 'NONE',  ( 23.32430482491560042, -49.33365190531349498, -34.64999999999999858 ) ) ;
#39447 = CARTESIAN_POINT ( 'NONE',  ( 22.58862951581259892, -11.28899428718860065, -81.23899999999999011 ) ) ;
#39448 = CIRCLE ( 'NONE', #18518, 1.000000000000000888 ) ;
#39449 =( BOUNDED_SURFACE ( )  B_SPLINE_SURFACE ( 2, 2, ( 
 ( #8440, #48524, #36713 ),
 ( #24122, #16292, #31995 ),
 ( #816, #28072, #44077 ) ),
 .UNSPECIFIED., .F., .F., .T. ) 
 B_SPLINE_SURFACE_WITH_KNOTS ( ( 3, 3 ),
 ( 3, 3 ),
 ( -1.570546326878010213, -1.285150385668689982E-13 ),
 ( 1.570796326791910058, 3.141592653593380025 ),
 .UNSPECIFIED. ) 
 GEOMETRIC_REPRESENTATION_ITEM ( )  RATIONAL_B_SPLINE_SURFACE ( (
 ( 1.000000000000000000, 0.7071067811842219886, 1.000000000000000000),
 ( 0.7071951639803649714, 0.5000624960712040101, 0.7071951639803649714),
 ( 1.000000000000000000, 0.7071067811842219886, 1.000000000000000000) ) ) 
 REPRESENTATION_ITEM ( '' )  SURFACE ( )  );
#39450 = CARTESIAN_POINT ( 'NONE',  ( 61.51131554793239786, 14.10369252969250020, -47.28580145422539971 ) ) ;
#39451 = AXIS2_PLACEMENT_3D ( 'NONE', #21891, #29750, #9857 ) ;
#39452 = ORIENTED_EDGE ( 'NONE', *, *, #1045, .T. ) ;
#39453 = AXIS2_PLACEMENT_3D ( 'NONE', #48463, #28265, #44267 ) ;
#39454 = CARTESIAN_POINT ( 'NONE',  ( 23.83903502047883194, -13.54550035082508508, -53.42433795965683885 ) ) ;
#39455 = ORIENTED_EDGE ( 'NONE', *, *, #36112, .T. ) ;
#39456 = CARTESIAN_POINT ( 'NONE',  ( 82.75389963950189554, 14.36256073625980001, -47.67227237920639737 ) ) ;
#39457 = EDGE_CURVE ( 'NONE', #36574, #12279, #28160, .T. ) ;
#39458 = FACE_OUTER_BOUND ( 'NONE', #49076, .T. ) ;
#39459 = ORIENTED_EDGE ( 'NONE', *, *, #2722, .T. ) ;
#39460 = CARTESIAN_POINT ( 'NONE',  ( 59.34499803081116198, -28.79149204250002825, -15.68015151901640181 ) ) ;
#39461 = CARTESIAN_POINT ( 'NONE',  ( 51.62415613633279321, -50.67669871992969632, -76.24933076846630797 ) ) ;
#39462 = CARTESIAN_POINT ( 'NONE',  ( 60.27360767123079910, 14.56433066022209921, -47.49318409392830631 ) ) ;
#39463 = DIRECTION ( 'NONE',  ( -0.7782863420137342558, -0.3536342755907660451, 0.5188575613424891708 ) ) ;
#39464 = CARTESIAN_POINT ( 'NONE',  ( 16.13393739769620083, -15.61618894467929941, -32.14999999999999858 ) ) ;
#39465 = CARTESIAN_POINT ( 'NONE',  ( -2.700142691300089659, 17.56628513837100058, -5.083883929925409717 ) ) ;
#39466 = EDGE_CURVE ( 'NONE', #33614, #49749, #18123, .T. ) ;
#39467 = DIRECTION ( 'NONE',  ( 0.9441882088883092328, -0.3294064756441295039, 0.000000000000000000 ) ) ;
#39468 = DIRECTION ( 'NONE',  ( 1.000000000000000000, 0.000000000000000000, 0.000000000000000000 ) ) ;
#39469 = CARTESIAN_POINT ( 'NONE',  ( 23.78998258546389977, -17.34005676619050007, -49.35800193134529934 ) ) ;
#39470 = ADVANCED_FACE ( 'NONE', ( #13440 ), #33585, .T. ) ;
#39471 = VERTEX_POINT ( 'NONE', #46184 ) ;
#39472 = CARTESIAN_POINT ( 'NONE',  ( 56.72051766773449799, -50.68676931991499401, -53.84018978630579966 ) ) ;
#39473 = CARTESIAN_POINT ( 'NONE',  ( 57.49678186962110260, 18.90849154042449953, -52.63232334799329237 ) ) ;
#39474 = EDGE_CURVE ( 'NONE', #28709, #34084, #18976, .T. ) ;
#39475 = CARTESIAN_POINT ( 'NONE',  ( 71.90718900442469419, 0.9644290104345999426, -70.31590730770628284 ) ) ;
#39476 = CARTESIAN_POINT ( 'NONE',  ( 45.77061686725269141, -40.08029671403183158, -58.07308786245754106 ) ) ;
#39477 = CARTESIAN_POINT ( 'NONE',  ( 15.78591284857189869, 19.69271321420649912, -20.28298178678300090 ) ) ;
#39478 = VECTOR ( 'NONE', #17046, 1000.000000000000000 ) ;
#39479 = CIRCLE ( 'NONE', #24359, 3.000000000000003997 ) ;
#39480 = AXIS2_PLACEMENT_3D ( 'NONE', #50792, #30845, #19066 ) ;
#39481 = CARTESIAN_POINT ( 'NONE',  ( 12.04533177224588236, -22.42911352436259875, -32.17980570764689929 ) ) ;
#39482 = CARTESIAN_POINT ( 'NONE',  ( 53.63393739769619373, 21.88381105532059934, 11.84999999999999964 ) ) ;
#39483 = CARTESIAN_POINT ( 'NONE',  ( 48.50426931947900044, -54.16735222170059671, -55.28601062726929882 ) ) ;
#39484 = FACE_OUTER_BOUND ( 'NONE', #18590, .T. ) ;
#39485 = FACE_OUTER_BOUND ( 'NONE', #8643, .T. ) ;
#39486 = CARTESIAN_POINT ( 'NONE',  ( 47.69758263342730942, 23.27859210216669794, -55.15459985148470423 ) ) ;
#39487 = VERTEX_POINT ( 'NONE', #29648 ) ;
#39488 = CARTESIAN_POINT ( 'NONE',  ( 15.11696271606249908, -22.99673460733349728, -33.61092854022489718 ) ) ;
#39489 = DIRECTION ( 'NONE',  ( 1.000000000000000000, 0.000000000000000000, 0.000000000000000000 ) ) ;
#39490 = ORIENTED_EDGE ( 'NONE', *, *, #6376, .F. ) ;
#39491 = CARTESIAN_POINT ( 'NONE',  ( 62.63393739769619373, 21.88381105532059934, 17.35000000000000142 ) ) ;
#39492 = CARTESIAN_POINT ( 'NONE',  ( 60.61713456004790146, -45.58380821826049356, -47.21957072048249415 ) ) ;
#39493 = CARTESIAN_POINT ( 'NONE',  ( 0.3198662801700680181, -20.69846475549559983, -34.64999999999999858 ) ) ;
#39494 = CARTESIAN_POINT ( 'NONE',  ( 83.63329895952738013, 13.29802447021414658, -46.55718444776781695 ) ) ;
#39496 = CARTESIAN_POINT ( 'NONE',  ( 8.133937397696209715, 23.57564693985150228, -21.14999999999999858 ) ) ;
#39495 = CARTESIAN_POINT ( 'NONE',  ( 84.02703262422839714, 13.40384015226580061, -47.45290575524859378 ) ) ;
#39497 = CARTESIAN_POINT ( 'NONE',  ( 29.92510725984174158, 4.389127169904199377, -84.60896002036976427 ) ) ;
#39498 = CARTESIAN_POINT ( 'NONE',  ( 56.84932596551129791, 19.42421318737730118, -53.85230338955989993 ) ) ;
#39499 = ORIENTED_EDGE ( 'NONE', *, *, #17749, .F. ) ;
#39500 = DIRECTION ( 'NONE',  ( -0.8660254037844387076, -0.4999999999999998890, 0.000000000000000000 ) ) ;
#39501 = ORIENTED_EDGE ( 'NONE', *, *, #30555, .F. ) ;
#39502 = ORIENTED_EDGE ( 'NONE', *, *, #29257, .F. ) ;
#39503 = LINE ( 'NONE', #3602, #1880 ) ;
#39504 = DIRECTION ( 'NONE',  ( 0.000000000000000000, 0.000000000000000000, -1.000000000000000000 ) ) ;
#39505 = DIRECTION ( 'NONE',  ( 1.000000000000000000, 0.000000000000000000, 0.000000000000000000 ) ) ;
#39506 = CARTESIAN_POINT ( 'NONE',  ( 9.182372922795538628, -63.76165471016090436, -46.66759804741280249 ) ) ;
#39507 = ORIENTED_EDGE ( 'NONE', *, *, #40577, .T. ) ;
#39508 = VERTEX_POINT ( 'NONE', #34089 ) ;
#39509 = CARTESIAN_POINT ( 'NONE',  ( 55.73977427078670388, 19.85292510813409805, -53.93776639284670438 ) ) ;
#39510 = CARTESIAN_POINT ( 'NONE',  ( 57.34990408955430041, -45.12238703601330059, -25.32055789762510045 ) ) ;
#39511 = DIRECTION ( 'NONE',  ( 1.000000000000000000, 0.000000000000000000, 0.000000000000000000 ) ) ;
#39512 = ADVANCED_FACE ( 'NONE', ( #37792 ), #10532, .F. ) ;
#39513 = CARTESIAN_POINT ( 'NONE',  ( 15.64891603104893392, -8.847981134172776763, -45.93003584796989003 ) ) ;
#39514 = CARTESIAN_POINT ( 'NONE',  ( 59.04235309263319920, -3.122828794254560059, -15.65226437496019685 ) ) ;
#39515 = CARTESIAN_POINT ( 'NONE',  ( 58.41900308037850209, -49.15319073655110316, -51.55400195476909886 ) ) ;
#39516 = CIRCLE ( 'NONE', #18587, 5.499999999999998224 ) ;
#39517 = ORIENTED_EDGE ( 'NONE', *, *, #5945, .F. ) ;
#39518 = DIRECTION ( 'NONE',  ( -2.066387465239710029E-12, 1.205421602240320019E-11, 1.000000000000000000 ) ) ;
#39520 = DIRECTION ( 'NONE',  ( 0.000000000000000000, 0.000000000000000000, -1.000000000000000000 ) ) ;
#39519 = CIRCLE ( 'NONE', #16919, 3.500000000000003109 ) ;
#39521 = CARTESIAN_POINT ( 'NONE',  ( 64.92520290936280958, 0.8850831926798620186, -70.72000234600830026 ) ) ;
#39522 = CARTESIAN_POINT ( 'NONE',  ( 16.13393739769620083, -15.61618894467929941, -34.64999999999999858 ) ) ;
#39523 = CARTESIAN_POINT ( 'NONE',  ( 12.98069885294330028, -22.80255341299470118, -58.64411075632859394 ) ) ;
#39524 = CARTESIAN_POINT ( 'NONE',  ( 17.63393739769620083, -42.11618894467939356, -34.64999999999999858 ) ) ;
#39525 = CARTESIAN_POINT ( 'NONE',  ( 56.88828947208789799, 19.38381105532069881, -75.24793329859650726 ) ) ;
#39526 = CARTESIAN_POINT ( 'NONE',  ( -21.36606260230379917, -62.11618894467930119, 11.84999999999999964 ) ) ;
#39527 = CARTESIAN_POINT ( 'NONE',  ( 70.83745409581578656, -49.21324915460098026, -73.25000000000119371 ) ) ;
#39528 = CARTESIAN_POINT ( 'NONE',  ( 61.14309852062039852, -45.32067553311819808, -46.99564627970399755 ) ) ;
#39529 = CARTESIAN_POINT ( 'NONE',  ( 10.22106801927327346, -19.02425228399541979, -39.28615407111802682 ) ) ;
#39530 = CARTESIAN_POINT ( 'NONE',  ( 22.63286885114739988, -12.87639896407969964, -52.72018481709699955 ) ) ;
#39531 = CARTESIAN_POINT ( 'NONE',  ( 71.71126032029680175, 14.01986140997038888, -47.09707863094710945 ) ) ;
#39532 = EDGE_LOOP ( 'NONE', ( #39946, #28697, #21561, #25557 ) ) ;
#39533 = CARTESIAN_POINT ( 'NONE',  ( 11.19961949155312908, -65.24734059375452944, -18.17421237899869979 ) ) ;
#39534 = CARTESIAN_POINT ( 'NONE',  ( 65.07343865691001383, 1.370118064600909902, -60.90754237392700077 ) ) ;
#39535 = EDGE_CURVE ( 'NONE', #19506, #19682, #48282, .T. ) ;
#39536 = CARTESIAN_POINT ( 'NONE',  ( 44.22606915973489805, -46.08296596967250025, -8.447826951465771117 ) ) ;
#39537 = CARTESIAN_POINT ( 'NONE',  ( 8.223439258000311725, -15.61632852289070073, -42.50766849176289952 ) ) ;
#39538 = CARTESIAN_POINT ( 'NONE',  ( 11.63393739769619906, -41.61618894467930119, -35.14999999999999858 ) ) ;
#39539 = DIRECTION ( 'NONE',  ( -1.529205156547310004E-10, -1.048235172004079997E-08, -1.000000000000000000 ) ) ;
#39540 = CARTESIAN_POINT ( 'NONE',  ( 11.04564840988309982, 33.94644972953989992, -17.95839446270849749 ) ) ;
#39541 = DIRECTION ( 'NONE',  ( 1.687892000000000095E-11, 1.766113999999999920E-11, 1.000000000000000000 ) ) ;
#39543 = CARTESIAN_POINT ( 'NONE',  ( 44.14642363104649547, -37.85759600627010002, -69.58218121927448863 ) ) ;
#39542 = CARTESIAN_POINT ( 'NONE',  ( 63.63879714068243487, 0.6399062447643286689, -17.33502972194290237 ) ) ;
#39544 = CARTESIAN_POINT ( 'NONE',  ( 11.67619456822290047, 33.65927054772580362, -23.88710972541020183 ) ) ;
#39545 = CARTESIAN_POINT ( 'NONE',  ( 49.40539548389219959, 22.26547577746109852, -54.15746054660889541 ) ) ;
#39546 = ORIENTED_EDGE ( 'NONE', *, *, #22678, .F. ) ;
#39547 = CARTESIAN_POINT ( 'NONE',  ( 52.61723843343860096, -49.81156647556650086, -48.56633104006370161 ) ) ;
#39548 = CIRCLE ( 'NONE', #27830, 2.999999999999999112 ) ;
#39549 = EDGE_LOOP ( 'NONE', ( #6747, #49628, #42068 ) ) ;
#39550 = CARTESIAN_POINT ( 'NONE',  ( 40.77547000184679860, 7.884666264946645242, -85.73440608552456865 ) ) ;
#39551 = CARTESIAN_POINT ( 'NONE',  ( 66.72561048563109409, -33.11618894467930829, -20.64999999980150136 ) ) ;
#39552 = CARTESIAN_POINT ( 'NONE',  ( 57.77564497937559906, -3.116188944679349593, -20.65000000000000213 ) ) ;
#39553 = CARTESIAN_POINT ( 'NONE',  ( 47.13393739769619373, -39.28050807707779768, -35.14999999999999858 ) ) ;
#39554 = CARTESIAN_POINT ( 'NONE',  ( 10.07334972078679947, -19.22338116399880192, -55.28192787057680135 ) ) ;
#39555 = CARTESIAN_POINT ( 'NONE',  ( 16.13393739769620083, -15.61618894467929941, -14.65000000000000036 ) ) ;
#39556 = CARTESIAN_POINT ( 'NONE',  ( 55.17361021118440334, -45.21029328161770167, -14.82786001016749999 ) ) ;
#39557 = DIRECTION ( 'NONE',  ( 0.000000000000000000, 0.000000000000000000, 1.000000000000000000 ) ) ;
#39558 = VERTEX_POINT ( 'NONE', #31697 ) ;
#39559 = CARTESIAN_POINT ( 'NONE',  ( 17.93175953304550063, -23.25520614277689901, -45.71393110241879754 ) ) ;
#39560 = ORIENTED_EDGE ( 'NONE', *, *, #36725, .F. ) ;
#39561 = CARTESIAN_POINT ( 'NONE',  ( 11.28671405514150017, -65.00701117576899435, -16.86100849032779792 ) ) ;
#39562 = CARTESIAN_POINT ( 'NONE',  ( 11.68049157650639991, 33.98099422647310774, -47.05230233363739956 ) ) ;
#39563 = CARTESIAN_POINT ( 'NONE',  ( 73.08848314165430793, 0.9307121176571839793, -62.26576483763439995 ) ) ;
#39564 = CARTESIAN_POINT ( 'NONE',  ( 48.89387259858359869, -53.88404306600559579, -54.59098453863079925 ) ) ;
#39565 = CARTESIAN_POINT ( 'NONE',  ( 10.94680987515031489, -64.76538349226117930, -23.25394996400440917 ) ) ;
#39566 = CARTESIAN_POINT ( 'NONE',  ( 16.13393739769620083, -15.61618894467929941, -69.65000000000000568 ) ) ;
#39567 = ORIENTED_EDGE ( 'NONE', *, *, #39102, .T. ) ;
#39568 = CARTESIAN_POINT ( 'NONE',  ( 64.69948915615030671, 1.003508719579999875, -70.56164792957929421 ) ) ;
#39569 = CARTESIAN_POINT ( 'NONE',  ( 11.13393739769619906, -63.48571094816200855, -43.92550228023370096 ) ) ;
#39570 = ADVANCED_FACE ( 'NONE', ( #43282 ), #46506, .F. ) ;
#39571 = CARTESIAN_POINT ( 'NONE',  ( 16.13393739769620083, -15.61618894467929941, -28.45282021618999835 ) ) ;
#39572 = ORIENTED_EDGE ( 'NONE', *, *, #1106, .F. ) ;
#39573 = CARTESIAN_POINT ( 'NONE',  ( 24.03103897938508027, -16.12241053893984954, -43.81269848352728502 ) ) ;
#39574 = CARTESIAN_POINT ( 'NONE',  ( 17.61008469349813765, -7.820132634352628287, -77.06721755149550290 ) ) ;
#39575 = EDGE_CURVE ( 'NONE', #13982, #37163, #24087, .T. ) ;
#39576 = ORIENTED_EDGE ( 'NONE', *, *, #24172, .T. ) ;
#39577 = EDGE_CURVE ( 'NONE', #45957, #2565, #45793, .T. ) ;
#39578 = CARTESIAN_POINT ( 'NONE',  ( 9.221411231516558615, -19.60031519639062125, -36.34100132133150396 ) ) ;
#39579 = CARTESIAN_POINT ( 'NONE',  ( 52.57481508192923059, 20.19967092288929678, -75.83555757118507756 ) ) ;
#39580 = FACE_OUTER_BOUND ( 'NONE', #36562, .T. ) ;
#39581 = CARTESIAN_POINT ( 'NONE',  ( 50.00746865674540231, 21.72397341460670006, -53.49641930188690253 ) ) ;
#39582 = EDGE_CURVE ( 'NONE', #51003, #16762, #42412, .T. ) ;
#39583 = CARTESIAN_POINT ( 'NONE',  ( 15.23130163646179902, -7.420582271682119924, -71.25741468598400274 ) ) ;
#39584 = DIRECTION ( 'NONE',  ( 1.000000000000000000, 0.000000000000000000, 0.000000000000000000 ) ) ;
#39585 = FACE_BOUND ( 'NONE', #24474, .T. ) ;
#39586 = CONTEXT_DEPENDENT_SHAPE_REPRESENTATION ( #31772, #29883 ) ;
#39587 = ORIENTED_EDGE ( 'NONE', *, *, #44093, .F. ) ;
#39588 = ORIENTED_EDGE ( 'NONE', *, *, #39457, .T. ) ;
#39589 = AXIS2_PLACEMENT_3D ( 'NONE', #999, #21158, #5461 ) ;
#39590 = CARTESIAN_POINT ( 'NONE',  ( 17.56685828210809674, -8.305003572650919708, -53.79426207090799750 ) ) ;
#39591 = AXIS2_PLACEMENT_3D ( 'NONE', #1926, #17907, #13222 ) ;
#39592 = CARTESIAN_POINT ( 'NONE',  ( 53.63393739769619373, 21.88381105532059934, 16.35000000000000142 ) ) ;
#39593 = DIRECTION ( 'NONE',  ( 0.000000000000000000, 0.000000000000000000, -1.000000000000000000 ) ) ;
#39594 = CARTESIAN_POINT ( 'NONE',  ( 47.30620416954659646, 23.48429288067650234, -74.14999584438369595 ) ) ;
#39595 = CARTESIAN_POINT ( 'NONE',  ( -19.23636731124815924, 19.89349176177682210, 11.97999999999999865 ) ) ;
#39596 = ADVANCED_FACE ( 'NONE', ( #3186 ), #51395, .T. ) ;
#39597 = CARTESIAN_POINT ( 'NONE',  ( 10.06369629474122185, 22.76024865223496363, -34.79644414665609986 ) ) ;
#39598 = CARTESIAN_POINT ( 'NONE',  ( 12.10148745386679892, 33.86065729770509591, -16.50605066005979893 ) ) ;
#39599 = CARTESIAN_POINT ( 'NONE',  ( 22.76032741071229637, -10.70969568529780069, -77.30479070626310545 ) ) ;
#39600 = CARTESIAN_POINT ( 'NONE',  ( 52.82216258569669520, -49.58646061845040265, -27.28071896258420281 ) ) ;
#39601 = CIRCLE ( 'NONE', #245, 17.63819660112499932 ) ;
#39602 = CARTESIAN_POINT ( 'NONE',  ( 56.91185928905259317, -50.61618894550459657, -75.19908646239869654 ) ) ;
#39604 = CARTESIAN_POINT ( 'NONE',  ( 9.543027317544861887, -13.84507546134918243, -59.53614541435187846 ) ) ;
#39603 = CARTESIAN_POINT ( 'NONE',  ( -10.28442671929420094, 11.53361155615709954, -5.475821530260660097 ) ) ;
#39605 = CARTESIAN_POINT ( 'NONE',  ( 63.44018392888030178, 1.383811055320669947, -68.52712657046359368 ) ) ;
#39606 = CARTESIAN_POINT ( 'NONE',  ( 61.34198049900449945, 13.97791997643200190, -46.66621099661489325 ) ) ;
#39607 = DIRECTION ( 'NONE',  ( 0.000000000000000000, 0.000000000000000000, -1.000000000000000000 ) ) ;
#39608 = VERTEX_POINT ( 'NONE', #23319 ) ;
#39609 = CARTESIAN_POINT ( 'NONE',  ( 53.05372066228549954, -49.54357925801589602, -48.79446872794070345 ) ) ;
#39610 = CARTESIAN_POINT ( 'NONE',  ( 47.50357687577830035, 23.36731487144420072, -54.99836346755289895 ) ) ;
#39611 = ADVANCED_FACE ( 'NONE', ( #14970 ), #35136, .T. ) ;
#39612 = CARTESIAN_POINT ( 'NONE',  ( 60.26237441151779706, -45.38172583291230211, -27.01215158688860285 ) ) ;
#39613 = CARTESIAN_POINT ( 'NONE',  ( 16.13393739769620083, -15.61618894467929941, -8.655000000000001137 ) ) ;
#39614 = CARTESIAN_POINT ( 'NONE',  ( 61.62035637548115119, -45.25224449890009737, -47.09707516299204144 ) ) ;
#39615 = CARTESIAN_POINT ( 'NONE',  ( 13.94802033108170036, -22.73858042681539970, -78.82744428701170136 ) ) ;
#39616 = CARTESIAN_POINT ( 'NONE',  ( 51.09074887001380461, 17.58698902652399809, -76.44262319005990491 ) ) ;
#39617 = CARTESIAN_POINT ( 'NONE',  ( 53.19709010659749993, 18.24734634467580463, -48.94481910643570188 ) ) ;
#39618 = DIRECTION ( 'NONE',  ( -0.3502816565540492477, 0.000000000000000000, 0.9366444154970182678 ) ) ;
#39619 = CARTESIAN_POINT ( 'NONE',  ( 13.13393739769600010, 18.38381105532060289, -35.14999999999999858 ) ) ;
#39620 = B_SPLINE_CURVE_WITH_KNOTS ( 'NONE', 3,
 ( #17532, #48470, #45052, #36926, #24849, #25110, #41629, #16753, #12571, #5233, #5736, #28534, #33241, #45573, #21184, #1030, #37191, #25625 ),
 .UNSPECIFIED., .F., .F.,
 ( 4, 2, 2, 2, 2, 2, 2, 2, 4 ),
 ( 0.000000000000000000, 0.06249984979688257697, 0.1249996995937651539, 0.1874995493906477240, 0.2499993991875303079, 0.3124992489844128918, 0.3749990987812954479, 0.4374989485781780596, 0.4999987983750606158 ),
 .UNSPECIFIED. ) ;
#39621 = ORIENTED_EDGE ( 'NONE', *, *, #8384, .F. ) ;
#39622 = CARTESIAN_POINT ( 'NONE',  ( 22.90093739902486547, -15.61819515586083007, -40.45291899317828666 ) ) ;
#39623 = CONICAL_SURFACE ( 'NONE', #23694, 0.6299999999999998934, 0.7853981633974476129 ) ;
#39624 = CARTESIAN_POINT ( 'NONE',  ( 47.54281612864539852, -54.55267448867429891, -54.67232832126270381 ) ) ;
#39625 = CARTESIAN_POINT ( 'NONE',  ( 63.02122824129657630, -31.65172625870799195, -17.11446970408973201 ) ) ;
#39626 = CARTESIAN_POINT ( 'NONE',  ( 18.13393739769620083, -41.61618894467930119, -35.14999999999999858 ) ) ;
#39627 = CARTESIAN_POINT ( 'NONE',  ( 63.90257177041379322, -31.03871148548129710, -16.68334962132160015 ) ) ;
#39628 = CARTESIAN_POINT ( 'NONE',  ( 71.40029138921259744, 0.9945465939392541532, -60.62606712929739672 ) ) ;
#39629 = CARTESIAN_POINT ( 'NONE',  ( 16.13393739769620083, -15.61618894467929941, -28.45282021618999835 ) ) ;
#39630 = CIRCLE ( 'NONE', #24510, 14.49999999999999822 ) ;
#39631 = CARTESIAN_POINT ( 'NONE',  ( 72.30065220047070795, 1.277721627657099956, -61.41802414917730601 ) ) ;
#39632 = CARTESIAN_POINT ( 'NONE',  ( 16.13393739769620083, -15.61618894467929941, -643.2998782751060389 ) ) ;
#39633 = CARTESIAN_POINT ( 'NONE',  ( 21.20968439552399332, -11.07233059872317504, -66.22059550987238197 ) ) ;
#39634 = VERTEX_POINT ( 'NONE', #50618 ) ;
#39635 = ORIENTED_EDGE ( 'NONE', *, *, #34292, .T. ) ;
#39636 = CARTESIAN_POINT ( 'NONE',  ( 9.807722577752867821, -10.75457455335917345, -55.00065746664166255 ) ) ;
#39637 = DIRECTION ( 'NONE',  ( 1.000000000000000000, 0.000000000000000000, 0.000000000000000000 ) ) ;
#39638 = ORIENTED_EDGE ( 'NONE', *, *, #17095, .F. ) ;
#39639 = CARTESIAN_POINT ( 'NONE',  ( 16.65420337941059969, -51.11618894467930119, -15.67544740040250062 ) ) ;
#39640 = CARTESIAN_POINT ( 'NONE',  ( 9.807731428018854558, -20.47781564507460317, -78.29930256865087301 ) ) ;
#39641 = ORIENTED_EDGE ( 'NONE', *, *, #36893, .F. ) ;
#39642 = CARTESIAN_POINT ( 'NONE',  ( 51.13393739769659874, -50.61618894467899565, 11.34999999999999964 ) ) ;
#39643 = CARTESIAN_POINT ( 'NONE',  ( 44.28781032986178445, 6.722397411424160474, -68.88062643755992553 ) ) ;
#39644 = DIRECTION ( 'NONE',  ( 1.000000000000000000, 0.000000000000000000, 0.000000000000000000 ) ) ;
#39645 = EDGE_CURVE ( 'NONE', #5608, #40081, #7243, .T. ) ;
#39646 = CARTESIAN_POINT ( 'NONE',  ( 9.516401703503628795, -10.69776019232130082, -40.99578301968139726 ) ) ;
#39647 = VECTOR ( 'NONE', #36628, 1000.000000000000000 ) ;
#39648 = CARTESIAN_POINT ( 'NONE',  ( 15.09840566293024544, -23.52719084560120422, -68.04933387242864740 ) ) ;
#39649 = CARTESIAN_POINT ( 'NONE',  ( 11.57284508314511839, -22.11046742300001355, -50.48724504311571337 ) ) ;
#39650 = CARTESIAN_POINT ( 'NONE',  ( 60.19729760361229864, -28.87421560293969947, -15.80187452458650021 ) ) ;
#39651 = CARTESIAN_POINT ( 'NONE',  ( 19.54194781300750705, -9.703288880315998455, -64.11948836174622102 ) ) ;
#39652 = CARTESIAN_POINT ( 'NONE',  ( 46.77112351560430170, -53.52311952442669707, -76.01558715013979395 ) ) ;
#39653 = CARTESIAN_POINT ( 'NONE',  ( 23.84366418157409839, -17.08140582607870073, -76.07227559032499187 ) ) ;
#39654 = DIRECTION ( 'NONE',  ( 0.000000000000000000, 1.000000000000000000, 0.000000000000000000 ) ) ;
#39655 = CARTESIAN_POINT ( 'NONE',  ( 44.37484003570580171, 14.76830914866819988, -8.485749550088890203 ) ) ;
#39656 = CYLINDRICAL_SURFACE ( 'NONE', #36770, 1.999999999999999556 ) ;
#39657 = CIRCLE ( 'NONE', #40505, 1.000000000000000666 ) ;
#39658 = AXIS2_PLACEMENT_3D ( 'NONE', #34275, #3372, #19082 ) ;
#39659 = CARTESIAN_POINT ( 'NONE',  ( 84.25787305080559975, -43.86029743537079639, -47.19072229952409714 ) ) ;
#39660 = DIRECTION ( 'NONE',  ( 0.000000000000000000, -1.000000000000000000, 0.000000000000000000 ) ) ;
#39661 = CARTESIAN_POINT ( 'NONE',  ( 13.02783844833949978, -7.978462186946989831, -46.88472117783310011 ) ) ;
#39662 = VERTEX_POINT ( 'NONE', #11049 ) ;
#39663 = CARTESIAN_POINT ( 'NONE',  ( 83.63329895952738013, 13.29802447021414658, -46.55718444776781695 ) ) ;
#39664 = CARTESIAN_POINT ( 'NONE',  ( 15.91925957856740048, -50.98337423471310359, -20.31192411766179973 ) ) ;
#39665 = CARTESIAN_POINT ( 'NONE',  ( 75.47850982819889509, 12.19658742805970064, -13.41229538484630091 ) ) ;
#39666 = CARTESIAN_POINT ( 'NONE',  ( 61.62035637548115119, -45.25224449890009737, -47.09707516299204144 ) ) ;
#39667 = DIRECTION ( 'NONE',  ( 0.000000000000000000, 0.000000000000000000, 1.000000000000000000 ) ) ;
#39668 = EDGE_LOOP ( 'NONE', ( #26183, #28241, #46352, #44331, #47713 ) ) ;
#39669 = CARTESIAN_POINT ( 'NONE',  ( -2.760456472307890152, -48.90492574716959950, -5.324092234941129931 ) ) ;
#39670 = CARTESIAN_POINT ( 'NONE',  ( 47.18324198357279897, 23.57489020266570279, -54.61058319554400242 ) ) ;
#39671 = EDGE_CURVE ( 'NONE', #37113, #36574, #18640, .T. ) ;
#39672 = CARTESIAN_POINT ( 'NONE',  ( 47.13393739769619373, -38.26167638829240047, -54.64999999999999858 ) ) ;
#39673 = CARTESIAN_POINT ( 'NONE',  ( 63.47971227208819300, 1.385888765344519991, -62.64792042614390510 ) ) ;
#39674 = CARTESIAN_POINT ( 'NONE',  ( 57.34403477439209240, -50.39786884706040127, -53.00646970444169881 ) ) ;
#39675 = CARTESIAN_POINT ( 'NONE',  ( 42.63373765601389920, 12.86607404123980025, -5.023048285142680314 ) ) ;
#39676 = CARTESIAN_POINT ( 'NONE',  ( 47.64143405400680109, -54.53488714545009941, -74.14999999999999147 ) ) ;
#39677 = CARTESIAN_POINT ( 'NONE',  ( 64.54901150452380421, 0.9254890127232520136, -60.83838280017310041 ) ) ;
#39678 = CARTESIAN_POINT ( 'NONE',  ( 57.08448514777830241, -47.43174880974720509, -47.79773139290949757 ) ) ;
#39679 = CARTESIAN_POINT ( 'NONE',  ( 20.99557435765482083, -9.289990908401488667, -75.50070639236554371 ) ) ;
#39680 = ADVANCED_FACE ( 'NONE', ( #46967 ), #30939, .T. ) ;
#39681 = VECTOR ( 'NONE', #3104, 1000.000000000000000 ) ;
#39682 = CARTESIAN_POINT ( 'NONE',  ( 67.93183287108219304, -0.9264572295258779455, -17.84858513530449997 ) ) ;
#39683 = CARTESIAN_POINT ( 'NONE',  ( 18.11569087717129634, -52.24722748763079494, -75.79330468503940210 ) ) ;
#39684 = EDGE_CURVE ( 'NONE', #9603, #47075, #19799, .T. ) ;
#39685 = CARTESIAN_POINT ( 'NONE',  ( 15.49352249817719951, -23.03889485929130032, -59.59473792909209777 ) ) ;
#39686 = CARTESIAN_POINT ( 'NONE',  ( 24.04493741938377482, -14.58065008469615442, -41.46600060825795708 ) ) ;
#39687 = CARTESIAN_POINT ( 'NONE',  ( 52.52075712594130152, -50.56176064652730417, -50.61493809237359898 ) ) ;
#39688 = EDGE_LOOP ( 'NONE', ( #13336, #5963, #7674, #41433 ) ) ;
#39689 = CARTESIAN_POINT ( 'NONE',  ( 45.14276784632605910, 14.67923546272599289, -8.929571664405379749 ) ) ;
#39690 = CARTESIAN_POINT ( 'NONE',  ( 10.64863409883700029, 32.21085600226960111, -23.66469670114080159 ) ) ;
#39691 = CARTESIAN_POINT ( 'NONE',  ( 73.00373354607030763, 1.334812829108570131, -68.66140445374750811 ) ) ;
#39692 = FACE_OUTER_BOUND ( 'NONE', #4408, .T. ) ;
#39693 = CARTESIAN_POINT ( 'NONE',  ( 10.02166945824849975, -11.31308309140620061, -81.23899999999999011 ) ) ;
#39694 = ORIENTED_EDGE ( 'NONE', *, *, #49196, .T. ) ;
#39695 = CARTESIAN_POINT ( 'NONE',  ( 17.21347160910339724, 21.88381105532300097, -76.14999999999999147 ) ) ;
#39696 = ORIENTED_EDGE ( 'NONE', *, *, #3394, .T. ) ;
#39697 = VERTEX_POINT ( 'NONE', #47220 ) ;
#39698 = CIRCLE ( 'NONE', #25449, 36.50000000000000711 ) ;
#39699 = ORIENTED_EDGE ( 'NONE', *, *, #26962, .T. ) ;
#39700 = CARTESIAN_POINT ( 'NONE',  ( 57.24929578595760660, -52.61618894467940066, -63.99406948319280275 ) ) ;
#39701 = CARTESIAN_POINT ( 'NONE',  ( 23.51633084124399886, -16.17647175568000151, -81.23899999999999011 ) ) ;
#39702 = DIRECTION ( 'NONE',  ( 0.000000000000000000, 0.000000000000000000, -1.000000000000000000 ) ) ;
#39703 = VERTEX_POINT ( 'NONE', #10792 ) ;
#39704 = ADVANCED_FACE ( 'NONE', ( #26752 ), #27018, .F. ) ;
#39705 = DIRECTION ( 'NONE',  ( -1.000000000000000000, -7.683667316014053881E-33, 8.592609827796581962E-15 ) ) ;
#39706 = EDGE_LOOP ( 'NONE', ( #35228, #17599, #48199, #31279, #42347, #51370, #47832, #29198 ) ) ;
#39707 = CARTESIAN_POINT ( 'NONE',  ( 68.13393739769620083, 11.88381105532070059, -71.50000000000000000 ) ) ;
#39708 = DIRECTION ( 'NONE',  ( 0.000000000000000000, 0.000000000000000000, -1.000000000000000000 ) ) ;
#39709 = ORIENTED_EDGE ( 'NONE', *, *, #45978, .F. ) ;
#39710 = ORIENTED_EDGE ( 'NONE', *, *, #30493, .F. ) ;
#39711 = CARTESIAN_POINT ( 'NONE',  ( 8.617734227332851660, -18.16589664370942714, -50.40348811642825666 ) ) ;
#39712 = DIRECTION ( 'NONE',  ( 0.000000000000000000, 0.000000000000000000, 1.000000000000000000 ) ) ;
#39713 = CARTESIAN_POINT ( 'NONE',  ( 60.70528289702870239, 14.47951718819379963, -47.69124897247409933 ) ) ;
#39714 = CARTESIAN_POINT ( 'NONE',  ( 18.42426853117639141, -9.190374877662996767, -40.06164972454276807 ) ) ;
#39715 = CIRCLE ( 'NONE', #10431, 35.00000000000000000 ) ;
#39716 = PLANE ( 'NONE',  #41788 ) ;
#39717 = CARTESIAN_POINT ( 'NONE',  ( -3.373810796937729783, 17.44610948361469838, -5.485032747920929985 ) ) ;
#39718 = DIRECTION ( 'NONE',  ( 0.9805806756909202226, 0.000000000000000000, -0.1961161351381840445 ) ) ;
#39719 = CARTESIAN_POINT ( 'NONE',  ( 22.90066830340121840, -15.61618925674170022, -38.84718272210749035 ) ) ;
#39720 = CARTESIAN_POINT ( 'NONE',  ( 8.982413567481659200, -18.84766772212099895, -66.15241531683260234 ) ) ;
#39721 = ORIENTED_EDGE ( 'NONE', *, *, #37680, .T. ) ;
#39722 = CARTESIAN_POINT ( 'NONE',  ( 16.13393739769620083, -15.61618894467929941, -28.45282021618999835 ) ) ;
#39723 = TOROIDAL_SURFACE ( 'NONE', #32173, 9.000000000000000000, 1.000000000000000000 ) ;
#39724 = CARTESIAN_POINT ( 'NONE',  ( 42.48913757721220463, 14.65938426827190000, -7.200519650645810010 ) ) ;
#39725 = CARTESIAN_POINT ( 'NONE',  ( 72.43398376235579406, 1.116860450401449878, -69.82773512215300116 ) ) ;
#39726 = CARTESIAN_POINT ( 'NONE',  ( 42.28005749516919565, -39.79447665039643312, -74.97844900094325737 ) ) ;
#39727 = CARTESIAN_POINT ( 'NONE',  ( 15.58442563903700062, 19.61232422376169993, -20.41433498000760238 ) ) ;
#39728 = CARTESIAN_POINT ( 'NONE',  ( 50.03007040746459921, 10.05946586878370042, -78.14999999999999147 ) ) ;
#39729 = CARTESIAN_POINT ( 'NONE',  ( 10.31685475978553512, -21.02859939406643619, -32.26922283058762275 ) ) ;
#39730 = CARTESIAN_POINT ( 'NONE',  ( 24.04519454997480210, -15.61618869140488997, -79.50766696426083513 ) ) ;
#39731 = CARTESIAN_POINT ( 'NONE',  ( 48.56553214184410194, -54.10406106784840574, -54.94095612633750392 ) ) ;
#39732 = CARTESIAN_POINT ( 'NONE',  ( 52.10267377731729965, -33.11618894492853116, -20.31847448329631689 ) ) ;
#39733 = EDGE_CURVE ( 'NONE', #51582, #14157, #3920, .T. ) ;
#39734 = CARTESIAN_POINT ( 'NONE',  ( 55.58353086675839450, 22.61662994292931117, 16.85000000000000142 ) ) ;
#39735 = CARTESIAN_POINT ( 'NONE',  ( 24.04503344477293680, -15.61618896013167479, -37.50766614148061251 ) ) ;
#39736 = CARTESIAN_POINT ( 'NONE',  ( 24.04493737644245144, -14.58063772939740410, -71.75066733987638656 ) ) ;
#39737 = ADVANCED_FACE ( 'NONE', ( #18894 ), #38836, .T. ) ;
#39738 = VERTEX_POINT ( 'NONE', #40360 ) ;
#39739 = CARTESIAN_POINT ( 'NONE',  ( 12.95169883137720035, -21.91030696805099964, -79.49618351660049598 ) ) ;
#39740 =( BOUNDED_CURVE ( )  B_SPLINE_CURVE ( 3, ( #37901, #26081, #42088, #29505 ),
 .UNSPECIFIED., .F., .T. ) 
 B_SPLINE_CURVE_WITH_KNOTS ( ( 4, 4 ),
 ( -9.769962616701377556E-15, 0.7853981633974057575 ),
 .UNSPECIFIED. ) 
 CURVE ( )  GEOMETRIC_REPRESENTATION_ITEM ( )  RATIONAL_B_SPLINE_CURVE ( ( 1.000000000000000000, 0.9492530216741954519, 0.9492530216741954519, 1.000000000000000000 ) ) 
 REPRESENTATION_ITEM ( '' )  );
#39741 = CARTESIAN_POINT ( 'NONE',  ( 61.75019796695539753, 13.88381105532070059, -46.37203261889099792 ) ) ;
#39742 = VERTEX_POINT ( 'NONE', #48751 ) ;
#39743 = CARTESIAN_POINT ( 'NONE',  ( 71.39251316048110141, 1.372372808637209785, -70.31281467067098845 ) ) ;
#39744 = CARTESIAN_POINT ( 'NONE',  ( 60.91168278986669549, -45.44839912269959825, -47.20849308954799994 ) ) ;
#39745 = CARTESIAN_POINT ( 'NONE',  ( 8.222937397696199469, -15.61618894467929941, -32.14999999999999858 ) ) ;
#39746 = CARTESIAN_POINT ( 'NONE',  ( 2.633937397696199945, -15.61618894435254745, -11.11999999999999922 ) ) ;
#39748 = CARTESIAN_POINT ( 'NONE',  ( 9.127429636406484192, 23.77844269387289700, -22.14349223871028016 ) ) ;
#39747 = CARTESIAN_POINT ( 'NONE',  ( 41.94533325028437076, 8.526340366768270229, -76.59527892131112026 ) ) ;
#39749 = CARTESIAN_POINT ( 'NONE',  ( 16.13393739769620083, -15.61618894467929941, -19.08999999999999986 ) ) ;
#39750 = CARTESIAN_POINT ( 'NONE',  ( 20.11811607905615062, -8.703694080318976845, -67.17433328788270330 ) ) ;
#39751 = ORIENTED_EDGE ( 'NONE', *, *, #9284, .T. ) ;
#39752 = CARTESIAN_POINT ( 'NONE',  ( 0.06588876110915349582, 19.86606076565430001, -34.93030904342190013 ) ) ;
#39753 = AXIS2_PLACEMENT_3D ( 'NONE', #15994, #43770, #47710 ) ;
#39754 = ORIENTED_EDGE ( 'NONE', *, *, #29048, .F. ) ;
#39755 = CARTESIAN_POINT ( 'NONE',  ( 76.87859648677320479, 11.88381402801379849, -14.85884684523960075 ) ) ;
#39756 = DIRECTION ( 'NONE',  ( 0.000000000000000000, 0.000000000000000000, -1.000000000000000000 ) ) ;
#39757 = CARTESIAN_POINT ( 'NONE',  ( 12.64313521567289911, 34.23242425601760175, -47.04313497446949555 ) ) ;
#39758 = CARTESIAN_POINT ( 'NONE',  ( 10.85544419465600008, -64.15949727455540597, -45.65651250914780235 ) ) ;
#39759 = ORIENTED_EDGE ( 'NONE', *, *, #1805, .T. ) ;
#39760 = ADVANCED_FACE ( 'NONE', ( #20175 ), #35911, .T. ) ;
#39761 = CARTESIAN_POINT ( 'NONE',  ( -0.4123484725610440105, 14.05881538531380137, -35.12503119152799513 ) ) ;
#39762 = DIRECTION ( 'NONE',  ( 0.000000000000000000, 0.000000000000000000, 1.000000000000000000 ) ) ;
#39763 = CARTESIAN_POINT ( 'NONE',  ( 16.13393739769620083, -15.61618894467929941, -32.14999999999999858 ) ) ;
#39764 = AXIS2_PLACEMENT_3D ( 'NONE', #38183, #2277, #50497 ) ;
#39765 = CARTESIAN_POINT ( 'NONE',  ( 22.70470264617900824, -13.96621614738498884, -46.37453375972514635 ) ) ;
#39766 = EDGE_CURVE ( 'NONE', #5505, #2815, #8194, .T. ) ;
#39767 = CARTESIAN_POINT ( 'NONE',  ( 65.19625039218108498, 0.4699309295582059787, -17.22242890042259944 ) ) ;
#39768 = CARTESIAN_POINT ( 'NONE',  ( 51.95459423065859994, -49.70792072429919983, -76.89034159680979030 ) ) ;
#39769 = DIRECTION ( 'NONE',  ( 0.000000000000000000, -1.000000000000000000, 0.000000000000000000 ) ) ;
#39770 = ORIENTED_EDGE ( 'NONE', *, *, #50209, .F. ) ;
#39771 = CARTESIAN_POINT ( 'NONE',  ( 64.93393739769628326, 10.88381105532060111, -61.44999999999999574 ) ) ;
#39772 = CARTESIAN_POINT ( 'NONE',  ( 76.62512003803935556, 11.98806601119159509, -14.19602650844148251 ) ) ;
#39773 = CARTESIAN_POINT ( 'NONE',  ( 17.74255979488508572, -9.022132406956300699, -34.02905390904911087 ) ) ;
#39774 = CARTESIAN_POINT ( 'NONE',  ( 24.04468182044177738, -15.61618932230105017, -75.79232603942232060 ) ) ;
#39775 = CARTESIAN_POINT ( 'NONE',  ( 23.98148330126149830, -15.56354976708660054, -58.01035930781969796 ) ) ;
#39776 = CARTESIAN_POINT ( 'NONE',  ( 12.69633964006179916, -49.98156586428169845, -21.09933892718569837 ) ) ;
#39777 = CARTESIAN_POINT ( 'NONE',  ( 54.08392444393659559, 19.39418736748219629, -76.77911274294029909 ) ) ;
#39778 = CARTESIAN_POINT ( 'NONE',  ( 3.633937397696210159, -8.399310579809009525, -34.64999999999999858 ) ) ;
#39779 = CARTESIAN_POINT ( 'NONE',  ( 57.50723796698959944, 13.88381105532070059, -17.93020914085149897 ) ) ;
#39780 = CARTESIAN_POINT ( 'NONE',  ( 61.28265261588620660, -45.34131656260610299, -47.23924683292639770 ) ) ;
#39781 = DIRECTION ( 'NONE',  ( 0.000000000000000000, -1.000000000000000000, 0.000000000000000000 ) ) ;
#39782 = CARTESIAN_POINT ( 'NONE',  ( 20.88396115700760092, -10.40276075773470055, -58.58238571580489662 ) ) ;
#39783 = CARTESIAN_POINT ( 'NONE',  ( 46.95755860539310333, -39.50979427423180113, -54.16316400158059707 ) ) ;
#39784 = VERTEX_POINT ( 'NONE', #12328 ) ;
#39785 = CONICAL_SURFACE ( 'NONE', #1296, 0.7350000000000003197, 0.06981317007977388966 ) ;
#39786 = CARTESIAN_POINT ( 'NONE',  ( 14.13833173590930059, -51.13036009974659635, -74.14993170018701107 ) ) ;
#39787 = CARTESIAN_POINT ( 'NONE',  ( 47.25314650905760772, -54.75284751476729639, -54.62484584475070193 ) ) ;
#39788 = CARTESIAN_POINT ( 'NONE',  ( 41.40756764072759921, -44.77159127043780273, -5.393983506378570603 ) ) ;
#39789 = DIRECTION ( 'NONE',  ( 1.000000000000000000, 0.000000000000000000, 0.000000000000000000 ) ) ;
#39790 = CARTESIAN_POINT ( 'NONE',  ( 22.46011834663439188, -10.75453258091564024, -47.29933625624753546 ) ) ;
#39791 = CYLINDRICAL_SURFACE ( 'NONE', #46546, 1.999999999999996891 ) ;
#39792 = CARTESIAN_POINT ( 'NONE',  ( 10.73482432378980000, 33.71481228277630038, -18.15071127990200139 ) ) ;
#39793 = CARTESIAN_POINT ( 'NONE',  ( 43.34604152446959802, 4.883811055320659733, -58.29242082535468938 ) ) ;
#39795 = CARTESIAN_POINT ( 'NONE',  ( 20.11811815720405860, -22.52868256293315241, -58.12566465286644757 ) ) ;
#39794 = CARTESIAN_POINT ( 'NONE',  ( 0.6045892726184427524, -8.790618991491967904, -34.79644291222913921 ) ) ;
#39796 = EDGE_CURVE ( 'NONE', #42552, #37955, #8848, .T. ) ;
#39797 = FACE_OUTER_BOUND ( 'NONE', #21239, .T. ) ;
#39798 = CARTESIAN_POINT ( 'NONE',  ( 16.13393739769620083, -15.61618894467929941, -6.189999999999999503 ) ) ;
#39799 = LINE ( 'NONE', #47165, #5513 ) ;
#39800 = VERTEX_POINT ( 'NONE', #8921 ) ;
#39801 = CARTESIAN_POINT ( 'NONE',  ( 52.83551392347279574, -49.68567921497080420, -48.92570524573309854 ) ) ;
#39802 = ORIENTED_EDGE ( 'NONE', *, *, #41265, .F. ) ;
#39803 = CARTESIAN_POINT ( 'NONE',  ( 45.84105415622519786, 7.939782908946126483, -61.60406984308864509 ) ) ;
#39804 = CARTESIAN_POINT ( 'NONE',  ( 14.28038400710293487, -41.76263555408612405, -34.79644660940672907 ) ) ;
#39805 = DIRECTION ( 'NONE',  ( 1.000000000000000000, 0.000000000000000000, 0.000000000000000000 ) ) ;
#39806 = CARTESIAN_POINT ( 'NONE',  ( 84.13361756236649569, 12.76145366115379964, -46.96659941728370313 ) ) ;
#39807 = CARTESIAN_POINT ( 'NONE',  ( 20.97293342565509988, -10.48523619318929967, -60.19350159652129406 ) ) ;
#39808 = CARTESIAN_POINT ( 'NONE',  ( 52.82359344163219816, 18.46824642947949968, -48.95125676800460468 ) ) ;
#39809 = CARTESIAN_POINT ( 'NONE',  ( 56.39862374920090105, -45.18896474930410534, -16.03846417670529689 ) ) ;
#39810 = DIRECTION ( 'NONE',  ( 0.000000000000000000, -1.000000000000000000, 0.000000000000000000 ) ) ;
#39811 = B_SPLINE_CURVE_WITH_KNOTS ( 'NONE', 3,
 ( #11251, #27213, #43226, #7318, #51341, #47420, #48966, #40055, #45020, #36618, #44499, #19868, #215 ),
 .UNSPECIFIED., .F., .F.,
 ( 4, 2, 2, 1, 2, 2, 4 ),
 ( 0.000000000000000000, 0.2500000000000435207, 0.3750000000000643929, 0.4375000000000756062, 0.4687500000000812128, 0.5000000000000868194, 1.000000000000000000 ),
 .UNSPECIFIED. ) ;
#39812 = ORIENTED_EDGE ( 'NONE', *, *, #31618, .F. ) ;
#39813 = CARTESIAN_POINT ( 'NONE',  ( 20.62477853380519832, -9.180422162592339674, -46.98143399943669607 ) ) ;
#39814 = ORIENTED_EDGE ( 'NONE', *, *, #19984, .F. ) ;
#39815 = CARTESIAN_POINT ( 'NONE',  ( 11.50351869910530134, -65.28212171173150580, -17.32566767997679946 ) ) ;
#39816 = CARTESIAN_POINT ( 'NONE',  ( 10.32439802925660111, 33.01400591537749563, -46.37725779926459779 ) ) ;
#39817 = CARTESIAN_POINT ( 'NONE',  ( 72.93015195551900831, 1.326578174762039986, -62.47191694777300341 ) ) ;
#39818 = DIRECTION ( 'NONE',  ( 0.000000000000000000, 0.000000000000000000, 1.000000000000000000 ) ) ;
#39819 = B_SPLINE_CURVE_WITH_KNOTS ( 'NONE', 3,
 ( #8813, #44970, #9343, #48126, #12225, #24237, #28706, #24764, #9072, #41034, #28188, #8289, #676, #40774, #40264, #4354, #32365, #20323 ),
 .UNSPECIFIED., .F., .F.,
 ( 4, 2, 2, 2, 2, 2, 2, 2, 4 ),
 ( 0.4999985363739877231, 0.5624987193272391606, 0.6249989022804905980, 0.6874990852337419245, 0.7499992681869933620, 0.8124994511402450215, 0.8749996340934966810, 0.9374998170467483405, 1.000000000000000000 ),
 .UNSPECIFIED. ) ;
#39820 = CARTESIAN_POINT ( 'NONE',  ( 8.798174420955659158, 31.95288804203559607, -46.67020513285999783 ) ) ;
#39821 = CARTESIAN_POINT ( 'NONE',  ( 12.95491128060869990, -49.88685839599860117, -82.14319696191608955 ) ) ;
#39822 = AXIS2_PLACEMENT_3D ( 'NONE', #32996, #24866, #16253 ) ;
#39823 = ORIENTED_EDGE ( 'NONE', *, *, #38766, .T. ) ;
#39824 = CARTESIAN_POINT ( 'NONE',  ( 64.78711365736019445, 1.264121749638649872, -70.45005197993610579 ) ) ;
#39825 = AXIS2_PLACEMENT_3D ( 'NONE', #46904, #38775, #22239 ) ;
#39826 = CARTESIAN_POINT ( 'NONE',  ( 11.13393739769619906, -63.23117314113459031, -43.74478398217730302 ) ) ;
#39827 = CARTESIAN_POINT ( 'NONE',  ( 70.03247032090600044, 18.72622661238320063, -71.50000000000139266 ) ) ;
#39828 = VERTEX_POINT ( 'NONE', #12858 ) ;
#39829 = EDGE_CURVE ( 'NONE', #36880, #22605, #37606, .T. ) ;
#39830 = CARTESIAN_POINT ( 'NONE',  ( 10.79762425054842012, -21.53695137437687990, -44.52557491237572407 ) ) ;
#39831 = CARTESIAN_POINT ( 'NONE',  ( 21.04251040983138310, -9.375720499378973116, -77.21978301587714100 ) ) ;
#39832 = CARTESIAN_POINT ( 'NONE',  ( 13.73896035130837490, -52.05916771826542089, -75.36997958382971774 ) ) ;
#39833 = LINE ( 'NONE', #31424, #42184 ) ;
#39834 = VERTEX_POINT ( 'NONE', #24348 ) ;
#39835 = CARTESIAN_POINT ( 'NONE',  ( 23.83903384211122400, -17.68688342934473212, -61.87566199814707346 ) ) ;
#39836 = DIRECTION ( 'NONE',  ( 0.000000000000000000, 0.000000000000000000, -1.000000000000000000 ) ) ;
#39837 = DIRECTION ( 'NONE',  ( 0.000000000000000000, -1.000000000000000000, 0.000000000000000000 ) ) ;
#39838 = CARTESIAN_POINT ( 'NONE',  ( 26.52624224310950396, -9.616188944679349149, -22.14999999999999858 ) ) ;
#39839 = CARTESIAN_POINT ( 'NONE',  ( 21.82943438648850076, -21.57807070353640100, -72.04960399662019199 ) ) ;
#39840 = LINE ( 'NONE', #3689, #1253 ) ;
#39841 = EDGE_CURVE ( 'NONE', #7973, #29283, #23889, .T. ) ;
#39842 = DIRECTION ( 'NONE',  ( 0.000000000000000000, 0.000000000000000000, -1.000000000000000000 ) ) ;
#39843 = APPLICATION_PROTOCOL_DEFINITION ( 'draft international standard', 'automotive_design', 1998, #33465 ) ;
#39844 = VERTEX_POINT ( 'NONE', #44289 ) ;
#39845 = CARTESIAN_POINT ( 'NONE',  ( 8.686118456258421716, -15.42465090483799983, -61.24084159088819490 ) ) ;
#39846 = AXIS2_PLACEMENT_3D ( 'NONE', #47878, #51800, #15392 ) ;
#39847 = CARTESIAN_POINT ( 'NONE',  ( 22.90121638405171467, -15.61618906730874734, -72.84718036870921765 ) ) ;
#39848 = CARTESIAN_POINT ( 'NONE',  ( 11.63393739769600010, 10.38381105532060111, -35.14999999999999858 ) ) ;
#39849 = AXIS2_PLACEMENT_3D ( 'NONE', #39864, #3194, #3966 ) ;
#39850 = CARTESIAN_POINT ( 'NONE',  ( 46.35275103504439898, 21.67755452994670406, -76.14999999999999147 ) ) ;
#39851 = CARTESIAN_POINT ( 'NONE',  ( 71.23851365796429036, 1.390208944942409985, -61.02997314496759884 ) ) ;
#39852 = PRODUCT_DEFINITION_SHAPE ( 'NONE', 'NONE',  #48485 ) ;
#39853 = CARTESIAN_POINT ( 'NONE',  ( 16.13393739769620083, -15.61618894467929941, -32.14999999999999858 ) ) ;
#39854 = CARTESIAN_POINT ( 'NONE',  ( 12.17667205660850094, 33.72359997743659932, -16.26506704563800199 ) ) ;
#39855 = AXIS2_PLACEMENT_3D ( 'NONE', #34497, #22434, #31072 ) ;
#39856 = CARTESIAN_POINT ( 'NONE',  ( 14.09735820809919993, -7.626503975077850050, -74.92822277435439560 ) ) ;
#39857 = CIRCLE ( 'NONE', #17272, 6.000000000000005329 ) ;
#39858 = CARTESIAN_POINT ( 'NONE',  ( 57.06416426806980269, -50.61857174473429666, -74.65301306984240171 ) ) ;
#39860 = CARTESIAN_POINT ( 'NONE',  ( 10.52466370152206565, -55.22087153724935860, -45.55758753228428048 ) ) ;
#39859 = CARTESIAN_POINT ( 'NONE',  ( 12.95491128060830022, 18.65448050664010182, -82.14319696191608955 ) ) ;
#39861 = EDGE_CURVE ( 'NONE', #42806, #16604, #38143, .T. ) ;
#39862 = CARTESIAN_POINT ( 'NONE',  ( 63.00666467042349694, 0.8838110553206759423, -68.76625967790960203 ) ) ;
#39863 = CARTESIAN_POINT ( 'NONE',  ( 61.28624124790810157, 14.05922653848760007, -47.08353149416500827 ) ) ;
#39864 = CARTESIAN_POINT ( 'NONE',  ( 57.77564497937559906, -28.11618894467929763, -20.65000000000000213 ) ) ;
#39865 = ADVANCED_FACE ( 'NONE', ( #29078 ), #13054, .T. ) ;
#39866 = ORIENTED_EDGE ( 'NONE', *, *, #2519, .F. ) ;
#39867 = CARTESIAN_POINT ( 'NONE',  ( 52.96846357502160174, -49.58824783477410136, -48.76456334744820253 ) ) ;
#39868 = ADVANCED_FACE ( 'NONE', ( #4457 ), #13124, .T. ) ;
#39869 = CARTESIAN_POINT ( 'NONE',  ( 58.60333746479689410, -45.35543772810689944, -26.24757126836300003 ) ) ;
#39870 = DIRECTION ( 'NONE',  ( 1.000000000000000000, 0.000000000000000000, 0.000000000000000000 ) ) ;
#39871 = CARTESIAN_POINT ( 'NONE',  ( 61.40708214766610240, 14.14652340182849954, -47.36186230186000046 ) ) ;
#39872 = CARTESIAN_POINT ( 'NONE',  ( 21.90095873945579896, -20.33298432383600129, -76.45087635510310520 ) ) ;
#39873 = EDGE_CURVE ( 'NONE', #43147, #4357, #20050, .T. ) ;
#39874 = CARTESIAN_POINT ( 'NONE',  ( 51.15450546912109786, 17.91792957071369941, -76.44814621710780500 ) ) ;
#39875 = CARTESIAN_POINT ( 'NONE',  ( 53.45906946093850109, 18.13273169594320322, -49.00044373679480003 ) ) ;
#39876 = CARTESIAN_POINT ( 'NONE',  ( 48.93887227096879400, 13.88381105532070059, -44.18916148508130703 ) ) ;
#39877 = CARTESIAN_POINT ( 'NONE',  ( -0.4410626023037830246, -8.356009309619699010, -35.14999999999999858 ) ) ;
#39878 = B_SPLINE_CURVE_WITH_KNOTS ( 'NONE', 3,
 ( #24551, #7581, #35341, #51343, #31906, #47421, #28239, #27473, #8340, #43983, #15441, #23525, #11775, #32158 ),
 .UNSPECIFIED., .F., .F.,
 ( 4, 2, 2, 2, 2, 2, 4 ),
 ( 3.901664560647569946, 4.407177605192729608, 8.834505823316810336, 16.99747883129379744, 26.70074659151990204, 31.55238047163300052, 38.13645368273460434 ),
 .UNSPECIFIED. ) ;
#39879 = CIRCLE ( 'NONE', #14776, 2.000000000000000000 ) ;
#39880 = VERTEX_POINT ( 'NONE', #44038 ) ;
#39881 = CARTESIAN_POINT ( 'NONE',  ( 7.349327706869664745, -6.831579253852827271, -22.14999999999998792 ) ) ;
#39882 = CARTESIAN_POINT ( 'NONE',  ( 47.49651569575760135, -54.60323047930179996, -54.97533461431780211 ) ) ;
#39883 = CARTESIAN_POINT ( 'NONE',  ( 17.41965231446239670, -8.681529881159590900, -68.40553316769369019 ) ) ;
#39884 = CARTESIAN_POINT ( 'NONE',  ( 38.67452568954060155, -36.11618894467930119, -81.65000000000000568 ) ) ;
#39885 = CARTESIAN_POINT ( 'NONE',  ( 62.08467266925860173, -31.29317986265380114, -16.78003447424929817 ) ) ;
#39886 = CARTESIAN_POINT ( 'NONE',  ( 71.48629080024771554, 0.9281439705311279598, -60.67386159597580075 ) ) ;
#39887 = CARTESIAN_POINT ( 'NONE',  ( 11.13393739769619906, 32.24192143019860168, -43.75640488079960733 ) ) ;
#39888 = CARTESIAN_POINT ( 'NONE',  ( 72.51356393101009701, 1.400155911913269824, -61.82657703151539863 ) ) ;
#39889 = AXIS2_PLACEMENT_3D ( 'NONE', #31522, #12150, #35734 ) ;
#39890 = ADVANCED_FACE ( 'NONE', ( #8142 ), #24086, .T. ) ;
#39891 = CARTESIAN_POINT ( 'NONE',  ( 9.367100842286962603, -16.03594358554465416, -41.82744396597921366 ) ) ;
#39892 = CIRCLE ( 'NONE', #42401, 9.500000000000000000 ) ;
#39893 = CARTESIAN_POINT ( 'NONE',  ( 22.84872475465979846, -14.59283129166942494, -66.40475728675967559 ) ) ;
#39894 = ORIENTED_EDGE ( 'NONE', *, *, #17547, .F. ) ;
#39895 = ORIENTED_EDGE ( 'NONE', *, *, #2144, .T. ) ;
#39896 = CARTESIAN_POINT ( 'NONE',  ( 20.11803733297233165, -8.703646999513249938, -55.45899019443132971 ) ) ;
#39897 = CARTESIAN_POINT ( 'NONE',  ( 50.37360157917204617, -30.41936351533771088, -16.20717240613429766 ) ) ;
#39898 = VERTEX_POINT ( 'NONE', #48486 ) ;
#39899 = EDGE_CURVE ( 'NONE', #16152, #30077, #6995, .T. ) ;
#39900 = CARTESIAN_POINT ( 'NONE',  ( 11.67619942398489918, -64.89165360645620240, -45.08494251881790404 ) ) ;
#39901 = DIRECTION ( 'NONE',  ( -0.04040038076619560659, -0.02935259477425090566, 0.9987523388778446476 ) ) ;
#39902 = ORIENTED_EDGE ( 'NONE', *, *, #8895, .F. ) ;
#39903 = CARTESIAN_POINT ( 'NONE',  ( 13.28146700901381827, -21.80339731933624847, -81.09015078194161674 ) ) ;
#39904 = CARTESIAN_POINT ( 'NONE',  ( 42.27050190383921802, 6.434495523153046292, -78.96717512227382940 ) ) ;
#39905 = AXIS2_PLACEMENT_3D ( 'NONE', #25990, #50636, #30443 ) ;
#39906 = CARTESIAN_POINT ( 'NONE',  ( 24.04493055343453278, -15.62694002210068156, -65.50809896301348090 ) ) ;
#39907 = CARTESIAN_POINT ( 'NONE',  ( 8.330844340317721475, -12.95264641754989832, -42.89703736520829125 ) ) ;
#39908 = CARTESIAN_POINT ( 'NONE',  ( 9.221425662475672524, -19.60033986558276808, -68.34100135745960358 ) ) ;
#39909 = CARTESIAN_POINT ( 'NONE',  ( 10.63085952368594889, 33.60671464058745528, -18.12437699077790398 ) ) ;
#39910 = CARTESIAN_POINT ( 'NONE',  ( 59.34191102089160097, -28.54411838181400185, -15.68387058390849731 ) ) ;
#39911 = CARTESIAN_POINT ( 'NONE',  ( 12.07188845762700069, -65.28371144306440499, -23.58588067924090126 ) ) ;
#39912 = CARTESIAN_POINT ( 'NONE',  ( 11.61399867763840099, -21.53875998735910002, -34.94015647776650013 ) ) ;
#39913 = ADVANCED_FACE ( 'NONE', ( #46123 ), #22236, .T. ) ;
#39914 = CARTESIAN_POINT ( 'NONE',  ( 41.10495153987889694, 13.67547663053780127, -5.488531527733360171 ) ) ;
#39915 = AXIS2_PLACEMENT_3D ( 'NONE', #30935, #22813, #18372 ) ;
#39916 = B_SPLINE_CURVE_WITH_KNOTS ( 'NONE', 3,
 ( #25787, #49677, #29981, #13768, #30247, #42588, #10092, #42062, #22122, #42326, #6684, #2230, #6426, #2486, #22644, #38661, #2749, #11394, #35994, #47806, #7721, #51730, #111, #3786, #15824, #19756, #11912, #47552, #47305 ),
 .UNSPECIFIED., .F., .F.,
 ( 4, 2, 1, 1, 1, 1, 1, 2, 2, 2, 2, 2, 2, 2, 2, 2, 4 ),
 ( 0.5000074908953238140, 0.5002516278626603086, 0.5004957648299966921, 0.5009840387646694593, 0.5019605866340145495, 0.5039136823727047299, 0.5078198738500852016, 0.5156322568048457011, 0.5312570227143668111, 0.5625065545334089201, 0.6250056181714933601, 0.6875046818095776890, 0.7500037454476620180, 0.8125028090857464580, 0.8750018727238310090, 0.9375009363619155600, 1.000000000000000000 ),
 .UNSPECIFIED. ) ;
#39917 = LINE ( 'NONE', #16059, #43481 ) ;
#39918 = CARTESIAN_POINT ( 'NONE',  ( 83.85202357338310719, -44.35879849486410365, -46.78691132286899546 ) ) ;
#39919 = AXIS2_PLACEMENT_3D ( 'NONE', #48824, #12929, #4791 ) ;
#39920 = CARTESIAN_POINT ( 'NONE',  ( 64.86412778899749298, 1.402436395646509792, -70.21307676274530252 ) ) ;
#39921 = CARTESIAN_POINT ( 'NONE',  ( 13.98591064026810038, -7.655742866829910120, -42.92377462465219651 ) ) ;
#39922 = ORIENTED_EDGE ( 'NONE', *, *, #22346, .T. ) ;
#39923 = CARTESIAN_POINT ( 'NONE',  ( 52.77132806972499424, -49.69320935574780407, -28.08932869332100069 ) ) ;
#39924 = CARTESIAN_POINT ( 'NONE',  ( 13.94847430741750038, -50.27910463884859382, -20.89779807319060012 ) ) ;
#39925 = CARTESIAN_POINT ( 'NONE',  ( 75.44242163376010524, 10.98619150729950000, -13.23847946865800118 ) ) ;
#39926 = CARTESIAN_POINT ( 'NONE',  ( 20.29253959100516624, -21.02756285422321625, -56.74444169921939363 ) ) ;
#39927 = CARTESIAN_POINT ( 'NONE',  ( 18.13393739769620083, -32.62399965035220362, -35.14999999999999858 ) ) ;
#39928 = ORIENTED_EDGE ( 'NONE', *, *, #33363, .T. ) ;
#39929 = CARTESIAN_POINT ( 'NONE',  ( -8.077363885194191795, -45.04970852165219952, -5.734713034113010366 ) ) ;
#39930 = DIRECTION ( 'NONE',  ( 0.000000000000000000, 0.000000000000000000, -1.000000000000000000 ) ) ;
#39931 = VECTOR ( 'NONE', #1275, 1000.000000000000114 ) ;
#39932 = LINE ( 'NONE', #23657, #23652 ) ;
#39933 = CARTESIAN_POINT ( 'NONE',  ( 63.46018632244250313, 1.384447124000270035, -62.70866005236110396 ) ) ;
#39934 = CARTESIAN_POINT ( 'NONE',  ( 57.55751162063140214, -50.09049722514059511, -52.57651812413949699 ) ) ;
#39935 = CARTESIAN_POINT ( 'NONE',  ( 43.46307289448610334, 11.85965047528820016, -4.765184494693460060 ) ) ;
#39936 = EDGE_CURVE ( 'NONE', #19952, #40162, #43196, .T. ) ;
#39937 = CARTESIAN_POINT ( 'NONE',  ( 16.13393739769620083, -15.61618894467929941, -74.14999999999999147 ) ) ;
#39938 = CARTESIAN_POINT ( 'NONE',  ( 0.1457839871805957643, 14.73018012514992137, -34.68167748489143776 ) ) ;
#39939 = CARTESIAN_POINT ( 'NONE',  ( 63.00666467042349694, 0.8838110553206759423, -68.76625967790960203 ) ) ;
#39940 = CARTESIAN_POINT ( 'NONE',  ( 9.807682588839810478, -10.75462586085395245, -75.00070004298494553 ) ) ;
#39941 = CARTESIAN_POINT ( 'NONE',  ( 68.13393739769625768, -15.41618894467990764, -28.20067248431510976 ) ) ;
#39942 = CARTESIAN_POINT ( 'NONE',  ( 17.21347160910390173, -53.11618894467930119, -76.14999999999999147 ) ) ;
#39943 = CARTESIAN_POINT ( 'NONE',  ( 21.49792027126889948, -10.44565879097549832, -64.82318737929099939 ) ) ;
#39944 = CARTESIAN_POINT ( 'NONE',  ( 9.807870126734302474, -10.75438522751455395, -72.71600167733724618 ) ) ;
#39945 = CARTESIAN_POINT ( 'NONE',  ( 55.78679745002460066, -46.85824937871690565, -46.15739089836610276 ) ) ;
#39946 = ORIENTED_EDGE ( 'NONE', *, *, #38340, .T. ) ;
#39947 = CARTESIAN_POINT ( 'NONE',  ( 8.808908491334550561, 32.01182072428549930, -46.67060441505820023 ) ) ;
#39948 = CARTESIAN_POINT ( 'NONE',  ( 22.80495416686178345, -16.79151856191942471, -34.50832474881546830 ) ) ;
#39949 = B_SPLINE_CURVE_WITH_KNOTS ( 'NONE', 3,
 ( #39998, #15891, #8547, #48374, #51788, #36054, #31847, #36302, #3843, #47609, #15636, #14668, #7775, #8280, #4087, #27925, #34573, #27672 ),
 .UNSPECIFIED., .F., .F.,
 ( 4, 2, 2, 2, 2, 2, 2, 2, 4 ),
 ( 0.5000000032568245878, 0.5625000028497215698, 0.6250000024426184408, 0.6875000020355153119, 0.7500000016284122939, 0.8125000012213092759, 0.8750000008142061469, 0.9375000004071030180, 1.000000000000000000 ),
 .UNSPECIFIED. ) ;
#39950 = CARTESIAN_POINT ( 'NONE',  ( 9.206240469540899696, -13.25622428000860076, -81.23899999999999011 ) ) ;
#39951 = ORIENTED_EDGE ( 'NONE', *, *, #27971, .F. ) ;
#39952 = CARTESIAN_POINT ( 'NONE',  ( 17.85447849914849883, 20.77357945327109690, -75.79069550273320033 ) ) ;
#39953 = VERTEX_POINT ( 'NONE', #1821 ) ;
#39954 = EDGE_LOOP ( 'NONE', ( #1817, #13409, #49548, #31416, #21578 ) ) ;
#39955 = EDGE_CURVE ( 'NONE', #21076, #9565, #21465, .T. ) ;
#39956 = CARTESIAN_POINT ( 'NONE',  ( 56.54338727600670467, -46.22346027527899537, -26.26862031791669949 ) ) ;
#39957 = CARTESIAN_POINT ( 'NONE',  ( 22.63910790963710085, -11.37884432564429815, -81.23899999999999011 ) ) ;
#39958 = CARTESIAN_POINT ( 'NONE',  ( 61.55801500889180033, 14.08519212220829964, -47.24870750647819762 ) ) ;
#39959 = ORIENTED_EDGE ( 'NONE', *, *, #43202, .T. ) ;
#39960 = DIRECTION ( 'NONE',  ( 0.000000000000000000, 0.000000000000000000, -1.000000000000000000 ) ) ;
#39961 = EDGE_LOOP ( 'NONE', ( #24500, #42662, #42928, #47391, #32898, #12839, #6315 ) ) ;
#39962 = DIRECTION ( 'NONE',  ( 1.000000000000000000, 0.000000000000000000, 0.000000000000000000 ) ) ;
#39963 = CARTESIAN_POINT ( 'NONE',  ( 16.13393739707289853, -15.61618894541809865, -10.45000000021869901 ) ) ;
#39964 = ORIENTED_EDGE ( 'NONE', *, *, #30668, .F. ) ;
#39965 = EDGE_LOOP ( 'NONE', ( #8676, #46610 ) ) ;
#39966 = CARTESIAN_POINT ( 'NONE',  ( 44.66893810599722059, 1.931900683508221306, -44.67038416013655677 ) ) ;
#39967 = DIRECTION ( 'NONE',  ( 0.3535533905932736198, -0.6123724356957950254, 0.7071067811865472397 ) ) ;
#39968 = CARTESIAN_POINT ( 'NONE',  ( 60.76852316973799617, 14.41550492289180063, -47.61461981903249807 ) ) ;
#39969 = VECTOR ( 'NONE', #29498, 1000.000000000000000 ) ;
#39970 = EDGE_CURVE ( 'NONE', #27228, #38928, #33240, .T. ) ;
#39971 = EDGE_CURVE ( 'NONE', #2811, #5359, #27462, .T. ) ;
#39972 = DIRECTION ( 'NONE',  ( 0.000000000000000000, 0.000000000000000000, -1.000000000000000000 ) ) ;
#39973 = CIRCLE ( 'NONE', #41650, 1.000000000000000888 ) ;
#39974 = CARTESIAN_POINT ( 'NONE',  ( 41.06001671441610057, -44.29932858193069478, -3.719606166043679885 ) ) ;
#39975 = CARTESIAN_POINT ( 'NONE',  ( -7.100262879277110528, 14.45415374298890043, -4.868184076090540380 ) ) ;
#39976 = CARTESIAN_POINT ( 'NONE',  ( 0.6045892726184849408, -22.44175889786657763, -34.79644291222908237 ) ) ;
#39977 = CARTESIAN_POINT ( 'NONE',  ( 57.57964031801950000, 14.54583681789700123, -26.30006412837039775 ) ) ;
#39978 = CARTESIAN_POINT ( 'NONE',  ( 23.31239132799949587, -18.78739492248890031, -67.41991821385059325 ) ) ;
#39979 = ORIENTED_EDGE ( 'NONE', *, *, #5333, .F. ) ;
#39980 = FACE_OUTER_BOUND ( 'NONE', #31089, .T. ) ;
#39981 = CARTESIAN_POINT ( 'NONE',  ( 21.80209328419340054, -11.41921765328320149, -76.64430199831019763 ) ) ;
#39982 = CARTESIAN_POINT ( 'NONE',  ( 11.74952994020519981, 33.73588971661489921, -45.42180763390059894 ) ) ;
#39983 = PRODUCT_DEFINITION_CONTEXT ( 'detailed design', #30789, 'design' ) ;
#39984 = CARTESIAN_POINT ( 'NONE',  ( 72.37391086482439562, 1.440335647928530083, -69.57825580936660970 ) ) ;
#39985 = CARTESIAN_POINT ( 'NONE',  ( 43.36319213471767853, -39.89965443588339156, -69.74287559708298545 ) ) ;
#39986 = EDGE_CURVE ( 'NONE', #48851, #36898, #16357, .T. ) ;
#39987 = CARTESIAN_POINT ( 'NONE',  ( 50.03007040746459921, 10.05946586878370042, -78.14999999999999147 ) ) ;
#39988 = CARTESIAN_POINT ( 'NONE',  ( 13.29299421255960034, 18.84434171226279986, -21.00266242150379981 ) ) ;
#39989 = EDGE_CURVE ( 'NONE', #49314, #49834, #26425, .T. ) ;
#39990 = CARTESIAN_POINT ( 'NONE',  ( 47.04950481043260169, 23.22170069367189882, -75.29714959418029707 ) ) ;
#39991 = CARTESIAN_POINT ( 'NONE',  ( 48.57498399731990446, -54.11662796927669916, -55.03331795735149967 ) ) ;
#39992 = CARTESIAN_POINT ( 'NONE',  ( -5.866062602303799167, -15.61618894467929586, -13.15000000000000036 ) ) ;
#39993 = CARTESIAN_POINT ( 'NONE',  ( 16.13393739769620083, -27.61618894467930474, -22.14999999999999858 ) ) ;
#39994 = DIRECTION ( 'NONE',  ( 0.5685928097855371677, 0.5944782866685501821, -0.5685928097855381669 ) ) ;
#39995 = CARTESIAN_POINT ( 'NONE',  ( 9.367870520905830389, -16.42710664673399990, -71.80902927999524366 ) ) ;
#39996 = VERTEX_POINT ( 'NONE', #6531 ) ;
#39997 = CARTESIAN_POINT ( 'NONE',  ( 22.99224927569089871, -17.26127340059479920, -80.92212427574548883 ) ) ;
#39998 = CARTESIAN_POINT ( 'NONE',  ( 22.90071877914020249, -15.61618922162072565, -76.45281474520940890 ) ) ;
#39999 = ORIENTED_EDGE ( 'NONE', *, *, #38516, .T. ) ;
#40000 = DIRECTION ( 'NONE',  ( 0.5516667872527449834, -0.8340645993220396903, -3.885780586188043947E-16 ) ) ;
#40001 = CARTESIAN_POINT ( 'NONE',  ( 60.87670858091210135, -45.49189414910050289, -47.32752941579799710 ) ) ;
#40002 = CARTESIAN_POINT ( 'NONE',  ( 48.03526516117433687, -54.27886751425135259, -54.71370355240628669 ) ) ;
#40003 = AXIS2_PLACEMENT_3D ( 'NONE', #46946, #2130, #10516 ) ;
#40004 = DIRECTION ( 'NONE',  ( -0.5877852522924744694, -0.8090169943749464521, 0.000000000000000000 ) ) ;
#40006 = CARTESIAN_POINT ( 'NONE',  ( 19.40270147970570136, 17.88381105532069881, -34.64999999999999858 ) ) ;
#40005 = CARTESIAN_POINT ( 'NONE',  ( 42.20273094283171389, 8.553841343497502692, -75.35254198661807834 ) ) ;
#40007 = CARTESIAN_POINT ( 'NONE',  ( 71.29497000743199919, 0.8840451408750739093, -70.74985906855570761 ) ) ;
#40008 = CYLINDRICAL_SURFACE ( 'NONE', #25267, 6.766999999999998572 ) ;
#40009 = EDGE_LOOP ( 'NONE', ( #32842, #26285 ) ) ;
#40010 = FACE_OUTER_BOUND ( 'NONE', #32145, .T. ) ;
#40011 = ORIENTED_EDGE ( 'NONE', *, *, #8398, .F. ) ;
#40012 = CIRCLE ( 'NONE', #37462, 1.999999999999999556 ) ;
#40013 = ORIENTED_EDGE ( 'NONE', *, *, #9772, .T. ) ;
#40014 = DIRECTION ( 'NONE',  ( 0.000000000000000000, -1.000000000000000000, 0.000000000000000000 ) ) ;
#40015 = CARTESIAN_POINT ( 'NONE',  ( 22.46011021147963405, -10.75452141403957107, -79.58400001792948331 ) ) ;
#40016 = CARTESIAN_POINT ( 'NONE',  ( 76.39175890687408810, -17.20318815803477008, -12.76101989214891042 ) ) ;
#40017 = CARTESIAN_POINT ( 'NONE',  ( 52.33875389174439619, -52.31399363568380068, -53.58658487175770091 ) ) ;
#40018 = ORIENTED_EDGE ( 'NONE', *, *, #50882, .F. ) ;
#40019 = ORIENTED_EDGE ( 'NONE', *, *, #48613, .F. ) ;
#40020 = CARTESIAN_POINT ( 'NONE',  ( 1.058369240368480124, -8.644356418428410294, -34.64999999999999858 ) ) ;
#40021 = DIRECTION ( 'NONE',  ( 1.000000000000000000, 0.000000000000000000, 0.000000000000000000 ) ) ;
#40022 = CARTESIAN_POINT ( 'NONE',  ( 56.37791752366599951, -50.59128047935769956, -52.96495778846580293 ) ) ;
#40023 = CARTESIAN_POINT ( 'NONE',  ( 12.72603455780808801, -9.703227352568038810, -35.78615263577922434 ) ) ;
#40024 = CARTESIAN_POINT ( 'NONE',  ( 61.86520133577609926, -0.04549255600530619642, -16.70179762356000097 ) ) ;
#40025 = CARTESIAN_POINT ( 'NONE',  ( 51.85719455852780158, -49.29163194590670116, -77.06877200303979691 ) ) ;
#40026 = EDGE_LOOP ( 'NONE', ( #28525, #47745, #10176, #25223 ) ) ;
#40027 = CARTESIAN_POINT ( 'NONE',  ( 63.02029346573409185, 0.8838110553206740549, -68.78868353141480441 ) ) ;
#40028 = CARTESIAN_POINT ( 'NONE',  ( 52.27433127813800695, -49.79152405959709426, -77.19764541630020460 ) ) ;
#40029 = CARTESIAN_POINT ( 'NONE',  ( 16.15327313186332248, -8.825424306557579257, -33.95380833013259547 ) ) ;
#40030 = DIRECTION ( 'NONE',  ( 0.000000000000000000, 0.000000000000000000, -1.000000000000000000 ) ) ;
#40031 = CARTESIAN_POINT ( 'NONE',  ( 9.097165979443349926, -12.14191267488699921, -55.15847778952939962 ) ) ;
#40032 = ADVANCED_FACE ( 'NONE', ( #38502 ), #2603, .T. ) ;
#40033 = CARTESIAN_POINT ( 'NONE',  ( 13.03464451127720025, -50.12146493690359961, -21.08705571738870077 ) ) ;
#40034 = CARTESIAN_POINT ( 'NONE',  ( 54.70720528295199614, 19.38381105532069881, -76.79588817750999397 ) ) ;
#40035 = CARTESIAN_POINT ( 'NONE',  ( -21.36606260230379917, 21.88381105532059934, 11.84999999999999964 ) ) ;
#40036 = EDGE_CURVE ( 'NONE', #33273, #13585, #6340, .T. ) ;
#40037 = CARTESIAN_POINT ( 'NONE',  ( 66.23540447448809232, -49.95860450174330225, -73.25000000000169109 ) ) ;
#40038 = CARTESIAN_POINT ( 'NONE',  ( 8.942935310824500661, 18.10006093832389951, -34.64999999999999858 ) ) ;
#40039 = DIRECTION ( 'NONE',  ( 0.7702700562049007438, -0.6377178376947748584, -1.307070999999999778E-15 ) ) ;
#40040 = AXIS2_PLACEMENT_3D ( 'NONE', #48670, #37383, #441 ) ;
#40041 = CARTESIAN_POINT ( 'NONE',  ( 17.30144337755399775, -22.57172551358950230, -51.29424405795189301 ) ) ;
#40042 = CARTESIAN_POINT ( 'NONE',  ( 17.80204587918421311, -52.64324137133318970, -76.02665054607163597 ) ) ;
#40043 = EDGE_LOOP ( 'NONE', ( #39546, #4613, #20793, #30398, #4085 ) ) ;
#40044 = CARTESIAN_POINT ( 'NONE',  ( 47.20214429186539462, 22.74469373903359681, -75.65864031442400517 ) ) ;
#40045 = CARTESIAN_POINT ( 'NONE',  ( 47.40268433751139554, -54.65101820823279866, -54.72406345013450135 ) ) ;
#40046 = CARTESIAN_POINT ( 'NONE',  ( 16.13393739769620083, -15.61618894467929941, -11.11999999999999922 ) ) ;
#40047 = DIRECTION ( 'NONE',  ( 0.000000000000000000, -1.000000000000000000, 0.000000000000000000 ) ) ;
#40048 =( BOUNDED_CURVE ( )  B_SPLINE_CURVE ( 3, ( #29032, #21665, #9640, #13079 ),
 .UNSPECIFIED., .F., .T. ) 
 B_SPLINE_CURVE_WITH_KNOTS ( ( 4, 4 ),
 ( 0.7390344460998500287, 0.8357509604174070406 ),
 .UNSPECIFIED. ) 
 CURVE ( )  GEOMETRIC_REPRESENTATION_ITEM ( )  RATIONAL_B_SPLINE_CURVE ( ( 1.000000000000000000, 0.9992206448841429722, 0.9992206448841429722, 1.000000000000000000 ) ) 
 REPRESENTATION_ITEM ( '' )  );
#40049 = CARTESIAN_POINT ( 'NONE',  ( 16.13393739769620083, -15.61618894467929941, -32.14999999999999858 ) ) ;
#40050 = CARTESIAN_POINT ( 'NONE',  ( 20.29253893682858845, -10.20481459075288555, -76.16113288888496413 ) ) ;
#40051 = EDGE_CURVE ( 'NONE', #4357, #23707, #35101, .T. ) ;
#40052 = CARTESIAN_POINT ( 'NONE',  ( 10.98409431999460040, 33.91773787654379646, -18.15364188623160047 ) ) ;
#40053 = CARTESIAN_POINT ( 'NONE',  ( 72.43509047223599850, 1.031856533264720266, -69.83351529264139401 ) ) ;
#40055 = CARTESIAN_POINT ( 'NONE',  ( 11.30082206529223043, 33.08990382518435780, -24.05782791655008879 ) ) ;
#40054 = CARTESIAN_POINT ( 'NONE',  ( 60.91034051252194104, 14.19489810164233567, -46.97125969379186472 ) ) ;
#40056 = DIRECTION ( 'NONE',  ( 0.000000000000000000, 1.000000000000000000, 0.000000000000000000 ) ) ;
#40057 = VERTEX_POINT ( 'NONE', #36611 ) ;
#40058 = CARTESIAN_POINT ( 'NONE',  ( 52.97994255623930115, -49.61893679407219793, -49.03242412254559923 ) ) ;
#40059 = ORIENTED_EDGE ( 'NONE', *, *, #43889, .F. ) ;
#40060 = CARTESIAN_POINT ( 'NONE',  ( 44.67636077250357118, 7.841592789065577662, -67.36726970128053438 ) ) ;
#40061 = DIRECTION ( 'NONE',  ( 0.000000000000000000, 0.000000000000000000, 1.000000000000000000 ) ) ;
#40062 = CARTESIAN_POINT ( 'NONE',  ( 11.89321781987602833, 34.20365306160432795, -18.08603052195102379 ) ) ;
#40064 = CARTESIAN_POINT ( 'NONE',  ( 54.64278745374110002, 16.37561111237029721, -26.20171088721290076 ) ) ;
#40063 = CARTESIAN_POINT ( 'NONE',  ( 84.44784216359251161, 11.88381105532070059, -47.47585302082339354 ) ) ;
#40065 = CARTESIAN_POINT ( 'NONE',  ( 22.95140634437030158, -13.80934754108039897, -50.37035414463250049 ) ) ;
#40066 = CARTESIAN_POINT ( 'NONE',  ( 52.74562310603300119, 18.50712734077499988, -48.86764753959050012 ) ) ;
#40067 = CARTESIAN_POINT ( 'NONE',  ( 56.79701897584680381, -45.18238399616610224, -16.80948030656859871 ) ) ;
#40068 = PLANE ( 'NONE',  #29796 ) ;
#40069 = ORIENTED_EDGE ( 'NONE', *, *, #32482, .F. ) ;
#40070 = CARTESIAN_POINT ( 'NONE',  ( 8.286224014182360875, -15.60423765184120093, -44.28799034327369100 ) ) ;
#40071 = VERTEX_POINT ( 'NONE', #8079 ) ;
#40072 = CARTESIAN_POINT ( 'NONE',  ( 11.56756868770579949, -65.34628264660689467, -17.53311441804959969 ) ) ;
#40073 = CARTESIAN_POINT ( 'NONE',  ( 10.43078750819270084, 32.63024664643640449, -45.92124766861530105 ) ) ;
#40074 = CARTESIAN_POINT ( 'NONE',  ( -9.882013117715120032, -40.49932216338130075, -19.14999999999999858 ) ) ;
#40075 = B_SPLINE_CURVE_WITH_KNOTS ( 'NONE', 3,
 ( #19957, #12120, #7925, #23875, #35949, #36203, #16295, #70, #40662, #16043, #31998, #48019, #5551, #45898, #20994, #45633, #5030, #36991 ),
 .UNSPECIFIED., .F., .F.,
 ( 4, 2, 2, 2, 2, 2, 2, 2, 4 ),
 ( 0.000000000000000000, 0.06250000038613703901, 0.1250000007722740780, 0.1875000011584111170, 0.2500000015445481560, 0.3125000019306851118, 0.3750000023168220120, 0.4375000027029589678, 0.5000000030890958680 ),
 .UNSPECIFIED. ) ;
#40076 = CARTESIAN_POINT ( 'NONE',  ( 48.48453225901420183, -53.88010102980479843, -54.18220335411630373 ) ) ;
#40077 = CARTESIAN_POINT ( 'NONE',  ( 11.36441734053757280, -65.23609907320785339, -22.79629275943423750 ) ) ;
#40078 = FACE_OUTER_BOUND ( 'NONE', #32000, .T. ) ;
#40079 = AXIS2_PLACEMENT_3D ( 'NONE', #41513, #1683, #6400 ) ;
#40080 = VECTOR ( 'NONE', #9909, 1000.000000000000000 ) ;
#40081 = VERTEX_POINT ( 'NONE', #39788 ) ;
#40082 = CARTESIAN_POINT ( 'NONE',  ( 20.99557930478071910, -9.289994860631022533, -75.21597186361574927 ) ) ;
#40083 = DIRECTION ( 'NONE',  ( 0.000000000000000000, -1.000000000000000000, 0.000000000000000000 ) ) ;
#40084 = DIRECTION ( 'NONE',  ( 0.000000000000000000, 0.000000000000000000, -1.000000000000000000 ) ) ;
#40085 = ORIENTED_EDGE ( 'NONE', *, *, #34427, .F. ) ;
#40086 = CARTESIAN_POINT ( 'NONE',  ( 82.75389963950320293, -45.59493862562369770, -47.67227237921210303 ) ) ;
#40087 = CARTESIAN_POINT ( 'NONE',  ( 8.575657855873597413, -13.18837314039375563, -76.60667932582364870 ) ) ;
#40088 = CARTESIAN_POINT ( 'NONE',  ( 13.39998208317153328, -51.78678246883065839, -74.34716300802820399 ) ) ;
#40089 = CARTESIAN_POINT ( 'NONE',  ( 13.49824643614018349, -8.118921815336832992, -48.89997689786164869 ) ) ;
#40090 = VERTEX_POINT ( 'NONE', #27722 ) ;
#40091 = DIRECTION ( 'NONE',  ( 1.000000000000000000, 0.000000000000000000, 0.000000000000000000 ) ) ;
#40092 = CARTESIAN_POINT ( 'NONE',  ( 57.20288283122350492, -50.17392941253179828, -52.64687565050539320 ) ) ;
#40093 = CARTESIAN_POINT ( 'NONE',  ( 49.45585557151159861, 22.20491319630109928, -54.07529678225080261 ) ) ;
#40094 = CARTESIAN_POINT ( 'NONE',  ( 13.71920826666440085, -7.732547446001079905, -69.19772247832989365 ) ) ;
#40095 = EDGE_CURVE ( 'NONE', #18259, #35705, #985, .T. ) ;
#40096 = FACE_OUTER_BOUND ( 'NONE', #27572, .T. ) ;
#40097 = CARTESIAN_POINT ( 'NONE',  ( 55.22814166963710392, 19.75351993034290032, -75.19629012753209452 ) ) ;
#40098 = APPLICATION_PROTOCOL_DEFINITION ( 'draft international standard', 'automotive_design', 1998, #30789 ) ;
#40099 = ORIENTED_EDGE ( 'NONE', *, *, #18275, .F. ) ;
#40100 = CARTESIAN_POINT ( 'NONE',  ( 23.57163437498810055, -16.04903704635959727, -64.25116097130579362 ) ) ;
#40101 = DIRECTION ( 'NONE',  ( 0.000000000000000000, -1.000000000000000000, 0.000000000000000000 ) ) ;
#40102 = CARTESIAN_POINT ( 'NONE',  ( 12.71325777259860068, -22.74941205225429997, -32.14999999999999858 ) ) ;
#40103 = CARTESIAN_POINT ( 'NONE',  ( 47.16988561617409914, 23.37564389197909875, -74.94862676396610368 ) ) ;
#40104 = DIRECTION ( 'NONE',  ( -0.000000000000000000, 0.7371541402007413257, 0.6757246285173463818 ) ) ;
#40105 = DIRECTION ( 'NONE',  ( 0.000000000000000000, 0.000000000000000000, -1.000000000000000000 ) ) ;
#40106 = VECTOR ( 'NONE', #19654, 1000.000000000000000 ) ;
#40107 = FACE_OUTER_BOUND ( 'NONE', #34914, .T. ) ;
#40108 = AXIS2_PLACEMENT_3D ( 'NONE', #34677, #30744, #2208 ) ;
#40110 = AXIS2_PLACEMENT_3D ( 'NONE', #49359, #14219, #37031 ) ;
#40109 = CARTESIAN_POINT ( 'NONE',  ( 11.99450341294459932, -22.74695377005799912, -70.17508691053730274 ) ) ;
#40111 = EDGE_CURVE ( 'NONE', #15986, #11267, #44483, .T. ) ;
#40112 = CARTESIAN_POINT ( 'NONE',  ( 54.14149310402689963, -50.61618454481969565, -76.93510071694009866 ) ) ;
#40114 = CARTESIAN_POINT ( 'NONE',  ( 40.59195266416351444, -39.62822065711511499, -83.00040738963430442 ) ) ;
#40113 = DIRECTION ( 'NONE',  ( -0.3535533905932768950, -0.6123724356957934711, 0.7071067811865469066 ) ) ;
#40116 = EDGE_CURVE ( 'NONE', #50303, #33352, #24401, .T. ) ;
#40115 = CARTESIAN_POINT ( 'NONE',  ( 63.23767253740619765, 1.267233196669050210, -68.81685389259939711 ) ) ;
#40117 = CARTESIAN_POINT ( 'NONE',  ( 61.39316702964359962, 13.94954103750900032, -46.44855131092970169 ) ) ;
#40118 = CARTESIAN_POINT ( 'NONE',  ( 8.223516320988901285, -15.61608250808600040, -78.50766849176299900 ) ) ;
#40119 = ORIENTED_EDGE ( 'NONE', *, *, #15560, .T. ) ;
#40120 = CARTESIAN_POINT ( 'NONE',  ( 52.82466438858409674, -49.66358825752709549, -48.56035088502149222 ) ) ;
#40121 = CARTESIAN_POINT ( 'NONE',  ( 57.37879763608390249, -45.44474840326299869, -26.07263843129119962 ) ) ;
#40122 = CARTESIAN_POINT ( 'NONE',  ( 22.33324507534229042, -20.60314842766364052, -66.00806682646168611 ) ) ;
#40123 = CARTESIAN_POINT ( 'NONE',  ( 56.84321736728299612, 14.68190763298639823, -26.22409755557089994 ) ) ;
#40124 = CARTESIAN_POINT ( 'NONE',  ( 9.474876936629032187, -18.95738746930799934, -77.08462780361209354 ) ) ;
#40125 = CARTESIAN_POINT ( 'NONE',  ( 50.12211818213420145, 17.38380696780440005, -76.14999999999999147 ) ) ;
#40126 = CARTESIAN_POINT ( 'NONE',  ( 52.94725091888329871, 18.37265018205049572, -48.86448475008189973 ) ) ;
#40127 = CARTESIAN_POINT ( 'NONE',  ( 71.27262092911099955, 0.8838110553206759423, -70.76364393196210756 ) ) ;
#40128 = DIRECTION ( 'NONE',  ( 0.000000000000000000, 0.000000000000000000, 1.000000000000000000 ) ) ;
#40129 = ORIENTED_EDGE ( 'NONE', *, *, #41996, .T. ) ;
#40130 = DIRECTION ( 'NONE',  ( 0.7071067811865457964, 0.000000000000000000, -0.7071067811865492381 ) ) ;
#40131 = CARTESIAN_POINT ( 'NONE',  ( 47.64370562464430492, -54.49759886933879471, -54.72342076385189813 ) ) ;
#40132 = CARTESIAN_POINT ( 'NONE',  ( -7.106986606757430103, 14.44895595925419940, -4.821389474212189441 ) ) ;
#40133 = DIRECTION ( 'NONE',  ( 1.000000000000000000, 0.000000000000000000, 0.000000000000000000 ) ) ;
#40134 = CARTESIAN_POINT ( 'NONE',  ( 59.10309207328680259, -28.11008969156920045, -15.65534454924780228 ) ) ;
#40135 = CARTESIAN_POINT ( 'NONE',  ( 71.16987874477759135, 1.383357884654609959, -60.97108096920410247 ) ) ;
#40136 = LINE ( 'NONE', #45370, #36778 ) ;
#40137 = CARTESIAN_POINT ( 'NONE',  ( 72.46078431608199821, 1.446932438105759999, -61.88285690311300158 ) ) ;
#40138 = CARTESIAN_POINT ( 'NONE',  ( 9.508341806066903601, -17.57833688292872054, -41.75489552743931654 ) ) ;
#40139 = CARTESIAN_POINT ( 'NONE',  ( 64.96229391979498757, 1.190292248953970011, -70.62687270921169613 ) ) ;
#40140 = EDGE_LOOP ( 'NONE', ( #25024, #47865 ) ) ;
#40141 = ORIENTED_EDGE ( 'NONE', *, *, #40384, .T. ) ;
#40142 = CARTESIAN_POINT ( 'NONE',  ( 23.83903348036886527, -13.54549273453152125, -55.70899880447446861 ) ) ;
#40143 = CIRCLE ( 'NONE', #25070, 1.999999999999998668 ) ;
#40144 = CARTESIAN_POINT ( 'NONE',  ( 51.17461318815491467, 0.4193470954621815738, -17.11446460828111427 ) ) ;
#40145 = EDGE_LOOP ( 'NONE', ( #8327, #43195, #15168, #20461 ) ) ;
#40146 = CARTESIAN_POINT ( 'NONE',  ( 12.89514948620979951, -65.50886967600349919, -47.53407058462189383 ) ) ;
#40147 = CARTESIAN_POINT ( 'NONE',  ( 16.23376603976204535, -8.830308542783665615, -49.95748267700136580 ) ) ;
#40148 = CIRCLE ( 'NONE', #38589, 5.461610137242767671 ) ;
#40149 = VECTOR ( 'NONE', #20806, 1000.000000000000114 ) ;
#40150 = ORIENTED_EDGE ( 'NONE', *, *, #27725, .F. ) ;
#40151 = CARTESIAN_POINT ( 'NONE',  ( -0.4123484725610440105, 14.05881538531380137, -35.12503119152799513 ) ) ;
#40152 = CIRCLE ( 'NONE', #30062, 9.999999999999998224 ) ;
#40153 = CARTESIAN_POINT ( 'NONE',  ( 53.63393739769619373, -63.11618894467929408, 16.35000000000000142 ) ) ;
#40154 = CARTESIAN_POINT ( 'NONE',  ( 22.22981637867615845, -20.73180715974339705, -65.73000105463430032 ) ) ;
#40155 = CIRCLE ( 'NONE', #25047, 1.999999999999998224 ) ;
#40156 = CARTESIAN_POINT ( 'NONE',  ( 13.15967284984390062, -7.926164857894950622, -47.17485964264369613 ) ) ;
#40157 = EDGE_CURVE ( 'NONE', #21630, #9438, #33788, .T. ) ;
#40158 = DIRECTION ( 'NONE',  ( 0.000000000000000000, 0.000000000000000000, 1.000000000000000000 ) ) ;
#40159 = AXIS2_PLACEMENT_3D ( 'NONE', #25013, #36833, #20573 ) ;
#40160 = CARTESIAN_POINT ( 'NONE',  ( 24.00939179868683482, -16.38255829204414482, -49.82319880720410055 ) ) ;
#40161 =( NAMED_UNIT ( * ) PLANE_ANGLE_UNIT ( ) SI_UNIT ( $, .RADIAN. ) );
#40162 = VERTEX_POINT ( 'NONE', #22170 ) ;
#40163 = CARTESIAN_POINT ( 'NONE',  ( 11.75958203967580040, -63.96014122186749518, -24.73059913046229852 ) ) ;
#40164 = CARTESIAN_POINT ( 'NONE',  ( 10.74321899375740053, -10.47353895711630045, -37.47516227180229720 ) ) ;
#40165 = CARTESIAN_POINT ( 'NONE',  ( 40.99540355667089386, 13.76721783747789907, -5.546227284263019364 ) ) ;
#40166 = CARTESIAN_POINT ( 'NONE',  ( 14.40490240792330034, 20.47201121247589839, -75.55956264724760274 ) ) ;
#40167 = CARTESIAN_POINT ( 'NONE',  ( 13.70487115333438588, -23.21378410962326555, -60.39054555587951967 ) ) ;
#40168 = CARTESIAN_POINT ( 'NONE',  ( 83.88693549187640031, -44.43477735121779659, -47.02124945944449763 ) ) ;
#40169 = DIRECTION ( 'NONE',  ( -0.3918900565005491998, -0.9200120562340454722, 0.000000000000000000 ) ) ;
#40170 = CARTESIAN_POINT ( 'NONE',  ( 10.44585770868170016, -9.647230060552569597, -42.76533676252499561 ) ) ;
#40171 = VERTEX_POINT ( 'NONE', #30033 ) ;
#40172 = CARTESIAN_POINT ( 'NONE',  ( 52.71556874866190157, -49.72995812607539534, -28.08384389970240136 ) ) ;
#40173 = CARTESIAN_POINT ( 'NONE',  ( 13.73505343097379949, -50.20716417821699906, -20.93075220000860170 ) ) ;
#40174 = CARTESIAN_POINT ( 'NONE',  ( 75.40827277404349616, 9.774041233901940018, -13.07349299794950070 ) ) ;
#40175 = CARTESIAN_POINT ( 'NONE',  ( 16.13393739769620083, -15.61618894467929941, -22.64999999999999858 ) ) ;
#40177 = EDGE_CURVE ( 'NONE', #51255, #25744, #2018, .T. ) ;
#40176 = CARTESIAN_POINT ( 'NONE',  ( 75.45689852989164592, 12.50467538828190328, -13.48414116180180145 ) ) ;
#40178 = CARTESIAN_POINT ( 'NONE',  ( 12.98723924884970060, -50.01451382913280241, -21.05373176175340078 ) ) ;
#40179 = VERTEX_POINT ( 'NONE', #17997 ) ;
#40180 = AXIS2_PLACEMENT_3D ( 'NONE', #7813, #18818, #30860 ) ;
#40181 = CARTESIAN_POINT ( 'NONE',  ( -5.240462745371109676, -47.41486970062130268, -5.522706056646890183 ) ) ;
#40182 = CONICAL_SURFACE ( 'NONE', #1690, 3.567506086244480734, 0.04995839572194331335 ) ;
#40183 = CARTESIAN_POINT ( 'NONE',  ( 47.32156641489019933, 23.47414238136689946, -54.76481957694370095 ) ) ;
#40185 = AXIS2_PLACEMENT_3D ( 'NONE', #48325, #11402, #40203 ) ;
#40184 = CARTESIAN_POINT ( 'NONE',  ( 17.18674513269237991, 18.38376737894684254, -83.21862149193310643 ) ) ;
#40186 = CARTESIAN_POINT ( 'NONE',  ( 63.39147977162330960, 1.370118064600909902, -62.58950125921379737 ) ) ;
#40187 = CARTESIAN_POINT ( 'NONE',  ( 68.13393739769847457, -50.70395984888145335, -72.15645085170113759 ) ) ;
#40188 = CLOSED_SHELL ( 'NONE', ( #31450, #17982, #27656, #10898, #10644, #29575, #5808, #20311, #47280, #26979, #36532, #10410, #40223, #38434, #1955, #34162, #9405, #32966, #50064, #12761, #6080, #41175, #18842, #31105, #21141, #27084, #41457, #9474, #15001, #14018, #39913, #3296, #30285, #40638, #15972, #15929, #2232, #42807, #18209, #38999, #28551, #19966, #33790, #49253, #30022, #18051, #2253, #31956, #6161, #21854, #23640, #26112, #40592, #33484, #46739, #30549, #49716, #20446, #615, #42787, #13031, #7684, #1183, #13378, #51118, #50802, #36529, #5812, #8017, #18554, #28267, #22578, #42712, #32144, #18745, #32558, #25657, #7576, #31545, #18546, #11065, #26124, #36006, #37220, #3069, #1878, #8088, #44004, #35468, #9291, #29798, #12614, #33357, #43733, #3549, #29054, #32450, #31249, #13771, #17859, #39275, #21634, #3006, #5078, #45008, #38148, #7506, #25357, #36687, #23611, #21504, #38664, #18117, #31326, #17964, #33392, #42481, #17812, #10602, #42846, #39868, #38371, #23315, #531, #46652, #39470, #50940, #50594, #35723, #13853, #26975, #13094, #48983, #24606 ) ) ;
#40189 = CARTESIAN_POINT ( 'NONE',  ( 42.68710801736580152, 12.13362923386000070, -4.456284347609099861 ) ) ;
#40190 = CARTESIAN_POINT ( 'NONE',  ( 9.366809454094768839, -15.61635577034980038, -65.45282021618999124 ) ) ;
#40191 = CARTESIAN_POINT ( 'NONE',  ( 9.366937397696199596, -15.61618894467949836, -28.45282021618999835 ) ) ;
#40192 = CARTESIAN_POINT ( 'NONE',  ( 57.69561854573869653, -47.11155889976559763, -47.75703836848589390 ) ) ;
#40193 = CARTESIAN_POINT ( 'NONE',  ( 14.06314481641416769, -7.911118301919978890, -75.20904927136304252 ) ) ;
#40194 = CARTESIAN_POINT ( 'NONE',  ( 31.58225770014201572, -28.80002732851900049, -102.2016796975550079 ) ) ;
#40195 = CARTESIAN_POINT ( 'NONE',  ( 12.89352330978772798, -8.399289503860947192, -32.14999999999999858 ) ) ;
#40196 = CARTESIAN_POINT ( 'NONE',  ( 9.543049689180366002, -17.38738376894362503, -61.36949275306091067 ) ) ;
#40197 =( BOUNDED_CURVE ( )  B_SPLINE_CURVE ( 2, ( #43427, #40263, #35557 ),
 .UNSPECIFIED., .F., .T. ) 
 B_SPLINE_CURVE_WITH_KNOTS ( ( 3, 3 ),
 ( 2.168627590050199672, 3.232274745523169734 ),
 .UNSPECIFIED. ) 
 CURVE ( )  GEOMETRIC_REPRESENTATION_ITEM ( )  RATIONAL_B_SPLINE_CURVE ( ( 1.425426480542939967, 1.425426480542939967, 1.323085463760209857 ) ) 
 REPRESENTATION_ITEM ( '' )  );
#40198 = CARTESIAN_POINT ( 'NONE',  ( 15.00545154534380110, -8.943947291303700808, -81.89948870795299740 ) ) ;
#40199 = CARTESIAN_POINT ( 'NONE',  ( 63.52910586918969216, 1.391735898526599957, -62.39330133199160144 ) ) ;
#40200 = ORIENTED_EDGE ( 'NONE', *, *, #21909, .F. ) ;
#40201 = DIRECTION ( 'NONE',  ( 0.000000000000000000, 0.000000000000000000, 1.000000000000000000 ) ) ;
#40202 = CARTESIAN_POINT ( 'NONE',  ( 10.97210468079041235, -63.46994206267282834, -23.98816728309422075 ) ) ;
#40203 = DIRECTION ( 'NONE',  ( 0.000000000000000000, 0.000000000000000000, -1.000000000000000000 ) ) ;
#40204 = CARTESIAN_POINT ( 'NONE',  ( 9.898088180596179342, -11.52557894097520119, -81.23899999999999011 ) ) ;
#40205 = EDGE_LOOP ( 'NONE', ( #12555, #38043, #31110, #23874 ) ) ;
#40206 = CARTESIAN_POINT ( 'NONE',  ( 17.91138945588609843, 20.67521890232639947, -75.71427953954510315 ) ) ;
#40207 = ORIENTED_EDGE ( 'NONE', *, *, #41775, .T. ) ;
#40208 = ORIENTED_EDGE ( 'NONE', *, *, #50470, .F. ) ;
#40209 = DIRECTION ( 'NONE',  ( 0.000000000000000000, 1.000000000000000000, 0.000000000000000000 ) ) ;
#40210 = CARTESIAN_POINT ( 'NONE',  ( 22.80170779281839799, -18.40375469871939984, -81.23899999999999011 ) ) ;
#40211 = VECTOR ( 'NONE', #18571, 1000.000000000000114 ) ;
#40212 = CARTESIAN_POINT ( 'NONE',  ( -10.98165337464593350, -35.31681881277557977, -44.31573110638452562 ) ) ;
#40213 = CARTESIAN_POINT ( 'NONE',  ( 12.59310188071810011, -21.71578262099550116, -69.51459820258429545 ) ) ;
#40214 = DIRECTION ( 'NONE',  ( 0.000000000000000000, 0.000000000000000000, 1.000000000000000000 ) ) ;
#40215 = ORIENTED_EDGE ( 'NONE', *, *, #26416, .T. ) ;
#40216 = DIRECTION ( 'NONE',  ( 0.000000000000000000, 0.000000000000000000, -1.000000000000000000 ) ) ;
#40217 = ADVANCED_FACE ( 'NONE', ( #1247 ), #13061, .T. ) ;
#40218 = CARTESIAN_POINT ( 'NONE',  ( 57.59061018188805292, -45.77595549251508800, -26.30140927225744818 ) ) ;
#40220 = ORIENTED_EDGE ( 'NONE', *, *, #46627, .F. ) ;
#40219 =( GEOMETRIC_REPRESENTATION_CONTEXT ( 3 ) GLOBAL_UNCERTAINTY_ASSIGNED_CONTEXT ( ( #16914 ) ) GLOBAL_UNIT_ASSIGNED_CONTEXT ( ( #16560, #48285, #23884 ) ) REPRESENTATION_CONTEXT ( 'NONE', 'WORKASPACE' ) );
#40221 = CIRCLE ( 'NONE', #41044, 0.4999999999999962252 ) ;
#40222 = ORIENTED_EDGE ( 'NONE', *, *, #1600, .F. ) ;
#40223 = ADVANCED_FACE ( 'NONE', ( #29014 ), #48958, .T. ) ;
#40224 = CARTESIAN_POINT ( 'NONE',  ( 0.3198662801700840053, -10.53391313386299899, -34.64999999999999858 ) ) ;
#40225 = DIRECTION ( 'NONE',  ( -1.000000000000000000, 0.000000000000000000, 0.000000000000000000 ) ) ;
#40226 = CIRCLE ( 'NONE', #25985, 1.000000000000000888 ) ;
#40227 = CARTESIAN_POINT ( 'NONE',  ( 60.70907960343409826, 14.40011400920250040, -47.54491343677150184 ) ) ;
#40228 = AXIS2_PLACEMENT_3D ( 'NONE', #40347, #40859, #4699 ) ;
#40229 = EDGE_CURVE ( 'NONE', #17827, #29784, #29528, .T. ) ;
#40230 = CARTESIAN_POINT ( 'NONE',  ( 49.27319349346669952, 14.34782011532229973, -11.42332069360450042 ) ) ;
#40231 = DIRECTION ( 'NONE',  ( -0.4872913772396108012, -0.8732394366197184787, 0.000000000000000000 ) ) ;
#40232 = CARTESIAN_POINT ( 'NONE',  ( -9.455812343875759751, 12.48625188284650100, -5.621938366128030218 ) ) ;
#40233 = CARTESIAN_POINT ( 'NONE',  ( 47.18324200477937325, 23.57489024965510183, -74.17387245455509515 ) ) ;
#40234 = CARTESIAN_POINT ( 'NONE',  ( 55.69413454653252415, 14.72513308957886480, -17.00762811886805181 ) ) ;
#40235 = CARTESIAN_POINT ( 'NONE',  ( 14.63845944065399962, -7.912274753621379553, -64.72647455768748159 ) ) ;
#40236 = ORIENTED_EDGE ( 'NONE', *, *, #10066, .F. ) ;
#40237 = CARTESIAN_POINT ( 'NONE',  ( 54.22814610077939790, 17.69588697627349916, -48.59159517877870371 ) ) ;
#40238 = CARTESIAN_POINT ( 'NONE',  ( 9.989812541601329698, -12.15320050589289913, -76.01055054980109560 ) ) ;
#40239 = CARTESIAN_POINT ( 'NONE',  ( 53.91125626133197102, -50.74963256429811764, -76.32770878461298025 ) ) ;
#40241 = EDGE_CURVE ( 'NONE', #50570, #40830, #10536, .T. ) ;
#40240 = CARTESIAN_POINT ( 'NONE',  ( 72.08436319736711084, 1.441354674475110009, -69.87293635634929956 ) ) ;
#40242 = CARTESIAN_POINT ( 'NONE',  ( 42.58018652930225301, -39.82501111426791596, -73.52906714457603243 ) ) ;
#40243 = CYLINDRICAL_SURFACE ( 'NONE', #21452, 1.999999999999998890 ) ;
#40244 = CARTESIAN_POINT ( 'NONE',  ( 46.71778720834619492, 22.48989871831510001, -75.96273541337029656 ) ) ;
#40245 = CARTESIAN_POINT ( 'NONE',  ( 48.31363620257710068, -54.24728121639749645, -55.22991850671440517 ) ) ;
#40246 = DIRECTION ( 'NONE',  ( -1.000000000000000000, 0.000000000000000000, 0.000000000000000000 ) ) ;
#40247 = CARTESIAN_POINT ( 'NONE',  ( 29.13393739769619728, 1.883811055320659955, -53.85091742636659973 ) ) ;
#40248 = DIRECTION ( 'NONE',  ( 1.000000000000000000, 0.000000000000000000, 0.000000000000000000 ) ) ;
#40249 = CARTESIAN_POINT ( 'NONE',  ( 22.46011455092658693, -20.47785052632239200, -54.00066733230272575 ) ) ;
#40250 = PRODUCT_DEFINITION_FORMATION_WITH_SPECIFIED_SOURCE ( 'ANY', '', #22363, .NOT_KNOWN. ) ;
#40251 = EDGE_LOOP ( 'NONE', ( #37111, #39042 ) ) ;
#40252 = CARTESIAN_POINT ( 'NONE',  ( 23.28731277692780210, -13.53390210943540062, -32.97717709171589462 ) ) ;
#40253 = CARTESIAN_POINT ( 'NONE',  ( 64.64959960286040541, 1.134960180547699871, -60.82204151093920075 ) ) ;
#40254 = ORIENTED_EDGE ( 'NONE', *, *, #36462, .F. ) ;
#40255 = CARTESIAN_POINT ( 'NONE',  ( 71.60339545440879760, 0.9065823421260970072, -70.54525856488079683 ) ) ;
#40256 = CARTESIAN_POINT ( 'NONE',  ( 61.10834071495050068, -45.42417164445600264, -47.35406349611150034 ) ) ;
#40257 = CARTESIAN_POINT ( 'NONE',  ( 23.63393739769620083, -15.61618894467930119, -81.65000000000000568 ) ) ;
#40258 = CARTESIAN_POINT ( 'NONE',  ( 28.63393739769619728, -26.55370255794280254, -34.64999999999999858 ) ) ;
#40260 = CARTESIAN_POINT ( 'NONE',  ( 46.85765394103209758, 21.46248514361199966, -55.14905519569659731 ) ) ;
#40259 = CARTESIAN_POINT ( 'NONE',  ( 42.21716448694958501, 8.555370896169934625, -75.28279128881918325 ) ) ;
#40261 = ADVANCED_FACE ( 'NONE', ( #21651 ), #5492, .F. ) ;
#40262 = VECTOR ( 'NONE', #5290, 1000.000000000000000 ) ;
#40263 = CARTESIAN_POINT ( 'NONE',  ( 4.133937397696232807, -18.83157925385280862, -22.14999999999998792 ) ) ;
#40264 = CARTESIAN_POINT ( 'NONE',  ( 9.221418464489284261, -19.60032756090027561, -52.34100133722100168 ) ) ;
#40265 = VERTEX_POINT ( 'NONE', #45531 ) ;
#40266 = CARTESIAN_POINT ( 'NONE',  ( 83.85375176557759858, -44.83517184343819650, -47.43402238021350570 ) ) ;
#40267 = VERTEX_POINT ( 'NONE', #49474 ) ;
#40268 = EDGE_LOOP ( 'NONE', ( #20707, #14187, #23616, #35330 ) ) ;
#40269 = B_SPLINE_CURVE_WITH_KNOTS ( 'NONE', 3,
 ( #7028, #46874, #10960, #11736, #7282, #43186, #23232, #22465, #26924, #35306, #27436, #22979, #39000, #47381, #43439, #7542, #27943, #7796, #183, #36857, #48931, #28720, #20593, #16163, #36324, #20337, #20855, #24514, #32901 ),
 .UNSPECIFIED., .F., .F.,
 ( 4, 2, 1, 1, 1, 1, 1, 2, 2, 2, 2, 2, 2, 2, 2, 2, 4 ),
 ( 0.5000036478644217519, 0.5002477867082379959, 0.5004919255520542398, 0.5009802032396866167, 0.5019567586149512595, 0.5039098693654808780, 0.5078160908665402262, 0.5156285338686588116, 0.5312534198728956492, 0.5625031918813692133, 0.6250027358983164527, 0.6875022799152636921, 0.7500018239322110425, 0.8125013679491581708, 0.8750009119661055212, 0.9375004559830526496, 1.000000000000000000 ),
 .UNSPECIFIED. ) ;
#40270 = VERTEX_POINT ( 'NONE', #2275 ) ;
#40271 = CARTESIAN_POINT ( 'NONE',  ( 61.33923903537449718, -45.29997321760770035, -47.15257578971730368 ) ) ;
#40272 = CARTESIAN_POINT ( 'NONE',  ( 20.11808686960868897, -8.703676620365614625, -79.45899972692541269 ) ) ;
#40273 = CARTESIAN_POINT ( 'NONE',  ( 76.41382631677322479, -21.54755901427089526, -12.85609321466854027 ) ) ;
#40274 = CARTESIAN_POINT ( 'NONE',  ( 49.53395860104419768, -53.61039739033260076, -54.45855173817700745 ) ) ;
#40275 = ORIENTED_EDGE ( 'NONE', *, *, #27500, .F. ) ;
#40276 = VERTEX_POINT ( 'NONE', #41078 ) ;
#40277 = CARTESIAN_POINT ( 'NONE',  ( 0.3209249304026170480, -50.71887597443840434, -35.14999999999999858 ) ) ;
#40278 = CARTESIAN_POINT ( 'NONE',  ( 57.07913431483230227, -45.16254433447520000, -25.30508418749239752 ) ) ;
#40279 = CARTESIAN_POINT ( 'NONE',  ( 9.366488261363459245, -15.61629045172390029, -39.45282021618999835 ) ) ;
#40280 = DIRECTION ( 'NONE',  ( 1.000000000000000000, 0.000000000000000000, 0.000000000000000000 ) ) ;
#40281 = CARTESIAN_POINT ( 'NONE',  ( 60.81548642094829660, -0.5902880540152319888, -16.32683701710460156 ) ) ;
#40282 = CARTESIAN_POINT ( 'NONE',  ( 43.34604152446959802, 4.883811055320659733, -58.29242082535468938 ) ) ;
#40283 = EDGE_CURVE ( 'NONE', #1290, #38545, #37149, .T. ) ;
#40284 = ORIENTED_EDGE ( 'NONE', *, *, #40807, .F. ) ;
#40285 = CARTESIAN_POINT ( 'NONE',  ( -2.927827710953269769, 17.96742650791509988, -5.740515240579870060 ) ) ;
#40286 = CARTESIAN_POINT ( 'NONE',  ( 52.71937672608480341, -50.18624820298519751, -77.16972201296600531 ) ) ;
#40287 = CARTESIAN_POINT ( 'NONE',  ( 16.70374668832650045, -8.852716093271043363, -33.97954381835977244 ) ) ;
#40288 = CARTESIAN_POINT ( 'NONE',  ( 5.741632552282960766, -9.616188944679340267, -22.14999999999999858 ) ) ;
#40289 = ADVANCED_FACE ( 'NONE', ( #1756 ), #30603, .F. ) ;
#40290 = CARTESIAN_POINT ( 'NONE',  ( 23.92893553353459879, -16.52434733056690064, -54.04941275463870198 ) ) ;
#40291 = CARTESIAN_POINT ( 'NONE',  ( 12.76011332328899961, -50.09570302368800299, -21.12207829526439795 ) ) ;
#40292 = CARTESIAN_POINT ( 'NONE',  ( -22.80083709146214233, -13.57305611580116178, -54.72264480988580715 ) ) ;
#40293 = DIRECTION ( 'NONE',  ( -1.000000000000000000, -8.402539340422011355E-12, -1.147202196707759143E-22 ) ) ;
#40294 = CARTESIAN_POINT ( 'NONE',  ( 61.28398356449380202, -45.60471458446119897, -47.68178229846480320 ) ) ;
#40295 = CARTESIAN_POINT ( 'NONE',  ( 61.40713123412509589, -45.37885581412189850, -47.36177601773500356 ) ) ;
#40296 = CARTESIAN_POINT ( 'NONE',  ( 22.52282493614631420, -13.38585152154421820, -28.45282021618999835 ) ) ;
#40297 = CARTESIAN_POINT ( 'NONE',  ( 10.17382535701520041, -11.84529732107350064, -50.02674116093399448 ) ) ;
#40298 = CARTESIAN_POINT ( 'NONE',  ( 16.13393739846020125, -15.61618894405949831, -8.049999999938441064 ) ) ;
#40299 = AXIS2_PLACEMENT_3D ( 'NONE', #46606, #3090, #39505 ) ;
#40300 = ORIENTED_EDGE ( 'NONE', *, *, #4300, .F. ) ;
#40301 = CARTESIAN_POINT ( 'NONE',  ( 13.96298243069049860, -52.23921076650779582, -75.65449215554859563 ) ) ;
#40302 = CARTESIAN_POINT ( 'NONE',  ( 47.35344256344840375, -54.67958107652259514, -54.64484088995269673 ) ) ;
#40303 = DIRECTION ( 'NONE',  ( 0.000000000000000000, 0.000000000000000000, 1.000000000000000000 ) ) ;
#40304 = CARTESIAN_POINT ( 'NONE',  ( 12.48759467940610435, 34.23991394352164264, -47.62022110713834877 ) ) ;
#40305 = CARTESIAN_POINT ( 'NONE',  ( 9.367749763036480104, -16.28101815411259068, -77.81590886694031894 ) ) ;
#40306 = DIRECTION ( 'NONE',  ( 1.000000000000000000, 0.000000000000000000, 0.000000000000000000 ) ) ;
#40307 = CYLINDRICAL_SURFACE ( 'NONE', #8852, 0.4999999999999992784 ) ;
#40309 = CARTESIAN_POINT ( 'NONE',  ( 13.06064430388411957, -50.89607785224676917, -21.55066631622714723 ) ) ;
#40308 = CARTESIAN_POINT ( 'NONE',  ( 60.83133136721959744, 14.23629320661039976, -47.01992809069390233 ) ) ;
#40310 = CARTESIAN_POINT ( 'NONE',  ( 16.13393739769620083, -15.61618894467929941, -31.39999999999999858 ) ) ;
#40311 = CARTESIAN_POINT ( 'NONE',  ( 48.57499813573529934, 22.88423463883380293, -55.03262398412059753 ) ) ;
#40312 = ORIENTED_EDGE ( 'NONE', *, *, #24530, .T. ) ;
#40313 = CARTESIAN_POINT ( 'NONE',  ( 52.71454542960869816, -49.74875623591339746, -48.77936393691420136 ) ) ;
#40315 = ORIENTED_EDGE ( 'NONE', *, *, #35532, .F. ) ;
#40314 = AXIS2_PLACEMENT_3D ( 'NONE', #14065, #17991, #29521 ) ;
#40316 = CARTESIAN_POINT ( 'NONE',  ( 18.38332337263111427, -52.17615710686938968, -75.56421430878999956 ) ) ;
#40317 = CARTESIAN_POINT ( 'NONE',  ( 16.13393739769620083, -15.61618894467929941, -4.296538310234230273 ) ) ;
#40318 = CARTESIAN_POINT ( 'NONE',  ( 56.88339342946630239, -50.64986849223689802, -53.85640383950750021 ) ) ;
#40320 = CARTESIAN_POINT ( 'NONE',  ( 56.18972689709309520, 14.75003178236420176, -26.01119383299409904 ) ) ;
#40319 = CARTESIAN_POINT ( 'NONE',  ( 84.42643369580130752, 12.06118485168240007, -47.38360074682189804 ) ) ;
#40321 = EDGE_CURVE ( 'NONE', #33500, #6443, #33196, .T. ) ;
#40322 = CARTESIAN_POINT ( 'NONE',  ( 23.17208530007939871, -15.16118037244739902, -68.43227042713769492 ) ) ;
#40323 = CARTESIAN_POINT ( 'NONE',  ( 52.59025554715780260, 18.60560742025969816, -48.57067451951849790 ) ) ;
#40324 = CARTESIAN_POINT ( 'NONE',  ( 55.28820859282659939, -45.64641271493429997, -15.90562343326089945 ) ) ;
#40325 = CARTESIAN_POINT ( 'NONE',  ( 51.13393739769659874, -50.61618894467899565, 11.34999999999999964 ) ) ;
#40326 = ADVANCED_FACE ( 'NONE', ( #45271, #49726 ), #33712, .T. ) ;
#40327 = ORIENTED_EDGE ( 'NONE', *, *, #31558, .T. ) ;
#40328 = VERTEX_POINT ( 'NONE', #41331 ) ;
#40329 = EDGE_CURVE ( 'NONE', #23421, #12905, #43840, .T. ) ;
#40330 = CARTESIAN_POINT ( 'NONE',  ( 11.84787509014739904, -65.28991114173599897, -17.04454481949920108 ) ) ;
#40331 = CARTESIAN_POINT ( 'NONE',  ( 10.67388688448640188, 32.32518983410499658, -45.41653795764540291 ) ) ;
#40332 = CARTESIAN_POINT ( 'NONE',  ( 46.13393739769619373, 4.883811055320659733, -81.65000000000000568 ) ) ;
#40333 = CIRCLE ( 'NONE', #3500, 35.00000000000000000 ) ;
#40334 = CARTESIAN_POINT ( 'NONE',  ( 47.76312238234860530, -54.35589300656749856, -54.31785946381069863 ) ) ;
#40335 = CARTESIAN_POINT ( 'NONE',  ( 10.91980184567070644, -64.71824133905012388, -23.28490012654648922 ) ) ;
#40336 = CARTESIAN_POINT ( 'NONE',  ( 8.222930619450961487, -15.61639179890759976, -64.50766849176299900 ) ) ;
#40337 = VERTEX_POINT ( 'NONE', #29657 ) ;
#40338 = CARTESIAN_POINT ( 'NONE',  ( 13.43643018811596157, 20.02091947432642627, -22.14276202162402285 ) ) ;
#40339 = CARTESIAN_POINT ( 'NONE',  ( 10.97861341538039781, -63.23619217347560806, -44.74199978104029896 ) ) ;
#40340 = CARTESIAN_POINT ( 'NONE',  ( 13.84626747563856242, 20.91301623525153985, -75.51793353176734058 ) ) ;
#40341 = ORIENTED_EDGE ( 'NONE', *, *, #19095, .T. ) ;
#40342 = CARTESIAN_POINT ( 'NONE',  ( 72.27589226135678757, 1.457833794292699992, -69.65505222163159260 ) ) ;
#40343 = CARTESIAN_POINT ( 'NONE',  ( 63.46018632244250313, 1.384447124000270035, -62.70866005236110396 ) ) ;
#40344 = EDGE_LOOP ( 'NONE', ( #20854, #1640 ) ) ;
#40345 = CARTESIAN_POINT ( 'NONE',  ( 16.13393739769620083, -15.61618894467929941, -10.44999999999999929 ) ) ;
#40346 = CARTESIAN_POINT ( 'NONE',  ( 10.12953414447999911, 22.90954413163299819, -35.04035092416999220 ) ) ;
#40347 = CARTESIAN_POINT ( 'NONE',  ( 38.67452568954060155, -37.56081407618430035, -81.65000000000000568 ) ) ;
#40348 = CARTESIAN_POINT ( 'NONE',  ( 59.71523078726419698, 15.48044394707019933, -48.67158068971760088 ) ) ;
#40349 = EDGE_CURVE ( 'NONE', #10379, #8545, #1324, .T. ) ;
#40350 = CARTESIAN_POINT ( 'NONE',  ( 15.22672021889999883, -23.81128974005859789, -76.32742627405569635 ) ) ;
#40351 = CARTESIAN_POINT ( 'NONE',  ( 9.366584228470589579, -15.61631960056659985, -37.84717978380999881 ) ) ;
#40352 = DIRECTION ( 'NONE',  ( 0.000000000000000000, 0.000000000000000000, -1.000000000000000000 ) ) ;
#40353 = CONTEXT_DEPENDENT_SHAPE_REPRESENTATION ( #27427, #45384 ) ;
#40354 = ORIENTED_EDGE ( 'NONE', *, *, #40709, .F. ) ;
#40355 = CARTESIAN_POINT ( 'NONE',  ( 8.852402460927230265, -14.03950166758260032, -63.30053379854238926 ) ) ;
#40356 = CARTESIAN_POINT ( 'NONE',  ( 18.13393739769599833, 14.38381105532070059, -62.64999999999999858 ) ) ;
#40357 = CARTESIAN_POINT ( 'NONE',  ( 12.03469375213867032, 33.98406662134181744, -23.73059634278166996 ) ) ;
#40358 = CARTESIAN_POINT ( 'NONE',  ( 47.23197633308699750, 23.50398264039059981, -74.50254677461771280 ) ) ;
#40359 = CARTESIAN_POINT ( 'NONE',  ( 71.31427394968270050, 1.395196698723390138, -61.05633982442969909 ) ) ;
#40360 = CARTESIAN_POINT ( 'NONE',  ( 22.90099491887654182, -15.61618908163285546, -52.84717737022585027 ) ) ;
#40361 = AXIS2_PLACEMENT_3D ( 'NONE', #44977, #48657, #16946 ) ;
#40362 = CIRCLE ( 'NONE', #13630, 2.999999999999999112 ) ;
#40363 = CARTESIAN_POINT ( 'NONE',  ( -21.36606260230379917, 31.59091783650714547, 11.14289321881345174 ) ) ;
#40364 = CARTESIAN_POINT ( 'NONE',  ( 8.951113142255618271, -11.56776253131459953, -76.67103925775408868 ) ) ;
#40365 = CARTESIAN_POINT ( 'NONE',  ( 56.34559392600819905, -50.61618894589719986, -75.80272952737600178 ) ) ;
#40367 = CARTESIAN_POINT ( 'NONE',  ( 43.57203457279818082, -40.01153835713891027, -68.34812681792193700 ) ) ;
#40366 = FACE_OUTER_BOUND ( 'NONE', #40900, .T. ) ;
#40368 = CARTESIAN_POINT ( 'NONE',  ( 63.29300171101180439, 1.330484379554840002, -68.72860478453370092 ) ) ;
#40369 = CARTESIAN_POINT ( 'NONE',  ( 61.17186926503560329, 14.07231709399069963, -46.96206214597430062 ) ) ;
#40370 = CARTESIAN_POINT ( 'NONE',  ( -17.64362745039570157, -51.14126898808360266, -52.54414402675330109 ) ) ;
#40371 = ORIENTED_EDGE ( 'NONE', *, *, #46563, .F. ) ;
#40372 = CARTESIAN_POINT ( 'NONE',  ( 52.83359533572390632, -49.65890908409249960, -48.59873101611960067 ) ) ;
#40373 = CARTESIAN_POINT ( 'NONE',  ( 61.35829355718019684, -45.19500725088990123, -28.15102488364330213 ) ) ;
#40374 = CARTESIAN_POINT ( 'NONE',  ( 68.13393739769618662, -30.31618894467939995, -51.14999999999999858 ) ) ;
#40375 = CARTESIAN_POINT ( 'NONE',  ( 13.09773361826850113, 19.68112921523509939, -21.58185394810089974 ) ) ;
#40376 = CARTESIAN_POINT ( 'NONE',  ( 56.39899885288320291, 14.62458411682690063, -26.05220366909510332 ) ) ;
#40377 = CARTESIAN_POINT ( 'NONE',  ( 10.88488332746739928, -20.32681417541479973, -37.22001158807169929 ) ) ;
#40378 = CARTESIAN_POINT ( 'NONE',  ( 51.61772101699799720, 19.12659659585209937, -76.35065455175050886 ) ) ;
#40379 = B_SPLINE_SURFACE_WITH_KNOTS ( 'NONE', 3, 3, ( 
 ( #30593, #41368, #18552, #42417, #14105, #34528, #13600, #22469, #46614, #37961, #50281, #9915, #22209, #26142 ),
 ( #5483, #21440, #42153, #6252, #2314, #49762, #46097, #21949, #37439, #2578, #5989, #38218, #2058, #6509 ),
 ( #14367, #29811, #45828, #25878, #30335, #38478, #33496, #41892, #46357, #1540, #10444, #49509, #45569, #18036 ),
 ( #5731, #26397, #9662, #25621, #41624, #21691, #37697, #10182, #1794, #17777, #33747, #50015, #30072, #10964 ),
 ( #35310, #19330, #19839, #23490, #31873, #43697, #26656, #11740, #15147, #27440, #51311, #31106, #3101, #15406 ),
 ( #31359, #42678, #11483, #7801, #47387, #11221, #43443, #35829, #26928, #35576, #46877, #42934, #27184, #7546 ),
 ( #39514, #27699, #3614, #7033, #22983, #47134, #19586, #51561, #51813, #15662, #47891, #23751, #6774, #39767 ),
 ( #31615, #47633, #43191, #19067, #3869, #15919, #22725, #38748, #2841, #18807, #34786, #7286, #50793, #14881 ),
 ( #30846, #39005, #35041, #23236, #51050, #39253, #3356, #4627, #962, #4893, #24004, #36082, #48402, #12243 ),
 ( #11994, #187, #8055, #27949, #43953, #40281, #20091, #40024, #16167, #32907, #8573, #48667, #4114, #32382 ) ),
 .UNSPECIFIED., .F., .F., .F.,
 ( 4, 1, 1, 1, 1, 1, 1, 4 ),
 ( 4, 2, 2, 2, 2, 2, 4 ),
 ( -0.001601301838199999930, 0.1428571428571430157, 0.2857142857142860315, 0.4285714285714289917, 0.5714285714285709528, 0.7142857142857139685, 0.8571428571428569843, 1.000147433196030056 ),
 ( -0.001601301838199999930, 0.2220862982459869961, 0.4758992105271160344, 0.6345322807028209722, 0.7138488157906729414, 0.8407552719312380018, 0.9741502278125520053 ),
 .UNSPECIFIED. ) ;
#40380 = CARTESIAN_POINT ( 'NONE',  ( 53.46953806481329963, 18.11317590511340114, -48.93764703831700302 ) ) ;
#40381 = CARTESIAN_POINT ( 'NONE',  ( 71.15687762518609816, 1.370937308141420230, -70.40667188452539449 ) ) ;
#40382 = CARTESIAN_POINT ( 'NONE',  ( 16.13393739846020125, -15.61618894405949831, -8.049999999938441064 ) ) ;
#40383 = CARTESIAN_POINT ( 'NONE',  ( 20.63393739769620083, -41.61618894467930119, -35.14999999999999858 ) ) ;
#40384 = EDGE_CURVE ( 'NONE', #34827, #45182, #12560, .T. ) ;
#40385 = ORIENTED_EDGE ( 'NONE', *, *, #25195, .T. ) ;
#40386 = DIRECTION ( 'NONE',  ( 0.000000000000000000, 1.000000000000000000, 0.000000000000000000 ) ) ;
#40387 = EDGE_CURVE ( 'NONE', #3494, #33030, #8012, .T. ) ;
#40388 = CARTESIAN_POINT ( 'NONE',  ( 47.69553636805479613, -54.48351236463479808, -54.81782713205149804 ) ) ;
#40389 = CARTESIAN_POINT ( 'NONE',  ( 83.89200044194980421, 18.85811933572209753, -52.57651812407429759 ) ) ;
#40390 = CARTESIAN_POINT ( 'NONE',  ( 10.22105613155544113, -19.02423196159752905, -71.28615407210328669 ) ) ;
#40391 = CARTESIAN_POINT ( 'NONE',  ( 61.09078957334159554, 14.31200446843280005, -47.59852323931760054 ) ) ;
#40392 = CARTESIAN_POINT ( 'NONE',  ( 71.47398825900590680, 0.9272522097098119254, -60.66559564092809609 ) ) ;
#40393 = CARTESIAN_POINT ( 'NONE',  ( 62.09157612670949788, 1.883811055320649963, -65.34607522167520699 ) ) ;
#40394 = CARTESIAN_POINT ( 'NONE',  ( 71.77737262410839492, 1.421976796946140098, -61.21910751912620441 ) ) ;
#40395 = CYLINDRICAL_SURFACE ( 'NONE', #15122, 0.4999999999999982236 ) ;
#40396 = CARTESIAN_POINT ( 'NONE',  ( 65.07261215712630076, 1.274277262446069869, -70.59881390902160092 ) ) ;
#40397 = ORIENTED_EDGE ( 'NONE', *, *, #42419, .T. ) ;
#40398 = ORIENTED_EDGE ( 'NONE', *, *, #22678, .T. ) ;
#40399 = PLANE ( 'NONE',  #7828 ) ;
#40400 = CYLINDRICAL_SURFACE ( 'NONE', #18521, 7.910999999999997812 ) ;
#40401 = EDGE_LOOP ( 'NONE', ( #43737, #29041, #20619, #34774 ) ) ;
#40402 = DIRECTION ( 'NONE',  ( 0.6339889056055382222, 0.000000000000000000, -0.7733421413379021336 ) ) ;
#40403 = LINE ( 'NONE', #44594, #2639 ) ;
#40404 = FACE_OUTER_BOUND ( 'NONE', #22883, .T. ) ;
#40405 = EDGE_LOOP ( 'NONE', ( #10709, #2904, #18053, #36075, #33154 ) ) ;
#40406 = CIRCLE ( 'NONE', #263, 0.4999999999999982236 ) ;
#40407 = CARTESIAN_POINT ( 'NONE',  ( 31.13393739769620083, -33.99486860111965569, -83.77132034355965118 ) ) ;
#40408 = CARTESIAN_POINT ( 'NONE',  ( 42.31307469794116116, 6.441183479073752771, -78.75431333624337071 ) ) ;
#40409 = DIRECTION ( 'NONE',  ( 1.000000000000000000, 0.000000000000000000, 0.000000000000000000 ) ) ;
#40410 = EDGE_CURVE ( 'NONE', #33105, #23557, #18045, .T. ) ;
#40411 = CARTESIAN_POINT ( 'NONE',  ( 23.57040948703929928, -12.05506511639750045, -47.65017322902539831 ) ) ;
#40412 = CARTESIAN_POINT ( 'NONE',  ( -0.4410626023037830246, -8.356009309619699010, -35.14999999999999858 ) ) ;
#40413 = CARTESIAN_POINT ( 'NONE',  ( 41.79059739480540259, -37.58975971051863496, -81.36666986503341548 ) ) ;
#40414 = ADVANCED_FACE ( 'NONE', ( #14724 ), #32223, .T. ) ;
#40415 = ORIENTED_EDGE ( 'NONE', *, *, #22572, .T. ) ;
#40416 = CARTESIAN_POINT ( 'NONE',  ( 12.27549348550230057, -65.46856705471530802, -22.61746666998769939 ) ) ;
#40417 = CARTESIAN_POINT ( 'NONE',  ( 9.758604362744099703, -19.47129238020390218, -39.05954089307470412 ) ) ;
#40418 = DIRECTION ( 'NONE',  ( -0.05023550054956202326, 0.000000000000000000, 0.9987374001630934250 ) ) ;
#40419 = CARTESIAN_POINT ( 'NONE',  ( 14.52015376228360033, 20.37930389448659696, -75.46937177410659103 ) ) ;
#40420 = DIRECTION ( 'NONE',  ( 0.000000000000000000, 1.000000000000000000, 0.000000000000000000 ) ) ;
#40421 = CARTESIAN_POINT ( 'NONE',  ( 83.84636189228659475, -44.33791279555990172, -46.70679156566489354 ) ) ;
#40422 = CARTESIAN_POINT ( 'NONE',  ( 68.13393739824141448, -1.666188944678682837, -82.14999999999919567 ) ) ;
#40423 = CARTESIAN_POINT ( 'NONE',  ( 8.457331809849481630, -18.62491747308059686, -40.38876883061629997 ) ) ;
#40424 = ORIENTED_EDGE ( 'NONE', *, *, #25718, .F. ) ;
#40425 = CARTESIAN_POINT ( 'NONE',  ( 52.71556874866190157, -49.72995812607539534, -28.15000000000000213 ) ) ;
#40426 = CARTESIAN_POINT ( 'NONE',  ( 15.22027405774909958, -50.86891089868439764, -20.91173439138849943 ) ) ;
#40427 = CARTESIAN_POINT ( 'NONE',  ( 50.07689680525066223, -36.77944211564444288, -76.14999999999999147 ) ) ;
#40428 = DIRECTION ( 'NONE',  ( -1.000000000000000000, 0.000000000000000000, 0.000000000000000000 ) ) ;
#40429 = CARTESIAN_POINT ( 'NONE',  ( 22.90078880164185549, -15.66462774376105926, -56.45510315590827588 ) ) ;
#40430 = AXIS2_PLACEMENT_3D ( 'NONE', #8476, #40435, #20246 ) ;
#40431 = ORIENTED_EDGE ( 'NONE', *, *, #4594, .T. ) ;
#40432 = CARTESIAN_POINT ( 'NONE',  ( -4.138844267738590155, -48.25635689139589601, -5.557732677314410452 ) ) ;
#40433 = AXIS2_PLACEMENT_3D ( 'NONE', #49143, #28668, #29703 ) ;
#40434 = CARTESIAN_POINT ( 'NONE',  ( 47.20960036188380116, 23.55400766168000004, -54.63720401602729737 ) ) ;
#40435 = DIRECTION ( 'NONE',  ( 0.000000000000000000, -1.000000000000000000, 0.000000000000000000 ) ) ;
#40436 = CARTESIAN_POINT ( 'NONE',  ( 63.42952807919409253, 1.382830464309369844, -62.68920552647019662 ) ) ;
#40437 = CARTESIAN_POINT ( 'NONE',  ( 13.18314425874230089, 19.09886800652760286, -21.16865821970199946 ) ) ;
#40438 = CARTESIAN_POINT ( 'NONE',  ( 56.49020273170298623, 15.04445699649443569, -26.27688945974474422 ) ) ;
#40439 = CARTESIAN_POINT ( 'NONE',  ( 41.53965881163059493, 12.99627826066740077, -4.633657234686240578 ) ) ;
#40440 = DIRECTION ( 'NONE',  ( 0.000000000000000000, -1.000000000000000000, 0.000000000000000000 ) ) ;
#40441 = CARTESIAN_POINT ( 'NONE',  ( 11.97539491867874162, -21.02760647153319695, -65.16115419653750962 ) ) ;
#40442 = CARTESIAN_POINT ( 'NONE',  ( 20.13393739768959634, -55.41568642894479524, -74.14999999999999147 ) ) ;
#40443 = CARTESIAN_POINT ( 'NONE',  ( 57.22384866945419901, -47.50201179472099966, -48.27676837875709737 ) ) ;
#40444 = CARTESIAN_POINT ( 'NONE',  ( 24.04215757223157723, -15.38968104315445196, -75.78321347473215042 ) ) ;
#40445 = ADVANCED_FACE ( 'NONE', ( #19675 ), #27795, .T. ) ;
#40446 = CARTESIAN_POINT ( 'NONE',  ( 64.72741779930979078, 0.8986939045430379913, -60.71074964625670134 ) ) ;
#40447 = CARTESIAN_POINT ( 'NONE',  ( 17.69762321645020009, -52.06302405750739837, -75.84958893011570069 ) ) ;
#40448 = CARTESIAN_POINT ( 'NONE',  ( 21.54527544888350121, -19.77483684844828815, -60.66116240694285722 ) ) ;
#40449 = CARTESIAN_POINT ( 'NONE',  ( 51.04010994513039634, 13.88381105532070059, -11.02192607461959994 ) ) ;
#40450 = VERTEX_POINT ( 'NONE', #27025 ) ;
#40451 = CYLINDRICAL_SURFACE ( 'NONE', #23720, 0.4999999999999982236 ) ;
#40452 = CARTESIAN_POINT ( 'NONE',  ( 10.14595732507179981, 32.05463481625440636, -45.99315448786889959 ) ) ;
#40453 = CARTESIAN_POINT ( 'NONE',  ( 42.75215489670460300, 13.74995302045830137, -6.093637046069630081 ) ) ;
#40454 = CARTESIAN_POINT ( 'NONE',  ( 67.33934068966290454, -30.19343665506969998, -17.45359291235359933 ) ) ;
#40455 = EDGE_LOOP ( 'NONE', ( #41131, #24184, #48073, #1997, #14375 ) ) ;
#40456 = CARTESIAN_POINT ( 'NONE',  ( 18.24473874235309978, 20.10118929730710136, -74.92517623884199907 ) ) ;
#40457 = ORIENTED_EDGE ( 'NONE', *, *, #1370, .F. ) ;
#40458 = ORIENTED_EDGE ( 'NONE', *, *, #34724, .F. ) ;
#40459 = AXIS2_PLACEMENT_3D ( 'NONE', #19626, #12036, #15699 ) ;
#40460 = ORIENTED_EDGE ( 'NONE', *, *, #48823, .T. ) ;
#40461 = CARTESIAN_POINT ( 'NONE',  ( 57.40532849796809245, -45.80460617788560285, -26.27934586546770035 ) ) ;
#40463 = CARTESIAN_POINT ( 'NONE',  ( 22.65849246206020240, -18.66984389996769877, -81.23899999999999011 ) ) ;
#40462 = AXIS2_PLACEMENT_3D ( 'NONE', #37522, #49599, #16564 ) ;
#40464 = FACE_OUTER_BOUND ( 'NONE', #27259, .T. ) ;
#40465 = ORIENTED_EDGE ( 'NONE', *, *, #29192, .F. ) ;
#40466 = CARTESIAN_POINT ( 'NONE',  ( 75.27759724181119338, 4.400931120799945973, -12.42500406430217907 ) ) ;
#40467 = CARTESIAN_POINT ( 'NONE',  ( 11.13393739769619906, -15.61618894467929941, -46.14999999999999858 ) ) ;
#40468 = ORIENTED_EDGE ( 'NONE', *, *, #25652, .F. ) ;
#40469 = CARTESIAN_POINT ( 'NONE',  ( 54.47259998646330104, -46.25234364376770202, -15.76423879730199928 ) ) ;
#40470 = CONICAL_SURFACE ( 'NONE', #30511, 1.079032500000000727, 0.7853981633974476129 ) ;
#40471 = EDGE_CURVE ( 'NONE', #18008, #35377, #12181, .T. ) ;
#40472 = DIRECTION ( 'NONE',  ( -0.05643417272666771678, 0.04100182651872444350, -0.9975640502598241977 ) ) ;
#40473 = VERTEX_POINT ( 'NONE', #23586 ) ;
#40474 = AXIS2_PLACEMENT_3D ( 'NONE', #6485, #22443, #42651 ) ;
#40475 = ORIENTED_EDGE ( 'NONE', *, *, #39796, .T. ) ;
#40476 = CARTESIAN_POINT ( 'NONE',  ( 69.89373504110858448, 1.883811054953212993, -20.65000000000000924 ) ) ;
#40478 = CARTESIAN_POINT ( 'NONE',  ( 12.06284766121009966, 32.21085600226960111, -46.39999999999999858 ) ) ;
#40477 = CONICAL_SURFACE ( 'NONE', #32897, 0.7350000000000003197, 0.06981317007977388966 ) ;
#40479 = CARTESIAN_POINT ( 'NONE',  ( 74.93466528652979264, 13.88381105527180104, -15.31219498128760037 ) ) ;
#40480 = CARTESIAN_POINT ( 'NONE',  ( 47.38130800000779885, 14.91675872927610058, -10.59906833146859917 ) ) ;
#40481 = LINE ( 'NONE', #44675, #8311 ) ;
#40482 = CARTESIAN_POINT ( 'NONE',  ( -10.43962737580419819, 11.55570939729970092, -6.045128938053459855 ) ) ;
#40483 = LINE ( 'NONE', #24988, #3698 ) ;
#40484 = CARTESIAN_POINT ( 'NONE',  ( 61.07580650143209766, 14.01630602148660110, -27.53710762590180039 ) ) ;
#40485 = CARTESIAN_POINT ( 'NONE',  ( 10.75986719944589964, -9.897262674175308916, -58.54739793472509746 ) ) ;
#40486 = ORIENTED_EDGE ( 'NONE', *, *, #37070, .T. ) ;
#40487 = CARTESIAN_POINT ( 'NONE',  ( 60.03117800382469227, 14.75234466156519986, -47.69329595932870092 ) ) ;
#40488 = VECTOR ( 'NONE', #22624, 1000.000000000000114 ) ;
#40489 = CARTESIAN_POINT ( 'NONE',  ( 23.48034592329200265, -49.03431820457670653, -34.71551406240359938 ) ) ;
#40490 = CARTESIAN_POINT ( 'NONE',  ( 54.14338603149285234, -50.61618765074635462, -76.93434640323403073 ) ) ;
#40491 = CARTESIAN_POINT ( 'NONE',  ( 72.22985692015490145, 1.197080272271600077, -69.99851329395420407 ) ) ;
#40492 = CARTESIAN_POINT ( 'NONE',  ( 42.89310467332932575, -39.85583253097592404, -72.01652229824608753 ) ) ;
#40493 = PLANE ( 'NONE',  #37368 ) ;
#40494 = CARTESIAN_POINT ( 'NONE',  ( 12.38542484659079967, 18.88631011504679691, -21.15108199309460346 ) ) ;
#40495 = B_SPLINE_CURVE_WITH_KNOTS ( 'NONE', 3,
 ( #6087, #50371, #22560, #50620, #2669, #14201, #10274, #37795, #41715, #10794, #38054, #26754, #33839, #22302, #38576, #49604, #38838, #42768, #18642, #49852, #2147, #17620, #13944, #13691, #33588, #29650, #14716, #50103, #18380, #46710, #30171, #18127, #14456, #2395, #5824, #25972 ),
 .UNSPECIFIED., .F., .F.,
 ( 4, 2, 2, 2, 2, 2, 2, 2, 2, 2, 2, 2, 2, 1, 1, 1, 1, 1, 1, 2, 4 ),
 ( 0.000000000000000000, 0.06250075854269371289, 0.1250015170853874258, 0.1875022756280811387, 0.2500030341707748516, 0.3125037927134685645, 0.3437541719848153932, 0.3750045512561622774, 0.4062549305275091616, 0.4375053097988559903, 0.4687556890702028745, 0.4843808787058762610, 0.4921934735237130099, 0.4960997709326313565, 0.4980529196370905298, 0.4990294939893200610, 0.4995177811654347710, 0.4997619247534921261, 0.4998839965475208036, 0.4999450324445350868, 0.5000060683415493701 ),
 .UNSPECIFIED. ) ;
#40496 = CARTESIAN_POINT ( 'NONE',  ( 47.11356394356230481, 23.41745045323149910, -74.95177818529600700 ) ) ;
#40497 = CARTESIAN_POINT ( 'NONE',  ( 48.93508874961730015, -53.77152385436419735, -54.40024034726540236 ) ) ;
#40498 = CARTESIAN_POINT ( 'NONE',  ( 64.93393739769619799, 1.883811055320669947, -61.44999999999999574 ) ) ;
#40499 = EDGE_CURVE ( 'NONE', #18289, #39898, #48859, .T. ) ;
#40500 = CARTESIAN_POINT ( 'NONE',  ( 24.02064451092653741, -16.24823765856366009, -33.53311993805902347 ) ) ;
#40501 = DIRECTION ( 'NONE',  ( 0.000000000000000000, 0.000000000000000000, 1.000000000000000000 ) ) ;
#40502 = CARTESIAN_POINT ( 'NONE',  ( 17.16953199081255477, -23.52718221652492403, -54.25066654575565650 ) ) ;
#40503 = ORIENTED_EDGE ( 'NONE', *, *, #38637, .F. ) ;
#40504 = EDGE_CURVE ( 'NONE', #14841, #19647, #28221, .T. ) ;
#40505 = AXIS2_PLACEMENT_3D ( 'NONE', #5764, #6808, #37735 ) ;
#40506 = CARTESIAN_POINT ( 'NONE',  ( 17.86279105191340122, -8.369275161513289873, -42.64188668147749439 ) ) ;
#40507 = EDGE_CURVE ( 'NONE', #49314, #41906, #23197, .T. ) ;
#40508 = CARTESIAN_POINT ( 'NONE',  ( 64.88669131378958355, 1.400446703426900141, -61.07889042780649902 ) ) ;
#40509 = ORIENTED_EDGE ( 'NONE', *, *, #43889, .T. ) ;
#40510 = DIRECTION ( 'NONE',  ( 0.000000000000000000, 0.000000000000000000, -1.000000000000000000 ) ) ;
#40511 = CARTESIAN_POINT ( 'NONE',  ( 60.60295391979060042, -45.60334326694930240, -47.31465422358670025 ) ) ;
#40512 = CARTESIAN_POINT ( 'NONE',  ( 8.332397351126385132, -14.10177087609484303, -80.85327594137434915 ) ) ;
#40513 = CARTESIAN_POINT ( 'NONE',  ( 12.76110940284849882, 18.75367529502860009, -21.08964676157749807 ) ) ;
#40515 = CARTESIAN_POINT ( 'NONE',  ( 17.16945347175581560, -23.52719342952614312, -78.25066314212283203 ) ) ;
#40514 = CARTESIAN_POINT ( 'NONE',  ( 41.50304611168537150, 8.476976521895192462, -78.72953053759411546 ) ) ;
#40516 = EDGE_CURVE ( 'NONE', #32428, #13650, #2148, .T. ) ;
#40517 = DIRECTION ( 'NONE',  ( 0.000000000000000000, 0.7071067811865475727, 0.7071067811865475727 ) ) ;
#40518 = ORIENTED_EDGE ( 'NONE', *, *, #11891, .F. ) ;
#40519 = CARTESIAN_POINT ( 'NONE',  ( 82.89855244518309974, -45.51886959512750508, -47.58879117305969686 ) ) ;
#40520 = ORIENTED_EDGE ( 'NONE', *, *, #13223, .T. ) ;
#40521 = ORIENTED_EDGE ( 'NONE', *, *, #45729, .F. ) ;
#40522 = ORIENTED_EDGE ( 'NONE', *, *, #11312, .F. ) ;
#40523 = CARTESIAN_POINT ( 'NONE',  ( 61.62921802303379337, -45.24296170225480296, -47.09041573235759870 ) ) ;
#40524 = CARTESIAN_POINT ( 'NONE',  ( 53.16310686614889391, -49.55825684149800026, -49.15478280794970090 ) ) ;
#40525 = CARTESIAN_POINT ( 'NONE',  ( 24.04513741079867017, -15.61618875311435417, -79.79232954107749265 ) ) ;
#40526 = CARTESIAN_POINT ( 'NONE',  ( 76.44629721152865898, -6.610254442245663498, -12.99600492729799939 ) ) ;
#40527 = CARTESIAN_POINT ( 'NONE',  ( 52.78795861510499776, -52.32134061137240622, -54.06277347879859718 ) ) ;
#40528 = VERTEX_POINT ( 'NONE', #3192 ) ;
#40529 = EDGE_LOOP ( 'NONE', ( #51626, #18191 ) ) ;
#40530 = CARTESIAN_POINT ( 'NONE',  ( 48.25395546892340093, 22.92590509088350004, -54.66662523256869832 ) ) ;
#40531 = CARTESIAN_POINT ( 'NONE',  ( -15.34479443485247074, 7.407496050971681179, -48.42068391671703154 ) ) ;
#40532 = CARTESIAN_POINT ( 'NONE',  ( 19.47520249253551583, -9.405029089961901789, -66.50427882218234288 ) ) ;
#40533 = CIRCLE ( 'NONE', #20422, 22.00000000000000000 ) ;
#40534 = CARTESIAN_POINT ( 'NONE',  ( 8.800117217589539464, -63.19572640051600132, -46.67015592357310538 ) ) ;
#40535 = CARTESIAN_POINT ( 'NONE',  ( 8.222476383702659319, -15.61632876086509825, -54.50766849176299900 ) ) ;
#40536 = EDGE_CURVE ( 'NONE', #362, #26902, #6343, .T. ) ;
#40537 = DIRECTION ( 'NONE',  ( 0.000000000000000000, 0.000000000000000000, -1.000000000000000000 ) ) ;
#40538 = ORIENTED_EDGE ( 'NONE', *, *, #42112, .F. ) ;
#40539 = DIRECTION ( 'NONE',  ( 0.000000000000000000, 0.000000000000000000, -1.000000000000000000 ) ) ;
#40540 = CARTESIAN_POINT ( 'NONE',  ( 53.18839701416040100, -50.49756234138030209, -76.93089027597029883 ) ) ;
#40541 = CARTESIAN_POINT ( 'NONE',  ( 22.32406200693392506, -12.82697318663033137, -34.31802238708871045 ) ) ;
#40542 = CARTESIAN_POINT ( 'NONE',  ( 82.91593256429321457, -45.56280716946599085, -47.63721988159374376 ) ) ;
#40543 = CARTESIAN_POINT ( 'NONE',  ( 9.633650982238179949, -20.01312243389589796, -64.82318737929099939 ) ) ;
#40544 = CARTESIAN_POINT ( 'NONE',  ( -0.2865249686165656784, -3.826429500511919102, -35.01561944896762668 ) ) ;
#40545 = CARTESIAN_POINT ( 'NONE',  ( 54.35139833030309831, 19.38381105532069881, -76.94248449261100120 ) ) ;
#40546 = AXIS2_PLACEMENT_3D ( 'NONE', #41726, #37280, #21020 ) ;
#40547 = CARTESIAN_POINT ( 'NONE',  ( 43.19833518102579717, -43.80395068146980719, -5.006617643003630214 ) ) ;
#40548 = CARTESIAN_POINT ( 'NONE',  ( 18.86789271272390067, -51.78678247029300508, -15.81497036395479761 ) ) ;
#40549 = FACE_OUTER_BOUND ( 'NONE', #49125, .T. ) ;
#40550 = CARTESIAN_POINT ( 'NONE',  ( 9.366455112259469473, -15.61627688590920116, -55.45282021618999835 ) ) ;
#40551 = ADVANCED_FACE ( 'NONE', ( #19165 ), #50886, .T. ) ;
#40552 = CARTESIAN_POINT ( 'NONE',  ( 64.12576500581000971, 1.345243900246989810, -69.96281373730460018 ) ) ;
#40553 = CARTESIAN_POINT ( 'NONE',  ( 53.63393739769619373, -53.11618894467930119, 16.35000000000000142 ) ) ;
#40554 = ORIENTED_EDGE ( 'NONE', *, *, #41269, .T. ) ;
#40555 = CARTESIAN_POINT ( 'NONE',  ( 14.04826348280290027, -52.14694418483630045, -75.69083100613939052 ) ) ;
#40556 = CARTESIAN_POINT ( 'NONE',  ( 47.41638517356940241, -54.63912780781220135, -54.68870541073049907 ) ) ;
#40557 = CARTESIAN_POINT ( 'NONE',  ( 9.221415312945399734, -11.63205571590753529, -36.67433565377826454 ) ) ;
#40558 = DIRECTION ( 'NONE',  ( 0.000000000000000000, -1.000000000000000000, 0.000000000000000000 ) ) ;
#40559 = CARTESIAN_POINT ( 'NONE',  ( 23.76555765687864863, -13.48533909360518201, -55.42104307077845959 ) ) ;
#40560 = CARTESIAN_POINT ( 'NONE',  ( 23.14726890598120335, -14.09743467301990094, -32.14999999999999858 ) ) ;
#40561 = CARTESIAN_POINT ( 'NONE',  ( -0.007164427059776000244, -20.74946784552680157, -34.77269723891829756 ) ) ;
#40562 = AXIS2_PLACEMENT_3D ( 'NONE', #48410, #12512, #28478 ) ;
#40564 = CARTESIAN_POINT ( 'NONE',  ( 15.09841886250152321, -23.52719244016399713, -52.33399699069794053 ) ) ;
#40563 = DIRECTION ( 'NONE',  ( 1.000000000000000000, 0.000000000000000000, 0.000000000000000000 ) ) ;
#40565 = CARTESIAN_POINT ( 'NONE',  ( 24.04464518807997919, -15.61618401921712618, -71.50767245506341396 ) ) ;
#40566 = CARTESIAN_POINT ( 'NONE',  ( 48.83374951863850555, 22.78418287378880080, -55.08837257690210265 ) ) ;
#40567 = ORIENTED_EDGE ( 'NONE', *, *, #51867, .F. ) ;
#40568 = CARTESIAN_POINT ( 'NONE',  ( 19.47520249252229618, -9.405029089986481239, -66.50427882216689568 ) ) ;
#40569 = EDGE_LOOP ( 'NONE', ( #1925, #6072, #47268, #32163 ) ) ;
#40570 = FACE_OUTER_BOUND ( 'NONE', #21733, .T. ) ;
#40571 = LINE ( 'NONE', #33473, #11014 ) ;
#40572 = CARTESIAN_POINT ( 'NONE',  ( 56.99190259421959581, -50.63247588149960166, -53.87165542791530726 ) ) ;
#40574 = CARTESIAN_POINT ( 'NONE',  ( 54.30663165020069982, 16.75924678417570135, -26.35036544773539902 ) ) ;
#40573 = CARTESIAN_POINT ( 'NONE',  ( 83.75509190357360012, 13.34125973800720111, -46.98971415009500419 ) ) ;
#40575 = CARTESIAN_POINT ( 'NONE',  ( 9.250578338074079809, -17.15304507097850006, -69.38289759990119876 ) ) ;
#40577 = EDGE_CURVE ( 'NONE', #6332, #34997, #11363, .T. ) ;
#40576 = CARTESIAN_POINT ( 'NONE',  ( 52.56521993351460509, 18.62941884369810097, -48.47378032971769812 ) ) ;
#40578 = CARTESIAN_POINT ( 'NONE',  ( 56.62787340350230636, -45.26860272202350188, -17.10917261918480037 ) ) ;
#40579 = CARTESIAN_POINT ( 'NONE',  ( 20.99565895510886193, -21.94231944923553712, -80.08399982392677430 ) ) ;
#40580 = VERTEX_POINT ( 'NONE', #28557 ) ;
#40581 = ORIENTED_EDGE ( 'NONE', *, *, #25494, .F. ) ;
#40582 = CARTESIAN_POINT ( 'NONE',  ( 11.57222021527059930, -65.08436554735389734, -16.73996640653249912 ) ) ;
#40583 = CARTESIAN_POINT ( 'NONE',  ( 13.00893739769619906, 34.28605925116850273, -47.75434321273180416 ) ) ;
#40584 = CARTESIAN_POINT ( 'NONE',  ( 61.44122352006623800, -45.34727173273595469, -47.30181503080611094 ) ) ;
#40585 = DIRECTION ( 'NONE',  ( 0.000000000000000000, -1.000000000000000000, 0.000000000000000000 ) ) ;
#40586 = CARTESIAN_POINT ( 'NONE',  ( 68.13393739769620083, -42.61618894467930119, -65.65000000000000568 ) ) ;
#40587 = ORIENTED_EDGE ( 'NONE', *, *, #11230, .T. ) ;
#40588 = CARTESIAN_POINT ( 'NONE',  ( 22.46008168199778865, -10.75448223654004742, -75.29930970037709415 ) ) ;
#40589 = CARTESIAN_POINT ( 'NONE',  ( 11.10574934303680017, -63.48107579820671020, -44.26157399421149563 ) ) ;
#40590 = CARTESIAN_POINT ( 'NONE',  ( 13.88455142272560039, 20.94377921756336036, -75.56421430877985301 ) ) ;
#40591 = CARTESIAN_POINT ( 'NONE',  ( 46.25525774125586054, 2.762490711761019568, -54.56299356781535437 ) ) ;
#40592 = ADVANCED_FACE ( 'NONE', ( #16781 ), #9671, .T. ) ;
#40593 = CARTESIAN_POINT ( 'NONE',  ( 63.47971227208819300, 1.385888765344519991, -62.64792042614390510 ) ) ;
#40594 = CARTESIAN_POINT ( 'NONE',  ( 68.13393739823651174, -1.166188944679350081, -81.65000000000000568 ) ) ;
#40595 = ORIENTED_EDGE ( 'NONE', *, *, #36378, .T. ) ;
#40596 = CARTESIAN_POINT ( 'NONE',  ( -21.36606260230379917, 30.88381105532059934, 10.84999999999999964 ) ) ;
#40597 = DIRECTION ( 'NONE',  ( 1.000000000000000000, 0.000000000000000000, 0.000000000000000000 ) ) ;
#40598 = ORIENTED_EDGE ( 'NONE', *, *, #46340, .T. ) ;
#40599 = DIRECTION ( 'NONE',  ( 0.000000000000000000, -0.7071067811865292541, 0.7071067811865656694 ) ) ;
#40600 = CARTESIAN_POINT ( 'NONE',  ( 60.22029979666620392, 14.82624742056550105, -47.95282500047770213 ) ) ;
#40601 = B_SPLINE_CURVE_WITH_KNOTS ( 'NONE', 3,
 ( #6875, #50380, #10802, #5833, #21796, #46458 ),
 .UNSPECIFIED., .F., .F.,
 ( 4, 2, 4 ),
 ( 0.000000000000000000, 0.6321606378469137866, 1.000000000000000000 ),
 .UNSPECIFIED. ) ;
#40602 = CARTESIAN_POINT ( 'NONE',  ( 20.61809888542150304, -22.53536633855610205, -74.10929620427440057 ) ) ;
#40603 = VECTOR ( 'NONE', #15354, 1000.000000000000000 ) ;
#40604 = CARTESIAN_POINT ( 'NONE',  ( 68.13393739769810509, 19.38381105532030091, -71.50000000000198952 ) ) ;
#40605 = CARTESIAN_POINT ( 'NONE',  ( 56.57234443381329925, 19.50072803673270272, -74.30166440113460169 ) ) ;
#40606 = APPLICATION_PROTOCOL_DEFINITION ( 'draft international standard', 'automotive_design', 1998, #10382 ) ;
#40607 = CARTESIAN_POINT ( 'NONE',  ( 46.90719325741979873, -53.72294727813159909, -75.90528168595349712 ) ) ;
#40608 = ORIENTED_EDGE ( 'NONE', *, *, #28206, .F. ) ;
#40609 = CARTESIAN_POINT ( 'NONE',  ( 15.24815623221091521, -22.38319100513449200, -36.99448562645851979 ) ) ;
#40610 = CARTESIAN_POINT ( 'NONE',  ( 8.714178796388031500, -14.94248566914980003, -67.26148035172319339 ) ) ;
#40611 = CARTESIAN_POINT ( 'NONE',  ( 53.36506516905719621, -49.48367947020049940, -49.20548766773279681 ) ) ;
#40612 = EDGE_CURVE ( 'NONE', #32835, #36176, #8658, .T. ) ;
#40613 = CYLINDRICAL_SURFACE ( 'NONE', #24672, 0.9999999999999991118 ) ;
#40614 = DIRECTION ( 'NONE',  ( 0.000000000000000000, -1.000000000000000000, 0.000000000000000000 ) ) ;
#40615 = ADVANCED_FACE ( 'NONE', ( #4991 ), #44045, .F. ) ;
#40616 = CARTESIAN_POINT ( 'NONE',  ( 46.82266861842990124, 22.42583874316209958, -75.96020792128800281 ) ) ;
#40617 = CIRCLE ( 'NONE', #10479, 11.00000000000000000 ) ;
#40618 = CARTESIAN_POINT ( 'NONE',  ( 23.06214062797170072, -27.61618894467930119, -24.15000000000000213 ) ) ;
#40619 = EDGE_CURVE ( 'NONE', #2348, #12279, #16360, .T. ) ;
#40620 = CARTESIAN_POINT ( 'NONE',  ( 75.10755973209502656, -25.67677511771720944, -11.59100465374893574 ) ) ;
#40621 = DIRECTION ( 'NONE',  ( 0.000000000000000000, 0.000000000000000000, 1.000000000000000000 ) ) ;
#40622 = LINE ( 'NONE', #4720, #38943 ) ;
#40623 = CARTESIAN_POINT ( 'NONE',  ( 44.07452568954059302, -33.11618894467940066, -54.64999999999999858 ) ) ;
#40624 = CARTESIAN_POINT ( 'NONE',  ( 41.48201311892960774, -39.75838402827952223, -78.61445045689941935 ) ) ;
#40625 = CARTESIAN_POINT ( 'NONE',  ( 63.13616699414190236, 0.9259537755896120048, -68.96999734323989628 ) ) ;
#40626 = CARTESIAN_POINT ( 'NONE',  ( 61.14297824559450589, 14.08836494215110058, -46.99581295334250086 ) ) ;
#40627 = CARTESIAN_POINT ( 'NONE',  ( 6.264007226339749934, -63.37915212591551040, -47.23119725298560212 ) ) ;
#40628 = ORIENTED_EDGE ( 'NONE', *, *, #9938, .F. ) ;
#40629 = ADVANCED_FACE ( 'NONE', ( #28818 ), #23075, .F. ) ;
#40630 = CARTESIAN_POINT ( 'NONE',  ( 53.06802000122009844, -49.53608743370789824, -48.81041485548290382 ) ) ;
#40631 = CARTESIAN_POINT ( 'NONE',  ( 61.58999301232780255, -45.12803339529550328, -28.02454186838919981 ) ) ;
#40632 = AXIS2_PLACEMENT_3D ( 'NONE', #9112, #5698, #1504 ) ;
#40633 = CARTESIAN_POINT ( 'NONE',  ( 47.95926718124380272, -54.39950235201530404, -55.26638612347969826 ) ) ;
#40634 = CARTESIAN_POINT ( 'NONE',  ( 56.77968109326819501, 14.56960969026870067, -26.16725212139149903 ) ) ;
#40635 = CARTESIAN_POINT ( 'NONE',  ( 21.22754492721490038, -10.73789807064090063, -34.20969220765409347 ) ) ;
#40636 = CARTESIAN_POINT ( 'NONE',  ( 50.55910572479910314, 19.00727530243110053, -76.14999999999999147 ) ) ;
#40638 = ADVANCED_FACE ( 'NONE', ( #32463 ), #48492, .T. ) ;
#40637 = CARTESIAN_POINT ( 'NONE',  ( 53.32371982237880559, 18.17626688474259922, -48.89504544885870274 ) ) ;
#40639 = CARTESIAN_POINT ( 'NONE',  ( 71.24581987525910165, 0.9960089569207349891, -70.77007079217121088 ) ) ;
#40640 = CARTESIAN_POINT ( 'NONE',  ( 41.55663456559430102, -43.85962873145379604, -3.466044033466880059 ) ) ;
#40641 = CARTESIAN_POINT ( 'NONE',  ( 63.88486207242520720, -43.42060977382210041, -10.13980136567960066 ) ) ;
#40642 = VECTOR ( 'NONE', #34815, 1000.000000000000000 ) ;
#40643 = ORIENTED_EDGE ( 'NONE', *, *, #44814, .T. ) ;
#40644 = CARTESIAN_POINT ( 'NONE',  ( 8.222937397696199469, -15.61618894467929941, -32.14999999999999858 ) ) ;
#40645 = CARTESIAN_POINT ( 'NONE',  ( 73.13170780125059878, 0.9259537755896120048, -68.96999734323989628 ) ) ;
#40646 = CARTESIAN_POINT ( 'NONE',  ( 47.59050665785859735, -54.53298138600730027, -54.74365073385350655 ) ) ;
#40647 = CARTESIAN_POINT ( 'NONE',  ( 9.588669338623654781, -13.31599288703087858, -67.95535226952054586 ) ) ;
#40648 = LINE ( 'NONE', #45102, #4767 ) ;
#40649 = CARTESIAN_POINT ( 'NONE',  ( 42.11778985390380114, 12.11280974652049913, -3.278435070539889917 ) ) ;
#40650 = CARTESIAN_POINT ( 'NONE',  ( 59.73488990452629821, 15.43279671172489920, -48.60609801886729997 ) ) ;
#40651 = CARTESIAN_POINT ( 'NONE',  ( 71.53768886009270034, 0.9325382164350239922, -60.70884169071130287 ) ) ;
#40652 = LINE ( 'NONE', #40393, #20796 ) ;
#40653 = CARTESIAN_POINT ( 'NONE',  ( 72.15767745866649818, 1.191618978581419963, -61.23657242805779788 ) ) ;
#40654 = LINE ( 'NONE', #25168, #31820 ) ;
#40655 = CARTESIAN_POINT ( 'NONE',  ( 64.84489409100208945, 0.9242073871622918935, -70.66822101033309877 ) ) ;
#40656 = ORIENTED_EDGE ( 'NONE', *, *, #9310, .T. ) ;
#40657 = ORIENTED_EDGE ( 'NONE', *, *, #18510, .T. ) ;
#40658 = CARTESIAN_POINT ( 'NONE',  ( 9.221369605823916515, -11.63213385460635685, -54.95899190682911239 ) ) ;
#40659 = LINE ( 'NONE', #36714, #4306 ) ;
#40660 = VERTEX_POINT ( 'NONE', #12596 ) ;
#40661 = CARTESIAN_POINT ( 'NONE',  ( 11.38042686594670094, -64.49026764409909163, -44.43661832440050574 ) ) ;
#40662 = CARTESIAN_POINT ( 'NONE',  ( 15.09830787208028902, -7.705198857361269305, -58.96596456551435494 ) ) ;
#40663 = CARTESIAN_POINT ( 'NONE',  ( 40.57649240635721810, -36.11618894467930119, -83.97002642401369599 ) ) ;
#40664 = CARTESIAN_POINT ( 'NONE',  ( 52.48374443017399926, 19.52726341579099767, -76.33825989979830240 ) ) ;
#40665 = VERTEX_POINT ( 'NONE', #20180 ) ;
#40666 = CARTESIAN_POINT ( 'NONE',  ( 11.53605495837543948, -55.35105376503654639, -21.73576846289474318 ) ) ;
#40667 = DIRECTION ( 'NONE',  ( 0.000000000000000000, 0.000000000000000000, -1.000000000000000000 ) ) ;
#40668 = CARTESIAN_POINT ( 'NONE',  ( 18.40285012985609825, -23.54302659091490213, -40.20359370904520091 ) ) ;
#40669 = VECTOR ( 'NONE', #23205, 1000.000000000000114 ) ;
#40670 = CYLINDRICAL_SURFACE ( 'NONE', #15437, 6.766999999999998572 ) ;
#40671 = CARTESIAN_POINT ( 'NONE',  ( 43.08604041149931874, -37.79059854641297989, -74.88947594510764816 ) ) ;
#40672 =( NAMED_UNIT ( * ) SI_UNIT ( $, .STERADIAN. ) SOLID_ANGLE_UNIT ( ) );
#40673 = ORIENTED_EDGE ( 'NONE', *, *, #6143, .T. ) ;
#40674 = CARTESIAN_POINT ( 'NONE',  ( 64.93393739769619799, 4.883811055320659733, -61.44999999999999574 ) ) ;
#40675 = CARTESIAN_POINT ( 'NONE',  ( 22.38096263179139811, -11.55646364244059932, -36.04922151265719776 ) ) ;
#40676 = CARTESIAN_POINT ( 'NONE',  ( 15.09831361134191496, -7.705198193276967089, -32.96599948321726714 ) ) ;
#40677 = CIRCLE ( 'NONE', #25617, 6.999999999999999112 ) ;
#40678 = EDGE_CURVE ( 'NONE', #17738, #51359, #24612, .T. ) ;
#40679 = CARTESIAN_POINT ( 'NONE',  ( 13.80985048470530074, 20.88378464714680049, -75.46937177410670472 ) ) ;
#40680 = ADVANCED_FACE ( 'NONE', ( #8147 ), #10055, .T. ) ;
#40681 = CARTESIAN_POINT ( 'NONE',  ( 51.85719037988729951, 18.05925585374960107, -77.06876492569810466 ) ) ;
#40682 = CARTESIAN_POINT ( 'NONE',  ( 83.54531734280109845, -44.64140434283670089, -46.66630366969080512 ) ) ;
#40683 = DIRECTION ( 'NONE',  ( 0.000000000000000000, 0.000000000000000000, 1.000000000000000000 ) ) ;
#40684 = CARTESIAN_POINT ( 'NONE',  ( 11.19896969917839868, -22.22140010887079953, -50.21191628250519301 ) ) ;
#40685 = ORIENTED_EDGE ( 'NONE', *, *, #15091, .F. ) ;
#40686 = CARTESIAN_POINT ( 'NONE',  ( 53.03694355186379994, -49.40910104661059421, -27.39159970799200039 ) ) ;
#40687 = CARTESIAN_POINT ( 'NONE',  ( 14.61081989480809895, -51.05470123690699324, -21.82083395458209907 ) ) ;
#40688 = CARTESIAN_POINT ( 'NONE',  ( 50.40119816437731259, -36.24976658303432941, -76.18455893466475004 ) ) ;
#40689 = DIRECTION ( 'NONE',  ( 1.000000000000000000, 2.460964292799963328E-14, 0.000000000000000000 ) ) ;
#40690 = CARTESIAN_POINT ( 'NONE',  ( 16.51210842463290263, -8.573494442649787217, -56.36425564602672011 ) ) ;
#40691 = DIRECTION ( 'NONE',  ( -0.7071067811865475727, 0.7071067811865475727, 0.000000000000000000 ) ) ;
#40692 = ORIENTED_EDGE ( 'NONE', *, *, #36989, .F. ) ;
#40693 = CARTESIAN_POINT ( 'NONE',  ( -7.621576387460760493, -45.43712284492340103, -5.646501867015009779 ) ) ;
#40694 = CARTESIAN_POINT ( 'NONE',  ( 47.24472437627869681, 23.52728567798950010, -54.64339285785950295 ) ) ;
#40695 = VECTOR ( 'NONE', #15902, 1000.000000000000114 ) ;
#40696 = DIRECTION ( 'NONE',  ( -1.000000000000000000, 0.000000000000000000, 0.000000000000000000 ) ) ;
#40697 = CARTESIAN_POINT ( 'NONE',  ( 63.21844385136499511, 1.269319268680890067, -62.52104542963419931 ) ) ;
#40698 = DIRECTION ( 'NONE',  ( -0.8660254037844379305, 0.5000000000000011102, 0.000000000000000000 ) ) ;
#40699 = CARTESIAN_POINT ( 'NONE',  ( 11.93810463912310027, 34.20707664335219533, -17.87564887320120022 ) ) ;
#40700 = CARTESIAN_POINT ( 'NONE',  ( 68.13393739769620083, 0.8838110553206759423, -65.65000000000000568 ) ) ;
#40702 = EDGE_CURVE ( 'NONE', #47510, #44163, #33132, .T. ) ;
#40701 = CARTESIAN_POINT ( 'NONE',  ( 68.13393739769769297, 18.72622661238600017, -69.60146707679309941 ) ) ;
#40703 = CARTESIAN_POINT ( 'NONE',  ( 68.13393739769620083, -48.61618894467930119, -65.65000000000000568 ) ) ;
#40704 = CARTESIAN_POINT ( 'NONE',  ( 57.81609062655950027, -47.19091213400450613, -48.15256270216469403 ) ) ;
#40705 = VECTOR ( 'NONE', #19373, 1000.000000000000000 ) ;
#40706 = CARTESIAN_POINT ( 'NONE',  ( 68.13393739769847457, -50.70395984887981200, -74.34354914830335304 ) ) ;
#40707 = CARTESIAN_POINT ( 'NONE',  ( 64.87536163491139973, 1.372372808637209785, -60.98718532932910819 ) ) ;
#40708 = CARTESIAN_POINT ( 'NONE',  ( 17.73212549933870008, -52.38593004734789815, -75.99067819366339904 ) ) ;
#40709 = EDGE_CURVE ( 'NONE', #4493, #43673, #45478, .T. ) ;
#40710 = CARTESIAN_POINT ( 'NONE',  ( 16.65420337941489848, 17.88381105532299742, -17.90311212357439885 ) ) ;
#40711 = CARTESIAN_POINT ( 'NONE',  ( 12.09990282912350068, -65.24532120969969640, -16.83009741455080288 ) ) ;
#40712 = CARTESIAN_POINT ( 'NONE',  ( 17.70165363224570143, -22.49258516525739893, -61.27582937196799406 ) ) ;
#40713 = ORIENTED_EDGE ( 'NONE', *, *, #23919, .T. ) ;
#40714 = CARTESIAN_POINT ( 'NONE',  ( 44.13393739769620083, 4.883811055320659733, -35.14999999999999858 ) ) ;
#40715 = CARTESIAN_POINT ( 'NONE',  ( 9.299128317299539148, 32.06192745982850312, -46.53057822423220102 ) ) ;
#40716 = DIRECTION ( 'NONE',  ( 1.000000000000000000, 0.000000000000000000, 0.000000000000000000 ) ) ;
#40717 = AXIS2_PLACEMENT_3D ( 'NONE', #28628, #49101, #8734 ) ;
#40718 = CARTESIAN_POINT ( 'NONE',  ( 67.73239348926679781, -31.31112839167719741, -17.99563373446390102 ) ) ;
#40719 = VERTEX_POINT ( 'NONE', #6806 ) ;
#40720 = CARTESIAN_POINT ( 'NONE',  ( 18.76586980408200134, 20.63642445556759952, -74.86150924066380696 ) ) ;
#40721 = CIRCLE ( 'NONE', #21469, 36.55167969755429880 ) ;
#40722 = ORIENTED_EDGE ( 'NONE', *, *, #24406, .F. ) ;
#40723 = ORIENTED_EDGE ( 'NONE', *, *, #24509, .T. ) ;
#40724 = ORIENTED_EDGE ( 'NONE', *, *, #15718, .T. ) ;
#40725 = CARTESIAN_POINT ( 'NONE',  ( 10.67183281957709973, -63.52764994537149335, -45.41177609095300483 ) ) ;
#40726 = DIRECTION ( 'NONE',  ( 0.000000000000000000, 0.000000000000000000, -1.000000000000000000 ) ) ;
#40727 = CARTESIAN_POINT ( 'NONE',  ( 20.81226749614940275, -20.80205290968870102, -81.23899999999999011 ) ) ;
#40728 = CARTESIAN_POINT ( 'NONE',  ( 61.52836517851630305, 13.92984914567709964, -46.71062307070980069 ) ) ;
#40729 = EDGE_LOOP ( 'NONE', ( #815, #37637 ) ) ;
#40730 = CARTESIAN_POINT ( 'NONE',  ( 75.24618922237742424, 2.926750969086042709, -12.27132002303570069 ) ) ;
#40731 = CARTESIAN_POINT ( 'NONE',  ( 12.16177389586671964, 33.87933702454814977, -16.53048054918994936 ) ) ;
#40732 = ORIENTED_EDGE ( 'NONE', *, *, #43960, .T. ) ;
#40733 = CARTESIAN_POINT ( 'NONE',  ( 49.42577828663870321, -46.18035913434329842, -12.04425446003870093 ) ) ;
#40734 = CARTESIAN_POINT ( 'NONE',  ( 3.987490788289483667, -19.08029055981709732, -34.79644660940672907 ) ) ;
#40735 = CARTESIAN_POINT ( 'NONE',  ( 14.13393739769619906, -41.61618894467930119, -54.64999999999999858 ) ) ;
#40736 = ORIENTED_EDGE ( 'NONE', *, *, #20877, .T. ) ;
#40737 = ORIENTED_EDGE ( 'NONE', *, *, #44062, .T. ) ;
#40738 = CARTESIAN_POINT ( 'NONE',  ( 72.72759757326660690, 1.395196698723390138, -62.46966344801350601 ) ) ;
#40739 = CARTESIAN_POINT ( 'NONE',  ( 10.89208569015771388, -65.00086843820284344, -17.57297834641052603 ) ) ;
#40740 = DIRECTION ( 'NONE',  ( 0.000000000000000000, 0.000000000000000000, -1.000000000000000000 ) ) ;
#40741 = CARTESIAN_POINT ( 'NONE',  ( 50.20812286835639782, 14.95963111490540065, -12.60694443316879898 ) ) ;
#40742 = EDGE_CURVE ( 'NONE', #630, #10139, #27732, .T. ) ;
#40743 = CARTESIAN_POINT ( 'NONE',  ( 8.222946539407685052, -16.65180334102045023, -68.75066474143523010 ) ) ;
#40744 = CARTESIAN_POINT ( 'NONE',  ( -11.32734370190460105, 10.64934056395049922, -6.430192534648650593 ) ) ;
#40745 = DIRECTION ( 'NONE',  ( -0.8090169943749478954, -0.5877852522924724710, 0.000000000000000000 ) ) ;
#40746 = AXIS2_PLACEMENT_3D ( 'NONE', #40074, #24314, #48989 ) ;
#40747 = CARTESIAN_POINT ( 'NONE',  ( 55.78775146822957254, 14.70279260508580776, -17.21510844903624005 ) ) ;
#40748 = CARTESIAN_POINT ( 'NONE',  ( 14.14244093349880060, -8.025359608152760060, -58.70583579685229836 ) ) ;
#40749 = VERTEX_POINT ( 'NONE', #22758 ) ;
#40750 = CARTESIAN_POINT ( 'NONE',  ( 18.07449423817570278, 1.323206481297259929, -34.90839531524139971 ) ) ;
#40751 = CARTESIAN_POINT ( 'NONE',  ( 12.00070700938809942, 33.94152585701019831, -45.91242252782910072 ) ) ;
#40752 = CARTESIAN_POINT ( 'NONE',  ( 72.55698300813111246, 1.048861872235970161, -69.70476459732599039 ) ) ;
#40753 = CARTESIAN_POINT ( 'NONE',  ( 41.18693779094563467, -39.67249569471185566, -80.25382149713556146 ) ) ;
#40754 = CARTESIAN_POINT ( 'NONE',  ( 13.19614974924530060, 18.82172380121849997, -21.01902014306970301 ) ) ;
#40756 = EDGE_CURVE ( 'NONE', #51329, #28860, #6391, .T. ) ;
#40755 = CARTESIAN_POINT ( 'NONE',  ( 47.17214619674849985, 23.54985310318610203, -74.50417157308129390 ) ) ;
#40757 = CARTESIAN_POINT ( 'NONE',  ( 49.12468868441940373, -53.81509191060310116, -54.67300365794890382 ) ) ;
#40758 = CARTESIAN_POINT ( 'NONE',  ( 58.92073396209919878, -3.116188944679349593, -15.65000000000000036 ) ) ;
#40759 = CARTESIAN_POINT ( 'NONE',  ( 24.04493739840414435, -15.61820873891454120, -33.50774649806280081 ) ) ;
#40760 = FACE_OUTER_BOUND ( 'NONE', #9285, .T. ) ;
#40761 = EDGE_CURVE ( 'NONE', #49655, #20898, #39811, .T. ) ;
#40762 = CARTESIAN_POINT ( 'NONE',  ( 57.00722761779879733, 13.88381105532070059, -15.97596069844019873 ) ) ;
#40763 = ORIENTED_EDGE ( 'NONE', *, *, #20026, .F. ) ;
#40764 = CARTESIAN_POINT ( 'NONE',  ( 9.197401484353060042, -18.33485844670460096, -39.94844302531450353 ) ) ;
#40765 = CARTESIAN_POINT ( 'NONE',  ( 63.95069823516159602, 1.061277144319840104, -61.34795443974510221 ) ) ;
#40766 = VERTEX_POINT ( 'NONE', #20895 ) ;
#40767 = CARTESIAN_POINT ( 'NONE',  ( 84.41931977238152740, -43.28155736009810539, -47.35294579201847398 ) ) ;
#40768 = CARTESIAN_POINT ( 'NONE',  ( 60.35161375623229674, -45.78197740793289938, -47.56115285142140436 ) ) ;
#40769 = CARTESIAN_POINT ( 'NONE',  ( 56.99190255428169394, 19.40009799746960084, -53.87165542181880085 ) ) ;
#40770 = CARTESIAN_POINT ( 'NONE',  ( 12.28937882765760037, 18.77527565194250059, -21.14656491342549671 ) ) ;
#40772 = DIRECTION ( 'NONE',  ( 0.000000000000000000, 0.000000000000000000, -1.000000000000000000 ) ) ;
#40771 = CARTESIAN_POINT ( 'NONE',  ( 41.14613706618169431, 8.435299800057125097, -80.45036690760321108 ) ) ;
#40773 = CARTESIAN_POINT ( 'NONE',  ( 9.366365007129969555, -15.61616877484880028, -59.84717978381009118 ) ) ;
#40774 = CARTESIAN_POINT ( 'NONE',  ( 9.807778990346434966, -20.47787572195374750, -52.29933454858549169 ) ) ;
#40775 = ORIENTED_EDGE ( 'NONE', *, *, #5103, .F. ) ;
#40776 = CARTESIAN_POINT ( 'NONE',  ( 83.77685426296399385, -44.72604696044789563, -47.23654203728539613 ) ) ;
#40777 = VERTEX_POINT ( 'NONE', #27979 ) ;
#40778 = ORIENTED_EDGE ( 'NONE', *, *, #30330, .F. ) ;
#40779 = EDGE_LOOP ( 'NONE', ( #27540, #1974, #16619, #46284, #6120, #7947 ) ) ;
#40780 = CARTESIAN_POINT ( 'NONE',  ( 61.62976587585850297, -45.12285621563059834, -46.37194070680949665 ) ) ;
#40781 = DIRECTION ( 'NONE',  ( 1.000000000000000000, 0.000000000000000000, 0.000000000000000000 ) ) ;
#40782 = CARTESIAN_POINT ( 'NONE',  ( 76.42335732216182009, -22.53194434191319218, -12.89715778059380824 ) ) ;
#40783 = CARTESIAN_POINT ( 'NONE',  ( 56.15635836398279679, -50.90785405786900242, -53.88620114773970471 ) ) ;
#40784 = CIRCLE ( 'NONE', #46691, 2.000000000000001776 ) ;
#40785 = ORIENTED_EDGE ( 'NONE', *, *, #26605, .F. ) ;
#40786 = ORIENTED_EDGE ( 'NONE', *, *, #8269, .T. ) ;
#40787 = CARTESIAN_POINT ( 'NONE',  ( 48.64758560217519801, 22.70397928459539827, -54.52813621919599996 ) ) ;
#40788 = CARTESIAN_POINT ( 'NONE',  ( -8.565972701125874167, 14.56525628855416166, -42.60118799329718797 ) ) ;
#40789 = CARTESIAN_POINT ( 'NONE',  ( 22.03527629826074374, -11.75396699927941491, -66.66271668430944430 ) ) ;
#40790 = CARTESIAN_POINT ( 'NONE',  ( 16.13393739769620083, -15.61618894467929941, -170.7999095292539948 ) ) ;
#40791 = CARTESIAN_POINT ( 'NONE',  ( 22.46008339447744717, -10.75448427898152914, -59.58402698800288277 ) ) ;
#40792 = DIRECTION ( 'NONE',  ( -1.000000000000000000, 0.000000000000000000, 0.000000000000000000 ) ) ;
#40793 = ORIENTED_EDGE ( 'NONE', *, *, #50363, .F. ) ;
#40794 = DIRECTION ( 'NONE',  ( 0.000000000000000000, 0.000000000000000000, -1.000000000000000000 ) ) ;
#40795 = CARTESIAN_POINT ( 'NONE',  ( 53.48387799555199251, -50.52031544494510484, -77.13966324944060204 ) ) ;
#40796 = CARTESIAN_POINT ( 'NONE',  ( 16.73169708462201299, -22.35857779895397712, -46.92468125870891527 ) ) ;
#40797 = CARTESIAN_POINT ( 'NONE',  ( 60.49536215360559765, 14.41231689077920031, -47.20225698283260840 ) ) ;
#40798 = CARTESIAN_POINT ( 'NONE',  ( 10.56734057524939985, -21.14789278779199933, -62.76349517163679081 ) ) ;
#40799 = DIRECTION ( 'NONE',  ( 0.000000000000000000, 1.000000000000000000, 0.000000000000000000 ) ) ;
#40800 = EDGE_CURVE ( 'NONE', #12954, #19589, #1666, .T. ) ;
#40801 = CARTESIAN_POINT ( 'NONE',  ( 41.57868392304440164, -44.36040080565599908, -4.871763622046390019 ) ) ;
#40802 = DIRECTION ( 'NONE',  ( 1.000000000000000000, 0.000000000000000000, 0.000000000000000000 ) ) ;
#40803 = CARTESIAN_POINT ( 'NONE',  ( 71.79848734841171165, 0.9405967369903629471, -60.89823624368929700 ) ) ;
#40805 = EDGE_CURVE ( 'NONE', #11854, #44438, #47985, .T. ) ;
#40804 = CARTESIAN_POINT ( 'NONE',  ( 61.20230452259990273, -45.64718664723880437, -47.73655850518729693 ) ) ;
#40806 =( BOUNDED_CURVE ( )  B_SPLINE_CURVE ( 3, ( #30766, #30509, #34962, #40383 ),
 .UNSPECIFIED., .F., .T. ) 
 B_SPLINE_CURVE_WITH_KNOTS ( ( 4, 4 ),
 ( 2.356194490192344837, 3.141592653589793116 ),
 .UNSPECIFIED. ) 
 CURVE ( )  GEOMETRIC_REPRESENTATION_ITEM ( )  RATIONAL_B_SPLINE_CURVE ( ( 1.000000000000000000, 0.9492530216741911220, 0.9492530216741911220, 1.000000000000000000 ) ) 
 REPRESENTATION_ITEM ( '' )  );
#40807 = EDGE_CURVE ( 'NONE', #30733, #43378, #16696, .T. ) ;
#40808 = CARTESIAN_POINT ( 'NONE',  ( 64.17132984853199673, 1.406832289998090069, -69.92220598882080651 ) ) ;
#40809 = DIRECTION ( 'NONE',  ( -1.000000000000000000, -1.791661345120054866E-29, -4.486507500526829843E-12 ) ) ;
#40810 = EDGE_CURVE ( 'NONE', #19003, #10310, #11046, .T. ) ;
#40811 = CARTESIAN_POINT ( 'NONE',  ( 66.39756463022349919, 1.816743601633340033, -19.74079115529689687 ) ) ;
#40812 = B_SPLINE_SURFACE_WITH_KNOTS ( 'NONE', 3, 3, ( 
 ( #23159, #19247, #11655, #31280, #23672, #27874, #11140, #39176, #47814, #364, #11921, #43877, #39947, #4043, #36253, #35999 ),
 ( #27110, #43113, #24956, #9013, #9534, #13214, #45163, #44643, #44907, #21297, #21038, #29165, #37040, #8749, #37301, #17133 ),
 ( #48324, #40968, #12688, #36511, #28383, #24697, #613, #9277, #28641, #33354, #879, #16872, #25484, #32820, #49115, #40715 ),
 ( #32301, #44390, #28905, #1399, #29425, #49372, #8491, #37552, #4812, #25225, #45431, #5344, #20778, #41230, #17388, #13470 ),
 ( #12950, #5085, #16599, #24437, #41488, #36768, #5601, #32552, #1138, #21557, #12419, #16345, #40452, #4545, #48846, #33085 ),
 ( #20517, #48587, #10821, #22844, #41747, #18156, #29932, #13723, #34644, #18410, #22331, #38337, #26783, #5853, #10304, #46478 ),
 ( #2426, #30455, #6115, #14745, #1918, #33616, #26004, #42798, #1658, #30715, #2697, #26266, #46737, #25740, #50649, #6894 ),
 ( #10564, #22071, #34386, #50398, #9788, #17650, #49630, #14484, #26521, #42538, #10040, #6369, #34122, #29677, #45687, #50133 ),
 ( #14229, #18670, #38080, #13975, #37825, #21817, #42272, #2177, #46218, #17896, #38607, #33869, #49880, #30201, #45949, #6626 ),
 ( #22590, #43054, #51428, #19185, #11082, #2954, #27050, #34908, #38865, #18924, #35166, #50907, #14999, #30967, #19949, #19446 ),
 ( #16033, #51173, #15774, #39374, #23865, #47500, #15267, #31222, #27557, #3214, #47754, #46998, #15524, #39887, #47249, #7150 ) ),
 .UNSPECIFIED., .F., .F., .F.,
 ( 4, 1, 1, 1, 1, 1, 1, 1, 4 ),
 ( 4, 2, 2, 2, 2, 2, 2, 4 ),
 ( 0.000000000000000000, 0.1250000000000000000, 0.2500000000000000000, 0.3750000000000000000, 0.5000000000000000000, 0.6250000000000000000, 0.7500000000000000000, 0.8750000000000000000, 1.000000000000000000 ),
 ( -0.4072589812491140271, -0.3359886595305190404, -0.2545368632806960241, -0.2036294906245569858, -0.1781758042964870226, -0.1374499061715759862, -0.07228846917171800890, 0.000000000000000000 ),
 .UNSPECIFIED. ) ;
#40813 = EDGE_LOOP ( 'NONE', ( #4621, #7083, #6058, #42147 ) ) ;
#40814 = CARTESIAN_POINT ( 'NONE',  ( 14.44817841379610002, -51.79813798162680172, -75.64877291256318870 ) ) ;
#40815 = CARTESIAN_POINT ( 'NONE',  ( 47.31442551589749712, -54.70848342480089599, -54.65525844330269933 ) ) ;
#40816 = CARTESIAN_POINT ( 'NONE',  ( 20.11806848324613028, -8.703665624651682364, -37.17433713982433119 ) ) ;
#40817 = CARTESIAN_POINT ( 'NONE',  ( 84.37071824923931729, 12.21453748216318225, -47.23470636407145662 ) ) ;
#40818 = CARTESIAN_POINT ( 'NONE',  ( 60.87196308501805930, -45.45251507131489177, -47.10470314364983579 ) ) ;
#40819 = CIRCLE ( 'NONE', #20719, 0.5000000000000000000 ) ;
#40820 = CARTESIAN_POINT ( 'NONE',  ( 23.41199157575060141, -16.89843572899400215, -32.14999999999999858 ) ) ;
#40821 = CARTESIAN_POINT ( 'NONE',  ( 47.80576864997149755, -54.41529265479059774, -54.77142112296580478 ) ) ;
#40823 = CARTESIAN_POINT ( 'NONE',  ( -6.571053818291229476, -46.36898988238050379, -5.603118524855751126 ) ) ;
#40822 = CARTESIAN_POINT ( 'NONE',  ( 16.13393739769620083, -15.61618894467929941, -22.14999999999999858 ) ) ;
#40824 = AXIS2_PLACEMENT_3D ( 'NONE', #48575, #24686, #36755 ) ;
#40825 = DIRECTION ( 'NONE',  ( 0.000000000000000000, 0.000000000000000000, -1.000000000000000000 ) ) ;
#40826 = EDGE_CURVE ( 'NONE', #17149, #2490, #18004, .T. ) ;
#40827 = CARTESIAN_POINT ( 'NONE',  ( 48.51680376425250074, 22.79139865270589738, -54.61040359998320071 ) ) ;
#40828 = ORIENTED_EDGE ( 'NONE', *, *, #470, .F. ) ;
#40829 = CARTESIAN_POINT ( 'NONE',  ( 20.57457857590170036, -10.13683997779680013, -68.56397102982089109 ) ) ;
#40830 = VERTEX_POINT ( 'NONE', #49482 ) ;
#40831 = FACE_BOUND ( 'NONE', #48562, .T. ) ;
#40832 = CARTESIAN_POINT ( 'NONE',  ( 53.48663704675684016, -49.34136594389416075, -49.00013169077879382 ) ) ;
#40833 = CARTESIAN_POINT ( 'NONE',  ( 57.18371625260090241, -50.61638664230350315, -53.90359199106109855 ) ) ;
#40835 = CARTESIAN_POINT ( 'NONE',  ( 52.71768855521909813, 18.48070669118740028, -27.77299963332060173 ) ) ;
#40834 = CARTESIAN_POINT ( 'NONE',  ( 83.23750369908759694, 13.58709911348850063, -46.42259446247510368 ) ) ;
#40836 = CARTESIAN_POINT ( 'NONE',  ( 23.17486471576589935, -16.02594643184229994, -64.47132387395669184 ) ) ;
#40837 = CARTESIAN_POINT ( 'NONE',  ( 82.75389963950320293, -45.59493862562369770, -47.67227237921210303 ) ) ;
#40838 = CARTESIAN_POINT ( 'NONE',  ( 57.12835595156409596, -45.11618894467940066, -16.21298877816359862 ) ) ;
#40839 = DIRECTION ( 'NONE',  ( 0.000000000000000000, 0.000000000000000000, 1.000000000000000000 ) ) ;
#40840 = ORIENTED_EDGE ( 'NONE', *, *, #8920, .F. ) ;
#40841 = ORIENTED_EDGE ( 'NONE', *, *, #9625, .T. ) ;
#40842 = CARTESIAN_POINT ( 'NONE',  ( 11.43875273178739960, -65.00398667583539236, -16.70124317897120036 ) ) ;
#40843 = CARTESIAN_POINT ( 'NONE',  ( 12.94333334658009882, 34.28195096612819981, -47.69450768049080125 ) ) ;
#40844 = LINE ( 'NONE', #36133, #12323 ) ;
#40845 = CARTESIAN_POINT ( 'NONE',  ( 50.25595676683099811, -52.23737648766640262, -51.95249114396919765 ) ) ;
#40846 = CARTESIAN_POINT ( 'NONE',  ( 20.11812592182209158, -22.52867792443588257, -63.84100292245498309 ) ) ;
#40847 = EDGE_CURVE ( 'NONE', #15849, #5766, #42364, .T. ) ;
#40848 = ORIENTED_EDGE ( 'NONE', *, *, #51125, .F. ) ;
#40849 = CARTESIAN_POINT ( 'NONE',  ( 0.7611760784153190906, -51.27432484048290462, -34.14606254259449258 ) ) ;
#40850 = CARTESIAN_POINT ( 'NONE',  ( 54.57308664466630432, 16.87911987759756727, -26.75817216227180495 ) ) ;
#40851 = FACE_OUTER_BOUND ( 'NONE', #29356, .T. ) ;
#40852 = DIRECTION ( 'NONE',  ( 0.000000000000000000, 0.000000000000000000, -1.000000000000000000 ) ) ;
#40853 = CARTESIAN_POINT ( 'NONE',  ( 50.28917927772980079, -49.63951472337090109, -76.14999999999999147 ) ) ;
#40854 = LINE ( 'NONE', #32973, #14573 ) ;
#40855 = VERTEX_POINT ( 'NONE', #45279 ) ;
#40856 = CARTESIAN_POINT ( 'NONE',  ( 53.87584899166620289, -48.41195041224399631, -26.23515327084989934 ) ) ;
#40857 = CARTESIAN_POINT ( 'NONE',  ( 2.422196078461449797, -25.82482932757800143, -35.02873218748179340 ) ) ;
#40858 = ORIENTED_EDGE ( 'NONE', *, *, #40742, .F. ) ;
#40859 = DIRECTION ( 'NONE',  ( 0.000000000000000000, 1.000000000000000000, 0.000000000000000000 ) ) ;
#40860 = MECHANICAL_DESIGN_GEOMETRIC_PRESENTATION_REPRESENTATION (  '', ( #39190 ), #25796 ) ;
#40861 = CARTESIAN_POINT ( 'NONE',  ( 53.93371072663619969, -46.24504243184900076, -15.35642390276739988 ) ) ;
#40862 = CARTESIAN_POINT ( 'NONE',  ( 16.12625695005860038, -7.768470256960290143, -35.51218288575169879 ) ) ;
#40863 = CARTESIAN_POINT ( 'NONE',  ( 13.64848148378749926, -51.39660537786010508, -23.00152637257979649 ) ) ;
#40864 = CARTESIAN_POINT ( 'NONE',  ( 0.3209249304026040028, 15.01904124785189865, -34.64999999999999858 ) ) ;
#40865 = EDGE_CURVE ( 'NONE', #39487, #13362, #6219, .T. ) ;
#40866 = CARTESIAN_POINT ( 'NONE',  ( 47.50285049045650254, -54.59925851099900029, -74.19801721955809626 ) ) ;
#40867 = EDGE_LOOP ( 'NONE', ( #7214, #37079, #47066, #8755 ) ) ;
#40868 = CARTESIAN_POINT ( 'NONE',  ( 38.67452568954060155, -36.11618894467930119, -84.65000000000000568 ) ) ;
#40869 = EDGE_CURVE ( 'NONE', #47211, #4764, #17906, .T. ) ;
#40870 = ADVANCED_FACE ( 'NONE', ( #46319 ), #9886, .T. ) ;
#40871 = CARTESIAN_POINT ( 'NONE',  ( 57.27851914992729832, -50.15376702335620251, -52.63313635724109929 ) ) ;
#40872 = CARTESIAN_POINT ( 'NONE',  ( 52.77360392991350579, -49.72529414377589774, -48.90177011830709830 ) ) ;
#40873 = CARTESIAN_POINT ( 'NONE',  ( 9.138897765566639464, -16.51739104625019650, -31.80638701630149967 ) ) ;
#40874 = PLANE ( 'NONE',  #27880 ) ;
#40875 = EDGE_CURVE ( 'NONE', #47320, #4677, #1366, .T. ) ;
#40876 = CARTESIAN_POINT ( 'NONE',  ( 47.48811402935950099, 23.34517892920809956, -74.50151902752439526 ) ) ;
#40877 = DIRECTION ( 'NONE',  ( 1.000000000000000000, 0.000000000000000000, 0.000000000000000000 ) ) ;
#40878 = CARTESIAN_POINT ( 'NONE',  ( 59.28524734660857831, -29.42491135532547020, -15.78018370959630445 ) ) ;
#40879 = CARTESIAN_POINT ( 'NONE',  ( 28.71032976354209865, -4.650001368963800452, -34.65450330891889763 ) ) ;
#40880 = CARTESIAN_POINT ( 'NONE',  ( 19.13393739769620083, -49.61618894467939356, -83.01107220193038927 ) ) ;
#40881 = DIRECTION ( 'NONE',  ( 0.000000000000000000, 1.000000000000000000, 0.000000000000000000 ) ) ;
#40882 = CARTESIAN_POINT ( 'NONE',  ( 30.38062185377579638, -35.62460461499323827, -84.60948432506590677 ) ) ;
#40883 = CARTESIAN_POINT ( 'NONE',  ( 63.30180592418038543, 1.263738073398970041, -68.93858679394679712 ) ) ;
#40884 = DIRECTION ( 'NONE',  ( 0.000000000000000000, -1.000000000000000000, 0.000000000000000000 ) ) ;
#40885 = EDGE_CURVE ( 'NONE', #50266, #9028, #10151, .T. ) ;
#40886 = CARTESIAN_POINT ( 'NONE',  ( -33.45614285200539939, -20.42943855637770056, -56.47882598457800185 ) ) ;
#40887 = ORIENTED_EDGE ( 'NONE', *, *, #27688, .F. ) ;
#40888 = CARTESIAN_POINT ( 'NONE',  ( 52.75872680408620141, -49.70160015685030430, -48.48805751657780405 ) ) ;
#40889 = CIRCLE ( 'NONE', #24970, 1.000000000000000888 ) ;
#40890 = DIRECTION ( 'NONE',  ( 0.4808500020228050897, 0.3493579760610313056, 0.8041966675616158966 ) ) ;
#40891 = CARTESIAN_POINT ( 'NONE',  ( 16.13393739769620083, -29.64169738395614218, -34.79644660940672907 ) ) ;
#40892 = CARTESIAN_POINT ( 'NONE',  ( 57.22461981268290288, 14.53251969692440149, -26.23717558781860149 ) ) ;
#40893 = CARTESIAN_POINT ( 'NONE',  ( 12.76051422255349976, -9.422436061403089980, -35.79407082892649328 ) ) ;
#40895 = CARTESIAN_POINT ( 'NONE',  ( 51.36576727628780503, 19.27592626937499887, -76.23494648113261007 ) ) ;
#40894 = AXIS2_PLACEMENT_3D ( 'NONE', #4487, #44322, #48518 ) ;
#40896 = CARTESIAN_POINT ( 'NONE',  ( 52.92152585432570078, 18.39031306738499794, -48.88490681319890285 ) ) ;
#40897 = CARTESIAN_POINT ( 'NONE',  ( 71.40743923234819590, 0.9234936569010840923, -70.67837287176459427 ) ) ;
#40898 = CARTESIAN_POINT ( 'NONE',  ( 42.29536634146680285, -43.17774985521609921, -3.241362036132339863 ) ) ;
#40899 = CARTESIAN_POINT ( 'NONE',  ( 75.47882570655470147, -43.69042101453369753, -13.44752134567739965 ) ) ;
#40900 = EDGE_LOOP ( 'NONE', ( #36525, #41058, #6512, #44776 ) ) ;
#40901 = CARTESIAN_POINT ( 'NONE',  ( 22.12150465969970270, -11.18271033062140063, -76.86446490096111006 ) ) ;
#40902 = ORIENTED_EDGE ( 'NONE', *, *, #43882, .T. ) ;
#40903 = CARTESIAN_POINT ( 'NONE',  ( 73.13041444294920268, 0.8910129994591549085, -68.97194292341539779 ) ) ;
#40904 = CARTESIAN_POINT ( 'NONE',  ( 47.46127172027109964, -54.61040224951049993, -54.70311265894389408 ) ) ;
#40905 = DIRECTION ( 'NONE',  ( 0.000000000000000000, 0.000000000000000000, -1.000000000000000000 ) ) ;
#40906 = CARTESIAN_POINT ( 'NONE',  ( 73.14840136429539541, 1.194703186106690129, -62.54674175640080591 ) ) ;
#40907 = CARTESIAN_POINT ( 'NONE',  ( 60.43132024577979422, -30.38530924120979648, -16.18952559267319913 ) ) ;
#40908 = CARTESIAN_POINT ( 'NONE',  ( 71.23750802749680133, 1.369613126987639928, -60.92417343964400089 ) ) ;
#40909 = CARTESIAN_POINT ( 'NONE',  ( 23.18393739769649642, -15.61618894467929941, -20.74999999999999289 ) ) ;
#40910 = CARTESIAN_POINT ( 'NONE',  ( 71.55783046266638792, 1.229734285826160178, -60.85522740516210405 ) ) ;
#40911 = EDGE_CURVE ( 'NONE', #19573, #30947, #26094, .T. ) ;
#40912 = CARTESIAN_POINT ( 'NONE',  ( 8.223124147305879816, -15.61599092713959891, -72.50766849176299900 ) ) ;
#40913 = CARTESIAN_POINT ( 'NONE',  ( 64.85231939490250852, 0.9948723650351710690, -70.66407068423170301 ) ) ;
#40914 = ORIENTED_EDGE ( 'NONE', *, *, #5430, .F. ) ;
#40915 = EDGE_CURVE ( 'NONE', #1577, #31691, #20389, .T. ) ;
#40916 = EDGE_LOOP ( 'NONE', ( #13165, #20551, #41967, #25381 ) ) ;
#40917 = CARTESIAN_POINT ( 'NONE',  ( 8.806603807574589382, -63.23125877106109982, -46.67034945549170288 ) ) ;
#40918 = CARTESIAN_POINT ( 'NONE',  ( 68.13393739769620083, -42.11618894467930119, -65.65000000000000568 ) ) ;
#40919 = ORIENTED_EDGE ( 'NONE', *, *, #41710, .F. ) ;
#40920 = CARTESIAN_POINT ( 'NONE',  ( 8.223124147305879816, -15.61599092713959891, -72.50766849176299900 ) ) ;
#40921 = CARTESIAN_POINT ( 'NONE',  ( 22.90093740148115486, -14.73038825474736413, -70.41115655435802978 ) ) ;
#40922 = LINE ( 'NONE', #12370, #12771 ) ;
#40923 = CARTESIAN_POINT ( 'NONE',  ( 52.12109120452969790, 19.65124629421640279, -76.21339085878619812 ) ) ;
#40924 = VERTEX_POINT ( 'NONE', #7253 ) ;
#40925 = CARTESIAN_POINT ( 'NONE',  ( 42.34723858680553832, 6.446719989108320448, -78.58349325317209377 ) ) ;
#40926 = CARTESIAN_POINT ( 'NONE',  ( 24.01558619446240073, -16.31994774379832336, -65.53600668441687560 ) ) ;
#40927 = CARTESIAN_POINT ( 'NONE',  ( 7.933294100319239206, -16.47185801921769865, -48.75923826391599647 ) ) ;
#40928 = LINE ( 'NONE', #13934, #12942 ) ;
#40929 = CARTESIAN_POINT ( 'NONE',  ( 42.59156136795025560, -37.71660974778794895, -77.36181849303467573 ) ) ;
#40930 = ORIENTED_EDGE ( 'NONE', *, *, #15601, .F. ) ;
#40931 = EDGE_CURVE ( 'NONE', #16669, #33243, #31582, .T. ) ;
#40932 = CARTESIAN_POINT ( 'NONE',  ( 12.93852378631490119, -65.51408294560670242, -23.45535008101469998 ) ) ;
#40933 = CARTESIAN_POINT ( 'NONE',  ( 8.886083854397551107, -17.34109845536059780, -37.15828654754790250 ) ) ;
#40935 = CARTESIAN_POINT ( 'NONE',  ( 53.16045469121779377, -49.55285059943579995, -49.13860152736959463 ) ) ;
#40934 = CIRCLE ( 'NONE', #11658, 1.999999999999997335 ) ;
#40936 = AXIS2_PLACEMENT_3D ( 'NONE', #213, #48171, #43727 ) ;
#40937 = CARTESIAN_POINT ( 'NONE',  ( 10.90613698351470084, -11.11335884447900035, -32.14999999999999858 ) ) ;
#40938 = AXIS2_PLACEMENT_3D ( 'NONE', #42484, #29877, #9984 ) ;
#40939 = ADVANCED_FACE ( 'NONE', ( #22698 ), #15374, .T. ) ;
#40940 = CARTESIAN_POINT ( 'NONE',  ( 14.43857095918710165, 21.38897561371040013, -76.01805773991210913 ) ) ;
#40941 = CARTESIAN_POINT ( 'NONE',  ( 8.222928832386770637, -16.58847042571065344, -60.75319795691873992 ) ) ;
#40942 = CARTESIAN_POINT ( 'NONE',  ( 84.22671941158239406, -43.79042781477089363, -46.99905560746359612 ) ) ;
#40943 = CARTESIAN_POINT ( 'NONE',  ( 12.51690838597220079, -23.02563034314670176, -48.15222407485109812 ) ) ;
#40944 = ORIENTED_EDGE ( 'NONE', *, *, #24545, .T. ) ;
#40945 = CARTESIAN_POINT ( 'NONE',  ( 52.80815860113929716, -49.65884401321449815, -27.90951286951370136 ) ) ;
#40946 = DIRECTION ( 'NONE',  ( -1.000000000000000000, 0.000000000000000000, 0.000000000000000000 ) ) ;
#40947 = DIRECTION ( 'NONE',  ( 0.000000000000000000, 0.000000000000000000, -1.000000000000000000 ) ) ;
#40948 = DIRECTION ( 'NONE',  ( 1.964275807512749840E-11, -1.000000000000000000, -5.103645611290830066E-11 ) ) ;
#40949 = DIRECTION ( 'NONE',  ( -0.9441882088883105650, 0.3294064756441258957, 0.000000000000000000 ) ) ;
#40950 = VERTEX_POINT ( 'NONE', #6999 ) ;
#40951 = CARTESIAN_POINT ( 'NONE',  ( -5.156079666866680178, -47.20144821879819830, -5.042520396575470798 ) ) ;
#40952 = CARTESIAN_POINT ( 'NONE',  ( 47.21369982259609799, 23.55075984592539839, -54.62698095723159497 ) ) ;
#40953 = CARTESIAN_POINT ( 'NONE',  ( 63.18170070234948810, 0.9989215084294049696, -62.27490163988890259 ) ) ;
#40954 = DIRECTION ( 'NONE',  ( -1.000000000000000000, 0.000000000000000000, 0.000000000000000000 ) ) ;
#40955 = CARTESIAN_POINT ( 'NONE',  ( 10.99341259034149942, 33.83928202847379652, -17.55111665511150321 ) ) ;
#40956 = CARTESIAN_POINT ( 'NONE',  ( 9.366943396716600034, -16.50203108585677825, -53.41115344186808755 ) ) ;
#40957 = CARTESIAN_POINT ( 'NONE',  ( 14.13393739769619906, -32.62399965035220362, -35.14999999999999858 ) ) ;
#40958 = CARTESIAN_POINT ( 'NONE',  ( 71.36792781540339092, 1.399433130755050048, -61.07453677926569924 ) ) ;
#40959 = CARTESIAN_POINT ( 'NONE',  ( 59.93954269256689571, -46.08041885259859782, -47.78497886280250384 ) ) ;
#40960 = CARTESIAN_POINT ( 'NONE',  ( 22.87803198333132570, -16.19128746702614308, -66.47989374956529218 ) ) ;
#40961 = CARTESIAN_POINT ( 'NONE',  ( 53.21122265239769433, 20.71035719222260241, -53.42198562142930029 ) ) ;
#40962 = AXIS2_PLACEMENT_3D ( 'NONE', #36047, #158, #16394 ) ;
#40963 = CARTESIAN_POINT ( 'NONE',  ( 11.27237125087875036, -9.289939099700770697, -72.79933495156693368 ) ) ;
#40964 = CIRCLE ( 'NONE', #9178, 1.000000000000000888 ) ;
#40965 = CARTESIAN_POINT ( 'NONE',  ( 24.04493737658144425, -16.65173835530648105, -75.54933311882003011 ) ) ;
#40966 = EDGE_LOOP ( 'NONE', ( #3094, #5012, #47765, #27055 ) ) ;
#40967 = DIRECTION ( 'NONE',  ( -1.000000000000000000, 0.000000000000000000, 0.000000000000000000 ) ) ;
#40968 = CARTESIAN_POINT ( 'NONE',  ( 9.275098868232870331, 31.89349584429000117, -46.53342726108229499 ) ) ;
#40969 = FACE_OUTER_BOUND ( 'NONE', #1039, .T. ) ;
#40970 = VECTOR ( 'NONE', #51649, 1000.000000000000000 ) ;
#40971 = EDGE_CURVE ( 'NONE', #16597, #13585, #25576, .T. ) ;
#40972 = CIRCLE ( 'NONE', #14193, 1.999999999999998446 ) ;
#40973 = CIRCLE ( 'NONE', #7496, 1.000000000000000888 ) ;
#40974 = CARTESIAN_POINT ( 'NONE',  ( 66.71248721992220965, -29.77431715107189802, -17.03569988378740163 ) ) ;
#40975 = VERTEX_POINT ( 'NONE', #11703 ) ;
#40976 = CARTESIAN_POINT ( 'NONE',  ( 18.62136613317600009, 20.52576179366229780, -75.06145659859170394 ) ) ;
#40977 = VERTEX_POINT ( 'NONE', #22951 ) ;
#40978 = EDGE_CURVE ( 'NONE', #5671, #19643, #8528, .T. ) ;
#40979 = ORIENTED_EDGE ( 'NONE', *, *, #39214, .F. ) ;
#40980 = CIRCLE ( 'NONE', #15025, 33.00000000000000000 ) ;
#40981 = ORIENTED_EDGE ( 'NONE', *, *, #44423, .F. ) ;
#40982 = CARTESIAN_POINT ( 'NONE',  ( 12.92578146920380000, -65.51322971429019049, -47.67849912756199871 ) ) ;
#40983 = CARTESIAN_POINT ( 'NONE',  ( 57.18780975371719677, -45.32813116653040453, -25.90209649327980301 ) ) ;
#40984 = CARTESIAN_POINT ( 'NONE',  ( 23.35742708719739724, -16.95913214825089810, -81.23899999999999011 ) ) ;
#40985 = ADVANCED_FACE ( 'NONE', ( #46843 ), #44040, .T. ) ;
#40986 = CARTESIAN_POINT ( 'NONE',  ( 61.60447260105160439, 13.96386167667579947, -46.92884096198559263 ) ) ;
#40987 = LINE ( 'NONE', #13990, #14224 ) ;
#40988 = VERTEX_POINT ( 'NONE', #51015 ) ;
#40989 = EDGE_LOOP ( 'NONE', ( #11288, #10622, #3692, #30779, #28179 ) ) ;
#40990 = DIRECTION ( 'NONE',  ( 0.3805321250008310008, 0.000000000000000000, -0.9247677015566404535 ) ) ;
#40991 = ORIENTED_EDGE ( 'NONE', *, *, #19032, .T. ) ;
#40992 = CARTESIAN_POINT ( 'NONE',  ( 9.367366684597708826, -15.61630833865650025, -41.84717978380999170 ) ) ;
#40993 = CARTESIAN_POINT ( 'NONE',  ( 23.24415347406168308, -19.18663440281774157, -33.94030009962079930 ) ) ;
#40994 = CARTESIAN_POINT ( 'NONE',  ( 14.13393739769619906, -32.62399965035220362, -35.14999999999999858 ) ) ;
#40995 = ORIENTED_EDGE ( 'NONE', *, *, #47384, .F. ) ;
#40996 = ORIENTED_EDGE ( 'NONE', *, *, #16744, .T. ) ;
#40997 = CARTESIAN_POINT ( 'NONE',  ( 9.894687805641289913, 22.37488585622680048, -34.64999999999999858 ) ) ;
#40998 = CARTESIAN_POINT ( 'NONE',  ( 47.04949829066929823, -54.45405841347059805, -75.29717685666371096 ) ) ;
#40999 = LINE ( 'NONE', #37328, #3607 ) ;
#41000 = ADVANCED_FACE ( 'NONE', ( #39484 ), #3582, .T. ) ;
#41001 = CARTESIAN_POINT ( 'NONE',  ( 23.06214062797170072, -3.616188944679349593, -24.15000000000000213 ) ) ;
#41002 = CARTESIAN_POINT ( 'NONE',  ( 13.00893796619580023, 34.28605843179359880, -23.32157451048000141 ) ) ;
#41003 = CARTESIAN_POINT ( 'NONE',  ( -11.32734370190460105, 10.64934056395049922, -6.430192534648650593 ) ) ;
#41004 = AXIS2_PLACEMENT_3D ( 'NONE', #45512, #21629, #37634 ) ;
#41005 = VECTOR ( 'NONE', #49516, 1000.000000000000000 ) ;
#41006 = AXIS2_PLACEMENT_3D ( 'NONE', #49689, #25288, #17196 ) ;
#41007 = CARTESIAN_POINT ( 'NONE',  ( 11.34401365722481536, 24.09645396166900611, -21.54733585199151236 ) ) ;
#41008 = CARTESIAN_POINT ( 'NONE',  ( 37.63393739769620083, -15.61618894467929941, -11.65000000000000036 ) ) ;
#41009 = CIRCLE ( 'NONE', #25085, 30.99999999999999645 ) ;
#41010 = CARTESIAN_POINT ( 'NONE',  ( 18.97802158468009992, -8.301960802179829457, -70.90555118064968099 ) ) ;
#41011 = B_SPLINE_SURFACE_WITH_KNOTS ( 'NONE', 3, 3, ( 
 ( #34999, #51267, #51004, #11178, #27145, #15362, #19540, #51521, #47594, #24213 ),
 ( #20552, #25262, #32339, #4850, #21077, #48101, #21334, #37080, #40237, #1177 ),
 ( #17173, #24475, #12452, #41268, #37339, #4328, #32595, #20297, #48358, #12990 ),
 ( #48886, #40487, #5124, #36285, #36810, #28941, #44945, #28422, #12200, #33125 ),
 ( #4579, #24736, #8785, #9318, #9046, #16121, #49153, #32082, #13249, #36548 ) ),
 .UNSPECIFIED., .F., .F., .F.,
 ( 4, 1, 4 ),
 ( 4, 2, 2, 2, 4 ),
 ( 0.000000000000000000, 0.5000000000000000000, 1.000000000000000000 ),
 ( -5.804775000000000375E-14, 0.9800148840114050186, 2.548038698429749616, 5.056876801499090135, 7.840119072091650487 ),
 .UNSPECIFIED. ) ;
#41012 = ORIENTED_EDGE ( 'NONE', *, *, #20030, .F. ) ;
#41013 = CARTESIAN_POINT ( 'NONE',  ( -11.32756203325930144, -41.88149018212450159, -6.430250179200330152 ) ) ;
#41014 = CARTESIAN_POINT ( 'NONE',  ( 12.45971295116610023, 34.17435175702340189, -46.68166270206700119 ) ) ;
#41015 = CARTESIAN_POINT ( 'NONE',  ( 72.79374086912940811, 1.313759828078489900, -69.15881847709009378 ) ) ;
#41016 = CARTESIAN_POINT ( 'NONE',  ( 23.04645056301411543, -11.63203867424703120, -43.34097441868176048 ) ) ;
#41017 = CARTESIAN_POINT ( 'NONE',  ( 47.10255859972780712, 23.39255633749860053, -75.00952388492770240 ) ) ;
#41018 = CARTESIAN_POINT ( 'NONE',  ( 49.45469051709810060, -53.54401829445560423, -54.26811687044310162 ) ) ;
#41019 = CARTESIAN_POINT ( 'NONE',  ( 41.66707677620669870, -44.64833008590599661, -5.278831885195840457 ) ) ;
#41020 = CARTESIAN_POINT ( 'NONE',  ( 16.33480707122532394, -23.55604788584398079, -33.99953662611090976 ) ) ;
#41021 = CARTESIAN_POINT ( 'NONE',  ( 14.30191975431818818, -32.45848243737157901, -34.77490583097449672 ) ) ;
#41022 = DIRECTION ( 'NONE',  ( 0.000000000000000000, 1.000000000000000000, 0.000000000000000000 ) ) ;
#41023 = ORIENTED_EDGE ( 'NONE', *, *, #28206, .T. ) ;
#41024 = CARTESIAN_POINT ( 'NONE',  ( 22.56719568149739885, -11.85854577478619909, -40.89907019807789368 ) ) ;
#41025 = CARTESIAN_POINT ( 'NONE',  ( 64.58432100436870371, 1.316034553465939894, -61.01355869227559481 ) ) ;
#41026 = ORIENTED_EDGE ( 'NONE', *, *, #39971, .T. ) ;
#41027 = CARTESIAN_POINT ( 'NONE',  ( 54.71776772591253035, -45.61739577595168527, -15.43675199817832500 ) ) ;
#41028 = CARTESIAN_POINT ( 'NONE',  ( 60.61561495333980076, -45.70472510158130319, -47.62765810040219350 ) ) ;
#41029 = DIRECTION ( 'NONE',  ( 0.000000000000000000, 0.000000000000000000, -1.000000000000000000 ) ) ;
#41030 = DIRECTION ( 'NONE',  ( 0.8545454545454508333, 0.000000000000000000, 0.5193766129849408664 ) ) ;
#41032 = CARTESIAN_POINT ( 'NONE',  ( 32.63393739769630031, -15.61618894467929941, -6.649999999999999467 ) ) ;
#41031 = CARTESIAN_POINT ( 'NONE',  ( 45.04234838772278948, 8.801119246186837941, -61.60717924809139845 ) ) ;
#41033 = DIRECTION ( 'NONE',  ( -0.8660254037844387076, 0.4999999999999998890, 0.000000000000000000 ) ) ;
#41034 = CARTESIAN_POINT ( 'NONE',  ( 15.09839649219260593, -23.52718973776712375, -52.04933381677249571 ) ) ;
#41035 = ORIENTED_EDGE ( 'NONE', *, *, #10791, .T. ) ;
#41036 = CARTESIAN_POINT ( 'NONE',  ( 83.86237639949339950, -44.73853788847340240, -47.35515635286719771 ) ) ;
#41037 = VERTEX_POINT ( 'NONE', #38714 ) ;
#41038 = EDGE_CURVE ( 'NONE', #37399, #49444, #39013, .T. ) ;
#41039 = ORIENTED_EDGE ( 'NONE', *, *, #13740, .F. ) ;
#41040 = EDGE_LOOP ( 'NONE', ( #17245, #45495, #34532, #24568 ) ) ;
#41041 = CARTESIAN_POINT ( 'NONE',  ( 61.50451778728459828, -45.34291071716570087, -47.29822066312470241 ) ) ;
#41042 = VECTOR ( 'NONE', #41511, 1000.000000000000000 ) ;
#41043 = CARTESIAN_POINT ( 'NONE',  ( 14.06328890421924882, -7.911080998336773362, -79.20899914491724303 ) ) ;
#41044 = AXIS2_PLACEMENT_3D ( 'NONE', #43224, #47665, #8085 ) ;
#41045 = CARTESIAN_POINT ( 'NONE',  ( 76.39434454947775066, -13.53395835587781626, -12.77213375745345481 ) ) ;
#41046 = DIRECTION ( 'NONE',  ( -0.9304380493636928984, 0.3664492274467039401, 0.000000000000000000 ) ) ;
#41047 = AXIS2_PLACEMENT_3D ( 'NONE', #2370, #38542, #6313 ) ;
#41048 = ORIENTED_EDGE ( 'NONE', *, *, #14378, .T. ) ;
#41049 = ORIENTED_EDGE ( 'NONE', *, *, #10779, .T. ) ;
#41050 = CIRCLE ( 'NONE', #4235, 5.251829701412241924 ) ;
#41051 = VECTOR ( 'NONE', #28139, 999.9999999999998863 ) ;
#41052 = FACE_OUTER_BOUND ( 'NONE', #49248, .T. ) ;
#41053 = CARTESIAN_POINT ( 'NONE',  ( 56.52293937402539825, 19.39991365250580202, -53.14906066056489919 ) ) ;
#41054 = LINE ( 'NONE', #5166, #6188 ) ;
#41055 = CARTESIAN_POINT ( 'NONE',  ( 29.13393739769619728, 1.883811055320659955, -81.65000000000000568 ) ) ;
#41056 = CARTESIAN_POINT ( 'NONE',  ( 17.90524532213879993, -9.025332794473378328, -36.03615195047114383 ) ) ;
#41057 = LINE ( 'NONE', #20343, #35979 ) ;
#41058 = ORIENTED_EDGE ( 'NONE', *, *, #14370, .T. ) ;
#41059 = B_SPLINE_CURVE_WITH_KNOTS ( 'NONE', 3,
 ( #45085, #46398, #50573, #22250, #6813, #30373, #34043, #14147 ),
 .UNSPECIFIED., .F., .F.,
 ( 4, 2, 2, 4 ),
 ( 0.5000003605123823913, 0.6250000000001332268, 0.8250000000000607958, 1.000000000000000000 ),
 .UNSPECIFIED. ) ;
#41060 = DIRECTION ( 'NONE',  ( 0.000000000000000000, 0.000000000000000000, 1.000000000000000000 ) ) ;
#41061 = CARTESIAN_POINT ( 'NONE',  ( 52.91674793875649385, -50.26601136226660316, -77.24667101312410011 ) ) ;
#41062 = FACE_OUTER_BOUND ( 'NONE', #9033, .T. ) ;
#41063 = CARTESIAN_POINT ( 'NONE',  ( 60.31436991762949873, 14.50714379426369938, -47.22798074803809953 ) ) ;
#41064 = CARTESIAN_POINT ( 'NONE',  ( 14.82090148184650147, -23.35328686801410214, -66.56600386269050773 ) ) ;
#41065 = EDGE_CURVE ( 'NONE', #49152, #27637, #14196, .T. ) ;
#41066 = DIRECTION ( 'NONE',  ( -0.000000000000000000, 1.000000000000000000, 0.000000000000000000 ) ) ;
#41067 = CARTESIAN_POINT ( 'NONE',  ( -10.56362341667716187, -35.01310227033097533, -54.64999999999999858 ) ) ;
#41068 = EDGE_CURVE ( 'NONE', #27066, #51151, #11962, .T. ) ;
#41069 = CARTESIAN_POINT ( 'NONE',  ( 42.70036219403750266, -44.15320494937070350, -5.071714815372149410 ) ) ;
#41070 = CARTESIAN_POINT ( 'NONE',  ( 69.22748654599971019, -50.70395984888047991, -72.15645085170115181 ) ) ;
#41071 = CARTESIAN_POINT ( 'NONE',  ( 67.77185291767722219, 1.249071374518028188, -19.08055332124363446 ) ) ;
#41072 = CARTESIAN_POINT ( 'NONE',  ( 64.11017304249050142, 1.191621070196819954, -70.06340612986369365 ) ) ;
#41073 = CARTESIAN_POINT ( 'NONE',  ( 17.36723149245495179, -52.99263552516109854, -76.14999999999999147 ) ) ;
#41074 = CARTESIAN_POINT ( 'NONE',  ( 67.77844493121459379, 0.7065659173237569535, -18.45139661994250346 ) ) ;
#41075 = ORIENTED_EDGE ( 'NONE', *, *, #42242, .F. ) ;
#41076 = CARTESIAN_POINT ( 'NONE',  ( 14.12318226124150122, -51.80504026018019914, -75.54815173289030383 ) ) ;
#41077 = CARTESIAN_POINT ( 'NONE',  ( 57.25380934771570196, 19.38381105532069881, -53.86267014602349690 ) ) ;
#41078 = CARTESIAN_POINT ( 'NONE',  ( 18.38332385620206111, 20.94377882893676102, -75.56421372420827254 ) ) ;
#41079 = DIRECTION ( 'NONE',  ( 0.000000000000000000, 0.000000000000000000, -1.000000000000000000 ) ) ;
#41080 = CARTESIAN_POINT ( 'NONE',  ( 24.00223188529327345, -14.76797646811701803, -55.47349681351633421 ) ) ;
#41081 = AXIS2_PLACEMENT_3D ( 'NONE', #41536, #32608, #37600 ) ;
#41082 = CARTESIAN_POINT ( 'NONE',  ( 22.73493107740300090, -13.03252716129409983, -32.14999999999999858 ) ) ;
#41084 = AXIS2_PLACEMENT_3D ( 'NONE', #26937, #46883, #27447 ) ;
#41083 = CARTESIAN_POINT ( 'NONE',  ( 55.29972780508609986, -46.05201784173636526, -16.43382449896097697 ) ) ;
#41085 = CARTESIAN_POINT ( 'NONE',  ( 47.75981413591419766, -54.46820368462779527, -54.94005077776210300 ) ) ;
#41087 = CARTESIAN_POINT ( 'NONE',  ( -9.066986571212598989, -44.13582524313829936, -5.880785460427049749 ) ) ;
#41086 = CARTESIAN_POINT ( 'NONE',  ( 13.89738755482740018, 19.98851976907650041, -22.99807273771689964 ) ) ;
#41088 = CARTESIAN_POINT ( 'NONE',  ( 56.46191916141020073, 19.54532074681500120, -53.81431225014880226 ) ) ;
#41089 = CARTESIAN_POINT ( 'NONE',  ( 42.70036219816795153, 12.92082705528767583, -5.071714813363838559 ) ) ;
#41090 = CARTESIAN_POINT ( 'NONE',  ( 48.78347455189079795, 22.74609578351320138, -54.78766944749870049 ) ) ;
#41091 = ORIENTED_EDGE ( 'NONE', *, *, #34292, .F. ) ;
#41092 = CARTESIAN_POINT ( 'NONE',  ( 22.03527629823739886, -11.75396699929470046, -66.66271668429399710 ) ) ;
#41093 = ORIENTED_EDGE ( 'NONE', *, *, #10880, .F. ) ;
#41094 = FACE_OUTER_BOUND ( 'NONE', #20211, .T. ) ;
#41095 = CARTESIAN_POINT ( 'NONE',  ( 65.09597585808539577, 1.387131204727280132, -61.00757424182599920 ) ) ;
#41096 = DIRECTION ( 'NONE',  ( 1.000000000000000000, 2.460964292799963328E-14, 0.000000000000000000 ) ) ;
#41098 = CARTESIAN_POINT ( 'NONE',  ( 52.66668290531129770, 18.52378580962789911, -27.74344827129370117 ) ) ;
#41097 = CARTESIAN_POINT ( 'NONE',  ( 84.44784216359251161, 11.88381105532070059, -47.47585302082339354 ) ) ;
#41099 = CARTESIAN_POINT ( 'NONE',  ( 22.83553112445549971, -13.41818980498730163, -60.35193945864850207 ) ) ;
#41100 = CARTESIAN_POINT ( 'NONE',  ( 12.86517331568640010, -49.11618894467930829, -34.64999999999999858 ) ) ;
#41101 = CARTESIAN_POINT ( 'NONE',  ( 16.13393739769639623, 7.383811055320659733, -84.65000000000000568 ) ) ;
#41102 = CARTESIAN_POINT ( 'NONE',  ( 8.428884788794746896, -17.68704093276265965, -80.70899836890637857 ) ) ;
#41103 = EDGE_LOOP ( 'NONE', ( #4849, #17900, #43876, #18482, #19255, #22786, #13197, #42909, #27128 ) ) ;
#41104 = EDGE_CURVE ( 'NONE', #5682, #43692, #7980, .T. ) ;
#41105 = ORIENTED_EDGE ( 'NONE', *, *, #48464, .F. ) ;
#41106 = CARTESIAN_POINT ( 'NONE',  ( 11.59391792476989913, -64.95860477368741215, -16.50763286606999714 ) ) ;
#41107 = CARTESIAN_POINT ( 'NONE',  ( 11.65647435635129980, 33.66779149316020181, -45.60641158798500072 ) ) ;
#41108 = LINE ( 'NONE', #5218, #23997 ) ;
#41109 = CARTESIAN_POINT ( 'NONE',  ( 47.69072379162619768, -54.40457714162659641, -54.20239749881680069 ) ) ;
#41110 = CARTESIAN_POINT ( 'NONE',  ( -31.36606260230380272, -62.11618894467930119, 11.84999999999999964 ) ) ;
#41111 = VERTEX_POINT ( 'NONE', #40498 ) ;
#41112 = CARTESIAN_POINT ( 'NONE',  ( 10.67151123448148375, 24.00903292272008827, -45.35245340590078200 ) ) ;
#41113 = DIRECTION ( 'NONE',  ( 0.000000000000000000, -1.000000000000000000, 0.000000000000000000 ) ) ;
#41114 = CARTESIAN_POINT ( 'NONE',  ( 9.807761426623416767, -20.47785318488935857, -60.29935320495772544 ) ) ;
#41115 = LINE ( 'NONE', #29307, #42601 ) ;
#41116 = CARTESIAN_POINT ( 'NONE',  ( 63.44650199127489998, 1.383928098097870096, -62.75238677440889035 ) ) ;
#41117 = CARTESIAN_POINT ( 'NONE',  ( 22.35126475695570036, -53.65744759104629935, -34.65028073423250277 ) ) ;
#41118 =( BOUNDED_CURVE ( )  B_SPLINE_CURVE ( 3, ( #15454, #36127, #232, #48187 ),
 .UNSPECIFIED., .F., .T. ) 
 B_SPLINE_CURVE_WITH_KNOTS ( ( 4, 4 ),
 ( 0.000000000000000000, 0.8959462480744248003 ),
 .UNSPECIFIED. ) 
 CURVE ( )  GEOMETRIC_REPRESENTATION_ITEM ( )  RATIONAL_B_SPLINE_CURVE ( ( 1.000000000000000000, 0.9342179155434778837, 0.9342179155434778837, 1.000000000000000000 ) ) 
 REPRESENTATION_ITEM ( '' )  );
#41119 = ORIENTED_EDGE ( 'NONE', *, *, #24530, .F. ) ;
#41120 = CARTESIAN_POINT ( 'NONE',  ( 55.91595722987329964, -45.90465052577939531, -25.32543029193989881 ) ) ;
#41122 = FACE_OUTER_BOUND ( 'NONE', #2935, .T. ) ;
#41121 = VECTOR ( 'NONE', #13923, 1000.000000000000227 ) ;
#41123 = ORIENTED_EDGE ( 'NONE', *, *, #38966, .T. ) ;
#41124 = CARTESIAN_POINT ( 'NONE',  ( 12.64094934536730364, -55.46337509643738173, -75.46694760811912772 ) ) ;
#41125 = LINE ( 'NONE', #29819, #35346 ) ;
#41126 = AXIS2_PLACEMENT_3D ( 'NONE', #2120, #22535, #22790 ) ;
#41127 = CARTESIAN_POINT ( 'NONE',  ( 18.52227178108019601, -8.140722163069080253, -33.61092854022489718 ) ) ;
#41128 = CARTESIAN_POINT ( 'NONE',  ( 55.90673615822279885, 19.65302146644049941, -74.84519705601209694 ) ) ;
#41129 = EDGE_CURVE ( 'NONE', #21618, #42976, #36558, .T. ) ;
#41130 = CARTESIAN_POINT ( 'NONE',  ( 47.32558733251070038, -54.23003007210349580, -75.35929005681119008 ) ) ;
#41131 = ORIENTED_EDGE ( 'NONE', *, *, #13717, .F. ) ;
#41132 = CARTESIAN_POINT ( 'NONE',  ( 55.99603443303359285, 14.48522708022579941, -17.30520569459709890 ) ) ;
#41133 = CARTESIAN_POINT ( 'NONE',  ( 57.27159525777589977, -50.25201018848400025, -52.75109249795529109 ) ) ;
#41134 = CARTESIAN_POINT ( 'NONE',  ( 20.51938203757270074, -21.13981406646960082, -35.13358212097359257 ) ) ;
#41135 = CARTESIAN_POINT ( 'NONE',  ( -0.007164427059776000244, -22.82436266295209748, -34.77269723891829756 ) ) ;
#41136 = CARTESIAN_POINT ( 'NONE',  ( 47.09676272639270422, 22.96834012079289877, -75.51614565245159838 ) ) ;
#41137 = CARTESIAN_POINT ( 'NONE',  ( 65.23737843152770211, 1.383411777981069957, -60.92458877361669778 ) ) ;
#41138 = DIRECTION ( 'NONE',  ( 1.000000000000000000, 0.000000000000000000, 0.000000000000000000 ) ) ;
#41139 = CARTESIAN_POINT ( 'NONE',  ( 12.36320305067610015, 33.31445045643330616, -15.76422791930239953 ) ) ;
#41140 = CARTESIAN_POINT ( 'NONE',  ( 30.13393739769619728, -38.61618894467930119, -59.64999999999999147 ) ) ;
#41141 = FACE_OUTER_BOUND ( 'NONE', #28975, .T. ) ;
#41143 = DIRECTION ( 'NONE',  ( 0.9083627212242632032, 0.3704194192529746688, -0.1940789028471167077 ) ) ;
#41142 = CARTESIAN_POINT ( 'NONE',  ( 64.77932207159139466, 0.8936201581567920771, -60.67538646459720297 ) ) ;
#41144 = DIRECTION ( 'NONE',  ( 0.000000000000000000, 0.000000000000000000, -1.000000000000000000 ) ) ;
#41145 = CARTESIAN_POINT ( 'NONE',  ( -17.48391069661419905, -50.96347608314179922, -52.50953498851679768 ) ) ;
#41146 = ORIENTED_EDGE ( 'NONE', *, *, #33117, .T. ) ;
#41147 = VECTOR ( 'NONE', #32103, 1000.000000000000000 ) ;
#41148 = CARTESIAN_POINT ( 'NONE',  ( 53.13753028352629570, -49.50378124343389885, -48.89206903948300464 ) ) ;
#41149 = AXIS2_PLACEMENT_3D ( 'NONE', #30198, #38862, #2174 ) ;
#41150 = CARTESIAN_POINT ( 'NONE',  ( 61.64818500071270080, -45.11839462663610334, -27.88144317553240015 ) ) ;
#41151 = CARTESIAN_POINT ( 'NONE',  ( 63.88393739769619373, 11.88381105532070059, -61.44999999999999574 ) ) ;
#41152 = CARTESIAN_POINT ( 'NONE',  ( 57.39314836427140420, 14.50720453784729891, -26.25563593084900305 ) ) ;
#41153 = VECTOR ( 'NONE', #8830, 1000.000000000000000 ) ;
#41154 = CARTESIAN_POINT ( 'NONE',  ( 22.43485972733980205, -19.59174867206459680, -80.41182290828409407 ) ) ;
#41155 = CARTESIAN_POINT ( 'NONE',  ( 51.18091049923660307, 19.51488979195089968, -76.16568857009508520 ) ) ;
#41156 = CARTESIAN_POINT ( 'NONE',  ( 53.20332254885359902, 18.25314851316870346, -48.99213401679070046 ) ) ;
#41157 = CARTESIAN_POINT ( 'NONE',  ( 71.26764986431300031, 0.9952464559119579279, -70.75693755662150863 ) ) ;
#41158 = CARTESIAN_POINT ( 'NONE',  ( 16.13393739769620083, -15.61618894467929941, -21.14999999999999858 ) ) ;
#41159 = CARTESIAN_POINT ( 'NONE',  ( 69.10082108401860523, -43.71177200353350401, -11.63456562794259952 ) ) ;
#41160 = ORIENTED_EDGE ( 'NONE', *, *, #33913, .F. ) ;
#41161 = ADVANCED_FACE ( 'NONE', ( #28688 ), #32866, .F. ) ;
#41162 = CARTESIAN_POINT ( 'NONE',  ( 21.18999090978099886, -10.14416763429719914, -74.80477269330700096 ) ) ;
#41163 = VERTEX_POINT ( 'NONE', #28433 ) ;
#41164 = EDGE_CURVE ( 'NONE', #29628, #6450, #51569, .T. ) ;
#41165 = CARTESIAN_POINT ( 'NONE',  ( 73.08672326322148649, 0.8966068345641440285, -69.03681046574699565 ) ) ;
#41166 = CARTESIAN_POINT ( 'NONE',  ( 47.46364465723310389, -54.60385569402070161, -54.65913311076389647 ) ) ;
#41167 = CARTESIAN_POINT ( 'NONE',  ( -2.623662905535780077, 17.43154064245049994, -4.296538310234220504 ) ) ;
#41168 = CARTESIAN_POINT ( 'NONE',  ( 73.15966969277990017, 1.196343736543249880, -62.56767596405429543 ) ) ;
#41169 = CARTESIAN_POINT ( 'NONE',  ( 56.75852129267509838, 18.90901482631310060, -52.43727812511399833 ) ) ;
#41171 = EDGE_CURVE ( 'NONE', #12686, #40179, #16393, .T. ) ;
#41170 = CARTESIAN_POINT ( 'NONE',  ( 71.62484648860569791, 0.9098571636355680115, -60.77008670988870165 ) ) ;
#41172 = CARTESIAN_POINT ( 'NONE',  ( 2.470463535281269607, -25.59369663964760377, -34.75586992539665232 ) ) ;
#41173 = CARTESIAN_POINT ( 'NONE',  ( 72.03321845393109868, 1.179532368575649803, -61.12950465565599956 ) ) ;
#41174 = DIRECTION ( 'NONE',  ( 0.000000000000000000, 0.000000000000000000, -1.000000000000000000 ) ) ;
#41175 = ADVANCED_FACE ( 'NONE', ( #43668 ), #36823, .T. ) ;
#41176 = ORIENTED_EDGE ( 'NONE', *, *, #21264, .F. ) ;
#41177 = CARTESIAN_POINT ( 'NONE',  ( 65.17800597998869705, 1.373356196620459935, -70.43126475061649217 ) ) ;
#41178 = EDGE_LOOP ( 'NONE', ( #33422, #33677, #50851, #1161 ) ) ;
#41179 = ORIENTED_EDGE ( 'NONE', *, *, #44975, .T. ) ;
#41180 = CARTESIAN_POINT ( 'NONE',  ( 13.68997055320560108, -51.35827251201860122, -23.13969638325859890 ) ) ;
#41181 = CARTESIAN_POINT ( 'NONE',  ( 15.05440318628110141, 21.88381105532300097, -76.14999999999999147 ) ) ;
#41182 = ORIENTED_EDGE ( 'NONE', *, *, #15945, .T. ) ;
#41183 = DIRECTION ( 'NONE',  ( 0.7071067811865473507, 0.7071067811865476838, 0.000000000000000000 ) ) ;
#41184 = LINE ( 'NONE', #41435, #41954 ) ;
#41185 = DIRECTION ( 'NONE',  ( 0.4640893551880597712, 0.8857883891771956009, 0.000000000000000000 ) ) ;
#41186 = CARTESIAN_POINT ( 'NONE',  ( 53.33359353556529925, 19.40928134151669937, -76.65020911032560491 ) ) ;
#41187 = ORIENTED_EDGE ( 'NONE', *, *, #50209, .T. ) ;
#41188 = FACE_OUTER_BOUND ( 'NONE', #26542, .T. ) ;
#41189 = DIRECTION ( 'NONE',  ( 1.000000000000000000, 0.000000000000000000, 0.000000000000000000 ) ) ;
#41190 = CARTESIAN_POINT ( 'NONE',  ( 50.03007040746459921, 17.38381105532069881, -76.14999999999999147 ) ) ;
#41191 = CARTESIAN_POINT ( 'NONE',  ( 10.67428282541060192, -21.79477227803790029, -56.52269350815079463 ) ) ;
#41192 = CARTESIAN_POINT ( 'NONE',  ( 35.88493617910660305, 12.02948893129472019, -35.12503119152809461 ) ) ;
#41193 = CARTESIAN_POINT ( 'NONE',  ( 41.91508555065757946, -37.61000887859182029, -80.74419515902299338 ) ) ;
#41194 = EDGE_CURVE ( 'NONE', #19736, #14545, #23968, .T. ) ;
#41195 = EDGE_LOOP ( 'NONE', ( #19363, #41405, #324, #45111, #48075, #45297 ) ) ;
#41196 = FACE_OUTER_BOUND ( 'NONE', #2701, .T. ) ;
#41197 = CARTESIAN_POINT ( 'NONE',  ( 9.992168748469609341, -19.83345958628190076, -49.04112620709079806 ) ) ;
#41198 = VECTOR ( 'NONE', #20580, 1000.000000000000000 ) ;
#41199 = CIRCLE ( 'NONE', #18591, 6.000000000000000000 ) ;
#41200 = CARTESIAN_POINT ( 'NONE',  ( 18.20456740063047008, -7.911074884095184778, -33.09099907805137519 ) ) ;
#41201 = CARTESIAN_POINT ( 'NONE',  ( 14.24699128871759868, 20.74698410172580054, -75.72128529899769944 ) ) ;
#41202 = CARTESIAN_POINT ( 'NONE',  ( 51.95831930592699877, 18.21933529978510080, -77.09973198023169516 ) ) ;
#41203 = CARTESIAN_POINT ( 'NONE',  ( 82.49223220840650583, -45.10152342427350192, -46.59234684980519603 ) ) ;
#41204 = ADVANCED_FACE ( 'NONE', ( #51783 ), #20564, .F. ) ;
#41205 = CARTESIAN_POINT ( 'NONE',  ( 10.05407090363459943, -21.18556450423380255, -52.27160849015929500 ) ) ;
#41206 = EDGE_LOOP ( 'NONE', ( #4792, #49737, #44403, #32452 ) ) ;
#41207 = CARTESIAN_POINT ( 'NONE',  ( 55.95580649448950084, -45.88747549310949836, -25.57469933290609987 ) ) ;
#41208 = CARTESIAN_POINT ( 'NONE',  ( 54.43935813201120055, -51.17211618503599624, -75.39236096530039788 ) ) ;
#41209 = CYLINDRICAL_SURFACE ( 'NONE', #29070, 6.766999999999998572 ) ;
#41210 = DIRECTION ( 'NONE',  ( -0.6911981449639438280, -0.7226652920947587155, -3.885780586188048385E-16 ) ) ;
#41211 = DIRECTION ( 'NONE',  ( -0.5720614028176839172, 0.4156269377774525209, -0.7071067811865484609 ) ) ;
#41212 = ORIENTED_EDGE ( 'NONE', *, *, #14001, .T. ) ;
#41213 = CARTESIAN_POINT ( 'NONE',  ( -5.658245767086419242, -46.75968762783350030, -4.712742916676430305 ) ) ;
#41214 = CARTESIAN_POINT ( 'NONE',  ( 47.29521656555830589, 23.49172283449389909, -54.72089720754819808 ) ) ;
#41215 = CARTESIAN_POINT ( 'NONE',  ( 22.13834065091180037, 22.90954413163309766, -35.04035092416999220 ) ) ;
#41216 = CARTESIAN_POINT ( 'NONE',  ( 63.30180592418049912, 1.263738073398960049, -62.36141320605320004 ) ) ;
#41217 = CARTESIAN_POINT ( 'NONE',  ( 57.31533492135169894, -50.46532389091750304, -53.15033574623170409 ) ) ;
#41218 = CARTESIAN_POINT ( 'NONE',  ( 11.79333626495519916, 34.19002346076609911, -17.82631612918970276 ) ) ;
#41219 = CARTESIAN_POINT ( 'NONE',  ( 38.67452568954060155, -37.56081407618430035, -81.65000000000000568 ) ) ;
#41220 = DIRECTION ( 'NONE',  ( 0.6339889056055382222, 0.000000000000000000, -0.7733421413379021336 ) ) ;
#41221 = DIRECTION ( 'NONE',  ( -1.000000000000000000, 0.000000000000000000, 0.000000000000000000 ) ) ;
#41222 = CARTESIAN_POINT ( 'NONE',  ( 57.05080397350140231, -47.54530775247659591, -48.23310989717779762 ) ) ;
#41223 = CARTESIAN_POINT ( 'NONE',  ( 16.13393739769620083, -15.61618894467929941, -6.721843382729280059 ) ) ;
#41224 = CARTESIAN_POINT ( 'NONE',  ( 52.32346883964469697, 21.19168061802760050, -53.80955079009429909 ) ) ;
#41225 = CONICAL_SURFACE ( 'NONE', #6073, 12.92820323027549989, 0.7481802937784480800 ) ;
#41226 = CARTESIAN_POINT ( 'NONE',  ( 63.27581436415109550, 1.132579237369250036, -69.08822821206570097 ) ) ;
#41227 = CARTESIAN_POINT ( 'NONE',  ( 11.97534830454654298, -10.20480668565649118, -47.74448746576103986 ) ) ;
#41228 = VERTEX_POINT ( 'NONE', #16925 ) ;
#41229 = CARTESIAN_POINT ( 'NONE',  ( 16.13393739769620083, -15.61618894467929941, -28.45282021618999835 ) ) ;
#41230 = CARTESIAN_POINT ( 'NONE',  ( 9.744550898871700895, 32.05767636941019560, -46.29747639044499863 ) ) ;
#41231 = AXIS2_PLACEMENT_3D ( 'NONE', #11812, #28276, #20410 ) ;
#41232 = CARTESIAN_POINT ( 'NONE',  ( 31.37998729184774405, -15.61618894467929941, -7.101316701949489385 ) ) ;
#41233 = CARTESIAN_POINT ( 'NONE',  ( 14.64227698520870113, -7.857630305424530448, -81.23899999999999011 ) ) ;
#41234 = EDGE_CURVE ( 'NONE', #37257, #6515, #46704, .T. ) ;
#41235 = EDGE_LOOP ( 'NONE', ( #30729, #29536, #31092, #40778 ) ) ;
#41236 = CARTESIAN_POINT ( 'NONE',  ( 18.14361831065170350, 20.57417486552859742, -75.54540032568610286 ) ) ;
#41237 = VERTEX_POINT ( 'NONE', #21864 ) ;
#41238 = VERTEX_POINT ( 'NONE', #22120 ) ;
#41239 = CARTESIAN_POINT ( 'NONE',  ( 16.13393739769620083, -15.61618894467929941, -34.64999999999999858 ) ) ;
#41240 = ORIENTED_EDGE ( 'NONE', *, *, #43172, .F. ) ;
#41241 = CARTESIAN_POINT ( 'NONE',  ( 11.56804367855430016, -65.08699574139150457, -46.73148076027570141 ) ) ;
#41242 = CARTESIAN_POINT ( 'NONE',  ( 56.34549632421120435, -45.90303496147449636, -26.05542634681239988 ) ) ;
#41243 = CARTESIAN_POINT ( 'NONE',  ( 20.58428850091829787, -20.97262704213749984, -81.23899999999999011 ) ) ;
#41244 = CARTESIAN_POINT ( 'NONE',  ( 44.13393739769620083, 1.883811055320659955, -54.35294145922169662 ) ) ;
#41245 = CARTESIAN_POINT ( 'NONE',  ( 61.64879318626500293, 13.92293292261859960, -46.76047835613849202 ) ) ;
#41246 = CARTESIAN_POINT ( 'NONE',  ( 16.13393739769620083, -15.61618894467929941, -14.68999999999999950 ) ) ;
#41247 = ORIENTED_EDGE ( 'NONE', *, *, #31602, .F. ) ;
#41248 = CARTESIAN_POINT ( 'NONE',  ( 22.83067611733696722, -17.21599180179194022, -68.92243437301439712 ) ) ;
#41249 = ORIENTED_EDGE ( 'NONE', *, *, #16219, .F. ) ;
#41250 = CARTESIAN_POINT ( 'NONE',  ( 50.81623145755629878, -45.20523958689630462, -11.75436512841420011 ) ) ;
#41251 = AXIS2_PLACEMENT_3D ( 'NONE', #37493, #13654, #49307 ) ;
#41252 = DIRECTION ( 'NONE',  ( 0.000000000000000000, 0.000000000000000000, -1.000000000000000000 ) ) ;
#41253 = FACE_OUTER_BOUND ( 'NONE', #42409, .T. ) ;
#41254 = ORIENTED_EDGE ( 'NONE', *, *, #46241, .T. ) ;
#41255 = LINE ( 'NONE', #5366, #29991 ) ;
#41256 = CARTESIAN_POINT ( 'NONE',  ( 46.71028574728679672, -53.65544939505299737, -75.98322477344710535 ) ) ;
#41257 = CARTESIAN_POINT ( 'NONE',  ( 60.41031538789670208, 14.61374794153990031, -47.73939764575179368 ) ) ;
#41258 = CARTESIAN_POINT ( 'NONE',  ( 50.01275137939290261, 14.95673839075170086, -12.46590880385850042 ) ) ;
#41259 = DIRECTION ( 'NONE',  ( -0.6653150774946533508, -0.7465626883646701017, 0.000000000000000000 ) ) ;
#41260 = DIRECTION ( 'NONE',  ( 0.000000000000000000, 0.000000000000000000, -1.000000000000000000 ) ) ;
#41261 = VECTOR ( 'NONE', #7650, 1000.000000000000114 ) ;
#41262 = AXIS2_PLACEMENT_3D ( 'NONE', #22159, #11172, #6464 ) ;
#41263 = LINE ( 'NONE', #44677, #50563 ) ;
#41264 = CARTESIAN_POINT ( 'NONE',  ( 61.58984847289840303, 13.89565763300190149, -28.15139565950990175 ) ) ;
#41265 = EDGE_CURVE ( 'NONE', #29694, #15474, #31064, .T. ) ;
#41266 = CARTESIAN_POINT ( 'NONE',  ( 17.56455728119119897, -7.899967399639820087, -68.84585897299560031 ) ) ;
#41267 = VERTEX_POINT ( 'NONE', #45475 ) ;
#41269 = EDGE_CURVE ( 'NONE', #20846, #25361, #49161, .T. ) ;
#41268 = CARTESIAN_POINT ( 'NONE',  ( 58.95547274812099658, 15.24358996499610086, -47.69626354652410072 ) ) ;
#41270 = CARTESIAN_POINT ( 'NONE',  ( 22.90085274204890808, -15.61618877333890332, -76.84718755697707593 ) ) ;
#41271 = CARTESIAN_POINT ( 'NONE',  ( 46.25525774125583922, -33.99486860111965569, -54.56299356781535437 ) ) ;
#41272 = EDGE_CURVE ( 'NONE', #37879, #28243, #22251, .T. ) ;
#41273 = CARTESIAN_POINT ( 'NONE',  ( 11.28671405514150017, -65.00701117576899435, -16.86100849032779792 ) ) ;
#41274 = CARTESIAN_POINT ( 'NONE',  ( 14.06317034403552313, -7.911111693438598103, -42.92429533349460513 ) ) ;
#41275 = CARTESIAN_POINT ( 'NONE',  ( 65.05887334876689465, 1.388715606738730068, -70.28003120372629553 ) ) ;
#41276 = CARTESIAN_POINT ( 'NONE',  ( 49.24754892657740157, -53.85074344983969752, -55.23177050136099808 ) ) ;
#41277 = DIRECTION ( 'NONE',  ( 0.000000000000000000, 0.000000000000000000, -1.000000000000000000 ) ) ;
#41278 = CIRCLE ( 'NONE', #10355, 18.00000000000000000 ) ;
#41279 = CARTESIAN_POINT ( 'NONE',  ( 60.68764924188080556, -0.5980872046737689685, -16.28104295442377847 ) ) ;
#41280 = CARTESIAN_POINT ( 'NONE',  ( 18.48305433236689765, -51.32863061914290626, -74.59027663912431194 ) ) ;
#41281 = SPHERICAL_SURFACE ( 'NONE', #33169, 3.000000000000000000 ) ;
#41282 = ORIENTED_EDGE ( 'NONE', *, *, #34835, .F. ) ;
#41283 = CARTESIAN_POINT ( 'NONE',  ( 22.55572082845609927, -19.39340907418709747, -47.23658468316739345 ) ) ;
#41284 = CARTESIAN_POINT ( 'NONE',  ( 64.22068262707080066, 1.025918948572249745, -61.10071074863649443 ) ) ;
#41285 = VERTEX_POINT ( 'NONE', #29211 ) ;
#41286 = CYLINDRICAL_SURFACE ( 'NONE', #10876, 1.000000000000000888 ) ;
#41287 = CARTESIAN_POINT ( 'NONE',  ( 60.95712442611549875, -45.66700790346930461, -47.71416869798230209 ) ) ;
#41288 = DIRECTION ( 'NONE',  ( -1.000000000000000000, 0.000000000000000000, 0.000000000000000000 ) ) ;
#41289 = CARTESIAN_POINT ( 'NONE',  ( 50.90851972497010536, 19.66920513271909954, -76.14999999999999147 ) ) ;
#41291 = CARTESIAN_POINT ( 'NONE',  ( 68.13393739769624347, 0.8838110553206759423, -71.15000000000000568 ) ) ;
#41290 = CARTESIAN_POINT ( 'NONE',  ( 43.26733082018852627, 8.658673373363992454, -70.20620505724502891 ) ) ;
#41292 = CARTESIAN_POINT ( 'NONE',  ( 51.08534762786979400, -51.03566300605200468, -76.14824064460249531 ) ) ;
#41293 = DIRECTION ( 'NONE',  ( 0.000000000000000000, 0.000000000000000000, 1.000000000000000000 ) ) ;
#41294 = EDGE_CURVE ( 'NONE', #40081, #24770, #14843, .T. ) ;
#41295 = EDGE_LOOP ( 'NONE', ( #15229, #44729 ) ) ;
#41296 = ORIENTED_EDGE ( 'NONE', *, *, #5872, .F. ) ;
#41297 = EDGE_LOOP ( 'NONE', ( #51249, #11971, #20018, #35106 ) ) ;
#41298 = EDGE_LOOP ( 'NONE', ( #33934, #14178, #1465, #23292, #46380 ) ) ;
#41299 = CARTESIAN_POINT ( 'NONE',  ( 61.42101946455129990, -45.29358752071379968, -47.17308591776039606 ) ) ;
#41300 = CARTESIAN_POINT ( 'NONE',  ( 47.18324681005260146, -54.80726426785999905, -54.61059023070370699 ) ) ;
#41301 = CIRCLE ( 'NONE', #29580, 11.00000000000000000 ) ;
#41302 = CARTESIAN_POINT ( 'NONE',  ( 55.58382303305679528, -50.93169950793019751, -53.05694829722840211 ) ) ;
#41303 = AXIS2_PLACEMENT_3D ( 'NONE', #244, #13346, #8892 ) ;
#41304 = ORIENTED_EDGE ( 'NONE', *, *, #28926, .T. ) ;
#41305 = ORIENTED_EDGE ( 'NONE', *, *, #39280, .F. ) ;
#41306 = ORIENTED_EDGE ( 'NONE', *, *, #14014, .F. ) ;
#41307 = CARTESIAN_POINT ( 'NONE',  ( 20.29253929434950976, -21.02756302329809657, -72.74444564148153347 ) ) ;
#41308 = CARTESIAN_POINT ( 'NONE',  ( -3.040980549493681906, 18.38569933621215924, -37.85816068168108472 ) ) ;
#41309 = CARTESIAN_POINT ( 'NONE',  ( 9.366647546311250849, -15.61604444486649967, -65.84717978381009118 ) ) ;
#41310 = FACE_OUTER_BOUND ( 'NONE', #39954, .T. ) ;
#41311 = ORIENTED_EDGE ( 'NONE', *, *, #1215, .T. ) ;
#41312 = CARTESIAN_POINT ( 'NONE',  ( 2.457383035027194129, 23.39947848051994939, -8.319647256471711216 ) ) ;
#41313 = CARTESIAN_POINT ( 'NONE',  ( 52.81902783802529910, -50.66264935548120718, -76.50043241030529373 ) ) ;
#41314 = CARTESIAN_POINT ( 'NONE',  ( 20.93810839686982561, -20.38192891622346892, -46.70153489369711508 ) ) ;
#41315 = CARTESIAN_POINT ( 'NONE',  ( 83.95017614158776098, -44.74867211454660776, -47.46180894508327697 ) ) ;
#41316 = CARTESIAN_POINT ( 'NONE',  ( 8.474797562328269862, -17.32625460829050112, -68.94257179459920337 ) ) ;
#41317 = DIRECTION ( 'NONE',  ( 1.000000000000000000, 0.000000000000000000, 0.000000000000000000 ) ) ;
#41318 = CIRCLE ( 'NONE', #47983, 11.00000000000000000 ) ;
#41319 = CARTESIAN_POINT ( 'NONE',  ( 45.45709021471650146, 14.00253322601350092, -8.052805789834080130 ) ) ;
#41320 = CARTESIAN_POINT ( 'NONE',  ( 42.20562640647980146, -44.31827357521319755, -5.077271965990960645 ) ) ;
#41321 = DIRECTION ( 'NONE',  ( 0.000000000000000000, 0.000000000000000000, -1.000000000000000000 ) ) ;
#41322 = CARTESIAN_POINT ( 'NONE',  ( 16.13393739769620083, -15.61618894467929941, -21.14999999999999858 ) ) ;
#41323 = CARTESIAN_POINT ( 'NONE',  ( 64.22355794744891000, 1.454950765200730078, -69.87277598216670071 ) ) ;
#41324 = CARTESIAN_POINT ( 'NONE',  ( 21.90486186017893644, -19.18926943320902012, -33.02368868574395577 ) ) ;
#41325 = CARTESIAN_POINT ( 'NONE',  ( 66.55657083749090930, -1.025637880372419986, -16.96067586332220145 ) ) ;
#41326 = VERTEX_POINT ( 'NONE', #49931 ) ;
#41328 = EDGE_CURVE ( 'NONE', #33083, #39662, #36472, .T. ) ;
#41327 = CARTESIAN_POINT ( 'NONE',  ( 14.06555357016280006, -51.72389970538209525, -75.45052476223459337 ) ) ;
#41329 = CARTESIAN_POINT ( 'NONE',  ( 57.27213619417380386, 19.37967000028660181, -53.75872744438189699 ) ) ;
#41330 = EDGE_CURVE ( 'NONE', #2432, #12711, #46003, .T. ) ;
#41331 = CARTESIAN_POINT ( 'NONE',  ( 0.1457840918200039859, -10.50670027737364620, -34.68167776469301344 ) ) ;
#41332 = CIRCLE ( 'NONE', #27123, 3.500000000000003109 ) ;
#41333 = CARTESIAN_POINT ( 'NONE',  ( 16.13393739769620083, -15.61618894467929941, -54.64999999999999858 ) ) ;
#41334 = CARTESIAN_POINT ( 'NONE',  ( 23.38712508359760278, -17.09264023749170391, -32.14999999999999858 ) ) ;
#41335 = CARTESIAN_POINT ( 'NONE',  ( 54.47259832750690123, -46.25232753665150653, -15.76422791930239953 ) ) ;
#41336 = DIRECTION ( 'NONE',  ( -1.000000000000000000, 0.000000000000000000, 0.000000000000000000 ) ) ;
#41338 = CARTESIAN_POINT ( 'NONE',  ( 9.366468209001951095, -15.46638865352482561, -49.85422095549364485 ) ) ;
#41337 = DIRECTION ( 'NONE',  ( 0.000000000000000000, 0.000000000000000000, 1.000000000000000000 ) ) ;
#41339 = CARTESIAN_POINT ( 'NONE',  ( 56.44840490959330026, 19.52003022522620412, -53.50788452149080143 ) ) ;
#41340 = CARTESIAN_POINT ( 'NONE',  ( 48.66928706773219915, 22.73500733612779712, -54.62024785781569847 ) ) ;
#41341 = ORIENTED_EDGE ( 'NONE', *, *, #40116, .F. ) ;
#41342 = CARTESIAN_POINT ( 'NONE',  ( 15.64736352786460039, -8.580152770550549590, -60.32520219920449733 ) ) ;
#41343 = VERTEX_POINT ( 'NONE', #42061 ) ;
#41344 = CARTESIAN_POINT ( 'NONE',  ( 2.557755973795389881, -6.043492780141719756, -34.65000333055159842 ) ) ;
#41345 = CARTESIAN_POINT ( 'NONE',  ( 65.13185782384009315, 1.385888765344509999, -60.99577487439199786 ) ) ;
#41346 = CARTESIAN_POINT ( 'NONE',  ( 50.95182575631829991, 19.71852405838109945, -78.14999999999999147 ) ) ;
#41348 = CARTESIAN_POINT ( 'NONE',  ( 54.20264060170759990, 16.79968848045730212, -26.08911483772730122 ) ) ;
#41347 = CARTESIAN_POINT ( 'NONE',  ( 84.41763914545359171, 12.29456635737889947, -47.43918784650060161 ) ) ;
#41349 = CARTESIAN_POINT ( 'NONE',  ( 21.29521595269359935, -10.80955161965160194, -66.21414035735629966 ) ) ;
#41350 = CARTESIAN_POINT ( 'NONE',  ( 16.86121012496890259, -15.61618894467929941, -82.15000000000000568 ) ) ;
#41351 = CARTESIAN_POINT ( 'NONE',  ( 55.48947750614289731, -45.11618894467940066, -14.40595025803260043 ) ) ;
#41352 = EDGE_CURVE ( 'NONE', #26727, #24020, #33583, .T. ) ;
#41353 = DIRECTION ( 'NONE',  ( 1.260570937617230037E-11, 1.376914871200490071E-11, 1.000000000000000000 ) ) ;
#41354 = CIRCLE ( 'NONE', #51392, 0.5000000000000034417 ) ;
#41355 = VERTEX_POINT ( 'NONE', #22500 ) ;
#41356 = EDGE_CURVE ( 'NONE', #14490, #6375, #7317, .T. ) ;
#41357 = VERTEX_POINT ( 'NONE', #3391 ) ;
#41358 = CARTESIAN_POINT ( 'NONE',  ( 11.66836325772209904, -64.97277996009040635, -16.48189043738600290 ) ) ;
#41359 = CARTESIAN_POINT ( 'NONE',  ( 13.00893739769619906, 34.28605925116850273, -47.75434321273180416 ) ) ;
#41360 = CARTESIAN_POINT ( 'NONE',  ( 55.10456381066440201, 13.97851885024129892, -14.92011627202030155 ) ) ;
#41361 = CARTESIAN_POINT ( 'NONE',  ( 14.36273960662768090, -22.20707503043608000, -55.03615486043509009 ) ) ;
#41362 = DIRECTION ( 'NONE',  ( 1.000000000000000000, 0.000000000000000000, 0.000000000000000000 ) ) ;
#41363 = ORIENTED_EDGE ( 'NONE', *, *, #828, .T. ) ;
#41364 = CARTESIAN_POINT ( 'NONE',  ( -22.86606125915950116, -13.70232240041790028, -54.87897021767069106 ) ) ;
#41365 = DIRECTION ( 'NONE',  ( -0.9876883405951387696, -0.1564344650402249015, 0.000000000000000000 ) ) ;
#41366 = TOROIDAL_SURFACE ( 'NONE', #2888, 19.30901699437490038, 0.5000000000000000000 ) ;
#41367 = CARTESIAN_POINT ( 'NONE',  ( 13.80986494171299483, 20.88376505836721364, -75.46937998419059568 ) ) ;
#41368 = CARTESIAN_POINT ( 'NONE',  ( 59.34401236131339630, -2.970618261826989848, -15.68001078640890178 ) ) ;
#41369 = CARTESIAN_POINT ( 'NONE',  ( 63.50007682179899149, 1.388189907116970101, -62.58632377286669879 ) ) ;
#41370 = B_SPLINE_CURVE_WITH_KNOTS ( 'NONE', 3,
 ( #4023, #97, #4523, #47793, #12149, #40429, #15810, #31771, #32025, #48050, #28103, #8210, #44364, #27854, #43855, #16326, #39926, #48300, #45664, #44886, #5059, #45407, #21795, #21535, #29144, #9255, #29658, #29910, #17626 ),
 .UNSPECIFIED., .F., .F.,
 ( 4, 2, 1, 1, 1, 1, 1, 2, 2, 2, 2, 2, 2, 2, 2, 2, 4 ),
 ( 0.5000037344877438228, 0.5002478732892634561, 0.5004920120907830894, 0.5009802896938223560, 0.5019568448999010002, 0.5039099553120580666, 0.5078161761363726434, 0.5156286177850016861, 0.5312535010822597714, 0.5625032676767758311, 0.6250028008658078393, 0.6875023340548398476, 0.7500018672438718559, 0.8125014004329038642, 0.8750009336219359835, 0.9375004668109679917, 1.000000000000000000 ),
 .UNSPECIFIED. ) ;
#41371 = CARTESIAN_POINT ( 'NONE',  ( 22.21935039506121257, -53.95817006707829933, -34.76477869314940961 ) ) ;
#41372 = VERTEX_POINT ( 'NONE', #42450 ) ;
#41373 = DIRECTION ( 'NONE',  ( -8.409939412270706254E-12, 1.000000000000000000, 0.000000000000000000 ) ) ;
#41374 = CARTESIAN_POINT ( 'NONE',  ( 70.83745409581385388, 17.98087126524510637, -71.50000000000081002 ) ) ;
#41375 = ORIENTED_EDGE ( 'NONE', *, *, #21004, .T. ) ;
#41376 = CARTESIAN_POINT ( 'NONE',  ( 55.27618969335288313, -51.00839723918451085, -75.15723747982120528 ) ) ;
#41377 = CARTESIAN_POINT ( 'NONE',  ( 48.91612765617589531, -46.17266810153950019, -11.68042562226399994 ) ) ;
#41378 = CARTESIAN_POINT ( 'NONE',  ( 23.77197502537190132, -17.41816804884900094, -34.08624212660669883 ) ) ;
#41379 = DIRECTION ( 'NONE',  ( 0.000000000000000000, 0.000000000000000000, 1.000000000000000000 ) ) ;
#41380 = CARTESIAN_POINT ( 'NONE',  ( 53.83029454980940187, 19.62285200761009918, -76.11627055017599730 ) ) ;
#41381 = CARTESIAN_POINT ( 'NONE',  ( 46.35275103504449845, -52.90993241930539881, -76.14999999999999147 ) ) ;
#41382 = ORIENTED_EDGE ( 'NONE', *, *, #45017, .T. ) ;
#41383 = CARTESIAN_POINT ( 'NONE',  ( 54.50029541982960524, 14.92341241185250134, -15.72721313530920106 ) ) ;
#41384 = CARTESIAN_POINT ( 'NONE',  ( 56.93466175439829868, -50.26424374751940150, -52.70269902980160026 ) ) ;
#41385 = CARTESIAN_POINT ( 'NONE',  ( 52.63829942681260121, -49.80293474851259816, -48.69642957805589845 ) ) ;
#41386 = CARTESIAN_POINT ( 'NONE',  ( 16.00572161013059969, -8.564513971789889268, -34.34139281033739621 ) ) ;
#41387 = DIRECTION ( 'NONE',  ( -0.3535533905932731202, -0.6123724356957964687, 0.7071067811865462405 ) ) ;
#41388 = VECTOR ( 'NONE', #38297, 1000.000000000000000 ) ;
#41390 = EDGE_CURVE ( 'NONE', #13595, #16677, #18075, .T. ) ;
#41389 = CARTESIAN_POINT ( 'NONE',  ( 46.50762589553990267, 21.90427357326890245, -76.13714234130850400 ) ) ;
#41391 = CARTESIAN_POINT ( 'NONE',  ( 64.93204900141920177, 0.9940695285616559795, -60.58508503553749591 ) ) ;
#41392 = CARTESIAN_POINT ( 'NONE',  ( 61.00705302608983516, -45.67218455906213137, -47.73074504205541047 ) ) ;
#41393 = CARTESIAN_POINT ( 'NONE',  ( 28.81656660489900190, -4.610261985355189829, -34.68308842254609914 ) ) ;
#41394 = CARTESIAN_POINT ( 'NONE',  ( 20.94623932155910140, -8.921080969116559345, -79.20604505178991417 ) ) ;
#41395 = DIRECTION ( 'NONE',  ( 0.000000000000000000, 0.000000000000000000, -1.000000000000000000 ) ) ;
#41396 = CARTESIAN_POINT ( 'NONE',  ( 68.13393739769620083, 4.883811055320659733, -65.65000000000000568 ) ) ;
#41398 = CARTESIAN_POINT ( 'NONE',  ( 47.18760304122697136, -39.34341269553539178, -54.66681054946693052 ) ) ;
#41397 = CARTESIAN_POINT ( 'NONE',  ( 64.84324960441180963, 0.8888742037077599356, -60.63285689971630177 ) ) ;
#41399 = VECTOR ( 'NONE', #29462, 1000.000000000000000 ) ;
#41400 = CARTESIAN_POINT ( 'NONE',  ( 54.36675628530522886, -55.06578241374116089, 16.85000000000000142 ) ) ;
#41401 = CARTESIAN_POINT ( 'NONE',  ( 11.27224164520935901, -9.290037151915401026, -68.79933606627460563 ) ) ;
#41402 = CARTESIAN_POINT ( 'NONE',  ( 6.211423689671518922, -64.98190781011250294, -48.42816009188030080 ) ) ;
#41403 = ORIENTED_EDGE ( 'NONE', *, *, #12008, .T. ) ;
#41404 = CARTESIAN_POINT ( 'NONE',  ( 52.72266114154869854, -49.72553381474750012, -48.47378032971909789 ) ) ;
#41405 = ORIENTED_EDGE ( 'NONE', *, *, #18614, .T. ) ;
#41406 = CARTESIAN_POINT ( 'NONE',  ( 61.66998612247429890, -45.11833688862720493, -28.01639554107829966 ) ) ;
#41407 = CARTESIAN_POINT ( 'NONE',  ( 48.76904876940009359, -54.05456627190059749, -55.30034376619679648 ) ) ;
#41408 = CARTESIAN_POINT ( 'NONE',  ( 13.32539556584979934, 19.89887940024619795, -21.90066023095720027 ) ) ;
#41409 = CARTESIAN_POINT ( 'NONE',  ( 55.91421057036799880, 14.69455263003700018, -25.53646976440970207 ) ) ;
#41410 = CARTESIAN_POINT ( 'NONE',  ( 11.03079100840449911, -10.74787757151459822, -37.69532517445329489 ) ) ;
#41411 = CARTESIAN_POINT ( 'NONE',  ( 50.52803440128089818, 19.14656596045000114, -76.14999999999999147 ) ) ;
#41412 = CARTESIAN_POINT ( 'NONE',  ( 52.72966687298379895, 18.49590603975559588, -48.70009282041390009 ) ) ;
#41413 = CARTESIAN_POINT ( 'NONE',  ( 60.61194832405840316, -45.58361201891599990, -47.15894465080069864 ) ) ;
#41414 = CARTESIAN_POINT ( 'NONE',  ( 64.87855344762060383, -43.72806524318039578, -10.46215703267770003 ) ) ;
#41415 = VERTEX_POINT ( 'NONE', #35606 ) ;
#41416 = CARTESIAN_POINT ( 'NONE',  ( 23.47605554803709893, -16.88109819232330011, -75.12164841756148803 ) ) ;
#41417 = EDGE_CURVE ( 'NONE', #4867, #49956, #26442, .T. ) ;
#41418 = CARTESIAN_POINT ( 'NONE',  ( 72.77398937677050128, 1.387412027389909985, -68.69511434646409498 ) ) ;
#41419 = CARTESIAN_POINT ( 'NONE',  ( 47.52424585455850092, -54.57167504433569860, -54.72304599233210354 ) ) ;
#41420 = CARTESIAN_POINT ( 'NONE',  ( 22.76597515051138032, -11.21741694172178150, -49.60607765262594882 ) ) ;
#41421 = CARTESIAN_POINT ( 'NONE',  ( 72.80768847294999091, 1.384447124000270035, -62.70866005236110396 ) ) ;
#41422 =( BOUNDED_CURVE ( )  B_SPLINE_CURVE ( 3, ( #17938, #50441, #26045, #26307 ),
 .UNSPECIFIED., .F., .T. ) 
 B_SPLINE_CURVE_WITH_KNOTS ( ( 4, 4 ),
 ( 0.7853981633974366217, 1.053572925743754274 ),
 .UNSPECIFIED. ) 
 CURVE ( )  GEOMETRIC_REPRESENTATION_ITEM ( )  RATIONAL_B_SPLINE_CURVE ( ( 1.000000000000000000, 0.9940158321278126374, 0.9940158321278126374, 1.000000000000000000 ) ) 
 REPRESENTATION_ITEM ( '' )  );
#41423 = CARTESIAN_POINT ( 'NONE',  ( 60.34156420439850876, 15.53871978590400005, -48.95535497881819964 ) ) ;
#41424 = CARTESIAN_POINT ( 'NONE',  ( 51.13393739769620083, -15.61618894467929941, 9.349999999999999645 ) ) ;
#41425 = CARTESIAN_POINT ( 'NONE',  ( 8.222342146248220018, -15.61610160653870061, -76.79233150823698395 ) ) ;
#41426 = CARTESIAN_POINT ( 'NONE',  ( 72.19114968843099689, 1.019773975906300034, -61.22921083583120350 ) ) ;
#41427 = CARTESIAN_POINT ( 'NONE',  ( 24.04476371472169305, -15.67281184061405597, -71.50995035837887315 ) ) ;
#41428 = CARTESIAN_POINT ( 'NONE',  ( 65.09597585808549525, 1.387131204727280132, -70.29242575817399086 ) ) ;
#41429 = ORIENTED_EDGE ( 'NONE', *, *, #14057, .T. ) ;
#41430 = AXIS2_PLACEMENT_3D ( 'NONE', #23499, #51827, #15927 ) ;
#41431 = CARTESIAN_POINT ( 'NONE',  ( 13.65323237295500114, -51.39160756102839400, -23.15000000000000213 ) ) ;
#41432 = CARTESIAN_POINT ( 'NONE',  ( 15.94849651692706338, -50.98802678465642657, -15.66350744312629217 ) ) ;
#41433 = ORIENTED_EDGE ( 'NONE', *, *, #21013, .T. ) ;
#41434 = LINE ( 'NONE', #21507, #7467 ) ;
#41435 = CARTESIAN_POINT ( 'NONE',  ( -4.666062602303798990, -15.61618894467930119, -11.54999999999999893 ) ) ;
#41436 = CARTESIAN_POINT ( 'NONE',  ( 10.13393739769619906, -54.15188668067469990, -35.14999999999999858 ) ) ;
#41437 = CARTESIAN_POINT ( 'NONE',  ( 53.60866038548149959, 19.65083965924290155, -76.14577118446059956 ) ) ;
#41438 = ORIENTED_EDGE ( 'NONE', *, *, #40756, .T. ) ;
#41439 = DIRECTION ( 'NONE',  ( 0.000000000000000000, 0.000000000000000000, -1.000000000000000000 ) ) ;
#41440 = DIRECTION ( 'NONE',  ( 0.000000000000000000, -1.000000000000000000, 0.000000000000000000 ) ) ;
#41441 = CARTESIAN_POINT ( 'NONE',  ( 23.79191596521776830, -13.56499935927118194, -43.70900647343250256 ) ) ;
#41442 = B_SPLINE_SURFACE_WITH_KNOTS ( 'NONE', 3, 3, ( 
 ( #51229, #43109, #23155, #2751, #15581, #23411 ),
 ( #18981, #6949, #3530, #3267, #44313, #4478 ),
 ( #31275, #22646, #27358, #24370, #39431, #38918 ),
 ( #19501, #47554, #35491, #47049, #11396, #18723 ),
 ( #50451, #3009, #14540, #14801, #43365, #51482 ),
 ( #46533, #26575, #42590, #46788, #31025, #6686 ),
 ( #10879, #34701, #50702, #42852, #11136, #22901 ),
 ( #27105, #7457, #5272, #21223, #45613, #40641 ),
 ( #16799, #16530, #20969, #25672, #41414, #28834 ),
 ( #8674, #1587, #44838, #37486, #49301, #41674 ),
 ( #20706, #45361, #36436, #36697, #41159, #33016 ),
 ( #17576, #9463, #12878, #5009, #8945, #5532 ),
 ( #24887, #33284, #5780, #13649, #49562, #25154 ),
 ( #44573, #21487, #544, #32480, #40899, #37235 ) ),
 .UNSPECIFIED., .F., .F., .F.,
 ( 4, 2, 2, 2, 2, 2, 4 ),
 ( 4, 1, 1, 4 ),
 ( 3.150553799287940215, 8.744225258584139127, 18.73762555410890229, 24.98350073881190170, 28.10643833116330015, 33.10313847892570038, 38.05651419634610022 ),
 ( 0.000000000000000000, 0.3333333333333329818, 0.6666666666666670737, 1.000235426512150028 ),
 .UNSPECIFIED. ) ;
#41443 = CARTESIAN_POINT ( 'NONE',  ( 21.87095150668039878, -21.53813027917859912, -56.04737992176900008 ) ) ;
#41444 = DIRECTION ( 'NONE',  ( 0.000000000000000000, 0.000000000000000000, 1.000000000000000000 ) ) ;
#41445 = CARTESIAN_POINT ( 'NONE',  ( 43.99195235186844144, -37.91623234883149962, -70.35986276463864897 ) ) ;
#41446 = VERTEX_POINT ( 'NONE', #47419 ) ;
#41447 = CARTESIAN_POINT ( 'NONE',  ( 56.56423663003400293, -46.20304009252470223, -26.26562856521130129 ) ) ;
#41448 = CARTESIAN_POINT ( 'NONE',  ( 8.841563762076869892, -14.09041682418759933, -47.29830972369120445 ) ) ;
#41449 = CARTESIAN_POINT ( 'NONE',  ( 44.88838914241820532, 14.87646786394859966, -8.899003544310730263 ) ) ;
#41450 = EDGE_CURVE ( 'NONE', #30137, #16752, #15439, .T. ) ;
#41451 = CARTESIAN_POINT ( 'NONE',  ( 14.34420360062739874, 19.88380572466640217, -74.33583724502659607 ) ) ;
#41452 = EDGE_CURVE ( 'NONE', #35762, #12879, #19206, .T. ) ;
#41453 = DIRECTION ( 'NONE',  ( 1.000000000000000000, 0.000000000000000000, 0.000000000000000000 ) ) ;
#41454 = ADVANCED_FACE ( 'NONE', ( #46649 ), #30633, .F. ) ;
#41455 = DIRECTION ( 'NONE',  ( -1.000000000000000000, 0.000000000000000000, 0.000000000000000000 ) ) ;
#41456 = AXIS2_PLACEMENT_3D ( 'NONE', #38843, #2931, #34886 ) ;
#41457 = ADVANCED_FACE ( 'NONE', ( #3644 ), #51594, .T. ) ;
#41458 = CARTESIAN_POINT ( 'NONE',  ( 21.97196478570849720, -21.43857307197580297, -55.75724145695859590 ) ) ;
#41459 = VERTEX_POINT ( 'NONE', #7064 ) ;
#41460 = CARTESIAN_POINT ( 'NONE',  ( 52.86912716173040394, -49.53963500218709726, -27.34061465770520272 ) ) ;
#41461 = VECTOR ( 'NONE', #41835, 1000.000000000000000 ) ;
#41462 = CARTESIAN_POINT ( 'NONE',  ( 15.92174032689569785, -51.05401459586040147, -20.83925419535820112 ) ) ;
#41463 = CARTESIAN_POINT ( 'NONE',  ( 4.229204521551100271, 25.38381512987610122, -9.628996958294839814 ) ) ;
#41464 = CARTESIAN_POINT ( 'NONE',  ( 71.33393739769628894, 1.883811055320669947, -62.44999999999999574 ) ) ;
#41465 = CARTESIAN_POINT ( 'NONE',  ( 50.01275587524209953, 14.95672356651379964, -12.46590248485050090 ) ) ;
#41466 = AXIS2_PLACEMENT_3D ( 'NONE', #42376, #33963, #14071 ) ;
#41467 = ORIENTED_EDGE ( 'NONE', *, *, #17913, .F. ) ;
#41468 = B_SPLINE_CURVE_WITH_KNOTS ( 'NONE', 3,
 ( #44475, #40542, #4632, #27448, #20869, #36869, #37131, #1489, #37386, #41315 ),
 .UNSPECIFIED., .F., .F.,
 ( 4, 2, 2, 2, 4 ),
 ( 0.000000000000000000, 0.1774999999751137592, 0.3374999999737621770, 0.4374999999729171085, 0.5000013127411032654 ),
 .UNSPECIFIED. ) ;
#41469 = CARTESIAN_POINT ( 'NONE',  ( -6.906756203940550343, -45.84230676707479546, -4.921515829384339291 ) ) ;
#41470 = CARTESIAN_POINT ( 'NONE',  ( 47.47474619565739573, 23.38248241296770047, -54.92426841363709400 ) ) ;
#41471 = CARTESIAN_POINT ( 'NONE',  ( 46.63393739769619373, 4.883811055320659733, -34.64999999999999858 ) ) ;
#41472 = CARTESIAN_POINT ( 'NONE',  ( 63.50659274611129490, 1.388313565858570131, -62.46994910431339321 ) ) ;
#41473 = CARTESIAN_POINT ( 'NONE',  ( 60.66036711866519937, 14.32586616646070077, -47.11242423095009713 ) ) ;
#41474 = CARTESIAN_POINT ( 'NONE',  ( 42.53968775098609711, 12.99877936061140105, -5.088323969512570599 ) ) ;
#41475 = DIRECTION ( 'NONE',  ( 0.000000000000000000, 1.000000000000000000, 0.000000000000000000 ) ) ;
#41476 = CARTESIAN_POINT ( 'NONE',  ( 52.93498290923280081, 18.37341140428640074, -48.74287987618620122 ) ) ;
#41477 = DIRECTION ( 'NONE',  ( 0.000000000000000000, 1.000000000000000000, 0.000000000000000000 ) ) ;
#41478 = VECTOR ( 'NONE', #23445, 1000.000000000000000 ) ;
#41479 = CARTESIAN_POINT ( 'NONE',  ( 56.65979965533069418, -47.79656003688090493, -48.39907199131990012 ) ) ;
#41480 = CARTESIAN_POINT ( 'NONE',  ( -21.36606260230379917, 21.88381105532059934, 11.84999999999999964 ) ) ;
#41481 = CARTESIAN_POINT ( 'NONE',  ( 54.22654478441499748, 20.21700441338549936, -53.14607073534880044 ) ) ;
#41482 = EDGE_CURVE ( 'NONE', #37056, #18491, #7208, .T. ) ;
#41483 = CARTESIAN_POINT ( 'NONE',  ( 63.55206628625449383, 1.395841248662849976, -68.96826120918760239 ) ) ;
#41484 = DIRECTION ( 'NONE',  ( -1.000000000000000000, 0.000000000000000000, 0.000000000000000000 ) ) ;
#41485 = CARTESIAN_POINT ( 'NONE',  ( 9.367777563323313572, -16.29676251027069966, -61.81516750865657883 ) ) ;
#41486 = ORIENTED_EDGE ( 'NONE', *, *, #35690, .F. ) ;
#41487 = LINE ( 'NONE', #2176, #25413 ) ;
#41488 = CARTESIAN_POINT ( 'NONE',  ( 10.13923265016959974, 31.95181006972909543, -45.99474826666039462 ) ) ;
#41489 = CARTESIAN_POINT ( 'NONE',  ( 28.49955684666385025, -22.75548266223732341, -34.64999999999999858 ) ) ;
#41490 = FACE_OUTER_BOUND ( 'NONE', #48608, .T. ) ;
#41491 = CONICAL_SURFACE ( 'NONE', #49072, 0.7349999999999987654, 0.06981317007977388966 ) ;
#41492 = CARTESIAN_POINT ( 'NONE',  ( 8.761419361326980848, -12.64912489806860840, -80.62955707704453800 ) ) ;
#41493 = ORIENTED_EDGE ( 'NONE', *, *, #6824, .T. ) ;
#41494 = ORIENTED_EDGE ( 'NONE', *, *, #5784, .T. ) ;
#41495 = CARTESIAN_POINT ( 'NONE',  ( 47.64143405402000297, 23.30250925608569901, -55.14905519569659731 ) ) ;
#41496 = ORIENTED_EDGE ( 'NONE', *, *, #25587, .T. ) ;
#41497 = CARTESIAN_POINT ( 'NONE',  ( 10.32185532229130054, -63.49178473827629432, -45.85329026226229843 ) ) ;
#41498 = CARTESIAN_POINT ( 'NONE',  ( 56.94849961771190294, -45.38884577364979833, -25.89141764539759905 ) ) ;
#41499 = CARTESIAN_POINT ( 'NONE',  ( 24.04493739766370553, -15.61621743414952945, -77.50767718564499376 ) ) ;
#41500 = CARTESIAN_POINT ( 'NONE',  ( 22.46011667808101109, -10.75453029109795011, -63.29933646154306359 ) ) ;
#41501 = CARTESIAN_POINT ( 'NONE',  ( 61.54360026869530031, 13.96084431199959930, -46.89388919338750128 ) ) ;
#41502 = CARTESIAN_POINT ( 'NONE',  ( 63.64445560419389381, 1.419970371293449940, -62.18985507218640407 ) ) ;
#41503 = ORIENTED_EDGE ( 'NONE', *, *, #7411, .F. ) ;
#41504 = EDGE_CURVE ( 'NONE', #5359, #34565, #28556, .T. ) ;
#41505 = CARTESIAN_POINT ( 'NONE',  ( 75.24376310073057539, 2.809539095331776259, -12.25943769873225442 ) ) ;
#41506 = VECTOR ( 'NONE', #29724, 1000.000000000000114 ) ;
#41507 = EDGE_LOOP ( 'NONE', ( #1258, #41568, #49948, #49240, #45244 ) ) ;
#41508 = CARTESIAN_POINT ( 'NONE',  ( 49.51534909287300223, -45.20344304405800528, -10.82567614850110083 ) ) ;
#41509 = TOROIDAL_SURFACE ( 'NONE', #6347, 40.00000000000310507, 2.000000000000059952 ) ;
#41510 = CARTESIAN_POINT ( 'NONE',  ( 24.04493117584121364, -15.62644129081893674, -33.79274222580392717 ) ) ;
#41511 = DIRECTION ( 'NONE',  ( 0.000000000000000000, 1.000000000000000000, 0.000000000000000000 ) ) ;
#41512 = ORIENTED_EDGE ( 'NONE', *, *, #1285, .F. ) ;
#41513 = CARTESIAN_POINT ( 'NONE',  ( 19.61497263573680172, -40.47764751925419802, -35.14999999999999858 ) ) ;
#41514 = CARTESIAN_POINT ( 'NONE',  ( 47.20045633199760005, -54.78545101841919518, -74.36298856109941369 ) ) ;
#41515 = CARTESIAN_POINT ( 'NONE',  ( 16.13393739769620083, -15.61618894467929941, -32.14999999999999858 ) ) ;
#41516 = VECTOR ( 'NONE', #6926, 1000.000000000000000 ) ;
#41517 = CARTESIAN_POINT ( 'NONE',  ( 55.10456381066440201, 13.97851885024129892, -14.92011627202030155 ) ) ;
#41518 = FACE_OUTER_BOUND ( 'NONE', #51601, .T. ) ;
#41519 = CARTESIAN_POINT ( 'NONE',  ( 19.72595728692159867, -21.68578137661910077, -63.17708371749489515 ) ) ;
#41520 = CARTESIAN_POINT ( 'NONE',  ( 60.77271789202009700, 13.90791468296399991, -26.82299636899789874 ) ) ;
#41521 = EDGE_CURVE ( 'NONE', #8545, #11667, #8063, .T. ) ;
#41522 = CARTESIAN_POINT ( 'NONE',  ( 23.98053627935140142, -15.48339521895720061, -73.28211911255830557 ) ) ;
#41523 = VERTEX_POINT ( 'NONE', #51847 ) ;
#41524 = AXIS2_PLACEMENT_3D ( 'NONE', #409, #48370, #16396 ) ;
#41525 = CARTESIAN_POINT ( 'NONE',  ( 52.26132335211670465, 19.59060111016600203, -50.93306148729159588 ) ) ;
#41526 = CARTESIAN_POINT ( 'NONE',  ( 73.23379646625190276, 0.8840451408750739093, -62.48896739026430680 ) ) ;
#41527 = DIRECTION ( 'NONE',  ( 0.000000000000000000, -1.000000000000000000, 0.000000000000000000 ) ) ;
#41528 = CARTESIAN_POINT ( 'NONE',  ( 72.96828430334601023, 1.031491003830610209, -69.18984148332670259 ) ) ;
#41529 = CARTESIAN_POINT ( 'NONE',  ( 12.56262532525460074, -39.78532101326960202, -74.14999999999999147 ) ) ;
#41530 = CIRCLE ( 'NONE', #49117, 4.296700167715679086 ) ;
#41531 = CARTESIAN_POINT ( 'NONE',  ( 23.85151994168742462, -13.77020273865184841, -65.43299463483448619 ) ) ;
#41532 = CARTESIAN_POINT ( 'NONE',  ( 2.633937397696199945, -15.61618894467930119, 4.349999999999999645 ) ) ;
#41533 = CARTESIAN_POINT ( 'NONE',  ( 48.96779238971210191, -53.80776418538130201, -54.50050231667190559 ) ) ;
#41534 = AXIS2_PLACEMENT_3D ( 'NONE', #14604, #6753, #14862 ) ;
#41535 = CARTESIAN_POINT ( 'NONE',  ( -18.35638189584738100, -50.24588423573534612, 11.97999999999999865 ) ) ;
#41536 = CARTESIAN_POINT ( 'NONE',  ( 63.88393739769619373, 20.38443354211860026, -61.44999999999999574 ) ) ;
#41538 = EDGE_CURVE ( 'NONE', #22408, #40267, #43201, .T. ) ;
#41537 = CYLINDRICAL_SURFACE ( 'NONE', #35699, 2.000000000000001776 ) ;
#41539 = ORIENTED_EDGE ( 'NONE', *, *, #1174, .T. ) ;
#41540 = CARTESIAN_POINT ( 'NONE',  ( 12.88601828706359953, -8.911137431892139915, -40.42375661169619860 ) ) ;
#41541 = CARTESIAN_POINT ( 'NONE',  ( 64.01820444265550236, 1.113948672550079788, -61.29006734358329567 ) ) ;
#41542 = VERTEX_POINT ( 'NONE', #31645 ) ;
#41543 = CARTESIAN_POINT ( 'NONE',  ( 55.55365133010059964, -45.11618894467940066, -14.32025150907159983 ) ) ;
#41544 = CARTESIAN_POINT ( 'NONE',  ( 61.12101616177810826, -45.46746661123680155, -47.45428572051350358 ) ) ;
#41545 = CARTESIAN_POINT ( 'NONE',  ( 1.167123001759671430, -26.49021611209005655, 7.849999999999997868 ) ) ;
#41546 = CARTESIAN_POINT ( 'NONE',  ( 9.221357130620331688, -19.60022191152414095, -62.34097168116907994 ) ) ;
#41548 = CARTESIAN_POINT ( 'NONE',  ( 68.13393739769618662, -2.166188944679360073, -100.2061629005786898 ) ) ;
#41547 = CARTESIAN_POINT ( 'NONE',  ( 44.56598291179225413, 8.767012424567191431, -63.91637373492464747 ) ) ;
#41549 = LINE ( 'NONE', #37106, #41863 ) ;
#41550 = DIRECTION ( 'NONE',  ( 0.000000000000000000, 0.000000000000000000, 1.000000000000000000 ) ) ;
#41551 = ORIENTED_EDGE ( 'NONE', *, *, #23928, .T. ) ;
#41552 = EDGE_LOOP ( 'NONE', ( #24311, #36102, #49768, #17209 ) ) ;
#41553 = ORIENTED_EDGE ( 'NONE', *, *, #4774, .T. ) ;
#41554 = ORIENTED_EDGE ( 'NONE', *, *, #41754, .T. ) ;
#41555 = CARTESIAN_POINT ( 'NONE',  ( 61.45294886705139703, -45.16075153748559501, -46.46810862312010215 ) ) ;
#41556 = CARTESIAN_POINT ( 'NONE',  ( 53.02878341227049930, -49.61154767067039728, -49.09821772105390636 ) ) ;
#41557 = CARTESIAN_POINT ( 'NONE',  ( 48.12002887478553959, -54.05111908400336063, -53.67198234080560582 ) ) ;
#41558 = CARTESIAN_POINT ( 'NONE',  ( 54.43067208826479941, -51.42334665385340031, -53.21919371617259742 ) ) ;
#41559 = VECTOR ( 'NONE', #46258, 1000.000000000000114 ) ;
#41560 = EDGE_CURVE ( 'NONE', #34524, #31052, #9186, .T. ) ;
#41561 = EDGE_LOOP ( 'NONE', ( #6132, #23300, #40685, #38343, #32573, #29881, #10378, #45171, #36684, #19778, #545, #5610, #23691, #3967, #11539, #22541, #6167, #19428, #44130, #5599, #5093, #10204, #370, #51105, #18886, #12570, #2766, #36016, #1278, #19891, #22387, #40200, #19942, #46200, #5365, #2826, #8193, #7364, #42681, #6121, #22138, #3398, #8567, #41675, #26652, #49553, #2574, #46193, #42803, #39770, #1678, #10046, #3119, #22033, #48791, #44079, #9137, #10483, #25702, #36364, #48920, #50010, #9919, #9910, #837, #9760, #50582, #50316, #37967, #48689, #2629, #18276, #23571, #36379, #19710, #46609, #15009, #36330, #9954, #18426, #12226, #8901, #49829, #18856, #35356, #16612, #31600, #5799, #2012, #26805, #24619, #43176, #17362, #20988, #45572, #30613, #1067, #4494, #26922, #34517, #45024, #43120, #15537 ) ) ;
#41562 = ORIENTED_EDGE ( 'NONE', *, *, #8824, .F. ) ;
#41563 = CARTESIAN_POINT ( 'NONE',  ( 24.03110856329654155, -15.13910014759192535, -77.48847149410299551 ) ) ;
#41564 = EDGE_CURVE ( 'NONE', #44442, #39070, #20371, .T. ) ;
#41565 = B_SPLINE_CURVE_WITH_KNOTS ( 'NONE', 3,
 ( #18028, #18542, #41360, #30058, #6501, #33992 ),
 .UNSPECIFIED., .F., .F.,
 ( 4, 1, 1, 4 ),
 ( 0.000000000000000000, 0.3333333470322403236, 0.6666666937979618401, 1.000000000000000000 ),
 .UNSPECIFIED. ) ;
#41566 = CARTESIAN_POINT ( 'NONE',  ( 54.02518786316219490, -51.81565143108780092, -54.18996768095620098 ) ) ;
#41567 = DIRECTION ( 'NONE',  ( 0.000000000000000000, 0.000000000000000000, -1.000000000000000000 ) ) ;
#41568 = ORIENTED_EDGE ( 'NONE', *, *, #16556, .T. ) ;
#41569 = CARTESIAN_POINT ( 'NONE',  ( 24.04484584168765338, -15.65733071861149028, -49.50932076728930298 ) ) ;
#41570 = CARTESIAN_POINT ( 'NONE',  ( 51.61768760778490162, -50.35895232405650290, -76.35064948397560158 ) ) ;
#41571 = CARTESIAN_POINT ( 'NONE',  ( 60.51833370568750325, 14.40028145102449919, -47.19438552604259485 ) ) ;
#41572 = VECTOR ( 'NONE', #39756, 1000.000000000000000 ) ;
#41573 = CARTESIAN_POINT ( 'NONE',  ( 21.51830670342329910, -9.906958280997308464, -59.75317579121929867 ) ) ;
#41574 = TOROIDAL_SURFACE ( 'NONE', #23958, 48.00000000000000000, 2.000000000000000000 ) ;
#41575 = CARTESIAN_POINT ( 'NONE',  ( 14.13393739769640156, 10.38381105532060111, -35.14999999999999858 ) ) ;
#41576 = CARTESIAN_POINT ( 'NONE',  ( 45.76571748013050467, 13.88566788246860106, -7.589016501219620459 ) ) ;
#41577 = CARTESIAN_POINT ( 'NONE',  ( 42.29463402943059691, -44.11680428309589530, -4.936190359317110143 ) ) ;
#41578 = CARTESIAN_POINT ( 'NONE',  ( 72.19114968843099689, 1.019773975906310026, -61.22921083583130297 ) ) ;
#41579 = DIRECTION ( 'NONE',  ( 0.000000000000000000, 0.000000000000000000, 1.000000000000000000 ) ) ;
#41580 = EDGE_CURVE ( 'NONE', #47534, #25231, #22295, .T. ) ;
#41581 = CARTESIAN_POINT ( 'NONE',  ( 63.80720226989929245, 1.275251724699800082, -69.71680052808839889 ) ) ;
#41582 = CARTESIAN_POINT ( 'NONE',  ( -21.36606260230379917, -53.11618894467930119, 17.35000000000000142 ) ) ;
#41583 = CARTESIAN_POINT ( 'NONE',  ( 65.61159314286859967, 0.5046460432913409955, -17.31747064995380114 ) ) ;
#41584 = ADVANCED_FACE ( 'NONE', ( #28235 ), #25614, .T. ) ;
#41585 = EDGE_LOOP ( 'NONE', ( #48669, #8712, #19062, #37560, #28341, #43213 ) ) ;
#41586 = CARTESIAN_POINT ( 'NONE',  ( 14.97377065893240022, -52.94069807145589834, -76.14999999999999147 ) ) ;
#41587 = AXIS2_PLACEMENT_3D ( 'NONE', #18505, #49466, #42624 ) ;
#41588 = CARTESIAN_POINT ( 'NONE',  ( 16.13393739769620083, -15.61618894467929941, -14.03562394879499919 ) ) ;
#41589 = CARTESIAN_POINT ( 'NONE',  ( 9.469557472586508595, 33.05699343160934944, -46.83899467898784508 ) ) ;
#41590 = FACE_OUTER_BOUND ( 'NONE', #9542, .T. ) ;
#41591 = CIRCLE ( 'NONE', #23978, 33.97624844042359626 ) ;
#41592 = CARTESIAN_POINT ( 'NONE',  ( 23.38129519385890021, -17.13736245159219607, -32.14999999999999858 ) ) ;
#41593 = CARTESIAN_POINT ( 'NONE',  ( 7.853097003783780394, -60.52042854835909935, -20.86915960608759946 ) ) ;
#41594 = CARTESIAN_POINT ( 'NONE',  ( 20.12545638205761733, -8.759847604476449945, -45.17547658566174817 ) ) ;
#41595 = CARTESIAN_POINT ( 'NONE',  ( 56.48532678114089833, 19.53534987139169843, -53.84780880325180163 ) ) ;
#41596 = CARTESIAN_POINT ( 'NONE',  ( 14.06319310886902407, -23.32127208991568779, -46.37571296203240934 ) ) ;
#41597 = CARTESIAN_POINT ( 'NONE',  ( 48.08307792209969733, 23.04244796336689660, -54.77528017867940235 ) ) ;
#41598 = CARTESIAN_POINT ( 'NONE',  ( 15.07367541409689871, -22.58887879154509903, -65.39521378727610568 ) ) ;
#41599 = B_SPLINE_CURVE_WITH_KNOTS ( 'NONE', 3,
 ( #14850, #51781, #46841, #7768, #11701, #19294, #42901, #23717, #51274, #15884, #15372 ),
 .UNSPECIFIED., .F., .F.,
 ( 4, 1, 1, 1, 1, 1, 1, 1, 4 ),
 ( 0.000000000000000000, 0.1249775000236086064, 0.2499805368352087664, 0.3749835736468090097, 0.4999866104584091420, 0.6249896472700092742, 0.7499926840816094620, 0.8749957208932096497, 1.000000000000000000 ),
 .UNSPECIFIED. ) ;
#41600 = ORIENTED_EDGE ( 'NONE', *, *, #50405, .F. ) ;
#41601 = DIRECTION ( 'NONE',  ( -1.000000000000000000, 0.000000000000000000, 0.000000000000000000 ) ) ;
#41602 = AXIS2_PLACEMENT_3D ( 'NONE', #6185, #13279, #25553 ) ;
#41603 = CARTESIAN_POINT ( 'NONE',  ( 18.21836968370325138, -14.10176024214774593, -22.64999999999999858 ) ) ;
#41604 = CARTESIAN_POINT ( 'NONE',  ( 9.543099337633478285, -17.38756428688266809, -43.36948683488909495 ) ) ;
#41606 = CARTESIAN_POINT ( 'NONE',  ( 53.38525277802689573, 17.73587511727710009, -26.66601672333850104 ) ) ;
#41605 = CARTESIAN_POINT ( 'NONE',  ( 82.92203328426339226, 13.96022355596819864, -47.12557951548500057 ) ) ;
#41607 = CARTESIAN_POINT ( 'NONE',  ( 10.04829391747680134, -19.18094729950349731, -71.28415194542810696 ) ) ;
#41608 = CARTESIAN_POINT ( 'NONE',  ( 11.68991505668612518, 33.67328296886341832, -16.36861125145141216 ) ) ;
#41609 = CARTESIAN_POINT ( 'NONE',  ( 56.92059784994150107, -45.11618894467940066, -15.82169481042769732 ) ) ;
#41610 = CARTESIAN_POINT ( 'NONE',  ( 8.643872352929088620, -48.75656286698969666, -35.12503119152809461 ) ) ;
#41611 = ORIENTED_EDGE ( 'NONE', *, *, #44817, .F. ) ;
#41612 = ORIENTED_EDGE ( 'NONE', *, *, #50472, .F. ) ;
#41613 = CARTESIAN_POINT ( 'NONE',  ( 11.62560706825669854, -64.94769956958019463, -16.46999247997619875 ) ) ;
#41614 = CARTESIAN_POINT ( 'NONE',  ( 11.25984818798209908, 33.08560177680430314, -44.83508380383680247 ) ) ;
#41615 = FACE_OUTER_BOUND ( 'NONE', #7203, .T. ) ;
#41616 = DIRECTION ( 'NONE',  ( 1.000000000000000000, 0.000000000000000000, 0.000000000000000000 ) ) ;
#41617 = CARTESIAN_POINT ( 'NONE',  ( 16.13393739769620083, -15.61618894467929941, -76.14999999999999147 ) ) ;
#41618 = ORIENTED_EDGE ( 'NONE', *, *, #32140, .F. ) ;
#41619 = CARTESIAN_POINT ( 'NONE',  ( -20.84783344275790284, -28.76004404052860153, -53.00251837860739101 ) ) ;
#41620 = DIRECTION ( 'NONE',  ( 0.000000000000000000, 0.000000000000000000, -1.000000000000000000 ) ) ;
#41621 = EDGE_CURVE ( 'NONE', #29694, #15276, #48431, .T. ) ;
#41622 = CARTESIAN_POINT ( 'NONE',  ( 53.40028332572070013, -49.44759849848939837, -49.16199268861880256 ) ) ;
#41623 = CARTESIAN_POINT ( 'NONE',  ( 52.08434102009589850, 19.14628782832189913, -49.21477419871119707 ) ) ;
#41624 = CARTESIAN_POINT ( 'NONE',  ( 60.24110131066720442, -2.014342208693430170, -15.82687703305419724 ) ) ;
#41625 = CARTESIAN_POINT ( 'NONE',  ( 50.62541591398729679, -49.13085010712609346, -76.22054775283200456 ) ) ;
#41626 = ADVANCED_FACE ( 'NONE', ( #20630 ), #19867, .T. ) ;
#41627 = DIRECTION ( 'NONE',  ( 0.000000000000000000, 0.000000000000000000, -1.000000000000000000 ) ) ;
#41628 = ORIENTED_EDGE ( 'NONE', *, *, #34110, .T. ) ;
#41629 = CARTESIAN_POINT ( 'NONE',  ( 12.72604264528349027, -9.703222777469695970, -67.78615274844003125 ) ) ;
#41630 = CARTESIAN_POINT ( 'NONE',  ( 8.222845792583640900, -15.61638830267690103, -48.79233150823699816 ) ) ;
#41631 = ORIENTED_EDGE ( 'NONE', *, *, #22824, .F. ) ;
#41632 = CARTESIAN_POINT ( 'NONE',  ( 24.04493739826821042, -14.58063923811300988, -53.75066785666746938 ) ) ;
#41633 = DIRECTION ( 'NONE',  ( 0.8660254037844387076, -0.4999999999999998890, 0.000000000000000000 ) ) ;
#41634 = CARTESIAN_POINT ( 'NONE',  ( 15.88724090743389894, -23.46003292791059991, -38.52250226616929751 ) ) ;
#41635 = CARTESIAN_POINT ( 'NONE',  ( 52.95214323273720680, -49.63863283588430164, -49.03964316977230453 ) ) ;
#41636 = CARTESIAN_POINT ( 'NONE',  ( 13.69516921742209981, -51.31182003115529966, -22.67922162956820031 ) ) ;
#41637 = CARTESIAN_POINT ( 'NONE',  ( 53.76985203492770182, 19.90181730786409986, -75.72009270347381005 ) ) ;
#41638 = CARTESIAN_POINT ( 'NONE',  ( 47.41051750594289871, -54.24117355536539975, -75.29851419728690587 ) ) ;
#41639 = ORIENTED_EDGE ( 'NONE', *, *, #25277, .T. ) ;
#41640 = CARTESIAN_POINT ( 'NONE',  ( 55.88004532031900595, 14.19452913225929969, -16.19747281084099910 ) ) ;
#41641 = CARTESIAN_POINT ( 'NONE',  ( 12.71325777259860068, -22.74941205225429997, -32.14999999999999858 ) ) ;
#41642 = CARTESIAN_POINT ( 'NONE',  ( 56.99190259417219551, -50.63247588150580469, -53.87165542819400343 ) ) ;
#41643 = CARTESIAN_POINT ( 'NONE',  ( 52.74474875099170390, -49.74042103855280317, -48.86872004196769836 ) ) ;
#41644 = AXIS2_PLACEMENT_3D ( 'NONE', #96, #12927, #1115 ) ;
#41645 = CARTESIAN_POINT ( 'NONE',  ( 23.15448228781169959, -14.94201639938200010, -34.81670639671909839 ) ) ;
#41646 = CARTESIAN_POINT ( 'NONE',  ( 41.64265090548820325, -46.42699119287450316, -4.296538310234230273 ) ) ;
#41647 = EDGE_CURVE ( 'NONE', #309, #20803, #16199, .T. ) ;
#41648 = VERTEX_POINT ( 'NONE', #27978 ) ;
#41649 = CARTESIAN_POINT ( 'NONE',  ( 46.99746007022550032, 22.70443078719620189, -75.76112237679920725 ) ) ;
#41650 = AXIS2_PLACEMENT_3D ( 'NONE', #42261, #14218, #10027 ) ;
#41651 = CARTESIAN_POINT ( 'NONE',  ( 16.13393739769620083, -1.759782484128330049, -47.64999999999999858 ) ) ;
#41652 = CARTESIAN_POINT ( 'NONE',  ( 75.33555834693952136, -38.13639482886969745, -12.70678390277496739 ) ) ;
#41653 = CARTESIAN_POINT ( 'NONE',  ( 20.11812230705482918, -8.703697806114258029, -57.45899798619976195 ) ) ;
#41654 = CARTESIAN_POINT ( 'NONE',  ( 43.87440825508269882, -45.06628648458400477, -6.621182746357190396 ) ) ;
#41655 = CARTESIAN_POINT ( 'NONE',  ( 28.93686911782399918, -4.565436177846480703, -34.75221567031820058 ) ) ;
#41656 = CARTESIAN_POINT ( 'NONE',  ( 17.67958691229047119, -49.61617040957372637, -83.18681078537983353 ) ) ;
#41657 = CARTESIAN_POINT ( 'NONE',  ( 0.3209249304026170480, -20.69829881652800196, -34.64999999999999858 ) ) ;
#41659 = CARTESIAN_POINT ( 'NONE',  ( 42.32061802937450068, -37.64775053028490248, -78.71596476449020940 ) ) ;
#41658 = DIRECTION ( 'NONE',  ( 0.000000000000000000, 0.000000000000000000, 1.000000000000000000 ) ) ;
#41660 = CARTESIAN_POINT ( 'NONE',  ( 61.26653127891100326, 14.00827977936110003, -46.51747653042859554 ) ) ;
#41661 = CARTESIAN_POINT ( 'NONE',  ( 63.66068354842759192, 0.9098571636355720083, -62.44999999999999574 ) ) ;
#41662 = CARTESIAN_POINT ( 'NONE',  ( -12.80120649412369893, 25.67501472466429746, -52.53814278327410392 ) ) ;
#41663 = ORIENTED_EDGE ( 'NONE', *, *, #37719, .F. ) ;
#41664 = CARTESIAN_POINT ( 'NONE',  ( 52.98906690378920104, -49.58008332147559827, -48.84983108313470268 ) ) ;
#41665 = EDGE_LOOP ( 'NONE', ( #41975, #21815, #16543, #16220, #25247, #30596, #25455 ) ) ;
#41666 = CARTESIAN_POINT ( 'NONE',  ( 61.75057827614799777, -45.11618897208180101, -28.00818819871750165 ) ) ;
#41667 = CARTESIAN_POINT ( 'NONE',  ( 49.48213591681099643, -53.75081833664790310, -55.18208724449630154 ) ) ;
#41668 = CARTESIAN_POINT ( 'NONE',  ( 55.94694845493520319, 14.62810299609100007, -25.32096506064640096 ) ) ;
#41669 = CARTESIAN_POINT ( 'NONE',  ( 13.34527985300699982, -22.09430192571580065, -43.08221248677949688 ) ) ;
#41670 = CARTESIAN_POINT ( 'NONE',  ( 28.96098294488680125, -26.67590919638950098, -34.77057949856859409 ) ) ;
#41671 = CARTESIAN_POINT ( 'NONE',  ( 53.14599511491060468, 18.29042438231470058, -49.02433925890680655 ) ) ;
#41672 = CARTESIAN_POINT ( 'NONE',  ( 65.00985940095789317, 1.385702546077159925, -61.00218178904909649 ) ) ;
#41673 = CARTESIAN_POINT ( 'NONE',  ( 60.87621821856699711, -45.44515361684550214, -47.03457408321020239 ) ) ;
#41674 = CARTESIAN_POINT ( 'NONE',  ( 67.50573363472270216, -43.40389107515569833, -11.14099675621210039 ) ) ;
#41675 = ORIENTED_EDGE ( 'NONE', *, *, #33330, .F. ) ;
#41676 = CARTESIAN_POINT ( 'NONE',  ( 11.07009171580209994, -10.15137776328389840, -74.32945910692518510 ) ) ;
#41677 = CARTESIAN_POINT ( 'NONE',  ( 72.93868606741401095, 1.327097482837290121, -68.80945595804269033 ) ) ;
#41678 = CARTESIAN_POINT ( 'NONE',  ( 47.43330265715069771, -54.63190133673469973, -54.73918112570320460 ) ) ;
#41679 = CARTESIAN_POINT ( 'NONE',  ( 8.222845792583640900, -15.61638830267690103, -48.79233150823699816 ) ) ;
#41680 = CARTESIAN_POINT ( 'NONE',  ( 73.14800808192789816, 0.9948723650351710690, -62.36838199720629916 ) ) ;
#41681 = CARTESIAN_POINT ( 'NONE',  ( 11.90332973437990027, -65.43688732449989232, -18.04110290864220190 ) ) ;
#41682 = CARTESIAN_POINT ( 'NONE',  ( 71.52584472686049821, 1.187931651339009909, -60.80292108597650014 ) ) ;
#41683 = DIRECTION ( 'NONE',  ( 0.000000000000000000, 1.000000000000000000, 0.000000000000000000 ) ) ;
#41684 = CARTESIAN_POINT ( 'NONE',  ( 8.222944117552916765, -14.58059227398267410, -44.83399173169763685 ) ) ;
#41685 = CIRCLE ( 'NONE', #36613, 20.00000000000001421 ) ;
#41686 = CARTESIAN_POINT ( 'NONE',  ( 50.03007040746459921, -32.48240620400619605, -78.14999999999999147 ) ) ;
#41687 = CARTESIAN_POINT ( 'NONE',  ( 64.74970223533068747, 0.9307121176571799825, -70.60454574395809857 ) ) ;
#41688 = VERTEX_POINT ( 'NONE', #4143 ) ;
#41689 = CARTESIAN_POINT ( 'NONE',  ( 13.77296168464159898, -51.29346510734379905, -23.09857315614619822 ) ) ;
#41690 = EDGE_CURVE ( 'NONE', #39, #12214, #37387, .T. ) ;
#41691 = CARTESIAN_POINT ( 'NONE',  ( 8.223528471986069732, -15.61608932669300032, -46.79233150823699816 ) ) ;
#41692 = ORIENTED_EDGE ( 'NONE', *, *, #1467, .T. ) ;
#41693 = DIRECTION ( 'NONE',  ( 0.5112408204145798551, -0.8594375041513067082, 0.000000000000000000 ) ) ;
#41694 = DIRECTION ( 'NONE',  ( 0.000000000000000000, 0.000000000000000000, -1.000000000000000000 ) ) ;
#41695 = CARTESIAN_POINT ( 'NONE',  ( 16.13393739769620083, -15.61618894467929941, -20.65000000000000213 ) ) ;
#41696 = CARTESIAN_POINT ( 'NONE',  ( 52.96553908380789721, 19.62936139908589794, -76.26079946550269995 ) ) ;
#41697 = ORIENTED_EDGE ( 'NONE', *, *, #43426, .T. ) ;
#41698 = CARTESIAN_POINT ( 'NONE',  ( 63.34104417888273986, -39.36618894467940066, 17.05710678118654755 ) ) ;
#41699 = CARTESIAN_POINT ( 'NONE',  ( 22.84576648276765454, -14.72542540978770198, -72.41083198718504832 ) ) ;
#41700 = CARTESIAN_POINT ( 'NONE',  ( 0.5406133260286669628, -43.55985091651039909, -21.14999999999999858 ) ) ;
#41701 = CARTESIAN_POINT ( 'NONE',  ( 9.243092856068470198, -11.08860884499529931, -50.97736833369750542 ) ) ;
#41702 = DIRECTION ( 'NONE',  ( 0.5000000000000003331, -0.8660254037844383745, 0.000000000000000000 ) ) ;
#41703 = CARTESIAN_POINT ( 'NONE',  ( 43.66604041426285931, -37.87226800533215254, -71.98948473448078289 ) ) ;
#41704 = B_SPLINE_CURVE_WITH_KNOTS ( 'NONE', 3,
 ( #33718, #29276, #24816, #45022, #13822, #21409 ),
 .UNSPECIFIED., .F., .F.,
 ( 4, 2, 4 ),
 ( 0.4942347057900616236, 0.7471173528950307841, 1.000000000000000000 ),
 .UNSPECIFIED. ) ;
#41705 = EDGE_LOOP ( 'NONE', ( #21462, #39638, #38087, #25354, #5262 ) ) ;
#41706 = ADVANCED_FACE ( 'NONE', ( #36617 ), #28500, .T. ) ;
#41707 = CARTESIAN_POINT ( 'NONE',  ( 18.84631954156857958, 20.57173965347324085, -74.52173647808412227 ) ) ;
#41708 = CARTESIAN_POINT ( 'NONE',  ( 8.997941842051611516, -17.75727774128869996, -47.13987186156389697 ) ) ;
#41709 = CARTESIAN_POINT ( 'NONE',  ( 9.063471803478160282, -18.03476473673429936, -32.14999999999999858 ) ) ;
#41710 = EDGE_CURVE ( 'NONE', #45901, #34463, #2710, .T. ) ;
#41711 = ADVANCED_FACE ( 'NONE', ( #48699 ), #8923, .F. ) ;
#41712 = CARTESIAN_POINT ( 'NONE',  ( 14.38800548507090049, 20.00715776053360173, -74.86150924066380696 ) ) ;
#41713 = CARTESIAN_POINT ( 'NONE',  ( 17.46614295537689188, -52.40467206555150170, -76.02665054608505102 ) ) ;
#41714 = CARTESIAN_POINT ( 'NONE',  ( 43.16863801754030305, -45.22759163273670424, -6.804293086635070154 ) ) ;
#41715 = CARTESIAN_POINT ( 'NONE',  ( 12.76582758031636544, -8.383476218416783254, -60.86875003376393778 ) ) ;
#41716 = CIRCLE ( 'NONE', #48417, 5.999999999999998224 ) ;
#41717 = AXIS2_PLACEMENT_3D ( 'NONE', #29456, #33386, #34352 ) ;
#41719 = AXIS2_PLACEMENT_3D ( 'NONE', #41952, #22528, #29868 ) ;
#41718 = CARTESIAN_POINT ( 'NONE',  ( 8.466531389232500260, -12.58409300121869911, -48.62753766123279320 ) ) ;
#41720 = ORIENTED_EDGE ( 'NONE', *, *, #41560, .T. ) ;
#41721 = CARTESIAN_POINT ( 'NONE',  ( 53.59918250157210196, -48.73737415287079955, -26.59416019702899803 ) ) ;
#41722 = CARTESIAN_POINT ( 'NONE',  ( 15.12151582310530173, -51.00866790501009973, -21.37863257647040172 ) ) ;
#41724 = CARTESIAN_POINT ( 'NONE',  ( 12.06284766121009966, 32.21085600226960111, -22.25048313876769868 ) ) ;
#41723 = CARTESIAN_POINT ( 'NONE',  ( 0.3082428996584600234, 22.56277195501860078, -8.880561424264220349 ) ) ;
#41725 = AXIS2_PLACEMENT_3D ( 'NONE', #13714, #13967, #30193 ) ;
#41726 = CARTESIAN_POINT ( 'NONE',  ( 68.13393739769620083, -20.61618894467929763, -65.65000000000000568 ) ) ;
#41727 = CARTESIAN_POINT ( 'NONE',  ( 51.64361810415240939, 19.01350634637644532, 16.21999999999999886 ) ) ;
#41728 = EDGE_LOOP ( 'NONE', ( #40486, #33874, #20267, #48532, #33685 ) ) ;
#41729 =( BOUNDED_CURVE ( )  B_SPLINE_CURVE ( 3, ( #51034, #31093, #23226, #47623 ),
 .UNSPECIFIED., .F., .T. ) 
 B_SPLINE_CURVE_WITH_KNOTS ( ( 4, 4 ),
 ( 4.712388980384688786, 5.070260775219134430 ),
 .UNSPECIFIED. ) 
 CURVE ( )  GEOMETRIC_REPRESENTATION_ITEM ( )  RATIONAL_B_SPLINE_CURVE ( ( 1.000000000000000000, 0.9893557610490355536, 0.9893557610490355536, 1.000000000000000000 ) ) 
 REPRESENTATION_ITEM ( '' )  );
#41730 = CARTESIAN_POINT ( 'NONE',  ( -6.526761852427129362, -46.19170520793110057, -5.162139400474170081 ) ) ;
#41731 = CARTESIAN_POINT ( 'NONE',  ( 47.61834138556270091, 23.27905552449800197, -54.71304456415500539 ) ) ;
#41732 = CARTESIAN_POINT ( 'NONE',  ( 71.25019707560589666, 0.8838110553206759423, -70.77727272727270247 ) ) ;
#41733 = CARTESIAN_POINT ( 'NONE',  ( 63.13616699414190236, 0.9259537755896120048, -62.33000265676009377 ) ) ;
#41734 = CARTESIAN_POINT ( 'NONE',  ( 60.89647461220410207, 14.20609866861669879, -47.10144183209600044 ) ) ;
#41735 = CARTESIAN_POINT ( 'NONE',  ( 41.53147733802239827, 13.48015055944119922, -5.331435674896719767 ) ) ;
#41736 = CARTESIAN_POINT ( 'NONE',  ( 10.63552672802458687, -20.03320595643863911, -57.63175854304461865 ) ) ;
#41737 = CARTESIAN_POINT ( 'NONE',  ( 52.87018954733409970, 18.40735846197139836, -48.66536493865070412 ) ) ;
#41738 = DIRECTION ( 'NONE',  ( 1.000000000000000000, 0.000000000000000000, 0.000000000000000000 ) ) ;
#41739 = CARTESIAN_POINT ( 'NONE',  ( 56.38058255011799957, -47.94564697141260012, -48.46858237008240167 ) ) ;
#41740 = CARTESIAN_POINT ( 'NONE',  ( 18.89370190350303602, -21.85803478350294426, -66.82003588566664121 ) ) ;
#41741 = CARTESIAN_POINT ( 'NONE',  ( 52.18370254490579896, 21.34631496022210229, -54.18358737671120196 ) ) ;
#41742 = CARTESIAN_POINT ( 'NONE',  ( 63.50128955454680124, 1.245298479525740021, -69.32855572113911080 ) ) ;
#41743 = DIRECTION ( 'NONE',  ( 0.000000000000000000, -1.000000000000000000, 0.000000000000000000 ) ) ;
#41744 = CARTESIAN_POINT ( 'NONE',  ( 18.20460759450573107, -23.32129168142665776, -75.92435657186162246 ) ) ;
#41745 = EDGE_LOOP ( 'NONE', ( #29500, #9360, #222, #22508 ) ) ;
#41746 = CARTESIAN_POINT ( 'NONE',  ( 13.36620148929459972, -22.10326818851440223, -73.47554475576528432 ) ) ;
#41747 = CARTESIAN_POINT ( 'NONE',  ( 10.48840365866050028, 31.96111183504329745, -45.62648676466370290 ) ) ;
#41748 = CARTESIAN_POINT ( 'NONE',  ( 45.14832757675640096, 2.060512883921409966, -35.14999999999999858 ) ) ;
#41749 = CARTESIAN_POINT ( 'NONE',  ( 65.34026062434320181, -32.03876047116569481, -17.56708739201410197 ) ) ;
#41750 = CARTESIAN_POINT ( 'NONE',  ( 9.080919143135764315, -11.95389120226177226, -80.66002922336500092 ) ) ;
#41751 = ORIENTED_EDGE ( 'NONE', *, *, #29740, .T. ) ;
#41752 = ORIENTED_EDGE ( 'NONE', *, *, #27247, .F. ) ;
#41753 = CARTESIAN_POINT ( 'NONE',  ( 68.13393739769620083, -49.36618894467930829, -69.74999999999998579 ) ) ;
#41754 = EDGE_CURVE ( 'NONE', #121, #19573, #27822, .T. ) ;
#41755 = VERTEX_POINT ( 'NONE', #14278 ) ;
#41756 = CARTESIAN_POINT ( 'NONE',  ( 11.18874931098019943, -64.42258565248579316, -45.43117042558289853 ) ) ;
#41757 = CARTESIAN_POINT ( 'NONE',  ( 57.02224680057370421, -45.69358534429309771, -26.17123580714500264 ) ) ;
#41758 = DIRECTION ( 'NONE',  ( 0.7071067811865473507, 0.7071067811865476838, 0.000000000000000000 ) ) ;
#41759 = CARTESIAN_POINT ( 'NONE',  ( -0.1295185695944109927, -31.87964491196989414, -84.65000000000000568 ) ) ;
#41760 = LINE ( 'NONE', #13229, #49403 ) ;
#41761 = EDGE_LOOP ( 'NONE', ( #7161, #17279, #45602, #43937 ) ) ;
#41762 = VECTOR ( 'NONE', #31053, 1000.000000000000114 ) ;
#41763 = CARTESIAN_POINT ( 'NONE',  ( 46.87892044299400141, 7.006504445231336753, -55.92504309812742491 ) ) ;
#41764 = CIRCLE ( 'NONE', #35087, 16.00000000000000000 ) ;
#41765 = VECTOR ( 'NONE', #43002, 1000.000000000000000 ) ;
#41766 = EDGE_LOOP ( 'NONE', ( #31809, #47183, #22143, #47253, #20449 ) ) ;
#41767 = CARTESIAN_POINT ( 'NONE',  ( 51.20902500803299517, -45.20577485588830058, -12.03792161267199923 ) ) ;
#41768 = CARTESIAN_POINT ( 'NONE',  ( 74.13393739769620083, -20.61618894467929763, -65.65000000000000568 ) ) ;
#41769 = CARTESIAN_POINT ( 'NONE',  ( 23.06214062797170072, -27.61618894467930119, -24.14999999999999858 ) ) ;
#41770 = CARTESIAN_POINT ( 'NONE',  ( 16.13393739769620083, -15.61618894467929941, -47.64999999999999858 ) ) ;
#41771 = VERTEX_POINT ( 'NONE', #49222 ) ;
#41772 = CARTESIAN_POINT ( 'NONE',  ( 29.13393739769619728, -35.78776181993320193, -84.63196841427449613 ) ) ;
#41773 = CARTESIAN_POINT ( 'NONE',  ( 47.06284339357189594, -54.38660427466870573, -75.35929005681109061 ) ) ;
#41774 = CARTESIAN_POINT ( 'NONE',  ( 56.20234825743239782, 13.88381317902869938, -9.796652857581651830 ) ) ;
#41775 = EDGE_CURVE ( 'NONE', #11777, #37946, #6677, .T. ) ;
#41776 = CARTESIAN_POINT ( 'NONE',  ( 50.95182575631829991, -50.95090194773979420, -76.14999999999999147 ) ) ;
#41777 = EDGE_CURVE ( 'NONE', #48296, #10465, #11435, .T. ) ;
#41778 = CARTESIAN_POINT ( 'NONE',  ( 52.21238886552460201, 21.07428037441609803, -53.50655909053360659 ) ) ;
#41779 = CARTESIAN_POINT ( 'NONE',  ( 52.69947992273029769, 19.98405221369169737, -75.94570066465868763 ) ) ;
#41780 = CARTESIAN_POINT ( 'NONE',  ( 59.38732174131899910, 13.88378496296120090, -25.87842628801869793 ) ) ;
#41781 = CARTESIAN_POINT ( 'NONE',  ( 16.87426238886190077, -23.42891363524900328, -73.75743269893999354 ) ) ;
#41782 = ORIENTED_EDGE ( 'NONE', *, *, #35062, .F. ) ;
#41783 = CARTESIAN_POINT ( 'NONE',  ( 22.66096180266447746, -13.24646063577329969, -48.73573848298972422 ) ) ;
#41784 = CARTESIAN_POINT ( 'NONE',  ( -11.21096888454679963, -42.00339129323769782, -6.430231290899450336 ) ) ;
#41785 = CARTESIAN_POINT ( 'NONE',  ( 75.63943938881949691, -41.11453081253210229, -13.15457824778729901 ) ) ;
#41786 = CARTESIAN_POINT ( 'NONE',  ( 72.71255372047811250, 1.170697810385189941, -69.47735791416680229 ) ) ;
#41787 = AXIS2_PLACEMENT_3D ( 'NONE', #45638, #37511, #13675 ) ;
#41788 = AXIS2_PLACEMENT_3D ( 'NONE', #11170, #47840, #27137 ) ;
#41789 = DIRECTION ( 'NONE',  ( 0.000000000000000000, 0.000000000000000000, -1.000000000000000000 ) ) ;
#41790 = AXIS2_PLACEMENT_3D ( 'NONE', #47550, #43866, #19496 ) ;
#41791 = CARTESIAN_POINT ( 'NONE',  ( 23.94246574329788046, -14.28158910010441396, -65.45377657909587299 ) ) ;
#41792 = CONICAL_SURFACE ( 'NONE', #40110, 1.079032500000000727, 0.7853981633974476129 ) ;
#41793 = CARTESIAN_POINT ( 'NONE',  ( 47.29473062437306652, -54.09431091756849241, -75.51963295453231240 ) ) ;
#41794 = CARTESIAN_POINT ( 'NONE',  ( 9.995687254861159943, -53.83794553065769861, -34.69483829921999529 ) ) ;
#41795 = CARTESIAN_POINT ( 'NONE',  ( 71.33393739769628894, 1.883811055320669947, -60.94999999999999574 ) ) ;
#41796 = CARTESIAN_POINT ( 'NONE',  ( 76.30778676816969153, -43.27873611837556922, -13.86615964815592683 ) ) ;
#41797 = CARTESIAN_POINT ( 'NONE',  ( 16.13393739769620083, -1.182432214938700099, -34.64999999999999858 ) ) ;
#41798 = ORIENTED_EDGE ( 'NONE', *, *, #44852, .F. ) ;
#41799 = CARTESIAN_POINT ( 'NONE',  ( 23.58208950757730094, -15.43807525510060152, -57.05973213505619412 ) ) ;
#41800 = CARTESIAN_POINT ( 'NONE',  ( 64.70718024653930911, 1.310552739454400095, -60.94577717611679901 ) ) ;
#41801 = ORIENTED_EDGE ( 'NONE', *, *, #46107, .T. ) ;
#41802 = DIRECTION ( 'NONE',  ( -0.8090169943749462300, -0.5877852522924749135, 0.000000000000000000 ) ) ;
#41803 = CARTESIAN_POINT ( 'NONE',  ( 60.75061855898859875, -45.69690118108319865, -47.68872599397300149 ) ) ;
#41804 = CARTESIAN_POINT ( 'NONE',  ( 22.90000843106822259, -14.87822356394483059, -74.81246489664891897 ) ) ;
#41805 = CARTESIAN_POINT ( 'NONE',  ( 14.06315599067715283, -23.32126188359937657, -62.09098641193147472 ) ) ;
#41807 = CARTESIAN_POINT ( 'NONE',  ( 15.09848396724155961, -7.705177579893296880, -35.25066358517401710 ) ) ;
#41806 = CARTESIAN_POINT ( 'NONE',  ( 44.69989113218067445, 8.776768675800711961, -63.26780307294824013 ) ) ;
#41808 = DIRECTION ( 'NONE',  ( 0.000000000000000000, 0.000000000000000000, -1.000000000000000000 ) ) ;
#41809 = CARTESIAN_POINT ( 'NONE',  ( 41.71811382534419721, -45.72808319846629388, -6.599653652364029455 ) ) ;
#41810 = ORIENTED_EDGE ( 'NONE', *, *, #47528, .T. ) ;
#41811 = ORIENTED_EDGE ( 'NONE', *, *, #49644, .T. ) ;
#41812 = EDGE_CURVE ( 'NONE', #23932, #1009, #2744, .T. ) ;
#41813 = ORIENTED_EDGE ( 'NONE', *, *, #28477, .F. ) ;
#41814 = CARTESIAN_POINT ( 'NONE',  ( -22.75275928769006839, -18.47887437259823429, -54.69860443186151855 ) ) ;
#41815 = CARTESIAN_POINT ( 'NONE',  ( 53.27482191496699926, -49.51724129999239921, -49.18843185985679867 ) ) ;
#41816 = CARTESIAN_POINT ( 'NONE',  ( 60.86539860968923676, 14.21958044004319532, -47.09330236170970352 ) ) ;
#41817 = EDGE_CURVE ( 'NONE', #37257, #21277, #16435, .T. ) ;
#41818 = CARTESIAN_POINT ( 'NONE',  ( 55.64349245618699769, -51.00987811372980474, -53.26417807816250161 ) ) ;
#41819 = EDGE_CURVE ( 'NONE', #16471, #1290, #991, .T. ) ;
#41820 = VERTEX_POINT ( 'NONE', #22378 ) ;
#41821 = EDGE_CURVE ( 'NONE', #4059, #21277, #30243, .T. ) ;
#41822 = ORIENTED_EDGE ( 'NONE', *, *, #23177, .T. ) ;
#41823 = CARTESIAN_POINT ( 'NONE',  ( 11.13393739770110002, -63.48207374982479934, -22.73376795960439978 ) ) ;
#41824 = CARTESIAN_POINT ( 'NONE',  ( 47.64143405402000297, 23.30250925608569901, -55.14905519569659731 ) ) ;
#41825 = B_SPLINE_CURVE_WITH_KNOTS ( 'NONE', 3,
 ( #14675, #22778, #6558, #22263, #39057, #41946, #22004, #19118, #34055, #3150 ),
 .UNSPECIFIED., .F., .F.,
 ( 4, 2, 2, 2, 4 ),
 ( -5.804775000000000375E-14, 0.9800148840114050186, 2.548038698429749616, 5.056876801499090135, 7.840119072091650487 ),
 .UNSPECIFIED. ) ;
#41826 = CARTESIAN_POINT ( 'NONE',  ( 3.633937397696210159, -22.83306730954970121, -34.64999999999999858 ) ) ;
#41827 = CIRCLE ( 'NONE', #15942, 6.999999999999999112 ) ;
#41828 = VERTEX_POINT ( 'NONE', #5452 ) ;
#41829 = CARTESIAN_POINT ( 'NONE',  ( 24.04491473693991921, -15.63666989667861174, -49.50848968882522172 ) ) ;
#41830 = CARTESIAN_POINT ( 'NONE',  ( 52.47362271920999888, -50.54282858732130279, -76.54035590516859600 ) ) ;
#41831 = CARTESIAN_POINT ( 'NONE',  ( 60.87675474826550470, 14.21249462454519907, -47.03427939643230360 ) ) ;
#41832 = CIRCLE ( 'NONE', #35958, 16.33504667647529729 ) ;
#41833 = CARTESIAN_POINT ( 'NONE',  ( 19.09934987693050346, -22.88207336569690042, -76.38915131457939367 ) ) ;
#41834 = B_SPLINE_CURVE_WITH_KNOTS ( 'NONE', 3,
 ( #50800, #14888, #30853, #27705, #4631, #12506, #15924, #19592, #28475, #31880, #44474, #40029, #40287, #39773, #16172, #8837, #8581, #3876, #20097, #24009, #40541, #51820, #19844, #35582, #11999, #24523 ),
 .UNSPECIFIED., .F., .F.,
 ( 4, 2, 2, 2, 2, 2, 2, 2, 2, 2, 2, 2, 4 ),
 ( 0.000000000000000000, 0.03124985050885574836, 0.06249970101771149672, 0.09374955152656724855, 0.1249994020354229934, 0.1562492525442786551, 0.1874991030531343028, 0.2187489535619900061, 0.2499988040708456538, 0.3124985050885567550, 0.3749982061062678285, 0.4374979071239790129, 0.4999976081416900864 ),
 .UNSPECIFIED. ) ;
#41835 = DIRECTION ( 'NONE',  ( 0.8732394366197182567, 0.4872913772396111343, 0.000000000000000000 ) ) ;
#41836 = CARTESIAN_POINT ( 'NONE',  ( 42.47710464005660214, 13.93869629074949934, -6.396644207099989821 ) ) ;
#41837 = VECTOR ( 'NONE', #51103, 1000.000000000000000 ) ;
#41838 = B_SPLINE_CURVE_WITH_KNOTS ( 'NONE', 3,
 ( #19945, #48005, #40647, #23860, #4745, #39883, #48258, #54, #547, #20712 ),
 .UNSPECIFIED., .F., .F.,
 ( 4, 1, 1, 1, 1, 1, 1, 4 ),
 ( 0.000000000000000000, 0.04151989875101936428, 0.1207388298145684186, 0.1999577608781174798, 0.2791766919418271486, 0.3583956230053761960, 0.4376145540690835611, 0.4999959824775806472 ),
 .UNSPECIFIED. ) ;
#41839 = EDGE_CURVE ( 'NONE', #34457, #5441, #6941, .T. ) ;
#41840 = CARTESIAN_POINT ( 'NONE',  ( 42.37474662285829652, -43.39983076957700092, -4.189334837963389901 ) ) ;
#41841 = CARTESIAN_POINT ( 'NONE',  ( 72.34709478978140851, 1.033004162168289941, -61.37787765298320153 ) ) ;
#41842 = CARTESIAN_POINT ( 'NONE',  ( -5.431977005845720186, 16.07634798542799714, -5.576406780277120667 ) ) ;
#41843 = CARTESIAN_POINT ( 'NONE',  ( 64.19630443091290317, 1.030838547160819907, -70.17805703969949604 ) ) ;
#41844 = DIRECTION ( 'NONE',  ( 1.000000000000000000, 0.000000000000000000, 0.000000000000000000 ) ) ;
#41845 = CARTESIAN_POINT ( 'NONE',  ( 66.13978414627780467, -0.1966566410384200103, -17.02377224954269863 ) ) ;
#41846 = ORIENTED_EDGE ( 'NONE', *, *, #39861, .F. ) ;
#41847 = CARTESIAN_POINT ( 'NONE',  ( 14.35835698848820030, -52.52234239888379363, -75.96669286083250938 ) ) ;
#41848 = DIRECTION ( 'NONE',  ( 0.000000000000000000, 0.000000000000000000, -1.000000000000000000 ) ) ;
#41849 = CARTESIAN_POINT ( 'NONE',  ( 46.38959050561425812, -40.11466081036353160, -55.06739743959177247 ) ) ;
#41850 = CARTESIAN_POINT ( 'NONE',  ( 72.83393739769620367, 0.8838110553206759423, -62.79342862858290886 ) ) ;
#41852 = EDGE_CURVE ( 'NONE', #3678, #1577, #10870, .T. ) ;
#41851 = CARTESIAN_POINT ( 'NONE',  ( 46.68381635779479666, -53.67199518238830080, -75.98463753095340678 ) ) ;
#41853 = CARTESIAN_POINT ( 'NONE',  ( 63.19469565515579745, 1.000225705806889964, -69.04426126474540126 ) ) ;
#41854 = FACE_OUTER_BOUND ( 'NONE', #43493, .T. ) ;
#41855 = CARTESIAN_POINT ( 'NONE',  ( 85.66799001034409855, 17.38381105532069881, -61.58097075742929860 ) ) ;
#41856 = CARTESIAN_POINT ( 'NONE',  ( 56.49779820569929711, 19.52786438580549699, -53.73084179205309852 ) ) ;
#41857 = CARTESIAN_POINT ( 'NONE',  ( 48.25700189825269604, 23.04030082563999926, -55.28230106632420160 ) ) ;
#41858 = AXIS2_PLACEMENT_3D ( 'NONE', #39963, #16366, #28145 ) ;
#41859 = ORIENTED_EDGE ( 'NONE', *, *, #30983, .F. ) ;
#41860 = AXIS2_PLACEMENT_3D ( 'NONE', #31389, #7832, #15690 ) ;
#41861 = CARTESIAN_POINT ( 'NONE',  ( 18.91091419587250044, -22.09931774463699838, -75.21836123916489214 ) ) ;
#41862 = ORIENTED_EDGE ( 'NONE', *, *, #13620, .F. ) ;
#41863 = VECTOR ( 'NONE', #41808, 1000.000000000000000 ) ;
#41864 = CARTESIAN_POINT ( 'NONE',  ( 82.61176995027730641, 14.02130663610568284, -47.15275950339798783 ) ) ;
#41865 = DIRECTION ( 'NONE',  ( 0.8340645993220398013, -0.5516667872527448724, 0.000000000000000000 ) ) ;
#41866 = CARTESIAN_POINT ( 'NONE',  ( 6.187261889072820154, -46.71083452957879700, -20.15000000000000213 ) ) ;
#41868 = CARTESIAN_POINT ( 'NONE',  ( 53.19499043075920497, 17.94716954222059613, -26.84764288680280231 ) ) ;
#41867 = CARTESIAN_POINT ( 'NONE',  ( 83.30156758793411598, 13.69860857563659984, -46.93423283396209911 ) ) ;
#41869 = AXIS2_PLACEMENT_3D ( 'NONE', #2955, #10041, #34387 ) ;
#41870 = CARTESIAN_POINT ( 'NONE',  ( 22.69578901594789855, -18.20166028220740273, -78.57229360328089740 ) ) ;
#41871 = CIRCLE ( 'NONE', #6755, 5.499999999999998224 ) ;
#41872 = CARTESIAN_POINT ( 'NONE',  ( 12.06284766121009966, 32.21085600226960111, -22.25048313876769868 ) ) ;
#41873 = CARTESIAN_POINT ( 'NONE',  ( 56.66909264166819327, -45.11618894467940066, -15.43624580850259953 ) ) ;
#41874 = CARTESIAN_POINT ( 'NONE',  ( 22.68450450196613843, -17.37076082248510289, -40.53613820532829237 ) ) ;
#41875 = B_SPLINE_SURFACE_WITH_KNOTS ( 'NONE', 3, 3, ( 
 ( #51209, #34942, #42835, #39413, #11118, #31257, #15302, #38646, #50942, #50684, #2734, #14781, #31768, #19222, #3513, #27851, #47033, #31517, #3249, #43852, #47288, #7183, #35208, #35471 ),
 ( #27593, #11379, #7948, #19480, #18707, #43601, #30750, #46772, #6930, #24933, #48555, #17109, #48046, #5056, #1113, #20491, #16845, #44361, #4786, #4267, #12144, #28616, #48297, #16572 ),
 ( #20237, #19980, #23898, #35974, #21016, #4518, #24671, #33062, #36226, #848, #24413, #8987, #32527, #337, #16321, #20754, #36482, #13191, #28880, #587, #40945, #32275, #39923, #49088 ),
 ( #29141, #37014, #12663, #45142, #28099, #4019, #93, #44617, #32794, #8466, #36741, #8723, #32021, #16064, #44107, #40686, #48817, #12925, #12394, #44882, #8206, #24152, #40172, #40425 ),
 ( #28356, #25201, #1376, #13694, #49607, #33593, #29654, #41988, #42248, #37276, #45658, #22044, #5316, #38057, #17363, #49346, #9761, #13445, #25456, #6090, #25713, #2151, #17623, #50109 ),
 ( #41207, #33842, #18131, #26240, #14204, #21272, #45404, #34094, #5576, #6346, #41721, #5827, #18383, #21790, #30174, #1632, #41460, #33329, #37799, #49857, #1894, #46194, #22305, #29404 ),
 ( #38312, #29906, #17871, #45924, #34358, #9509, #10277, #21532, #37529, #13947, #10014, #25975, #2399, #50375, #14459, #30427, #9252, #50623, #7126, #11313, #15242, #31191, #3704, #14720 ),
 ( #43286, #27021, #35669, #51398, #23077, #31451, #6870, #46453, #19672, #18645, #18897, #10540, #15498, #23583, #22818, #2928, #39600, #26496, #6602, #51654, #34620, #11570, #19422, #38840 ) ),
 .UNSPECIFIED., .F., .F., .F.,
 ( 4, 1, 1, 1, 1, 4 ),
 ( 4, 2, 2, 2, 2, 2, 2, 2, 2, 2, 2, 4 ),
 ( -1.333460192499999945E-05, 0.2000000000000000111, 0.4000000000000000222, 0.5999999999999999778, 0.8000000000000000444, 1.000000000000000000 ),
 ( -1.333460192499999945E-05, 1.104949632659680159, 2.367749212842169992, 3.156998950456220143, 3.551623819263250326, 4.183023609354489913, 4.647713308159810097, 5.112403006965129393, 5.464321026995399677, 5.816239047025679731, 6.065118473969059565, 6.313997900912440286 ),
 .UNSPECIFIED. ) ;
#41876 = CARTESIAN_POINT ( 'NONE',  ( 8.653191590476110306, -48.77463972988229557, -35.01184033120630090 ) ) ;
#41877 = ORIENTED_EDGE ( 'NONE', *, *, #22759, .T. ) ;
#41878 = ORIENTED_EDGE ( 'NONE', *, *, #21267, .F. ) ;
#41879 = CARTESIAN_POINT ( 'NONE',  ( 11.74347662706570006, -64.88511784619510081, -16.31133514117630057 ) ) ;
#41880 = CARTESIAN_POINT ( 'NONE',  ( 11.13319320311270033, 33.09033149884700009, -45.34134544340819417 ) ) ;
#41881 = DIRECTION ( 'NONE',  ( 0.8090169943749472292, -0.5877852522924734702, 0.000000000000000000 ) ) ;
#41882 = EDGE_CURVE ( 'NONE', #28130, #5735, #46524, .T. ) ;
#41883 =( BOUNDED_CURVE ( )  B_SPLINE_CURVE ( 3, ( #9852, #14042, #30003, #46025 ),
 .UNSPECIFIED., .F., .T. ) 
 B_SPLINE_CURVE_WITH_KNOTS ( ( 4, 4 ),
 ( 4.712388980384689674, 5.497787143782005614 ),
 .UNSPECIFIED. ) 
 CURVE ( )  GEOMETRIC_REPRESENTATION_ITEM ( )  RATIONAL_B_SPLINE_CURVE ( ( 1.000000000000000000, 0.9492530216742079974, 0.9492530216742079974, 1.000000000000000000 ) ) 
 REPRESENTATION_ITEM ( '' )  );
#41884 = CARTESIAN_POINT ( 'NONE',  ( 12.25380415227330033, 34.08744772704470449, -46.27199321459300307 ) ) ;
#41885 = CARTESIAN_POINT ( 'NONE',  ( 12.77233515483190018, -65.50098146117900910, -47.69352623515830203 ) ) ;
#41886 = ORIENTED_EDGE ( 'NONE', *, *, #27679, .T. ) ;
#41887 = EDGE_CURVE ( 'NONE', #4707, #50665, #41530, .T. ) ;
#41888 = CARTESIAN_POINT ( 'NONE',  ( -22.36136842496640043, -21.42584896580819986, -54.21115099506850044 ) ) ;
#41889 = CARTESIAN_POINT ( 'NONE',  ( 63.19893373200898168, -30.31618894467939995, -69.23549003898403953 ) ) ;
#41890 = CARTESIAN_POINT ( 'NONE',  ( 52.64726764441159901, -49.79428164651599786, -48.69236602696069838 ) ) ;
#41891 = CARTESIAN_POINT ( 'NONE',  ( 52.15791131231179634, 19.08239589345419773, -49.32805031943310325 ) ) ;
#41892 = CARTESIAN_POINT ( 'NONE',  ( 62.23727147033270057, -1.604945995984039975, -16.10252877210989908 ) ) ;
#41893 = CARTESIAN_POINT ( 'NONE',  ( 50.58622399129809821, -48.86524564621230127, -76.21981748726450689 ) ) ;
#41894 = VECTOR ( 'NONE', #19604, 1000.000000000000000 ) ;
#41895 = CARTESIAN_POINT ( 'NONE',  ( 56.57680611020050065, -50.33247776572370213, -52.64782081613199693 ) ) ;
#41896 = VERTEX_POINT ( 'NONE', #34692 ) ;
#41897 = CARTESIAN_POINT ( 'NONE',  ( 52.82216258569669520, -49.58646061845040265, -27.28071896258420281 ) ) ;
#41898 = CARTESIAN_POINT ( 'NONE',  ( 9.807870791654629272, -20.47799351597511475, -48.58399859126286202 ) ) ;
#41899 = ORIENTED_EDGE ( 'NONE', *, *, #37649, .F. ) ;
#41900 = CARTESIAN_POINT ( 'NONE',  ( 12.18502729926166595, -55.42069105936809592, -74.66536237510875651 ) ) ;
#41901 = DIRECTION ( 'NONE',  ( 0.8857883891771956009, -0.4640893551880597157, 2.775557561562888270E-17 ) ) ;
#41902 = CARTESIAN_POINT ( 'NONE',  ( 7.922186500973898760, -16.35708704190409790, -80.76368641361838741 ) ) ;
#41903 = CARTESIAN_POINT ( 'NONE',  ( 13.31268657292829971, -51.13566752317600361, -21.89251117597479990 ) ) ;
#41904 = CARTESIAN_POINT ( 'NONE',  ( 54.76877112936399783, 19.42876175676859773, -76.28131348449389293 ) ) ;
#41905 = CARTESIAN_POINT ( 'NONE',  ( 46.50118480118399589, -53.10011392806350727, -76.13977852870850427 ) ) ;
#41906 = VERTEX_POINT ( 'NONE', #17241 ) ;
#41907 = CARTESIAN_POINT ( 'NONE',  ( 54.83244439671879888, 14.27556882037980124, -15.28355485841840000 ) ) ;
#41908 = CARTESIAN_POINT ( 'NONE',  ( 13.56856140308030056, -9.046454919155269891, -78.22868061958250507 ) ) ;
#41909 = CARTESIAN_POINT ( 'NONE',  ( 57.34583854987740636, -50.23863174456870695, -52.73888232562049438 ) ) ;
#41910 = VECTOR ( 'NONE', #9477, 1000.000000000000000 ) ;
#41911 = CARTESIAN_POINT ( 'NONE',  ( 23.15708489307130336, -16.26268599235770296, -36.87639860437320038 ) ) ;
#41912 = DIRECTION ( 'NONE',  ( 1.000000000000000000, 0.000000000000000000, 0.000000000000000000 ) ) ;
#41913 = CIRCLE ( 'NONE', #2599, 20.00000000000000355 ) ;
#41914 = VERTEX_POINT ( 'NONE', #50694 ) ;
#41915 = CARTESIAN_POINT ( 'NONE',  ( 47.44037494016029655, 23.08122949994629991, -75.17655532006401131 ) ) ;
#41916 = CARTESIAN_POINT ( 'NONE',  ( 65.21909306016200958, 1.375383258925270136, -60.85412179317820147 ) ) ;
#41917 = CARTESIAN_POINT ( 'NONE',  ( 75.29749630104785751, -36.46059068598260922, -12.51818644522628610 ) ) ;
#41918 = CARTESIAN_POINT ( 'NONE',  ( 104.6856170952509757, -28.80002732851879088, -29.09832030244561807 ) ) ;
#41919 = CARTESIAN_POINT ( 'NONE',  ( -33.86606260230380627, -15.61618894467806307, -46.39999999999999858 ) ) ;
#41920 = ADVANCED_FACE ( 'NONE', ( #42844 ), #50444, .T. ) ;
#41921 = CARTESIAN_POINT ( 'NONE',  ( 14.34417029198879945, -51.11618894467930119, -74.14999999999999147 ) ) ;
#41923 = EDGE_CURVE ( 'NONE', #10696, #20725, #43233, .T. ) ;
#41922 = CARTESIAN_POINT ( 'NONE',  ( 12.20479792536879948, -10.10644435241950134, -32.14999999999999858 ) ) ;
#41924 = CARTESIAN_POINT ( 'NONE',  ( -9.412135025327549087, 14.13484241487110005, -42.98138733652569954 ) ) ;
#41926 = CARTESIAN_POINT ( 'NONE',  ( 44.17224985740909915, -39.08504712336350195, -69.61925960810538072 ) ) ;
#41925 = CARTESIAN_POINT ( 'NONE',  ( 14.14886614762370165, 1.362847559348080217, -35.02873218748179340 ) ) ;
#41927 = CARTESIAN_POINT ( 'NONE',  ( 61.27342693744519408, 14.00466695065149914, -46.49030966888999927 ) ) ;
#41928 = CARTESIAN_POINT ( 'NONE',  ( -12.67430703014560045, 25.29472265930930064, -51.91878751810720161 ) ) ;
#41929 = ADVANCED_FACE ( 'NONE', ( #46781 ), #27254, .T. ) ;
#41930 = ORIENTED_EDGE ( 'NONE', *, *, #43117, .F. ) ;
#41931 = CARTESIAN_POINT ( 'NONE',  ( 52.83705234978589971, -49.66563195679469800, -48.81125901731440564 ) ) ;
#41932 = ORIENTED_EDGE ( 'NONE', *, *, #45860, .F. ) ;
#41933 = CARTESIAN_POINT ( 'NONE',  ( 46.37276178491875811, 9.011627554650393890, -54.63167819045965246 ) ) ;
#41934 = CARTESIAN_POINT ( 'NONE',  ( 24.04493739796119556, -16.65172873511394869, -73.83399818621970212 ) ) ;
#41935 = CARTESIAN_POINT ( 'NONE',  ( 13.78923984081539977, 19.56813522593770216, -21.52746261380119819 ) ) ;
#41936 = CARTESIAN_POINT ( 'NONE',  ( 56.45642129034870038, 14.19690291267379934, -25.50404404838770134 ) ) ;
#41937 = CARTESIAN_POINT ( 'NONE',  ( 23.17755585561640075, -15.97674090469540076, -48.46909979910559230 ) ) ;
#41938 = FACE_OUTER_BOUND ( 'NONE', #21447, .T. ) ;
#41939 = CARTESIAN_POINT ( 'NONE',  ( 53.44641931178580307, 18.15579562409830316, -49.05897173235240416 ) ) ;
#41940 = CARTESIAN_POINT ( 'NONE',  ( 64.77932207159139466, 0.8936201581567889685, -60.67538646459720297 ) ) ;
#41941 = CARTESIAN_POINT ( 'NONE',  ( 60.75208945151790374, -45.51018815575340426, -47.06168269646809676 ) ) ;
#41942 = CARTESIAN_POINT ( 'NONE',  ( 65.03603135424580728, -15.61618894467929941, -19.52361391316370032 ) ) ;
#41943 = ORIENTED_EDGE ( 'NONE', *, *, #19264, .T. ) ;
#41944 = CARTESIAN_POINT ( 'NONE',  ( 16.83676928204470258, -23.03324507772050111, -73.53726979628909532 ) ) ;
#41945 = AXIS2_PLACEMENT_3D ( 'NONE', #27258, #43272, #3434 ) ;
#41946 = CARTESIAN_POINT ( 'NONE',  ( 57.40277299468780114, 16.17492991088059995, -48.23107244050790143 ) ) ;
#41947 = CYLINDRICAL_SURFACE ( 'NONE', #11149, 7.910999999999997812 ) ;
#41948 = CARTESIAN_POINT ( 'NONE',  ( 73.08914738367541020, 1.188582381068110205, -62.44003653085270145 ) ) ;
#41949 = CIRCLE ( 'NONE', #30224, 38.00000000000000000 ) ;
#41950 = CARTESIAN_POINT ( 'NONE',  ( 11.89948726634279907, -65.43656066622459377, -18.06739951304799874 ) ) ;
#41951 = CARTESIAN_POINT ( 'NONE',  ( 52.87578304523380268, 18.40442787170260175, -48.67531064471670277 ) ) ;
#41952 = CARTESIAN_POINT ( 'NONE',  ( 82.02429831058030629, -41.23866635630079713, -45.87976092105969883 ) ) ;
#41953 = CARTESIAN_POINT ( 'NONE',  ( 22.84259504164056409, -14.71167573906013004, -62.41017214630380039 ) ) ;
#41954 = VECTOR ( 'NONE', #41694, 1000.000000000000000 ) ;
#41955 = CIRCLE ( 'NONE', #10148, 0.5000000000000000000 ) ;
#41956 = CARTESIAN_POINT ( 'NONE',  ( 19.54197421750533081, -9.703304665228225545, -58.11948669415193081 ) ) ;
#41957 = ADVANCED_FACE ( 'NONE', ( #48832 ), #33073, .T. ) ;
#41958 = CARTESIAN_POINT ( 'NONE',  ( 65.01178944337659971, 1.369535599030039963, -70.36855090579189209 ) ) ;
#41959 = ORIENTED_EDGE ( 'NONE', *, *, #25061, .T. ) ;
#41960 = CARTESIAN_POINT ( 'NONE',  ( 8.963661153849718843, -63.19364268998111100, -46.63283991472749790 ) ) ;
#41961 = CARTESIAN_POINT ( 'NONE',  ( 72.72056432233058842, 1.396834109478129804, -68.84999999999999432 ) ) ;
#41962 = ORIENTED_EDGE ( 'NONE', *, *, #39899, .F. ) ;
#41963 = PLANE ( 'NONE',  #35050 ) ;
#41964 = DIRECTION ( 'NONE',  ( 0.000000000000000000, 0.000000000000000000, 1.000000000000000000 ) ) ;
#41965 = CYLINDRICAL_SURFACE ( 'NONE', #20290, 0.4999999999999994449 ) ;
#41966 = CARTESIAN_POINT ( 'NONE',  ( 52.16338521619510260, 18.67182647646719929, -76.93802992565549914 ) ) ;
#41967 = ORIENTED_EDGE ( 'NONE', *, *, #15680, .T. ) ;
#41968 = CARTESIAN_POINT ( 'NONE',  ( 68.13393739769620083, -42.11618894467930119, -65.65000000000000568 ) ) ;
#41969 = CARTESIAN_POINT ( 'NONE',  ( 68.13393739823159478, -1.166188946452521469, -49.15000000374099898 ) ) ;
#41970 = CARTESIAN_POINT ( 'NONE',  ( -19.86606260230379917, -15.61618894467933494, -19.14999999999999858 ) ) ;
#41971 = CARTESIAN_POINT ( 'NONE',  ( 13.85732796729022986, -23.21488026636175306, -66.10023604892785443 ) ) ;
#41972 = CARTESIAN_POINT ( 'NONE',  ( 9.336894014525560337, -20.28340667082309778, -48.60080040178890215 ) ) ;
#41973 = CARTESIAN_POINT ( 'NONE',  ( 21.64576443335199585, -11.59628691946671886, -56.25250486724262799 ) ) ;
#41974 = CARTESIAN_POINT ( 'NONE',  ( 45.48467495382262626, -38.09807257052023743, -62.89625465325211451 ) ) ;
#41975 = ORIENTED_EDGE ( 'NONE', *, *, #1070, .F. ) ;
#41976 = CARTESIAN_POINT ( 'NONE',  ( 68.13393739769618662, 0.9838110553206419473, -65.65000000000000568 ) ) ;
#41977 = CARTESIAN_POINT ( 'NONE',  ( 22.63087827937219743, -11.96975877461539994, -42.06986027349229573 ) ) ;
#41978 = CARTESIAN_POINT ( 'NONE',  ( 53.26966627192010151, -49.51099171206949734, -49.16957340299519785 ) ) ;
#41979 = CARTESIAN_POINT ( 'NONE',  ( 9.682426609870530498, -12.74603349750159964, -32.14999999999999858 ) ) ;
#41980 = CARTESIAN_POINT ( 'NONE',  ( 14.23591865958499980, 20.10714342530040000, -75.06145659859170394 ) ) ;
#41981 = CARTESIAN_POINT ( 'NONE',  ( 11.27236231982013770, -9.289945855619381021, -51.08399742131821597 ) ) ;
#41982 = VECTOR ( 'NONE', #47111, 1000.000000000000000 ) ;
#41983 = CARTESIAN_POINT ( 'NONE',  ( 42.30722599539220141, -45.03182078332450544, -6.083982332172880092 ) ) ;
#41984 = CARTESIAN_POINT ( 'NONE',  ( 47.64143405400680109, -54.53488714545009941, -74.14999999999999147 ) ) ;
#41985 = AXIS2_PLACEMENT_3D ( 'NONE', #32124, #30010, #17719 ) ;
#41986 = CARTESIAN_POINT ( 'NONE',  ( 7.889072482538179720, -15.54602314267300045, -60.51037732077569586 ) ) ;
#41987 = ORIENTED_EDGE ( 'NONE', *, *, #37088, .F. ) ;
#41988 = CARTESIAN_POINT ( 'NONE',  ( 54.06806631522740503, -48.25978409922480239, -26.47101390624369799 ) ) ;
#41989 = EDGE_CURVE ( 'NONE', #9028, #16471, #12935, .T. ) ;
#41990 = CARTESIAN_POINT ( 'NONE',  ( 56.57214737956470429, -50.73313417699420569, -74.14929904960109752 ) ) ;
#41991 = CARTESIAN_POINT ( 'NONE',  ( 9.131712051400846519, -19.42118211742113587, -40.34903064087519198 ) ) ;
#41993 = CARTESIAN_POINT ( 'NONE',  ( 41.24914385796110139, -39.67975193718725535, -79.95434115774115469 ) ) ;
#41992 = CARTESIAN_POINT ( 'NONE',  ( 1.813848851336939738, 24.38879552280330287, -10.83645643805460068 ) ) ;
#41994 = LINE ( 'NONE', #6094, #2056 ) ;
#41995 = DIRECTION ( 'NONE',  ( 0.5720614028176828070, -0.4156269377774550189, -0.7071067811865477948 ) ) ;
#41996 = EDGE_CURVE ( 'NONE', #14211, #46311, #34829, .T. ) ;
#41997 = EDGE_LOOP ( 'NONE', ( #13173, #32324, #42370, #33436 ) ) ;
#41998 = CARTESIAN_POINT ( 'NONE',  ( -2.623662900336269921, -48.66391853426490144, -4.386168476009399519 ) ) ;
#41999 = CARTESIAN_POINT ( 'NONE',  ( 47.54275987186800023, 23.32401250507800228, -54.69604644530389947 ) ) ;
#42000 = CARTESIAN_POINT ( 'NONE',  ( 22.60295963412389852, -10.99248356359692380, -65.59471942785054921 ) ) ;
#42001 = CARTESIAN_POINT ( 'NONE',  ( 63.34300561417320807, 1.326324093417230232, -62.46048956832549948 ) ) ;
#42002 = CARTESIAN_POINT ( 'NONE',  ( 13.09359062182869948, 19.38068958424499755, -21.36973451213659914 ) ) ;
#42003 = CARTESIAN_POINT ( 'NONE',  ( -18.49575789335964160, 18.87413034886438368, 11.97999999999999865 ) ) ;
#42004 = CARTESIAN_POINT ( 'NONE',  ( 11.86319492706100043, 34.16543365841759794, -17.45438025052920139 ) ) ;
#42005 = CARTESIAN_POINT ( 'NONE',  ( 7.768034174689467442, 29.40613003788450186, -20.78409677699325897 ) ) ;
#42006 = DIRECTION ( 'NONE',  ( -0.2260571801428161165, 7.216449660063443557E-16, 0.9741140340359943917 ) ) ;
#42007 = CARTESIAN_POINT ( 'NONE',  ( 51.13393739769659874, -50.61618894467899565, 16.85000000000000142 ) ) ;
#42008 = DIRECTION ( 'NONE',  ( 0.000000000000000000, 0.000000000000000000, -1.000000000000000000 ) ) ;
#42009 = CARTESIAN_POINT ( 'NONE',  ( 22.90093739934872374, -15.62378126355319985, -66.45317726807988379 ) ) ;
#42010 = CARTESIAN_POINT ( 'NONE',  ( 56.09099783350909973, 19.70331726233800040, -53.77926613765360031 ) ) ;
#42011 = FACE_OUTER_BOUND ( 'NONE', #47675, .T. ) ;
#42012 = CARTESIAN_POINT ( 'NONE',  ( 68.13393739823159478, -1.166188944768318247, -82.14999999999838565 ) ) ;
#42013 = CARTESIAN_POINT ( 'NONE',  ( 18.13393739769639978, 10.38381105532070059, -35.14999999999999858 ) ) ;
#42014 = DIRECTION ( 'NONE',  ( 0.000000000000000000, -3.054848041326977894E-12, 1.000000000000000000 ) ) ;
#42015 = CARTESIAN_POINT ( 'NONE',  ( 72.67019432586680239, 1.382578538659579914, -62.08265642326169598 ) ) ;
#42016 = CARTESIAN_POINT ( 'NONE',  ( 65.04199857771129700, -32.25459573065409558, -17.84398015535190041 ) ) ;
#42017 = EDGE_CURVE ( 'NONE', #48724, #37163, #15410, .T. ) ;
#42018 = CARTESIAN_POINT ( 'NONE',  ( 54.13393739769620083, -15.61618894467929941, 6.349999999999999645 ) ) ;
#42019 = EDGE_LOOP ( 'NONE', ( #27519, #48734, #37427, #36625, #38733 ) ) ;
#42020 = VERTEX_POINT ( 'NONE', #20765 ) ;
#42021 = CARTESIAN_POINT ( 'NONE',  ( 48.25528797735789510, 23.04103089059050191, -55.30957496453539335 ) ) ;
#42022 = EDGE_CURVE ( 'NONE', #39126, #28421, #44086, .T. ) ;
#42023 = CARTESIAN_POINT ( 'NONE',  ( 49.27279687193958324, -2.461837687523397378, -15.69245132549682431 ) ) ;
#42024 = VERTEX_POINT ( 'NONE', #12404 ) ;
#42025 = CARTESIAN_POINT ( 'NONE',  ( 12.36185612747330076, -65.36949588230230290, -46.58846889824079796 ) ) ;
#42026 = CARTESIAN_POINT ( 'NONE',  ( 56.96971367505879869, -45.85215597628009476, -26.22514245738749850 ) ) ;
#42027 = CARTESIAN_POINT ( 'NONE',  ( 24.04493438893774737, -15.62471349072081139, -77.50801464174854516 ) ) ;
#42028 = CARTESIAN_POINT ( 'NONE',  ( 10.47406283454438203, -59.02534396924340143, -45.62066736167659542 ) ) ;
#42029 = VERTEX_POINT ( 'NONE', #16857 ) ;
#42030 = AXIS2_PLACEMENT_3D ( 'NONE', #21104, #32622, #12750 ) ;
#42031 = DIRECTION ( 'NONE',  ( 0.000000000000000000, -0.9319748226751538578, -0.3625230060280530409 ) ) ;
#42032 = CARTESIAN_POINT ( 'NONE',  ( 46.44895917027370302, 6.966159365888272781, -58.07489105607155011 ) ) ;
#42033 = ORIENTED_EDGE ( 'NONE', *, *, #8742, .T. ) ;
#42034 = CARTESIAN_POINT ( 'NONE',  ( 47.51452104107959684, -45.56742998877640360, -10.18306270678010073 ) ) ;
#42035 = CARTESIAN_POINT ( 'NONE',  ( 21.72396248402345975, -21.29268565403493696, -34.04455158046467744 ) ) ;
#42036 = CARTESIAN_POINT ( 'NONE',  ( 16.35031946894069677, 19.87963569218470283, -20.80740584792750170 ) ) ;
#42037 = CARTESIAN_POINT ( 'NONE',  ( 18.57770503654736061, -22.23212114670332795, -49.23455185029879289 ) ) ;
#42038 = CARTESIAN_POINT ( 'NONE',  ( 68.13393739769620083, 17.38381105532069881, -65.65000000000000568 ) ) ;
#42039 = CARTESIAN_POINT ( 'NONE',  ( 47.06489453142850010, -54.53966941020699721, -75.17791912558919876 ) ) ;
#42040 = CARTESIAN_POINT ( 'NONE',  ( 60.59298274472079981, 13.73382843762409777, -10.31706438195179842 ) ) ;
#42041 = CARTESIAN_POINT ( 'NONE',  ( 50.36549737501839985, -50.07561419642740219, -76.14999999999999147 ) ) ;
#42042 = CARTESIAN_POINT ( 'NONE',  ( 28.63393739769619728, -12.15208732954159920, -35.14999999999999858 ) ) ;
#42043 =( BOUNDED_CURVE ( )  B_SPLINE_CURVE ( 2, ( #16818, #4758, #17591 ),
 .UNSPECIFIED., .F., .T. ) 
 B_SPLINE_CURVE_WITH_KNOTS ( ( 3, 3 ),
 ( -0.06696923885014899325, 0.06696923885011449307 ),
 .UNSPECIFIED. ) 
 CURVE ( )  GEOMETRIC_REPRESENTATION_ITEM ( )  RATIONAL_B_SPLINE_CURVE ( ( 1.000000000000000000, 0.9977583984878120038, 1.000000000000000000 ) ) 
 REPRESENTATION_ITEM ( '' )  );
#42044 = B_SPLINE_SURFACE_WITH_KNOTS ( 'NONE', 3, 3, ( 
 ( #686, #42995, #48660, #40274, #48135, #22785 ),
 ( #18864, #38804, #34848, #4620, #4104, #24248 ),
 ( #2898, #27237, #35105, #26989, #28459, #44459 ),
 ( #12491, #16674, #24508, #43255, #4362, #50848 ),
 ( #14941, #11020, #31162, #30904, #20082, #46934 ),
 ( #36074, #12759, #8042, #23996, #40017, #8566 ),
 ( #39063, #23043, #40527, #32374, #3156, #19125 ),
 ( #51104, #20333, #28716, #20589, #15207, #32117 ),
 ( #11277, #180, #44717, #47190, #16159, #44200 ),
 ( #12235, #36321, #32633, #8298, #28197, #432 ),
 ( #48393, #36583, #44980, #9602, #29234, #9351 ),
 ( #14043, #32896, #21369, #17205, #41558, #25296 ),
 ( #37897, #28981, #33937, #25555, #33425, #8823 ),
 ( #4885, #24774, #20852, #41818, #41302, #5674 ),
 ( #40783, #17971, #5411, #17715, #25810, #48928 ),
 ( #9082, #33683, #13539, #37117, #9853, #21622 ) ),
 .UNSPECIFIED., .F., .F., .F.,
 ( 4, 2, 2, 2, 2, 2, 2, 4 ),
 ( 4, 1, 1, 4 ),
 ( 0.000000000000000000, 1.325233610615540014, 2.839786308461869968, 3.786381744615829881, 4.259679462692810503, 5.016955811615980032, 6.228597969893040265, 7.536345830558680348 ),
 ( 0.000000000000000000, 0.3333333333333329818, 0.6666666666666670737, 1.000000000000000000 ),
 .UNSPECIFIED. ) ;
#42045 = CARTESIAN_POINT ( 'NONE',  ( 51.55044211529290266, 20.01891078301889948, -76.08578284841350126 ) ) ;
#42046 = CARTESIAN_POINT ( 'NONE',  ( 57.47755809313429864, 13.88376667797570008, -25.39851124859779929 ) ) ;
#42047 = CARTESIAN_POINT ( 'NONE',  ( 17.82483774787520048, -23.27958272219449753, -77.71837925212109610 ) ) ;
#42048 = ORIENTED_EDGE ( 'NONE', *, *, #15076, .T. ) ;
#42049 = DIRECTION ( 'NONE',  ( 0.000000000000000000, 0.000000000000000000, -1.000000000000000000 ) ) ;
#42050 = EDGE_CURVE ( 'NONE', #23386, #44397, #29467, .T. ) ;
#42051 = CARTESIAN_POINT ( 'NONE',  ( 73.15108049797990475, 0.8888742037077599356, -62.35931220671550790 ) ) ;
#42052 = FACE_OUTER_BOUND ( 'NONE', #43476, .T. ) ;
#42053 = CARTESIAN_POINT ( 'NONE',  ( 72.72276342993330900, 1.080095028449130190, -69.50719766003020084 ) ) ;
#42054 = CARTESIAN_POINT ( 'NONE',  ( 9.366504787982940172, -15.61629640169840094, -69.84717978381009118 ) ) ;
#42055 = VECTOR ( 'NONE', #20348, 1000.000000000000114 ) ;
#42056 = CARTESIAN_POINT ( 'NONE',  ( 24.04493737838489409, -16.65173502485940205, -35.83399554789317421 ) ) ;
#42057 = CARTESIAN_POINT ( 'NONE',  ( 24.04477596867337041, -15.61618922203197357, -43.50766101656756746 ) ) ;
#42058 = CARTESIAN_POINT ( 'NONE',  ( 41.62693577923219834, 12.58261528623730108, -3.742293453206330334 ) ) ;
#42059 = CARTESIAN_POINT ( 'NONE',  ( 11.97526630703813488, -21.02750917104722461, -79.16115263443646199 ) ) ;
#42060 = CARTESIAN_POINT ( 'NONE',  ( 19.55572504588462124, 24.23719298256126820, -75.54211829725619509 ) ) ;
#42061 = CARTESIAN_POINT ( 'NONE',  ( 63.63393739769619373, -53.11618894467930119, 16.35000000000000142 ) ) ;
#42062 = CARTESIAN_POINT ( 'NONE',  ( 22.89855973853233451, -15.80993545744688333, -62.46194232920734635 ) ) ;
#42063 = CARTESIAN_POINT ( 'NONE',  ( 18.11395681486079923, -51.16362366046149646, -74.57010117178208475 ) ) ;
#42064 = DIRECTION ( 'NONE',  ( 0.000000000000000000, 1.000000000000000000, 0.000000000000000000 ) ) ;
#42065 = VERTEX_POINT ( 'NONE', #28368 ) ;
#42066 = CARTESIAN_POINT ( 'NONE',  ( 22.33916946346290189, -11.49286633441439953, -50.88065551209390236 ) ) ;
#42067 = CARTESIAN_POINT ( 'NONE',  ( 63.84704430308629952, 1.199410787637519960, -61.48962906069409939 ) ) ;
#42068 = ORIENTED_EDGE ( 'NONE', *, *, #25652, .T. ) ;
#42069 = CARTESIAN_POINT ( 'NONE',  ( 52.68908936341578908, 18.51792035577400242, -48.47378032971769812 ) ) ;
#42070 = CARTESIAN_POINT ( 'NONE',  ( 40.79482532997379707, 8.392676044869128660, -82.14319696191608955 ) ) ;
#42071 = CARTESIAN_POINT ( 'NONE',  ( 9.909523820307871489, -18.91395403005434517, -75.69203052425869771 ) ) ;
#42072 = CARTESIAN_POINT ( 'NONE',  ( 16.92763237404272658, -23.48995300663941066, -61.97569791650314386 ) ) ;
#42074 = CARTESIAN_POINT ( 'NONE',  ( 18.64395816326117483, -9.025107475687542902, -54.46300130049679922 ) ) ;
#42073 = CARTESIAN_POINT ( 'NONE',  ( 43.63607212596370033, 8.691589028069600431, -68.42176024395821798 ) ) ;
#42075 = CARTESIAN_POINT ( 'NONE',  ( 10.70613124693099927, -19.68844507227139928, -81.23899999999999011 ) ) ;
#42076 = DIRECTION ( 'NONE',  ( 0.000000000000000000, 0.000000000000000000, 1.000000000000000000 ) ) ;
#42077 = ORIENTED_EDGE ( 'NONE', *, *, #34787, .T. ) ;
#42078 = VERTEX_POINT ( 'NONE', #28891 ) ;
#42079 = EDGE_CURVE ( 'NONE', #12246, #36840, #21027, .T. ) ;
#42080 = VERTEX_POINT ( 'NONE', #20248 ) ;
#42081 = CARTESIAN_POINT ( 'NONE',  ( 61.08134338338769709, -45.33768279644640131, -46.82317710124809906 ) ) ;
#42082 = CARTESIAN_POINT ( 'NONE',  ( 52.77282165433940264, -49.72616459520740051, -48.90295367273579785 ) ) ;
#42083 = LINE ( 'NONE', #29233, #33254 ) ;
#42084 = DIRECTION ( 'NONE',  ( 0.000000000000000000, -1.000000000000000000, 0.000000000000000000 ) ) ;
#42085 = ORIENTED_EDGE ( 'NONE', *, *, #36916, .T. ) ;
#42086 = VERTEX_POINT ( 'NONE', #1387 ) ;
#42087 = CARTESIAN_POINT ( 'NONE',  ( 14.34417021472880016, 20.88381098710710049, -23.14999995404869892 ) ) ;
#42088 = CARTESIAN_POINT ( 'NONE',  ( 28.18536260820836148, -8.658295355271512506, -34.89146800830130957 ) ) ;
#42089 = DIRECTION ( 'NONE',  ( -1.000000000000000000, 0.000000000000000000, 0.000000000000000000 ) ) ;
#42090 = AXIS2_PLACEMENT_3D ( 'NONE', #7135, #25987, #50118 ) ;
#42091 = ORIENTED_EDGE ( 'NONE', *, *, #4399, .F. ) ;
#42092 = CARTESIAN_POINT ( 'NONE',  ( 46.47536507427530239, 8.886826513564159313, -54.64999999999999858 ) ) ;
#42094 = CARTESIAN_POINT ( 'NONE',  ( 52.14531167019610081, -49.88992925342000007, -76.93287919525420193 ) ) ;
#42093 = CIRCLE ( 'NONE', #20334, 14.49999999999999822 ) ;
#42095 = CARTESIAN_POINT ( 'NONE',  ( 61.01670509829179423, 14.23156206065599960, -47.38493383915780299 ) ) ;
#42096 = CARTESIAN_POINT ( 'NONE',  ( 12.93056411727340205, -22.78034606313060095, -74.64633483117989954 ) ) ;
#42097 = CARTESIAN_POINT ( 'NONE',  ( 57.50723796701959856, -45.11618894467940066, -25.33268394681470070 ) ) ;
#42098 = CARTESIAN_POINT ( 'NONE',  ( 44.76368420724840291, 13.86998310020809910, -7.024004829805569727 ) ) ;
#42099 = CARTESIAN_POINT ( 'NONE',  ( 41.59466734061630433, -44.04155483751850397, -4.344851959883419212 ) ) ;
#42100 = DIRECTION ( 'NONE',  ( 0.5685928097855449392, 0.5944782866685399680, -0.5685928097855409424 ) ) ;
#42101 = CARTESIAN_POINT ( 'NONE',  ( -2.927826905750240183, 17.96742634125930138, -5.740514720776229929 ) ) ;
#42102 = CARTESIAN_POINT ( 'NONE',  ( 64.20744331450271147, 1.091543525800269920, -70.18026150519258977 ) ) ;
#42103 = DIRECTION ( 'NONE',  ( 0.000000000000000000, 0.000000000000000000, 1.000000000000000000 ) ) ;
#42104 = DIRECTION ( 'NONE',  ( 0.000000000000000000, 0.000000000000000000, -1.000000000000000000 ) ) ;
#42105 = VERTEX_POINT ( 'NONE', #44894 ) ;
#42106 = DIRECTION ( 'NONE',  ( 0.4936210606096666509, 0.8696770943991728453, 0.000000000000000000 ) ) ;
#42107 = AXIS2_PLACEMENT_3D ( 'NONE', #43279, #51391, #15489 ) ;
#42108 = ADVANCED_FACE ( 'NONE', ( #36240 ), #348, .T. ) ;
#42109 = CARTESIAN_POINT ( 'NONE',  ( 40.16190654090002710, 1.841152499458795999, 7.944363289481099599 ) ) ;
#42110 = CARTESIAN_POINT ( 'NONE',  ( 8.815605938792600682, 32.05029769220720226, -46.67186391141279955 ) ) ;
#42111 = EDGE_CURVE ( 'NONE', #35016, #12167, #8999, .T. ) ;
#42112 = EDGE_CURVE ( 'NONE', #38586, #26354, #25961, .T. ) ;
#42113 = CARTESIAN_POINT ( 'NONE',  ( 20.29013637266969994, -10.24695330870310173, -32.14999999999999858 ) ) ;
#42114 = EDGE_CURVE ( 'NONE', #28243, #51085, #51603, .T. ) ;
#42115 = CARTESIAN_POINT ( 'NONE',  ( 63.25638208530150308, 1.265664290790570190, -68.85308916926389600 ) ) ;
#42116 = CARTESIAN_POINT ( 'NONE',  ( 47.88434815289430446, -54.36569397686789529, -54.74340954032749806 ) ) ;
#42117 = B_SPLINE_CURVE_WITH_KNOTS ( 'NONE', 3,
 ( #23816, #51378, #12312, #35378, #36150, #8379, #27510, #3684, #8125, #35646, #24329, #24070, #28273, #4183, #27250, #39835, #51631, #43512 ),
 .UNSPECIFIED., .F., .F.,
 ( 4, 2, 2, 2, 2, 2, 2, 2, 4 ),
 ( 0.000000000000000000, 0.06250019386976815583, 0.1250003877395363117, 0.1875005816093044675, 0.2500007754790726233, 0.3125009693488408624, 0.3750011632186091570, 0.4375013570883773961, 0.5000015509581456907 ),
 .UNSPECIFIED. ) ;
#42118 = CARTESIAN_POINT ( 'NONE',  ( 17.97808210774817184, -7.902931223253473192, -45.08245229423729938 ) ) ;
#42119 = AXIS2_PLACEMENT_3D ( 'NONE', #17508, #49495, #13582 ) ;
#42120 = CARTESIAN_POINT ( 'NONE',  ( -3.306064913430322161, -48.27659316133668455, -4.296538305446551576 ) ) ;
#42121 = CARTESIAN_POINT ( 'NONE',  ( 48.18093947880029759, 23.07156810961839710, -55.22362743473310331 ) ) ;
#42122 = ORIENTED_EDGE ( 'NONE', *, *, #47847, .F. ) ;
#42123 = AXIS2_PLACEMENT_3D ( 'NONE', #33412, #18476, #17956 ) ;
#42124 = CARTESIAN_POINT ( 'NONE',  ( 16.79927617522759675, -22.63757652019199895, -73.31710689363809763 ) ) ;
#42125 = AXIS2_PLACEMENT_3D ( 'NONE', #34001, #10179, #34526 ) ;
#42126 = ORIENTED_EDGE ( 'NONE', *, *, #41171, .F. ) ;
#42127 = CARTESIAN_POINT ( 'NONE',  ( 71.26464087954850868, 1.328073773609210084, -70.46779242537471077 ) ) ;
#42128 = DIRECTION ( 'NONE',  ( 0.7071067811865475727, 0.000000000000000000, 0.7071067811865475727 ) ) ;
#42129 = DIRECTION ( 'NONE',  ( 0.000000000000000000, 1.000000000000000000, 0.000000000000000000 ) ) ;
#42131 = EDGE_CURVE ( 'NONE', #9203, #29653, #21543, .T. ) ;
#42130 = CARTESIAN_POINT ( 'NONE',  ( 15.65806028500812630, 19.62302339113210436, -20.25522482650049128 ) ) ;
#42133 = FACE_OUTER_BOUND ( 'NONE', #22107, .T. ) ;
#42132 = CARTESIAN_POINT ( 'NONE',  ( 83.58813978703560110, 13.49428892428420035, -46.95981403914270658 ) ) ;
#42134 = CARTESIAN_POINT ( 'NONE',  ( 10.53030345648840083, -19.89892701156700028, -75.24509849860899635 ) ) ;
#42135 = CARTESIAN_POINT ( 'NONE',  ( 18.06932202639930196, -55.56934008872529773, -76.14999999999999147 ) ) ;
#42136 = CARTESIAN_POINT ( 'NONE',  ( 71.60339545440879760, 0.9065823421260940096, -70.54525856488069735 ) ) ;
#42137 = CARTESIAN_POINT ( 'NONE',  ( 56.05190491853310419, -45.91616149951833847, -25.80821180466989517 ) ) ;
#42138 = ORIENTED_EDGE ( 'NONE', *, *, #11590, .F. ) ;
#42139 = CARTESIAN_POINT ( 'NONE',  ( 8.645706001916300565, -48.76012022032579551, -35.08633291502829366 ) ) ;
#42140 = ORIENTED_EDGE ( 'NONE', *, *, #49523, .T. ) ;
#42141 = EDGE_CURVE ( 'NONE', #28405, #23493, #18945, .T. ) ;
#42142 = ORIENTED_EDGE ( 'NONE', *, *, #25931, .T. ) ;
#42143 = CARTESIAN_POINT ( 'NONE',  ( 12.36320305068320025, -64.54682834576858852, -15.76422791927960176 ) ) ;
#42144 = CARTESIAN_POINT ( 'NONE',  ( 10.93711667326426706, -9.623292665671325352, -38.78027754126386384 ) ) ;
#42145 = CARTESIAN_POINT ( 'NONE',  ( 68.13393739806078031, -1.166188944679350081, -89.64999999988646096 ) ) ;
#42146 = CARTESIAN_POINT ( 'NONE',  ( 11.55867067482810029, -65.29213368340509760, -47.38009360661429525 ) ) ;
#42147 = ORIENTED_EDGE ( 'NONE', *, *, #25061, .F. ) ;
#42148 = EDGE_LOOP ( 'NONE', ( #23423, #5927, #15217 ) ) ;
#42149 = CARTESIAN_POINT ( 'NONE',  ( -22.86617264519300008, -18.55609227334679900, -54.83108237264280405 ) ) ;
#42150 = FACE_OUTER_BOUND ( 'NONE', #25157, .T. ) ;
#42151 = CARTESIAN_POINT ( 'NONE',  ( 53.05395541577509988, -49.58683839042910080, -49.07041596672719663 ) ) ;
#42152 = CARTESIAN_POINT ( 'NONE',  ( 53.43548356396929933, 18.14259979176529924, -49.05614973121760158 ) ) ;
#42153 = CARTESIAN_POINT ( 'NONE',  ( 59.43939780494530112, -2.800449505682500284, -15.69362887585340083 ) ) ;
#42154 = CARTESIAN_POINT ( 'NONE',  ( 51.08267997340979605, -48.71747343918639928, -76.44192736852110670 ) ) ;
#42155 = AXIS2_PLACEMENT_3D ( 'NONE', #1102, #36733, #20481 ) ;
#42156 = CARTESIAN_POINT ( 'NONE',  ( 57.38779215104710119, -50.16954271334839888, -52.66274956582070388 ) ) ;
#42157 = EDGE_LOOP ( 'NONE', ( #21307, #50049 ) ) ;
#42158 = CARTESIAN_POINT ( 'NONE',  ( 52.72378859808809892, -49.69239786187580421, -27.46381703610880010 ) ) ;
#42159 = EDGE_LOOP ( 'NONE', ( #4517, #23112, #23283, #28074 ) ) ;
#42160 = CARTESIAN_POINT ( 'NONE',  ( 54.57779867077987745, -51.14476727363286557, -75.37910404347289273 ) ) ;
#42161 = CARTESIAN_POINT ( 'NONE',  ( 57.59002137063620097, -47.30929821719110606, -48.19818069499370239 ) ) ;
#42162 = ADVANCED_FACE ( 'NONE', ( #34631 ), #27319, .F. ) ;
#42163 = CARTESIAN_POINT ( 'NONE',  ( 11.74154980093570089, -22.11954798377650278, -44.70157888913149691 ) ) ;
#42164 = CARTESIAN_POINT ( 'NONE',  ( 13.91136646146859945, -51.07664658664480584, -22.10163017854790013 ) ) ;
#42165 = CARTESIAN_POINT ( 'NONE',  ( 55.14382500610250304, 19.42312599486780300, -76.11832371178049073 ) ) ;
#42166 = CARTESIAN_POINT ( 'NONE',  ( 47.12413796937290300, -53.90319693934949896, -75.74320899229410031 ) ) ;
#42167 = ORIENTED_EDGE ( 'NONE', *, *, #38049, .F. ) ;
#42168 = CARTESIAN_POINT ( 'NONE',  ( 55.58645560292939791, 14.21669597304580002, -15.86644146958279755 ) ) ;
#42169 = DIRECTION ( 'NONE',  ( 0.000000000000000000, 0.000000000000000000, -1.000000000000000000 ) ) ;
#42170 = AXIS2_PLACEMENT_3D ( 'NONE', #45489, #25541, #1977 ) ;
#42171 = CARTESIAN_POINT ( 'NONE',  ( 82.13853704237929776, 13.88381105532070059, -46.37203261889099792 ) ) ;
#42172 = VECTOR ( 'NONE', #28222, 1000.000000000000000 ) ;
#42173 = CARTESIAN_POINT ( 'NONE',  ( 19.78667132190540201, -9.582939898486838359, -40.52046943329969508 ) ) ;
#42174 = CARTESIAN_POINT ( 'NONE',  ( 61.28398356453099893, 14.37233669519349988, -47.68178229854910199 ) ) ;
#42175 = EDGE_LOOP ( 'NONE', ( #10660, #426, #49864, #17501 ) ) ;
#42176 = CARTESIAN_POINT ( 'NONE',  ( 46.78634582468389880, 22.26413375686030349, -76.02748008299779769 ) ) ;
#42177 = CARTESIAN_POINT ( 'NONE',  ( 65.02843368015311398, 1.270877794983130027, -60.72281693841739525 ) ) ;
#42178 = CARTESIAN_POINT ( 'NONE',  ( 75.29643519189366430, -36.41381154147628507, -12.51292969751692574 ) ) ;
#42179 = CARTESIAN_POINT ( 'NONE',  ( 105.5832649133809156, -15.41618894467769962, -103.0993275156849762 ) ) ;
#42180 = LINE ( 'NONE', #2339, #3075 ) ;
#42181 = CARTESIAN_POINT ( 'NONE',  ( 23.13393739769569990, -15.61618894467929941, -23.74958330439410048 ) ) ;
#42182 = EDGE_CURVE ( 'NONE', #727, #22408, #42259, .T. ) ;
#42183 = CARTESIAN_POINT ( 'NONE',  ( 82.75736676522110713, 14.37198029891985840, -47.68254826574469973 ) ) ;
#42184 = VECTOR ( 'NONE', #43263, 1000.000000000000000 ) ;
#42185 = CARTESIAN_POINT ( 'NONE',  ( -21.86809497655350043, -6.965125899114559260, -53.78175932259858882 ) ) ;
#42187 = CARTESIAN_POINT ( 'NONE',  ( 47.36600735767230930, -39.35907597182351481, -53.77478896724066715 ) ) ;
#42186 = CARTESIAN_POINT ( 'NONE',  ( 8.038038740883376221, 29.03132506359100518, -21.05410134318715976 ) ) ;
#42188 = CARTESIAN_POINT ( 'NONE',  ( 12.79606686025591600, -8.364588515209828046, -70.87015286643487855 ) ) ;
#42189 = DIRECTION ( 'NONE',  ( 1.000000000000000000, 0.000000000000000000, 0.000000000000000000 ) ) ;
#42190 = CARTESIAN_POINT ( 'NONE',  ( 12.82281323259459960, 33.73355787245069592, -46.32794539105000098 ) ) ;
#42191 = ORIENTED_EDGE ( 'NONE', *, *, #12089, .T. ) ;
#42192 =( BOUNDED_CURVE ( )  B_SPLINE_CURVE ( 3, ( #14066, #30293, #10657, #30027 ),
 .UNSPECIFIED., .F., .T. ) 
 B_SPLINE_CURVE_WITH_KNOTS ( ( 4, 4 ),
 ( 2.356194490192073943, 3.141592653589802886 ),
 .UNSPECIFIED. ) 
 CURVE ( )  GEOMETRIC_REPRESENTATION_ITEM ( )  RATIONAL_B_SPLINE_CURVE ( ( 1.000000000000000000, 0.9492530216741552618, 0.9492530216741552618, 1.000000000000000000 ) ) 
 REPRESENTATION_ITEM ( '' )  );
#42193 = CARTESIAN_POINT ( 'NONE',  ( 53.10972322296039749, -49.53037264418929198, -48.97251034775650425 ) ) ;
#42194 = ORIENTED_EDGE ( 'NONE', *, *, #41538, .T. ) ;
#42195 = CARTESIAN_POINT ( 'NONE',  ( 47.21631652332737872, 8.040122714078041355, -54.78327235947799068 ) ) ;
#42196 = DIRECTION ( 'NONE',  ( 0.000000000000000000, 0.000000000000000000, -1.000000000000000000 ) ) ;
#42197 = CARTESIAN_POINT ( 'NONE',  ( 13.89444719274460027, 19.98929110357370220, -22.84407598213759982 ) ) ;
#42198 = CARTESIAN_POINT ( 'NONE',  ( 56.78931313380690682, 14.03059450484890114, -25.50518706664649926 ) ) ;
#42199 = CARTESIAN_POINT ( 'NONE',  ( 18.32725043397720199, -8.913060076642750573, -50.05347842037799211 ) ) ;
#42200 = DIRECTION ( 'NONE',  ( 0.000000000000000000, 0.000000000000000000, -1.000000000000000000 ) ) ;
#42201 = CARTESIAN_POINT ( 'NONE',  ( 53.02924604216119775, 18.36504672385269998, -49.05876171777440220 ) ) ;
#42202 = CARTESIAN_POINT ( 'NONE',  ( 64.97085660027880749, 1.369719003397489976, -60.94773069968270107 ) ) ;
#42203 = FACE_OUTER_BOUND ( 'NONE', #21871, .T. ) ;
#42204 = ORIENTED_EDGE ( 'NONE', *, *, #15659, .F. ) ;
#42205 = CARTESIAN_POINT ( 'NONE',  ( 16.02219763869389979, -23.46311588517269797, -37.79203799605679848 ) ) ;
#42206 = EDGE_CURVE ( 'NONE', #29477, #2118, #9775, .T. ) ;
#42207 = CARTESIAN_POINT ( 'NONE',  ( 72.87455824417588701, 1.326134026835569912, -68.94513744192749982 ) ) ;
#42208 = CARTESIAN_POINT ( 'NONE',  ( 24.00580240620973882, -14.79998447179700705, -49.75944949806702766 ) ) ;
#42209 = CARTESIAN_POINT ( 'NONE',  ( 72.89060928222170332, 1.370937308141420230, -62.62705977251020784 ) ) ;
#42210 = CARTESIAN_POINT ( 'NONE',  ( 10.73482432373229756, -64.94719017208709033, -18.15071128010919921 ) ) ;
#42211 = CARTESIAN_POINT ( 'NONE',  ( 52.93498290923280081, 18.37341140428640074, -48.74287987618630069 ) ) ;
#42212 = FACE_OUTER_BOUND ( 'NONE', #4875, .T. ) ;
#42213 = CARTESIAN_POINT ( 'NONE',  ( 22.88621463017819124, -15.16096302198837087, -62.43140197241153544 ) ) ;
#42214 = DIRECTION ( 'NONE',  ( 0.000000000000000000, -1.000000000000000000, 0.000000000000000000 ) ) ;
#42215 = CARTESIAN_POINT ( 'NONE',  ( 64.88003574513449223, 1.187237555532410171, -70.57991217294409125 ) ) ;
#42216 = ORIENTED_EDGE ( 'NONE', *, *, #30093, .F. ) ;
#42217 = CARTESIAN_POINT ( 'NONE',  ( 10.49070342362870001, -63.25259970453439706, -45.62560734925740036 ) ) ;
#42218 = CARTESIAN_POINT ( 'NONE',  ( 20.99563923973620305, -9.290042711380010587, -47.50066625719156121 ) ) ;
#42219 = ORIENTED_EDGE ( 'NONE', *, *, #24545, .F. ) ;
#42220 = DIRECTION ( 'NONE',  ( 1.224650706428208818E-16, 1.000000000000000000, 8.281540456132313294E-12 ) ) ;
#42221 = CARTESIAN_POINT ( 'NONE',  ( 16.65420337941489848, 17.88381105532299742, -17.90311212357439885 ) ) ;
#42222 = CARTESIAN_POINT ( 'NONE',  ( 53.23471704948639882, 19.19657966078460376, -77.19501645526850098 ) ) ;
#42223 = ORIENTED_EDGE ( 'NONE', *, *, #44104, .T. ) ;
#42224 = CARTESIAN_POINT ( 'NONE',  ( -13.36606260230359844, -50.61618894467959962, 11.34999999999999964 ) ) ;
#42225 = DIRECTION ( 'NONE',  ( 0.000000000000000000, 0.000000000000000000, 1.000000000000000000 ) ) ;
#42226 = CARTESIAN_POINT ( 'NONE',  ( 22.81271906878893674, -14.50446391198467211, -72.40033769317329870 ) ) ;
#42227 = EDGE_CURVE ( 'NONE', #26440, #22140, #5568, .T. ) ;
#42228 = CARTESIAN_POINT ( 'NONE',  ( 13.76993472929000006, -23.51518960550360049, -62.38489440685859222 ) ) ;
#42229 = EDGE_CURVE ( 'NONE', #33944, #14108, #36506, .T. ) ;
#42230 = TOROIDAL_SURFACE ( 'NONE', #32123, 16.49999999930319916, 0.5000000000336690675 ) ;
#42231 = CARTESIAN_POINT ( 'NONE',  ( 44.86124405867887077, -38.02577711452058651, -66.01342731499525485 ) ) ;
#42232 = EDGE_CURVE ( 'NONE', #45766, #1196, #10611, .T. ) ;
#42233 = ORIENTED_EDGE ( 'NONE', *, *, #9218, .T. ) ;
#42234 = B_SPLINE_CURVE_WITH_KNOTS ( 'NONE', 3,
 ( #3363, #34266, #38756, #26406, #26151, #30601, #19337, #15154, #22478, #42161, #2322, #47140, #38486, #31115, #42942, #18815 ),
 .UNSPECIFIED., .F., .F.,
 ( 4, 2, 2, 2, 2, 2, 2, 4 ),
 ( 0.000000000000000000, 1.372899869568840137, 2.941928291933239681, 3.922571055910980320, 4.412892437899861520, 5.197406649082060071, 6.452629386973570469, 7.845142111821970410 ),
 .UNSPECIFIED. ) ;
#42235 = CARTESIAN_POINT ( 'NONE',  ( 56.71514755247739714, -46.07503343450810007, -26.25075064288229854 ) ) ;
#42236 = CARTESIAN_POINT ( 'NONE',  ( 16.60938827565720288, -8.181093769243290126, -41.75298454923780156 ) ) ;
#42237 = CARTESIAN_POINT ( 'NONE',  ( 8.841948616896502244, -16.75224457701870406, -32.14999999999999858 ) ) ;
#42238 = DIRECTION ( 'NONE',  ( 1.000000000000000000, 0.000000000000000000, 0.000000000000000000 ) ) ;
#42239 = CIRCLE ( 'NONE', #20476, 2.999999999999998668 ) ;
#42240 = CARTESIAN_POINT ( 'NONE',  ( 13.62850291019639926, 20.22628383398669882, -74.56034069004439857 ) ) ;
#42241 = CARTESIAN_POINT ( 'NONE',  ( 18.20469862234147129, -7.911111929476298599, -51.37566333439941246 ) ) ;
#42242 = EDGE_CURVE ( 'NONE', #43941, #27825, #3047, .T. ) ;
#42243 = CARTESIAN_POINT ( 'NONE',  ( 43.82158222066500031, -45.08534330693629499, -6.692173543831889226 ) ) ;
#42244 = FACE_OUTER_BOUND ( 'NONE', #46832, .T. ) ;
#42245 = CARTESIAN_POINT ( 'NONE',  ( 11.15293902025540085, -22.18675786014680185, -66.21414035735639914 ) ) ;
#42246 = EDGE_CURVE ( 'NONE', #34780, #18612, #15404, .T. ) ;
#42247 = ORIENTED_EDGE ( 'NONE', *, *, #40826, .F. ) ;
#42248 = CARTESIAN_POINT ( 'NONE',  ( 53.98906395436699768, -48.34780241224260067, -26.51423003085930219 ) ) ;
#42249 = CARTESIAN_POINT ( 'NONE',  ( 56.57234934511910041, -50.73310576891860535, -74.30382550411290765 ) ) ;
#42251 = CARTESIAN_POINT ( 'NONE',  ( 42.22066838722344073, -39.78807865986343018, -75.26602574004256496 ) ) ;
#42250 = CARTESIAN_POINT ( 'NONE',  ( 2.830591470287960210, 25.45182595484199695, -11.52757872387000049 ) ) ;
#42252 = CARTESIAN_POINT ( 'NONE',  ( 63.43393739769620510, 1.383811055320669947, -68.50657137141709541 ) ) ;
#42253 = FACE_OUTER_BOUND ( 'NONE', #24974, .T. ) ;
#42254 = ORIENTED_EDGE ( 'NONE', *, *, #47218, .T. ) ;
#42255 = CARTESIAN_POINT ( 'NONE',  ( 20.82450310336395205, -9.200888125289733210, -81.20852785396732543 ) ) ;
#42256 = CARTESIAN_POINT ( 'NONE',  ( 47.49898707597870384, 23.35465752766770109, -54.71508157337640199 ) ) ;
#42257 = CARTESIAN_POINT ( 'NONE',  ( 43.87440825508269882, -45.06628648458400477, -6.621182746357190396 ) ) ;
#42258 = CARTESIAN_POINT ( 'NONE',  ( 63.33388541776029257, 1.264121749638649872, -62.30317625966389983 ) ) ;
#42259 = LINE ( 'NONE', #26509, #9748 ) ;
#42260 = CARTESIAN_POINT ( 'NONE',  ( 11.65450058717340021, 33.89481885373739800, -16.76600934541039933 ) ) ;
#42261 = CARTESIAN_POINT ( 'NONE',  ( 62.63393739769619373, -53.11618894467930119, 11.84999999999999964 ) ) ;
#42262 = CARTESIAN_POINT ( 'NONE',  ( 53.26902542446040201, 18.19839717132569845, -48.80947755968719548 ) ) ;
#42263 = CARTESIAN_POINT ( 'NONE',  ( 19.04984016102106281, 24.27634599866043175, -75.91709172409272810 ) ) ;
#42264 = CARTESIAN_POINT ( 'NONE',  ( 53.97934697425230155, -49.20473928360389948, -49.10921081283519385 ) ) ;
#42265 = CARTESIAN_POINT ( 'NONE',  ( 56.42508253464700374, 14.99986749066500025, -26.25079172228680235 ) ) ;
#42266 = CIRCLE ( 'NONE', #7110, 1.000000000000000444 ) ;
#42267 = CARTESIAN_POINT ( 'NONE',  ( 50.04538724767210311, 22.25689945218810095, -54.67691783917840098 ) ) ;
#42268 = CARTESIAN_POINT ( 'NONE',  ( 53.63393739769619373, 21.88381105532059934, 16.35000000000000142 ) ) ;
#42269 = CARTESIAN_POINT ( 'NONE',  ( 53.23851273770399928, 18.29663818490410421, -49.17579072038760302 ) ) ;
#42270 = DIRECTION ( 'NONE',  ( 0.000000000000000000, -1.000000000000000000, 0.000000000000000000 ) ) ;
#42271 = CARTESIAN_POINT ( 'NONE',  ( 20.02514464312236342, 23.87147242321097096, -18.88231557620769863 ) ) ;
#42272 = CARTESIAN_POINT ( 'NONE',  ( 11.10551642654870008, 32.05074912355050287, -44.25176302638880088 ) ) ;
#42273 = DIRECTION ( 'NONE',  ( 0.7071067811865487940, 0.000000000000000000, 0.7071067811865462405 ) ) ;
#42274 = B_SPLINE_CURVE_WITH_KNOTS ( 'NONE', 3,
 ( #28822, #4995, #1318, #33270, #45345, #41401, #5519, #21474, #1572, #49545, #9950, #10481, #10735, #6540, #21986, #26435, #2615, #26689 ),
 .UNSPECIFIED., .F., .F.,
 ( 4, 2, 2, 2, 2, 2, 2, 2, 4 ),
 ( 0.000000000000000000, 0.06250019453820399029, 0.1250003890764079806, 0.1875005836146119709, 0.2500007781528159612, 0.3125009726910198404, 0.3750011672292237197, 0.4375013617674275990, 0.5000015563056314782 ),
 .UNSPECIFIED. ) ;
#42275 = CARTESIAN_POINT ( 'NONE',  ( 65.46218529380999485, -32.54800987811099588, -18.25464570420819754 ) ) ;
#42276 = EDGE_LOOP ( 'NONE', ( #36698, #49370, #5305, #39499, #9659 ) ) ;
#42277 = CARTESIAN_POINT ( 'NONE',  ( 18.84529956396119843, 20.48963776793139857, -74.14994161014911356 ) ) ;
#42278 = ORIENTED_EDGE ( 'NONE', *, *, #22969, .T. ) ;
#42279 = EDGE_LOOP ( 'NONE', ( #21501, #44710, #9862, #44504 ) ) ;
#42280 = CARTESIAN_POINT ( 'NONE',  ( 42.29536634374500181, 11.94537196368429832, -3.241362035758810212 ) ) ;
#42281 = AXIS2_PLACEMENT_3D ( 'NONE', #8011, #15109, #39216 ) ;
#42282 = CARTESIAN_POINT ( 'NONE',  ( 49.58508211105249330, -2.000197079579435044, -15.77316264483759767 ) ) ;
#42283 = VERTEX_POINT ( 'NONE', #2685 ) ;
#42284 = CARTESIAN_POINT ( 'NONE',  ( 12.28449157720250007, -65.33530493076349899, -46.44573566506809925 ) ) ;
#42285 = CARTESIAN_POINT ( 'NONE',  ( 57.61832698878280468, -45.11897047559610030, -25.41289556137760286 ) ) ;
#42286 = CARTESIAN_POINT ( 'NONE',  ( 15.24811531979822377, -22.38318606151044676, -44.99450808075278729 ) ) ;
#42287 = FACE_OUTER_BOUND ( 'NONE', #34228, .T. ) ;
#42288 = CARTESIAN_POINT ( 'NONE',  ( 13.39998208310050032, -51.78678246903520233, -74.14999999999999147 ) ) ;
#42289 = EDGE_LOOP ( 'NONE', ( #16413, #47593, #21697 ) ) ;
#42290 = FACE_OUTER_BOUND ( 'NONE', #50206, .T. ) ;
#42291 = CARTESIAN_POINT ( 'NONE',  ( 46.40541215375579043, 6.961926829937682193, -58.29262626224165444 ) ) ;
#42292 = DIRECTION ( 'NONE',  ( 0.3863301728269249447, 0.9223605572461988089, -3.330669073875469621E-16 ) ) ;
#42293 = VERTEX_POINT ( 'NONE', #14732 ) ;
#42294 = CARTESIAN_POINT ( 'NONE',  ( 46.78799807556309531, -45.19957043902829952, -8.930844661211528646 ) ) ;
#42295 = ADVANCED_FACE ( 'NONE', ( #9522 ), #26553, .T. ) ;
#42296 = CARTESIAN_POINT ( 'NONE',  ( 52.01928562022798985, 1.750919267526578560, -19.49271441683317718 ) ) ;
#42297 = CARTESIAN_POINT ( 'NONE',  ( 14.28039018034760055, 19.72599742411139800, -21.66377081666459858 ) ) ;
#42298 = DIRECTION ( 'NONE',  ( -1.000000000000000000, 0.000000000000000000, 0.000000000000000000 ) ) ;
#42299 = EDGE_CURVE ( 'NONE', #16350, #9032, #47427, .T. ) ;
#42300 = CARTESIAN_POINT ( 'NONE',  ( 16.19411604853889486, -22.38296026765021907, -46.94999358384413313 ) ) ;
#42301 = LINE ( 'NONE', #22359, #27497 ) ;
#42302 = CARTESIAN_POINT ( 'NONE',  ( 47.16564018750800358, -54.32016963230069706, -75.35585495399020317 ) ) ;
#42303 = CARTESIAN_POINT ( 'NONE',  ( 64.36501694216710234, 13.88381105527329851, -12.32038502994480034 ) ) ;
#42304 = CIRCLE ( 'NONE', #13819, 3.000000000000004885 ) ;
#42305 = CARTESIAN_POINT ( 'NONE',  ( 14.13393739769640156, 10.38381105532060111, -35.14999999999999858 ) ) ;
#42306 = CARTESIAN_POINT ( 'NONE',  ( 52.19959685038109853, 19.92045540604299703, -76.05470843165690553 ) ) ;
#42307 = CARTESIAN_POINT ( 'NONE',  ( 61.43371642943920108, 13.93409536008670102, -28.09734365521990185 ) ) ;
#42308 = CARTESIAN_POINT ( 'NONE',  ( 11.18413446363969932, -9.526349358606669426, -80.57026077041129497 ) ) ;
#42309 = EDGE_CURVE ( 'NONE', #35448, #11637, #35414, .T. ) ;
#42310 = B_SPLINE_SURFACE_WITH_KNOTS ( 'NONE', 3, 3, ( 
 ( #42252, #6351, #34362, #22568, #15752, #19426, #28295, #31707, #12334, #39862 ),
 ( #39605, #16009, #8659, #44300, #3709, #19926, #32216, #3453, #31456, #43792 ),
 ( #11836, #7893, #20181, #20435, #15503, #23839, #279, #35406, #16263, #47481 ),
 ( #3964, #27536, #19677, #36171, #35919, #48240, #47731, #8407, #43542, #8149 ),
 ( #24354, #35674, #51404, #40368, #4465, #27796, #47988, #31966, #32464, #36422 ),
 ( #529, #39354, #16515, #34, #40115, #12087, #23587, #28041, #51659, #44046 ),
 ( #11574, #24093, #48494, #4209, #12597, #28558, #44560, #7642, #34223, #44822 ),
 ( #9884, #26106, #10149, #14075, #42115, #18522, #22432, #784, #28820, #37925 ),
 ( #48760, #30036, #49729, #18001, #2023, #24614, #4993, #20690, #40625, #36680 ),
 ( #6217, #22173, #46059, #38184, #34495, #38441, #16783, #8929, #33965, #20956 ),
 ( #2278, #13817, #49982, #18254, #4725, #36952, #32730, #12865, #24874, #6475 ),
 ( #2541, #1764, #50242, #25840, #10411, #14332, #17745, #33715, #30301, #5958 ),
 ( #46318, #26360, #42378, #29777, #40883, #50499, #45796, #41853, #21917, #14589 ),
 ( #30559, #46579, #3834, #26625, #22696, #35796, #50757, #27664, #35541, #38969 ),
 ( #51531, #3060, #15629, #11187, #11448, #10927, #39220, #31837, #31580, #26895 ),
 ( #3580, #42641, #2804, #15111, #51013, #35008, #31070, #43408, #43666, #38712 ) ),
 .UNSPECIFIED., .F., .F., .F.,
 ( 4, 2, 2, 2, 2, 2, 2, 4 ),
 ( 4, 1, 1, 1, 1, 1, 1, 4 ),
 ( -8.880243999999999390E-15, 0.07216186899280199740, 0.1546325764131560032, 0.2061767685508779924, 0.2319488646197390147, 0.2731842183299159621, 0.3391607842661999994, 0.4123535371017649775 ),
 ( 0.000000000000000000, 0.1428571428571430157, 0.2857142857142860315, 0.4285714285714289917, 0.5714285714285709528, 0.7142857142857139685, 0.8571428571428569843, 1.000000000000000000 ),
 .UNSPECIFIED. ) ;
#42311 = ORIENTED_EDGE ( 'NONE', *, *, #16748, .F. ) ;
#42312 = CIRCLE ( 'NONE', #37293, 5.500000000000000000 ) ;
#42313 = CARTESIAN_POINT ( 'NONE',  ( 9.740363391916037727, -12.79400397788338140, -47.97990518416660422 ) ) ;
#42314 = CARTESIAN_POINT ( 'NONE',  ( -5.143620389462549625, -47.12425989114009894, -5.067427102881679524 ) ) ;
#42315 = CARTESIAN_POINT ( 'NONE',  ( 75.68173550483029999, -18.74328204524080022, -11.58966857824820096 ) ) ;
#42316 = EDGE_CURVE ( 'NONE', #26368, #25343, #46043, .T. ) ;
#42317 = CARTESIAN_POINT ( 'NONE',  ( 62.63393739769619373, 21.88381105532059934, 11.84999999999999964 ) ) ;
#42318 = CARTESIAN_POINT ( 'NONE',  ( 74.93037156228848517, -45.11618894467250129, -15.31097063366330069 ) ) ;
#42319 = CARTESIAN_POINT ( 'NONE',  ( 13.13393739769600010, 18.38381105532060289, -83.01107220193038927 ) ) ;
#42320 = CARTESIAN_POINT ( 'NONE',  ( 71.33393739769628894, 1.530257664727401767, -69.99644660940670349 ) ) ;
#42321 = CARTESIAN_POINT ( 'NONE',  ( 82.32429201311688871, -45.44102527263400049, -47.46868292619190299 ) ) ;
#42322 = CARTESIAN_POINT ( 'NONE',  ( 41.44023872227730010, 12.74910146949009970, -3.815737712921210001 ) ) ;
#42323 = CARTESIAN_POINT ( 'NONE',  ( 22.72480952368614382, -17.38744173618666267, -78.53615067353597112 ) ) ;
#42324 = CARTESIAN_POINT ( 'NONE',  ( 0.3209249304026170480, -8.218592747557250888, -34.64999999999999858 ) ) ;
#42325 = CARTESIAN_POINT ( 'NONE',  ( 70.83745409581578656, -49.21324915460098026, -73.25000000000119371 ) ) ;
#42326 = CARTESIAN_POINT ( 'NONE',  ( 22.87920569102662682, -16.16927548186827579, -62.47886883811316494 ) ) ;
#42327 = DIRECTION ( 'NONE',  ( -0.2389682100434953882, -0.9710273912658735629, 0.000000000000000000 ) ) ;
#42328 = VERTEX_POINT ( 'NONE', #27804 ) ;
#42329 = CARTESIAN_POINT ( 'NONE',  ( 8.922492023814040607, -13.74489261382869998, -52.14815840911180089 ) ) ;
#42330 = B_SPLINE_CURVE_WITH_KNOTS ( 'NONE', 3,
 ( #34239, #5716, #5977, #25858, #42137, #38202, #22451, #21933 ),
 .UNSPECIFIED., .F., .F.,
 ( 4, 1, 1, 1, 1, 4 ),
 ( 0.000000000000000000, 0.2000000000001341816, 0.4000000000001006084, 0.6000000000000670353, 0.8000000000000334621, 1.000000000000000000 ),
 .UNSPECIFIED. ) ;
#42331 = CARTESIAN_POINT ( 'NONE',  ( 63.94317349953750096, 1.409272994606969975, -61.59476957024820365 ) ) ;
#42332 = ORIENTED_EDGE ( 'NONE', *, *, #23575, .F. ) ;
#42333 = CARTESIAN_POINT ( 'NONE',  ( 9.543078926210201374, -17.38749007367445998, -69.36948668258585826 ) ) ;
#42334 = DIRECTION ( 'NONE',  ( 1.000000000000000000, 0.000000000000000000, 0.000000000000000000 ) ) ;
#42335 = FACE_OUTER_BOUND ( 'NONE', #24461, .T. ) ;
#42336 = CARTESIAN_POINT ( 'NONE',  ( 21.26062805952274459, -21.67729426163444018, -61.78425362803765353 ) ) ;
#42337 = CARTESIAN_POINT ( 'NONE',  ( 45.76530515845411884, 8.847626787123020975, -58.09878025211985886 ) ) ;
#42338 = VECTOR ( 'NONE', #47410, 1000.000000000000000 ) ;
#42339 = LINE ( 'NONE', #38926, #29284 ) ;
#42340 = CARTESIAN_POINT ( 'NONE',  ( 10.13393739769630031, -54.15188668067469990, -35.09469305598949518 ) ) ;
#42341 = ORIENTED_EDGE ( 'NONE', *, *, #17349, .F. ) ;
#42342 = EDGE_LOOP ( 'NONE', ( #32611, #12371, #46677, #34867 ) ) ;
#42343 = EDGE_LOOP ( 'NONE', ( #15725, #15843, #30490, #14750, #31227 ) ) ;
#42344 = CARTESIAN_POINT ( 'NONE',  ( 61.25719188131670023, -45.31066424344650301, -47.12453700741409790 ) ) ;
#42345 = CARTESIAN_POINT ( 'NONE',  ( -20.77565199683915154, -28.32022799467020491, -53.08356737070175058 ) ) ;
#42346 = ORIENTED_EDGE ( 'NONE', *, *, #15743, .F. ) ;
#42347 = ORIENTED_EDGE ( 'NONE', *, *, #31196, .T. ) ;
#42348 = CARTESIAN_POINT ( 'NONE',  ( 22.89855956817655880, -15.80994150920190755, -72.46193828865773412 ) ) ;
#42349 = ADVANCED_FACE ( 'NONE', ( #3717 ), #10677, .T. ) ;
#42350 = AXIS2_PLACEMENT_3D ( 'NONE', #51778, #12207, #15881 ) ;
#42351 = DIRECTION ( 'NONE',  ( 1.000000000000000000, 0.000000000000000000, 0.000000000000000000 ) ) ;
#42352 = VERTEX_POINT ( 'NONE', #45874 ) ;
#42353 = DIRECTION ( 'NONE',  ( 0.000000000000000000, 0.000000000000000000, 1.000000000000000000 ) ) ;
#42354 = CARTESIAN_POINT ( 'NONE',  ( 51.73525746098499667, -50.43300767444429766, -76.36782564804489937 ) ) ;
#42355 = CARTESIAN_POINT ( 'NONE',  ( 60.63565020168820041, 14.37421254607160037, -47.39321454885000406 ) ) ;
#42356 = CIRCLE ( 'NONE', #39846, 3.000000000000003109 ) ;
#42357 = CARTESIAN_POINT ( 'NONE',  ( 21.17583492150360058, -21.63000777762489690, -78.29040566010620239 ) ) ;
#42358 = DIRECTION ( 'NONE',  ( -0.2389682100434953882, -0.9710273912658735629, 0.000000000000000000 ) ) ;
#42359 = CARTESIAN_POINT ( 'NONE',  ( 45.11068418675889546, 14.77969269803630148, -8.978235662926250527 ) ) ;
#42360 = CARTESIAN_POINT ( 'NONE',  ( 42.98728576779360111, -42.87622043099199942, -4.202726304278470160 ) ) ;
#42361 = DIRECTION ( 'NONE',  ( 1.000000000000000000, 0.000000000000000000, 0.000000000000000000 ) ) ;
#42362 = CARTESIAN_POINT ( 'NONE',  ( 56.61928438282120624, 14.09173444410579989, -25.29356196242219923 ) ) ;
#42363 = CARTESIAN_POINT ( 'NONE',  ( 64.66082326855108420, 1.024253516290760002, -70.53167046690938946 ) ) ;
#42364 = CIRCLE ( 'NONE', #34796, 1.000000000000000888 ) ;
#42365 = CARTESIAN_POINT ( 'NONE',  ( 27.22499013618942598, -28.04647486959190417, -34.79644660940672907 ) ) ;
#42366 = B_SPLINE_CURVE_WITH_KNOTS ( 'NONE', 3,
 ( #15679, #26947, #7051, #39783, #35593, #19085, #11239, #43461, #51836, #19855, #34807, #10983, #19346, #39022, #30865, #35845, #35061, #12012, #15935 ),
 .UNSPECIFIED., .F., .F.,
 ( 4, 3, 3, 3, 3, 3, 4 ),
 ( 0.000000000000000000, 0.04742532092110129938, 0.07033534312137200428, 0.1033624735406969974, 0.1094063869444049930, 0.1257965922736820064, 0.1407742777448500182 ),
 .UNSPECIFIED. ) ;
#42367 = DIRECTION ( 'NONE',  ( 1.000000000000000000, 0.000000000000000000, 0.000000000000000000 ) ) ;
#42368 = CARTESIAN_POINT ( 'NONE',  ( 11.43684957307149830, -21.90300961580910055, -49.99175337985419532 ) ) ;
#42369 = EDGE_CURVE ( 'NONE', #42020, #1082, #25406, .T. ) ;
#42370 = ORIENTED_EDGE ( 'NONE', *, *, #16385, .T. ) ;
#42371 = VECTOR ( 'NONE', #33234, 1000.000000000000000 ) ;
#42372 = PRESENTATION_STYLE_ASSIGNMENT (( #26355 ) ) ;
#42373 = CARTESIAN_POINT ( 'NONE',  ( 44.88839470740660431, 14.87643554339019936, -8.898984674148820773 ) ) ;
#42374 = ADVANCED_FACE ( 'NONE', ( #9959 ), #2221, .F. ) ;
#42375 = CARTESIAN_POINT ( 'NONE',  ( 46.13154385501714216, -40.10099849830307761, -56.32029921020890839 ) ) ;
#42376 = CARTESIAN_POINT ( 'NONE',  ( -30.36606260230379917, 8.133811055320650851, 16.35000000000000142 ) ) ;
#42377 = CARTESIAN_POINT ( 'NONE',  ( 46.85564613059059980, -54.06445821833459320, -75.74423906255060501 ) ) ;
#42378 = CARTESIAN_POINT ( 'NONE',  ( 63.43898171031389666, 1.369976237678190101, -68.83116145970220146 ) ) ;
#42379 = B_SPLINE_CURVE_WITH_KNOTS ( 'NONE', 3,
 ( #10630, #42075, #27114, #38144, #18218, #30775, #26329, #34184, #26069, #26852, #42863, #43118, #10889, #21880, #33929, #2499, #22655, #49945, #50712, #14036, #50201, #26584, #14294, #29996, #46282, #6957, #10368, #18479, #50460, #46799, #14550, #30519, #42602, #6697, #2761, #19251, #47818, #47564, #51491, #39441, #43630, #12421, #24183, #7209, #15837, #27624, #11662, #19769, #28386, #3541, #39180, #27876, #23163, #51240, #39950, #16347, #43879, #7733, #7976, #32304, #31800, #48326, #35233, #11925, #40204, #23676, #23927, #39693, #51741, #4045, #3798, #27367, #3277, #36255, #4292, #20264, #35758, #15331, #20009, #8231, #15592, #31284, #47317, #11407, #366, #36001, #118, #43374, #7468, #23420, #16091, #32050, #19511, #35501, #48072, #31546, #12170, #28129, #44134, #45435, #5346, #16601, #32557, #48848, #37554, #616, #33618, #8493, #28644, #1401, #41233, #1661 ),
 .UNSPECIFIED., .F., .F.,
 ( 4, 3, 3, 3, 3, 3, 3, 3, 3, 3, 3, 3, 3, 3, 3, 3, 3, 3, 3, 3, 3, 3, 3, 3, 3, 3, 3, 3, 3, 3, 3, 3, 3, 3, 3, 3, 3, 4 ),
 ( -1.533736992487469974, -1.476288708613060052, -1.420671483735689966, -1.384064782255480131, -1.360357242476590178, -1.351866781456839917, -1.295064174654980027, -1.237933406125270031, -1.182875639009639990, -1.170176701831340038, -1.162728788953599990, -1.127817871894019941, -1.070863248456429995, -1.013122296642539943, -0.9549592239029349727, -0.9075319219357990130, -0.8918603538934489761, -0.8833676238340290032, -0.8240633799986251118, -0.7652500160343930213, -0.7062545498940289157, -0.6468558762931539974, -0.6146511409503889745, -0.6051424443490369676, -0.5954651498571321699, -0.5353212793362460697, -0.4746770670517450608, -0.4139651071065320043, -0.3892179935510320377, -0.3405657443571530330, -0.3192803853348309406, -0.3088845131001689559, -0.2992958165493331268, -0.2386552343498948847, -0.1768311013664789488, -0.1147878690630650400, -0.05320817752461537431, 0.000000000000000000 ),
 .UNSPECIFIED. ) ;
#42380 = CARTESIAN_POINT ( 'NONE',  ( 47.75291977277729671, -54.48739848013099873, -55.20309039576459753 ) ) ;
#42381 = CARTESIAN_POINT ( 'NONE',  ( 13.00893739761190027, -65.51843714052189682, -47.75434321210310173 ) ) ;
#42382 = CARTESIAN_POINT ( 'NONE',  ( 10.94780721248439548, -10.83637588594239531, -36.08420929373698982 ) ) ;
#42383 = CARTESIAN_POINT ( 'NONE',  ( 47.81306074494699487, 23.22517729902449801, -55.08809726227399750 ) ) ;
#42384 = EDGE_LOOP ( 'NONE', ( #50781, #22862 ) ) ;
#42385 = CARTESIAN_POINT ( 'NONE',  ( 10.11051084926620014, -19.28509774568809831, -69.67303606471168109 ) ) ;
#42386 = ORIENTED_EDGE ( 'NONE', *, *, #38939, .T. ) ;
#42387 = CARTESIAN_POINT ( 'NONE',  ( 71.47398825900590680, 0.9272522097098119254, -70.63440435907199344 ) ) ;
#42388 = AXIS2_PLACEMENT_3D ( 'NONE', #2827, #34771, #46344 ) ;
#42389 = DIRECTION ( 'NONE',  ( 0.000000000000000000, 1.000000000000000000, 0.000000000000000000 ) ) ;
#42390 = DIRECTION ( 'NONE',  ( 0.000000000000000000, 0.000000000000000000, -1.000000000000000000 ) ) ;
#42391 = CARTESIAN_POINT ( 'NONE',  ( 16.13393739769620083, -15.61618894467929941, -15.18999999999999950 ) ) ;
#42393 = CARTESIAN_POINT ( 'NONE',  ( 55.92359121559390189, 14.66224575315600021, -25.40852202100330004 ) ) ;
#42392 = CARTESIAN_POINT ( 'NONE',  ( 82.89855244518290078, 14.28649170576880145, -47.58879117305969686 ) ) ;
#42394 = CARTESIAN_POINT ( 'NONE',  ( 23.06349459023610038, -14.30325489761369973, -72.39321698031869801 ) ) ;
#42395 = CARTESIAN_POINT ( 'NONE',  ( 8.222937397696199469, -15.61618894467929941, -32.14999999999999858 ) ) ;
#42396 = CARTESIAN_POINT ( 'NONE',  ( 8.223439258000311725, -15.61632852289070073, -42.50766849176289952 ) ) ;
#42397 = DIRECTION ( 'NONE',  ( 1.000000000000000000, 5.495516945195724241E-29, 2.619602780254359830E-11 ) ) ;
#42398 = ORIENTED_EDGE ( 'NONE', *, *, #49044, .T. ) ;
#42399 = CARTESIAN_POINT ( 'NONE',  ( 27.73905384484250192, -53.11618894467930119, -74.14999999999999147 ) ) ;
#42400 = B_SPLINE_CURVE_WITH_KNOTS ( 'NONE', 3,
 ( #21681, #30325, #1788, #46349, #6243, #5725, #37952, #34247, #14097, #22201 ),
 .UNSPECIFIED., .F., .F.,
 ( 4, 2, 2, 2, 4 ),
 ( 0.000000000000000000, 0.1338527402502077968, 0.2763488516921074889, 0.4029155702267074868, 0.4999999999999911737 ),
 .UNSPECIFIED. ) ;
#42401 = AXIS2_PLACEMENT_3D ( 'NONE', #46407, #22520, #2885 ) ;
#42402 = B_SPLINE_CURVE_WITH_KNOTS ( 'NONE', 3,
 ( #1172, #1691, #24471, #13245, #41519, #17168, #32851, #33120, #5636, #32588, #5373 ),
 .UNSPECIFIED., .F., .F.,
 ( 4, 1, 1, 1, 1, 1, 1, 1, 4 ),
 ( 0.4999978458836923934, 0.5065141047152040832, 0.5857330357787533526, 0.6649519668423027330, 0.7441708979060125406, 0.8233898289695594785, 0.9026087600332693972, 0.9818276910968208870, 1.000000000000000000 ),
 .UNSPECIFIED. ) ;
#42403 = ORIENTED_EDGE ( 'NONE', *, *, #24263, .F. ) ;
#42404 = CARTESIAN_POINT ( 'NONE',  ( 24.04523214473702097, -15.61618869705131729, -47.50766735973101618 ) ) ;
#42405 = CARTESIAN_POINT ( 'NONE',  ( 24.03855097274092500, -15.27262742755435632, -39.49384892683895032 ) ) ;
#42406 = CARTESIAN_POINT ( 'NONE',  ( 11.69945459769019891, 33.68403274003249948, -45.13438395913740209 ) ) ;
#42407 = CARTESIAN_POINT ( 'NONE',  ( 16.13393739769620083, -15.61618894467929941, -6.649999999999999467 ) ) ;
#42408 = AXIS2_PLACEMENT_3D ( 'NONE', #14470, #33855, #22576 ) ;
#42409 = EDGE_LOOP ( 'NONE', ( #40222, #7727, #23167, #17669 ) ) ;
#42410 = ORIENTED_EDGE ( 'NONE', *, *, #1668, .T. ) ;
#42411 = CARTESIAN_POINT ( 'NONE',  ( 51.29354596943910138, 21.74684883274469982, -54.72842898864520578 ) ) ;
#42412 = CIRCLE ( 'NONE', #31495, 0.5000000000000004441 ) ;
#42413 = CARTESIAN_POINT ( 'NONE',  ( 57.07057989771080031, 14.65163658184950002, -26.24936944650179882 ) ) ;
#42414 = CARTESIAN_POINT ( 'NONE',  ( 53.34803077867909593, -49.46767309333149854, -49.15544592153489845 ) ) ;
#42415 = ADVANCED_FACE ( 'NONE', ( #42980 ), #35351, .T. ) ;
#42416 = CARTESIAN_POINT ( 'NONE',  ( 48.43106010952779883, 22.58642710690570254, -53.38354561996749936 ) ) ;
#42417 = CARTESIAN_POINT ( 'NONE',  ( 59.95038794592539944, -2.512083940479500122, -15.76663620625850015 ) ) ;
#42418 = CARTESIAN_POINT ( 'NONE',  ( 51.37232876478519472, -49.64415483134600038, -76.46732863254598556 ) ) ;
#42419 = EDGE_CURVE ( 'NONE', #20901, #26902, #24737, .T. ) ;
#42420 = CARTESIAN_POINT ( 'NONE',  ( 56.58402204250390355, -50.55592571534859303, -53.00599847022490252 ) ) ;
#42421 = ORIENTED_EDGE ( 'NONE', *, *, #3918, .F. ) ;
#42422 = EDGE_CURVE ( 'NONE', #11667, #37038, #1436, .T. ) ;
#42423 = CARTESIAN_POINT ( 'NONE',  ( 10.33399650447251261, -10.17551119628275025, -33.03228949958723604 ) ) ;
#42424 = CARTESIAN_POINT ( 'NONE',  ( 67.04038824939809160, 19.47158195952359705, -70.40645085170191919 ) ) ;
#42425 = ORIENTED_EDGE ( 'NONE', *, *, #17043, .T. ) ;
#42426 = CARTESIAN_POINT ( 'NONE',  ( 9.366715917462860475, -15.61603296970410071, -51.45282021618999835 ) ) ;
#42427 = CARTESIAN_POINT ( 'NONE',  ( 54.13393739769620083, -15.61618894467929941, -3.187564294433600232 ) ) ;
#42428 = CARTESIAN_POINT ( 'NONE',  ( 22.27743955675109788, -20.49923397962109917, -44.22626530275000079 ) ) ;
#42429 = CARTESIAN_POINT ( 'NONE',  ( 13.86432996969659825, -51.09005464285149856, -22.12930180663200019 ) ) ;
#42430 = AXIS2_PLACEMENT_3D ( 'NONE', #45585, #9679, #29827 ) ;
#42431 = CARTESIAN_POINT ( 'NONE',  ( 56.42418868998549897, 19.40436683310219834, -75.33371615204529803 ) ) ;
#42432 = CARTESIAN_POINT ( 'NONE',  ( 47.58822567098650325, -54.46711296191460150, -74.72768729699521373 ) ) ;
#42433 = CARTESIAN_POINT ( 'NONE',  ( 55.45985160373810174, 14.08381916207730100, -15.39201607824520046 ) ) ;
#42434 = CARTESIAN_POINT ( 'NONE',  ( 47.73557342949970206, 23.25259336863290116, -54.98607376159549887 ) ) ;
#42435 = CARTESIAN_POINT ( 'NONE',  ( 82.45630311851421368, 13.86034003618500066, -46.38988467804559690 ) ) ;
#42436 = AXIS2_PLACEMENT_3D ( 'NONE', #2865, #18830, #7829 ) ;
#42437 = CARTESIAN_POINT ( 'NONE',  ( 23.10375731890249895, -14.53722210533389969, -44.79829171073519944 ) ) ;
#42438 = DIRECTION ( 'NONE',  ( 1.000000000000000000, 0.000000000000000000, 0.000000000000000000 ) ) ;
#42439 = ORIENTED_EDGE ( 'NONE', *, *, #43709, .T. ) ;
#42440 = CARTESIAN_POINT ( 'NONE',  ( 46.37900464578690674, 21.71116150353940100, -76.14999999999999147 ) ) ;
#42441 = CARTESIAN_POINT ( 'NONE',  ( 64.97448143965360146, 1.327097482837290121, -60.84525133028229504 ) ) ;
#42442 = EDGE_CURVE ( 'NONE', #41357, #39182, #26607, .T. ) ;
#42443 = CARTESIAN_POINT ( 'NONE',  ( 9.366937397696199596, -15.61618894467949836, -28.45282021618999835 ) ) ;
#42444 = CARTESIAN_POINT ( 'NONE',  ( 11.89611903400246540, -65.09453069998440355, -23.79086514498333216 ) ) ;
#42445 = CARTESIAN_POINT ( 'NONE',  ( 29.09106731080629871, -4.508242673544909707, -34.94555596725388824 ) ) ;
#42446 = VECTOR ( 'NONE', #48194, 1000.000000000000000 ) ;
#42447 = DIRECTION ( 'NONE',  ( 1.260570937617230037E-11, 1.376914871200490071E-11, 1.000000000000000000 ) ) ;
#42448 = CARTESIAN_POINT ( 'NONE',  ( 82.30072452188801435, 14.05343120103280086, -47.18357693586790447 ) ) ;
#42449 = CARTESIAN_POINT ( 'NONE',  ( 0.3976851907049809842, 20.06812262159460047, -34.91005868551109614 ) ) ;
#42451 = CARTESIAN_POINT ( 'NONE',  ( 45.32011839866689229, -39.20707424017311382, -63.91252006199604097 ) ) ;
#42450 = CARTESIAN_POINT ( 'NONE',  ( 22.90118952179220813, -15.61618876469732875, -46.84717865327674247 ) ) ;
#42452 = CARTESIAN_POINT ( 'NONE',  ( 23.96699468023455282, -14.48491286449858428, -71.46203103834751857 ) ) ;
#42453 = CARTESIAN_POINT ( 'NONE',  ( 6.156981251806739053, 33.30392151337740358, -47.78905844756960164 ) ) ;
#42454 = ORIENTED_EDGE ( 'NONE', *, *, #30602, .F. ) ;
#42455 = CARTESIAN_POINT ( 'NONE',  ( 52.77791368993419496, -49.69695095401060314, -48.73087024381919719 ) ) ;
#42456 = ORIENTED_EDGE ( 'NONE', *, *, #4717, .F. ) ;
#42457 = B_SPLINE_CURVE_WITH_KNOTS ( 'NONE', 3,
 ( #35040, #51049, #15146, #11220, #27183, #43190, #40023, #36081, #49195, #12242, #41056, #48935, #438, #4113, #13036, #16427, #28989, #24517 ),
 .UNSPECIFIED., .F., .F.,
 ( 4, 2, 2, 2, 2, 2, 2, 2, 4 ),
 ( 0.000000000000000000, 0.06249982867297892986, 0.1249996573459578597, 0.1874994860189367896, 0.2499993146919157194, 0.3124991433648947603, 0.3749989720378738012, 0.4374988007108528421, 0.4999986293838318829 ),
 .UNSPECIFIED. ) ;
#42458 = CARTESIAN_POINT ( 'NONE',  ( 46.39461793029816761, 9.013153168876611332, -54.52405409598588193 ) ) ;
#42459 = CARTESIAN_POINT ( 'NONE',  ( 20.99565881307366766, -21.94231955833456382, -74.08399818326770969 ) ) ;
#42460 = CARTESIAN_POINT ( 'NONE',  ( 14.12421044447399865, 19.90653214807120008, -22.60548794454369670 ) ) ;
#42461 = CARTESIAN_POINT ( 'NONE',  ( 57.53087442631830584, 14.06726690696280002, -25.93050682469580082 ) ) ;
#42462 = CARTESIAN_POINT ( 'NONE',  ( 9.151501097378190508, -14.62213562185059956, -41.49783386550709707 ) ) ;
#42463 = CARTESIAN_POINT ( 'NONE',  ( 51.00677359191169558, 19.62691423242569755, -76.14999999999999147 ) ) ;
#42464 = CARTESIAN_POINT ( 'NONE',  ( 52.86566475114400276, 18.43067181376370200, -48.91558075316019938 ) ) ;
#42465 = CARTESIAN_POINT ( 'NONE',  ( 55.25725834564570249, -45.84610244531269529, -16.15205766596429982 ) ) ;
#42466 = DIRECTION ( 'NONE',  ( 0.000000000000000000, 0.000000000000000000, -1.000000000000000000 ) ) ;
#42467 = ORIENTED_EDGE ( 'NONE', *, *, #44916, .F. ) ;
#42468 = CARTESIAN_POINT ( 'NONE',  ( 21.53393071017169902, -10.48321867350180092, -80.82541145414198525 ) ) ;
#42469 = CARTESIAN_POINT ( 'NONE',  ( 11.49541394825729768, -65.34930665952259687, -17.78290644886060079 ) ) ;
#42470 = CARTESIAN_POINT ( 'NONE',  ( 10.66940904945339952, 33.58243990817589264, -46.87940410059270135 ) ) ;
#42471 = CARTESIAN_POINT ( 'NONE',  ( 72.89924231985609993, 1.371651820402789879, -62.65029732562830844 ) ) ;
#42472 = CARTESIAN_POINT ( 'NONE',  ( 11.73545769477099832, -65.42259919599071338, -18.15007894733780347 ) ) ;
#42473 = CARTESIAN_POINT ( 'NONE',  ( 16.65420337943509566, -51.11618894467930119, -15.67544740040250062 ) ) ;
#42474 = CARTESIAN_POINT ( 'NONE',  ( 46.98749078828947034, -15.61618894467929941, -34.79644660940672907 ) ) ;
#42475 = CARTESIAN_POINT ( 'NONE',  ( 8.428852126995982630, -13.54545571365708767, -44.87565280027760650 ) ) ;
#42476 = CARTESIAN_POINT ( 'NONE',  ( 15.31576361048525747, -23.52281516480273282, -46.04045315081875600 ) ) ;
#42477 = VERTEX_POINT ( 'NONE', #14925 ) ;
#42478 = CARTESIAN_POINT ( 'NONE',  ( 65.05077035654551310, 1.384378348444520013, -70.31241234944640439 ) ) ;
#42479 = EDGE_LOOP ( 'NONE', ( #39895, #38286, #5088, #34230 ) ) ;
#42480 = CARTESIAN_POINT ( 'NONE',  ( 10.77457706359389888, -63.40313208684650448, -45.20848294960729419 ) ) ;
#42481 = ADVANCED_FACE ( 'NONE', ( #50576 ), #47680, .T. ) ;
#42482 = DIRECTION ( 'NONE',  ( -0.3502816565540492477, 0.000000000000000000, 0.9366444154970182678 ) ) ;
#42483 = ORIENTED_EDGE ( 'NONE', *, *, #48750, .F. ) ;
#42484 = CARTESIAN_POINT ( 'NONE',  ( -11.32734370190460105, 10.64934056395049922, 8.349999999999999645 ) ) ;
#42485 = CARTESIAN_POINT ( 'NONE',  ( 68.13393739769620083, -33.11618894467940066, -65.65000000000000568 ) ) ;
#42486 = EDGE_CURVE ( 'NONE', #3287, #26440, #38246, .T. ) ;
#42487 = CARTESIAN_POINT ( 'NONE',  ( 52.24694086453770581, 18.59896962735679793, -77.11046207536941210 ) ) ;
#42488 = VERTEX_POINT ( 'NONE', #26971 ) ;
#42489 = EDGE_CURVE ( 'NONE', #5288, #49378, #6457, .T. ) ;
#42490 = PLANE ( 'NONE',  #45056 ) ;
#42491 = CARTESIAN_POINT ( 'NONE',  ( 44.08684091409431005, 1.883811055320659511, -54.64999999999999858 ) ) ;
#42492 = CARTESIAN_POINT ( 'NONE',  ( 9.366908763506170743, -15.61636271700460021, -33.45282021618999835 ) ) ;
#42493 = TOROIDAL_SURFACE ( 'NONE', #8174, 38.50000000000000000, 0.5000000000000000000 ) ;
#42494 = CARTESIAN_POINT ( 'NONE',  ( 8.428822445502495597, -13.54556363260618923, -68.87566510286049493 ) ) ;
#42495 = EDGE_CURVE ( 'NONE', #677, #34827, #2870, .T. ) ;
#42496 = CARTESIAN_POINT ( 'NONE',  ( 16.29407891153249821, -23.85979705954510166, -64.28614875238559989 ) ) ;
#42497 = CARTESIAN_POINT ( 'NONE',  ( 24.04493742051697680, -16.65172778451557534, -47.54933648736709983 ) ) ;
#42498 = CARTESIAN_POINT ( 'NONE',  ( 44.17290358208205703, -37.93974571477343716, -69.45512797184353815 ) ) ;
#42499 = ORIENTED_EDGE ( 'NONE', *, *, #21241, .T. ) ;
#42500 = CARTESIAN_POINT ( 'NONE',  ( 65.46029542295769943, -1.463538230407920082, -16.55376543218019947 ) ) ;
#42501 = CARTESIAN_POINT ( 'NONE',  ( 12.32795013852219945, -22.02096488050650080, -54.90332710579869513 ) ) ;
#42502 = CARTESIAN_POINT ( 'NONE',  ( 9.303925792589840427, -18.78836378116810124, -32.14999999999999858 ) ) ;
#42503 = CARTESIAN_POINT ( 'NONE',  ( 9.386603864545342901, -14.93147129003910933, -61.48498468630781844 ) ) ;
#42504 = CARTESIAN_POINT ( 'NONE',  ( 14.46049191127040068, 20.21128881784729714, -75.25165125838280744 ) ) ;
#42505 = B_SPLINE_CURVE_WITH_KNOTS ( 'NONE', 3,
 ( #50929, #3233, #39909, #15288, #7686, #32007, #12129, #16051, #35452, #48031 ),
 .UNSPECIFIED., .F., .F.,
 ( 4, 2, 2, 2, 4 ),
 ( 0.000000000000000000, 0.1249361396779638672, 0.3249507363229993118, 0.6449740909550615298, 1.000000000000000000 ),
 .UNSPECIFIED. ) ;
#42506 = ADVANCED_FACE ( 'NONE', ( #3402 ), #3871, .T. ) ;
#42507 = CARTESIAN_POINT ( 'NONE',  ( 17.60468922291027027, -52.01452886433823153, -75.82251645567225751 ) ) ;
#42508 =( BOUNDED_CURVE ( )  B_SPLINE_CURVE ( 3, ( #2270, #34736, #33957, #10138 ),
 .UNSPECIFIED., .F., .T. ) 
 B_SPLINE_CURVE_WITH_KNOTS ( ( 4, 4 ),
 ( 5.485850788443479509, 6.283185307179586232 ),
 .UNSPECIFIED. ) 
 CURVE ( )  GEOMETRIC_REPRESENTATION_ITEM ( )  RATIONAL_B_SPLINE_CURVE ( ( 1.000000000000000000, 0.9477194463358846743, 0.9477194463358846743, 1.000000000000000000 ) ) 
 REPRESENTATION_ITEM ( '' )  );
#42509 = CARTESIAN_POINT ( 'NONE',  ( 40.88927314113769285, -45.09957127860379700, -5.596099653381020111 ) ) ;
#42510 = CARTESIAN_POINT ( 'NONE',  ( 16.13393739769620083, -15.61618894467929941, -20.58999999999999986 ) ) ;
#42511 = CARTESIAN_POINT ( 'NONE',  ( 12.16686956752729998, -8.388112192194309813, -66.84789180586530222 ) ) ;
#42512 = ORIENTED_EDGE ( 'NONE', *, *, #34752, .T. ) ;
#42513 = CARTESIAN_POINT ( 'NONE',  ( 19.90939373821190017, -22.53927847089380165, -32.14999999999999858 ) ) ;
#42514 = CARTESIAN_POINT ( 'NONE',  ( 56.68161731648030610, -50.69729438425329704, -74.14921287266520267 ) ) ;
#42516 = CARTESIAN_POINT ( 'NONE',  ( 41.23058856492793467, -39.67759845120787787, -80.04365382965534081 ) ) ;
#42515 = CARTESIAN_POINT ( 'NONE',  ( 12.13746661513899916, 33.80420561274659974, -16.30595336032680009 ) ) ;
#42517 = DIRECTION ( 'NONE',  ( 0.000000000000000000, 0.000000000000000000, 1.000000000000000000 ) ) ;
#42518 = DIRECTION ( 'NONE',  ( 1.000000000000000000, 0.000000000000000000, 0.000000000000000000 ) ) ;
#42519 = VERTEX_POINT ( 'NONE', #35555 ) ;
#42520 = CARTESIAN_POINT ( 'NONE',  ( 18.08327279923313569, -7.911801705270725016, -81.08663926983665249 ) ) ;
#42521 = CARTESIAN_POINT ( 'NONE',  ( 47.49808756796829812, 23.36748740488750187, -54.86913899898670621 ) ) ;
#42522 = EDGE_CURVE ( 'NONE', #37113, #27066, #39088, .T. ) ;
#42523 = CARTESIAN_POINT ( 'NONE',  ( 43.46647314489950276, -45.04259908834720250, -6.433232421327499395 ) ) ;
#42524 = CARTESIAN_POINT ( 'NONE',  ( 2.404741263826640107, -5.380232784273969671, -35.14999999999999858 ) ) ;
#42525 = CARTESIAN_POINT ( 'NONE',  ( 57.46491512144735481, 13.88414644239919404, -25.32915905940588885 ) ) ;
#42526 = CARTESIAN_POINT ( 'NONE',  ( 11.77474680307169841, 33.82436456779279865, -16.56178175560690136 ) ) ;
#42527 = CARTESIAN_POINT ( 'NONE',  ( 51.84245824985789852, 18.13569299140640112, -76.99756684514699145 ) ) ;
#42528 = CARTESIAN_POINT ( 'NONE',  ( 52.91916940086609600, 18.38207858727010091, -48.76921091615339776 ) ) ;
#42529 = DIRECTION ( 'NONE',  ( 0.000000000000000000, 1.000000000000000000, 0.000000000000000000 ) ) ;
#42530 = CARTESIAN_POINT ( 'NONE',  ( 57.55751162049570269, -50.61618894467930119, -53.92796738110899923 ) ) ;
#42531 = CARTESIAN_POINT ( 'NONE',  ( 53.18313144231220235, 18.10656684143660300, -27.45873945498200186 ) ) ;
#42532 = AXIS2_PLACEMENT_3D ( 'NONE', #45155, #9269, #41221 ) ;
#42533 = CARTESIAN_POINT ( 'NONE',  ( 17.63393739769620083, -32.58675169315650066, -35.14999999999999858 ) ) ;
#42534 = CARTESIAN_POINT ( 'NONE',  ( 24.04496217889941789, -15.61618911842929869, -37.79232902657031445 ) ) ;
#42535 = FACE_OUTER_BOUND ( 'NONE', #40009, .T. ) ;
#42536 = CARTESIAN_POINT ( 'NONE',  ( 14.06322549156652535, -23.32128047233873858, -76.09102434139356319 ) ) ;
#42537 = CARTESIAN_POINT ( 'NONE',  ( 71.36689417337970553, 0.9219904752505979628, -60.59541050710320320 ) ) ;
#42538 = CARTESIAN_POINT ( 'NONE',  ( 10.97915888064600054, 32.07709238800340046, -44.74319236371729858 ) ) ;
#42539 = CYLINDRICAL_SURFACE ( 'NONE', #10042, 0.4999999999999991118 ) ;
#42540 = DIRECTION ( 'NONE',  ( 1.000000000000000000, 0.000000000000000000, 0.000000000000000000 ) ) ;
#42541 = CARTESIAN_POINT ( 'NONE',  ( 12.73487912048826232, 24.23912916116268690, -75.56421958049274679 ) ) ;
#42542 = ORIENTED_EDGE ( 'NONE', *, *, #31306, .F. ) ;
#42543 = ORIENTED_EDGE ( 'NONE', *, *, #10791, .F. ) ;
#42544 = CARTESIAN_POINT ( 'NONE',  ( 41.06001733956060207, 13.06695014755839956, -3.719605790254209676 ) ) ;
#42545 = CARTESIAN_POINT ( 'NONE',  ( 76.55758335127733005, 0.1435741152385172914, -13.47555346654003827 ) ) ;
#42546 = ORIENTED_EDGE ( 'NONE', *, *, #51758, .T. ) ;
#42547 = CARTESIAN_POINT ( 'NONE',  ( 11.70108564249209948, -64.94919988858430315, -45.68669056181820309 ) ) ;
#42548 = CARTESIAN_POINT ( 'NONE',  ( 56.70280968235780250, -45.37092424972929905, -25.70441953237769894 ) ) ;
#42549 = CARTESIAN_POINT ( 'NONE',  ( 21.54527739906354711, -19.77483417149147016, -44.66116455897760318 ) ) ;
#42550 = ADVANCED_FACE ( 'NONE', ( #35021 ), #42914, .T. ) ;
#42551 = CARTESIAN_POINT ( 'NONE',  ( 56.52536539877749533, 19.51942783438209972, -53.84278118897309895 ) ) ;
#42552 = VERTEX_POINT ( 'NONE', #15126 ) ;
#42553 = LINE ( 'NONE', #38622, #34340 ) ;
#42554 = CARTESIAN_POINT ( 'NONE',  ( 45.09935103916460264, 6.822007087868398933, -64.82292987203024381 ) ) ;
#42555 = CARTESIAN_POINT ( 'NONE',  ( 10.73251648177490125, 33.05260077103709904, -23.50916409409499863 ) ) ;
#42556 = EDGE_CURVE ( 'NONE', #18612, #1476, #3011, .T. ) ;
#42557 = ORIENTED_EDGE ( 'NONE', *, *, #7102, .F. ) ;
#42558 = CARTESIAN_POINT ( 'NONE',  ( 51.63377760632049984, -45.11618894467940066, -11.44539556602689956 ) ) ;
#42559 = B_SPLINE_CURVE_WITH_KNOTS ( 'NONE', 3,
 ( #12108, #28065, #44069, #8172, #17332, #20982, #29365, #41172, #24116, #9212 ),
 .UNSPECIFIED., .F., .F.,
 ( 4, 2, 2, 2, 4 ),
 ( -0.1857717838172110170, -0.1853436703576350209, -0.1652145016252450083, -0.1459149143060420040, -0.1350635247397186933 ),
 .UNSPECIFIED. ) ;
#42560 = FACE_OUTER_BOUND ( 'NONE', #21373, .T. ) ;
#42561 = CARTESIAN_POINT ( 'NONE',  ( 16.33938386690500266, 19.86387930602199958, -20.40297663956880214 ) ) ;
#42562 = CARTESIAN_POINT ( 'NONE',  ( 9.456108772904830317, -16.86908816385087206, -51.39384808471273658 ) ) ;
#42563 = CARTESIAN_POINT ( 'NONE',  ( 21.10768686100733049, -20.20497612657083408, -46.69000373621759081 ) ) ;
#42564 = CARTESIAN_POINT ( 'NONE',  ( 68.13393739769618662, -0.5161889446793590519, -80.15000000000000568 ) ) ;
#42565 = CARTESIAN_POINT ( 'NONE',  ( 47.37011039443260074, -54.67477790795700088, -74.19794602913619030 ) ) ;
#42566 = CARTESIAN_POINT ( 'NONE',  ( 61.85779513593570300, 12.50882928757600077, -9.638490008265870657 ) ) ;
#42567 = CIRCLE ( 'NONE', #36656, 20.79999999999999716 ) ;
#42568 = CARTESIAN_POINT ( 'NONE',  ( 56.27102044028909944, 19.34483705538490028, -52.87264067008490542 ) ) ;
#42569 = CARTESIAN_POINT ( 'NONE',  ( 52.03834263415010497, 20.05835102498519973, -76.00976797213479585 ) ) ;
#42570 = CARTESIAN_POINT ( 'NONE',  ( 11.93174526809839975, 34.20691394249479345, -17.93019253464870033 ) ) ;
#42571 = CARTESIAN_POINT ( 'NONE',  ( 21.96499996289010070, -20.86864479655330129, -81.52088794317478460 ) ) ;
#42572 = ORIENTED_EDGE ( 'NONE', *, *, #26025, .T. ) ;
#42573 = LINE ( 'NONE', #17933, #397 ) ;
#42574 = CARTESIAN_POINT ( 'NONE',  ( 9.023247183187249831, -62.42415218838889501, -14.37474631752760068 ) ) ;
#42575 = CARTESIAN_POINT ( 'NONE',  ( 76.39865836638340113, -5.985310478428520042, -12.78927121757400087 ) ) ;
#42576 = CYLINDRICAL_SURFACE ( 'NONE', #38887, 0.5000000000000154321 ) ;
#42577 = CARTESIAN_POINT ( 'NONE',  ( 61.14784649246698933, -45.50800750378603254, -47.53180933876430458 ) ) ;
#42578 = CARTESIAN_POINT ( 'NONE',  ( 13.21803463400281231, -55.50872388801388979, -75.91709172390962124 ) ) ;
#42579 = CARTESIAN_POINT ( 'NONE',  ( 46.98749078828947034, -15.61618894467929941, -34.79644660940672907 ) ) ;
#42580 = ADVANCED_FACE ( 'NONE', ( #31084 ), #14831, .F. ) ;
#42581 = CARTESIAN_POINT ( 'NONE',  ( 82.48418901823390570, -45.09830753207049270, -46.54733415317949863 ) ) ;
#42582 = CARTESIAN_POINT ( 'NONE',  ( 52.82975622904280755, -49.66092049964720445, -48.47378032971909789 ) ) ;
#42583 = CARTESIAN_POINT ( 'NONE',  ( 42.73119093514949896, 11.67612964396700015, -3.876063987046979964 ) ) ;
#42584 = CARTESIAN_POINT ( 'NONE',  ( 68.13393739769618662, -0.5161889446793590519, -65.65000000000000568 ) ) ;
#42585 = CARTESIAN_POINT ( 'NONE',  ( 10.06369629473941352, -53.99262654158863484, -34.79644414665150975 ) ) ;
#42586 = CARTESIAN_POINT ( 'NONE',  ( 68.13393739769790614, -49.95860450174320277, -71.35146707679190570 ) ) ;
#42587 = ADVANCED_FACE ( 'NONE', ( #10423 ), #22446, .T. ) ;
#42588 = CARTESIAN_POINT ( 'NONE',  ( 22.90078882061835586, -15.66462506390463361, -62.45510662821025250 ) ) ;
#42589 = CARTESIAN_POINT ( 'NONE',  ( 18.67895139973730068, -51.93864758878049059, -75.09854824053090283 ) ) ;
#42590 = CARTESIAN_POINT ( 'NONE',  ( 58.57901109696710051, -44.96736093356130226, -9.776967083451840068 ) ) ;
#42591 = EDGE_CURVE ( 'NONE', #42921, #26465, #13176, .T. ) ;
#42592 = ORIENTED_EDGE ( 'NONE', *, *, #1285, .T. ) ;
#42593 = CARTESIAN_POINT ( 'NONE',  ( 15.06541911040859993, -22.98944894335520317, -49.61315261507599672 ) ) ;
#42594 = CARTESIAN_POINT ( 'NONE',  ( 63.90248588247730765, 1.347758125946160179, -61.55177802591560265 ) ) ;
#42595 = ORIENTED_EDGE ( 'NONE', *, *, #43755, .F. ) ;
#42596 = CARTESIAN_POINT ( 'NONE',  ( 9.367478339302499180, -15.61624867646989756, -69.45282021618999124 ) ) ;
#42597 = CARTESIAN_POINT ( 'NONE',  ( 74.93037295002240228, 11.88381105532070059, -15.31098073120859837 ) ) ;
#42598 = DIRECTION ( 'NONE',  ( 0.000000000000000000, 0.000000000000000000, 1.000000000000000000 ) ) ;
#42599 = VECTOR ( 'NONE', #10907, 1000.000000000000000 ) ;
#42600 = CARTESIAN_POINT ( 'NONE',  ( 45.40454100101857904, 8.825245881843775564, -59.84982165534362508 ) ) ;
#42601 = VECTOR ( 'NONE', #45309, 1000.000000000000000 ) ;
#42602 = CARTESIAN_POINT ( 'NONE',  ( 9.093616821199461242, -16.36736670071820043, -81.23899999999999011 ) ) ;
#42603 = CARTESIAN_POINT ( 'NONE',  ( 42.04042276467250616, -45.73515590541849463, -6.805329779705280302 ) ) ;
#42604 = VERTEX_POINT ( 'NONE', #2820 ) ;
#42605 = ORIENTED_EDGE ( 'NONE', *, *, #20877, .F. ) ;
#42606 = VERTEX_POINT ( 'NONE', #38724 ) ;
#42607 = CARTESIAN_POINT ( 'NONE',  ( 16.13393739769620083, -15.61618894467929941, -5.966499999999999915 ) ) ;
#42608 = CARTESIAN_POINT ( 'NONE',  ( 61.45294174207020177, -45.16075577691309917, -46.37196027249549957 ) ) ;
#42609 = DIRECTION ( 'NONE',  ( 3.757729999999999984E-12, -1.000000000000000000, 1.557061999999999974E-12 ) ) ;
#42610 = DIRECTION ( 'NONE',  ( 0.7675009104025395379, 0.5576220516902739011, 0.3162277660168420490 ) ) ;
#42611 = ORIENTED_EDGE ( 'NONE', *, *, #23895, .F. ) ;
#42612 = ADVANCED_FACE ( 'NONE', ( #30826 ), #45774, .F. ) ;
#42613 = CARTESIAN_POINT ( 'NONE',  ( 9.367479537931210132, -15.61613030728229923, -79.45282021618999124 ) ) ;
#42614 = ORIENTED_EDGE ( 'NONE', *, *, #34935, .T. ) ;
#42615 = CARTESIAN_POINT ( 'NONE',  ( 8.223551834036749497, -15.61610457483330094, -62.79233150823698395 ) ) ;
#42616 = CARTESIAN_POINT ( 'NONE',  ( 11.89321892217540011, -65.43602743108330344, -18.17421237901570308 ) ) ;
#42617 = ORIENTED_EDGE ( 'NONE', *, *, #43077, .F. ) ;
#42618 = CARTESIAN_POINT ( 'NONE',  ( 53.62552786343490396, -51.33071804962359153, -75.58099297212140755 ) ) ;
#42619 = CARTESIAN_POINT ( 'NONE',  ( 52.09209166129659963, -51.30114848017019824, -75.99731152592609362 ) ) ;
#42620 = CARTESIAN_POINT ( 'NONE',  ( 60.78179592255849428, 14.26585277497870052, -47.15482822166340071 ) ) ;
#42621 = LINE ( 'NONE', #46562, #17975 ) ;
#42622 = CARTESIAN_POINT ( 'NONE',  ( 41.26036424091849852, -44.20758967157720321, -4.192607877207990441 ) ) ;
#42623 = CARTESIAN_POINT ( 'NONE',  ( 0.5406133260286669628, -43.55985091651039909, -20.15000000000000213 ) ) ;
#42624 = DIRECTION ( 'NONE',  ( 0.2771081164311154366, 0.6505467637364714673, -0.7071067811865496822 ) ) ;
#42625 = TOROIDAL_SURFACE ( 'NONE', #20002, 1.499999999983230081, 0.4999999999993299804 ) ;
#42626 = AXIS2_PLACEMENT_3D ( 'NONE', #5118, #33384, #9040 ) ;
#42627 = CARTESIAN_POINT ( 'NONE',  ( 64.61284426162950467, 0.9526384849486110307, -70.50836581366849032 ) ) ;
#42628 = CARTESIAN_POINT ( 'NONE',  ( -13.73674066540299954, -0.6797460008306699386, -46.71145918530370267 ) ) ;
#42629 = CIRCLE ( 'NONE', #50184, 2.999999999999999112 ) ;
#42630 = LINE ( 'NONE', #34214, #47671 ) ;
#42631 = CARTESIAN_POINT ( 'NONE',  ( 12.69125976124770006, -22.66847360106410036, -47.93206117220019991 ) ) ;
#42632 = ORIENTED_EDGE ( 'NONE', *, *, #37018, .F. ) ;
#42633 = CARTESIAN_POINT ( 'NONE',  ( 14.21949999245200047, -52.31213937195320085, -75.84958893011570069 ) ) ;
#42635 = AXIS2_PLACEMENT_3D ( 'NONE', #27294, #22835, #38856 ) ;
#42634 = CARTESIAN_POINT ( 'NONE',  ( 57.55751162087899786, 19.38381105532060289, -53.87300832421969687 ) ) ;
#42636 = UNCERTAINTY_MEASURE_WITH_UNIT (LENGTH_MEASURE( 1.000000000000000082E-05 ), #11360, 'distance_accuracy_value', 'NONE');
#42637 = CARTESIAN_POINT ( 'NONE',  ( 71.62064552848029564, 0.9479899806831150189, -70.53291850127411067 ) ) ;
#42638 = CARTESIAN_POINT ( 'NONE',  ( 45.77958804137001891, -40.08084910885633434, -58.02946520578011302 ) ) ;
#42639 = CARTESIAN_POINT ( 'NONE',  ( 24.04501723819814529, -15.61618889329698412, -35.50767088183642528 ) ) ;
#42640 = CARTESIAN_POINT ( 'NONE',  ( 47.18305862770080239, -54.80685414274160649, -74.19838441418400521 ) ) ;
#42641 = CARTESIAN_POINT ( 'NONE',  ( 63.52141932237860544, 1.390806392144110060, -68.86952544730040415 ) ) ;
#42642 = CARTESIAN_POINT ( 'NONE',  ( 47.79229160385850150, -54.46650021306819411, -55.08202210981530556 ) ) ;
#42643 = CARTESIAN_POINT ( 'NONE',  ( 24.04018637339055786, -15.32013480239626801, -45.49576358883199134 ) ) ;
#42644 = EDGE_CURVE ( 'NONE', #12279, #45483, #30976, .T. ) ;
#42645 = CARTESIAN_POINT ( 'NONE',  ( 13.85919928309939309, -8.940252629490174741, -36.24264715586421914 ) ) ;
#42646 = CARTESIAN_POINT ( 'NONE',  ( 47.82372406217509564, 23.16461151845500410, -54.73644791471539861 ) ) ;
#42647 = ORIENTED_EDGE ( 'NONE', *, *, #21655, .F. ) ;
#42648 = CARTESIAN_POINT ( 'NONE',  ( 9.225955441871899865, -14.19409736079129836, -77.91180489532798958 ) ) ;
#42649 = VERTEX_POINT ( 'NONE', #34969 ) ;
#42650 = CARTESIAN_POINT ( 'NONE',  ( 71.23851365796429036, 1.390208944942409985, -70.27002685503239832 ) ) ;
#42651 = DIRECTION ( 'NONE',  ( 1.000000000000000000, 2.460964292799963328E-14, 0.000000000000000000 ) ) ;
#42652 = DIRECTION ( 'NONE',  ( 1.130501000000000083E-17, -8.343543999999999066E-19, -1.000000000000000000 ) ) ;
#42654 = CARTESIAN_POINT ( 'NONE',  ( 14.58123197128210080, 0.9736865341423419640, -34.65032322548069743 ) ) ;
#42653 = CARTESIAN_POINT ( 'NONE',  ( 16.13393739769620083, -15.61618894467929941, -20.58999999999999986 ) ) ;
#42655 = CARTESIAN_POINT ( 'NONE',  ( 19.97295785153600178, -9.699730489520039356, -74.13603346371829161 ) ) ;
#42656 = CARTESIAN_POINT ( 'NONE',  ( -13.73674066540309902, -30.55263188852779876, -46.71145918530379504 ) ) ;
#42657 = DIRECTION ( 'NONE',  ( -1.000000000000000000, 0.000000000000000000, 0.000000000000000000 ) ) ;
#42658 = CARTESIAN_POINT ( 'NONE',  ( 16.13393739769620083, -15.61618894467929941, -22.14999999999999858 ) ) ;
#42659 = ORIENTED_EDGE ( 'NONE', *, *, #21004, .F. ) ;
#42660 = DIRECTION ( 'NONE',  ( 0.000000000000000000, -1.000000000000000000, 0.000000000000000000 ) ) ;
#42661 = ORIENTED_EDGE ( 'NONE', *, *, #11436, .T. ) ;
#42662 = ORIENTED_EDGE ( 'NONE', *, *, #4402, .T. ) ;
#42663 = CARTESIAN_POINT ( 'NONE',  ( 12.28895731154639925, -64.62670895685438666, -15.84602084846439851 ) ) ;
#42664 = AXIS2_PLACEMENT_3D ( 'NONE', #3903, #19869, #47926 ) ;
#42665 = DIRECTION ( 'NONE',  ( -1.080939296543039954E-11, -1.000000000000000000, 2.435884827299240233E-11 ) ) ;
#42666 = AXIS2_PLACEMENT_3D ( 'NONE', #36208, #32254, #20998 ) ;
#42667 = CARTESIAN_POINT ( 'NONE',  ( 76.46740023287678412, -26.22475495909479903, -13.08694098715510812 ) ) ;
#42668 = CARTESIAN_POINT ( 'NONE',  ( 13.00893739769619906, -65.51843714052719747, -47.75434321273180416 ) ) ;
#42669 = AXIS2_PLACEMENT_3D ( 'NONE', #47219, #34878, #27524 ) ;
#42670 = VERTEX_POINT ( 'NONE', #6696 ) ;
#42671 = AXIS2_PLACEMENT_3D ( 'NONE', #17642, #33608, #45679 ) ;
#42672 = EDGE_LOOP ( 'NONE', ( #34823, #22462, #23031, #28189 ) ) ;
#42673 = EDGE_CURVE ( 'NONE', #37146, #16669, #37861, .T. ) ;
#42674 = DIRECTION ( 'NONE',  ( -1.000000000000000000, 0.000000000000000000, 0.000000000000000000 ) ) ;
#42675 = CARTESIAN_POINT ( 'NONE',  ( 56.59172680816769940, 14.94416698784849906, -26.26184181833360043 ) ) ;
#42676 = CARTESIAN_POINT ( 'NONE',  ( 49.71164272696770325, 21.47435747220460200, -52.28127911264229510 ) ) ;
#42677 = EDGE_CURVE ( 'NONE', #11471, #22490, #695, .T. ) ;
#42678 = CARTESIAN_POINT ( 'NONE',  ( 59.10140662637690667, -2.844898398060870193, -15.65498877140790057 ) ) ;
#42679 = CARTESIAN_POINT ( 'NONE',  ( 51.36577782788289426, -50.50831518850419855, -76.23494669504191279 ) ) ;
#42680 = CARTESIAN_POINT ( 'NONE',  ( 57.70617712934760135, -49.34354290365170215, -51.67788969020119794 ) ) ;
#42681 = ORIENTED_EDGE ( 'NONE', *, *, #40915, .F. ) ;
#42682 = DIRECTION ( 'NONE',  ( 0.000000000000000000, 0.000000000000000000, 1.000000000000000000 ) ) ;
#42683 = CARTESIAN_POINT ( 'NONE',  ( 23.83903863463931927, -17.68685968673479536, -47.87566667355078920 ) ) ;
#42684 = EDGE_LOOP ( 'NONE', ( #7605, #9638, #33873, #48077, #9019 ) ) ;
#42685 = PLANE ( 'NONE',  #41084 ) ;
#42686 = CARTESIAN_POINT ( 'NONE',  ( 46.03121886948380137, -45.11618894467940066, -7.582877905987319700 ) ) ;
#42687 = CARTESIAN_POINT ( 'NONE',  ( 9.965952473861209526, -20.46827195828559809, -42.80032454360480187 ) ) ;
#42688 = CARTESIAN_POINT ( 'NONE',  ( 13.51721644893999930, -51.27681913022160387, -22.28354840475149956 ) ) ;
#42689 = CARTESIAN_POINT ( 'NONE',  ( 54.61320183681609564, 19.39270185280140169, -76.58475370837619778 ) ) ;
#42690 = B_SPLINE_CURVE_WITH_KNOTS ( 'NONE', 3,
 ( #45053, #24071, #4184, #20160, #48213, #9156, #36151, #32193 ),
 .UNSPECIFIED., .F., .F.,
 ( 4, 2, 2, 4 ),
 ( -0.1350635247397783956, -0.1243669311589359894, -0.1075965482636560000, -0.1052074838081859948 ),
 .UNSPECIFIED. ) ;
#42692 = B_SPLINE_CURVE_WITH_KNOTS ( 'NONE', 3,
 ( #47802, #27864, #19751, #19993, #36498, #16587, #602, #4801, #32540, #35990, #16078, #44121, #28372, #48312, #48835, #12677, #9002, #20768 ),
 .UNSPECIFIED., .F., .F.,
 ( 4, 2, 2, 2, 2, 2, 2, 2, 4 ),
 ( 0.5000015509581456907, 0.5625013570883774516, 0.6250011632186092125, 0.6875009693488410845, 0.7500007754790728454, 0.8125005816093046063, 0.8750003877395364782, 0.9375001938697682391, 1.000000000000000000 ),
 .UNSPECIFIED. ) ;
#42691 = CARTESIAN_POINT ( 'NONE',  ( 47.13794097070190503, -53.89583813975270488, -75.74423906255060501 ) ) ;
#42693 = CARTESIAN_POINT ( 'NONE',  ( 56.31194726212379464, 13.95803596900150012, -15.90921559078330105 ) ) ;
#42694 = CARTESIAN_POINT ( 'NONE',  ( 47.77115924678660264, 23.22414640103279737, -54.89636912190230333 ) ) ;
#42695 = CARTESIAN_POINT ( 'NONE',  ( 56.72051766772629833, -50.68676931991719670, -53.84018978630530228 ) ) ;
#42696 = CARTESIAN_POINT ( 'NONE',  ( 9.132806620530429242, -16.46867179815689752, -47.80861109115259211 ) ) ;
#42697 = CARTESIAN_POINT ( 'NONE',  ( 21.74289213372750140, -11.34042165171269900, -44.63985384860789907 ) ) ;
#42698 = ORIENTED_EDGE ( 'NONE', *, *, #51590, .F. ) ;
#42699 = CARTESIAN_POINT ( 'NONE',  ( 47.57154850773209631, 23.33333469726499843, -74.14999583207048772 ) ) ;
#42700 = CARTESIAN_POINT ( 'NONE',  ( 64.90488303983269702, 1.264791438333819906, -60.78603624114159487 ) ) ;
#42701 = VECTOR ( 'NONE', #49130, 1000.000000000000000 ) ;
#42702 = CARTESIAN_POINT ( 'NONE',  ( 11.27234840095610480, -9.289956386053781046, -50.79933430464781452 ) ) ;
#42703 = CARTESIAN_POINT ( 'NONE',  ( 104.6856170952499951, -2.032350560838469100, -102.2016796975540274 ) ) ;
#42704 = VECTOR ( 'NONE', #15413, 1000.000000000000000 ) ;
#42705 = CARTESIAN_POINT ( 'NONE',  ( 57.73379141935919989, 13.88381105532070059, -10.52253854761309881 ) ) ;
#42706 = AXIS2_PLACEMENT_3D ( 'NONE', #50651, #38339, #2429 ) ;
#42707 = DIRECTION ( 'NONE',  ( -4.537176718267040445E-11, -1.000000000000000000, 6.290312716002009228E-11 ) ) ;
#42708 = CARTESIAN_POINT ( 'NONE',  ( 82.34446853826591450, 14.37294419959810021, -47.68359979375730262 ) ) ;
#42709 = DIRECTION ( 'NONE',  ( 0.000000000000000000, 0.000000000000000000, 1.000000000000000000 ) ) ;
#42711 = CARTESIAN_POINT ( 'NONE',  ( 15.09848549043149468, -23.52720049154072868, -58.33399804516979970 ) ) ;
#42710 = CARTESIAN_POINT ( 'NONE',  ( 47.58828883988076086, 23.23481555469353665, -74.72737448183970344 ) ) ;
#42712 = ADVANCED_FACE ( 'NONE', ( #18478 ), #7207, .T. ) ;
#42713 = CARTESIAN_POINT ( 'NONE',  ( 24.04490467417627642, -15.59160216054836212, -71.50668363288305329 ) ) ;
#42714 = CARTESIAN_POINT ( 'NONE',  ( -33.07468191286329784, -5.899192223876280394, -56.92399776842329828 ) ) ;
#42715 = EDGE_LOOP ( 'NONE', ( #12113, #25093, #38010, #13936, #28747, #46959 ) ) ;
#42716 = CARTESIAN_POINT ( 'NONE',  ( 52.88917640181519886, -49.63475167565859891, -48.82176623077139510 ) ) ;
#42717 = ORIENTED_EDGE ( 'NONE', *, *, #2891, .F. ) ;
#42718 = CARTESIAN_POINT ( 'NONE',  ( 47.88935567426931073, 8.085927491590410909, -51.43431970325507763 ) ) ;
#42719 = CARTESIAN_POINT ( 'NONE',  ( 40.57649240635721100, -15.61618894467929941, -83.97002642401369599 ) ) ;
#42720 = CARTESIAN_POINT ( 'NONE',  ( 13.77293538034790110, 20.06110664901489926, -23.09858809179250017 ) ) ;
#42721 = CARTESIAN_POINT ( 'NONE',  ( 84.44784216359251161, 11.88381105532070059, -47.47585302082339354 ) ) ;
#42722 = CARTESIAN_POINT ( 'NONE',  ( 11.35694743959450115, -10.42745830638049931, -43.71596393528839286 ) ) ;
#42723 = CARTESIAN_POINT ( 'NONE',  ( 64.77076777328539947, 1.370387345317999994, -61.01480881516509669 ) ) ;
#42724 = CARTESIAN_POINT ( 'NONE',  ( 52.64535713109459891, 18.55400356624080160, -48.56190053269869367 ) ) ;
#42725 = CARTESIAN_POINT ( 'NONE',  ( 54.65216101584789499, -46.12197618676970734, -15.81768032851119798 ) ) ;
#42726 = LINE ( 'NONE', #34051, #25605 ) ;
#42727 = ORIENTED_EDGE ( 'NONE', *, *, #32329, .F. ) ;
#42728 = CARTESIAN_POINT ( 'NONE',  ( 12.26232734644089994, -8.789961311109230735, -34.62328075351209122 ) ) ;
#42729 = ORIENTED_EDGE ( 'NONE', *, *, #49692, .T. ) ;
#42730 = AXIS2_PLACEMENT_3D ( 'NONE', #30025, #10397, #9377 ) ;
#42731 = CARTESIAN_POINT ( 'NONE',  ( 72.93398937763220147, 1.264121749638659864, -68.99682374033621102 ) ) ;
#42732 = CARTESIAN_POINT ( 'NONE',  ( 8.815605938091740867, 32.05029769240140070, -46.67186391159280134 ) ) ;
#42733 = CARTESIAN_POINT ( 'NONE',  ( 73.02743803608620965, 1.099344084866040072, -62.24193811877859162 ) ) ;
#42734 = CARTESIAN_POINT ( 'NONE',  ( 11.43830175781249991, -65.36132525204969568, -18.07704217317780149 ) ) ;
#42735 = DIRECTION ( 'NONE',  ( 0.000000000000000000, 0.000000000000000000, -1.000000000000000000 ) ) ;
#42736 = CARTESIAN_POINT ( 'NONE',  ( 68.13393739769618662, -1.166188944679350081, -65.65000000000000568 ) ) ;
#42737 = CARTESIAN_POINT ( 'NONE',  ( 22.90093739726882660, -15.61526481454825088, -62.45278487061211337 ) ) ;
#42738 = CARTESIAN_POINT ( 'NONE',  ( 22.06336741109733524, -20.87868580843650079, -45.73877504285819384 ) ) ;
#42739 = VERTEX_POINT ( 'NONE', #26583 ) ;
#42740 = CARTESIAN_POINT ( 'NONE',  ( 64.95388650200969494, 1.388313565858560139, -70.27734465158509636 ) ) ;
#42741 = ORIENTED_EDGE ( 'NONE', *, *, #19092, .T. ) ;
#42742 = CARTESIAN_POINT ( 'NONE',  ( 10.76899899952330131, -63.11543068638779630, -45.20723331625340791 ) ) ;
#42743 = CARTESIAN_POINT ( 'NONE',  ( 9.807821837080062721, -10.75444719097494328, -47.00066525792952632 ) ) ;
#42744 = VERTEX_POINT ( 'NONE', #35757 ) ;
#42745 = EDGE_CURVE ( 'NONE', #14302, #38090, #40648, .T. ) ;
#42746 = CARTESIAN_POINT ( 'NONE',  ( 13.88455093916192951, -52.17615671833033275, -75.56421372420085447 ) ) ;
#42747 = CARTESIAN_POINT ( 'NONE',  ( 56.96124594780639683, 19.37506853770539905, -53.44837636194950647 ) ) ;
#42748 = CARTESIAN_POINT ( 'NONE',  ( 51.99242832924639401, 18.79345593400340064, -76.70333696056400186 ) ) ;
#42749 = ORIENTED_EDGE ( 'NONE', *, *, #44547, .F. ) ;
#42750 = DIRECTION ( 'NONE',  ( 1.000000000000000000, 0.000000000000000000, 0.000000000000000000 ) ) ;
#42751 = CARTESIAN_POINT ( 'NONE',  ( -31.36606260230380272, -62.82329572586585442, 11.14289321881345174 ) ) ;
#42752 = AXIS2_PLACEMENT_3D ( 'NONE', #50722, #22404, #47070 ) ;
#42753 = CARTESIAN_POINT ( 'NONE',  ( 14.98932469835694015, 21.70055148386502708, -76.14999999999994884 ) ) ;
#42754 = CARTESIAN_POINT ( 'NONE',  ( 17.63499105033369929, -32.15889263939740772, -34.64999999999999858 ) ) ;
#42755 = B_SPLINE_SURFACE_WITH_KNOTS ( 'NONE', 3, 3, ( 
 ( #15110, #31325, #11447, #11959, #27663, #43406, #7508, #23455, #47601, #15628, #43918, #40754, #39988, #20052, #403, #48897 ),
 ( #16389, #12731, #40494, #32345, #28948, #16643, #20559, #36043, #21086, #37087, #153, #16129, #36555, #50182, #50443, #21595 ),
 ( #17940, #21860, #45733, #37871, #26567, #34691, #18970, #23659, #27095, #39163, #40437, #864, #32805, #36494, #15817, #12156 ),
 ( #347, #16333, #37810, #33854, #25989, #42002, #22057, #30187, #43298, #35413, #30442, #2940, #18911, #537, #19935, #16271 ),
 ( #24362, #40375, #32472, #20699, #8937, #17056, #33277, #49556, #21217, #37228, #33538, #13140, #29852, #41935, #9958, #13390 ),
 ( #13894, #41408, #21481, #6035, #29603, #14149, #44832, #45087, #9705, #25665, #5772, #10228, #2880, #39046, #47172, #35085 ),
 ( #51088, #6295, #15186, #6815, #14665, #30635, #39294, #46659, #11002, #50321, #26186, #14407, #31147, #26444, #18848, #43235 ),
 ( #27222, #10742, #7327, #7074, #23274, #19108, #18594, #26970, #11260, #3401, #19368, #34308, #30375, #22769, #35350, #34570 ),
 ( #46916, #50575, #46400, #46137, #51350, #30118, #42197, #22253, #10488, #26698, #38260, #38523, #42460, #2353, #18327, #6547 ),
 ( #22512, #2622, #42979, #42720, #30888, #38788, #23024, #34831, #50832, #14924, #3140, #51859, #4668, #20380, #7841, #11521 ) ),
 .UNSPECIFIED., .F., .F., .F.,
 ( 4, 1, 1, 1, 1, 1, 1, 4 ),
 ( 4, 2, 2, 2, 2, 2, 2, 4 ),
 ( -5.223883000000000085E-09, 0.1428571428571430157, 0.2857142857142860315, 0.4285714285714289917, 0.5714285714285709528, 0.7142857142857139685, 0.8571428571428569843, 1.000000005223879995 ),
 ( -5.223902000000000352E-09, 0.4421500870759600410, 0.9474644723056518947, 1.263285963074209928, 1.421196708458489999, 1.673853901073329986, 2.078105409257089864, 2.526571926298299964 ),
 .UNSPECIFIED. ) ;
#42756 = CARTESIAN_POINT ( 'NONE',  ( 17.30174806873700177, -23.77823147657889891, -68.24709530556638981 ) ) ;
#42757 = CARTESIAN_POINT ( 'NONE',  ( 8.222964014181659564, -16.65193127518642768, -48.46600188287622757 ) ) ;
#42758 = LINE ( 'NONE', #47969, #26682 ) ;
#42759 = ORIENTED_EDGE ( 'NONE', *, *, #27890, .F. ) ;
#42760 = ORIENTED_EDGE ( 'NONE', *, *, #43713, .F. ) ;
#42761 = CARTESIAN_POINT ( 'NONE',  ( 59.34499803081109803, -3.116188944679349593, -15.68015151901639825 ) ) ;
#42762 = CARTESIAN_POINT ( 'NONE',  ( 23.04786251081229764, -12.84052085656660047, -54.11113779516239930 ) ) ;
#42763 = CARTESIAN_POINT ( 'NONE',  ( 10.29616392687819904, -11.80022295320810066, -32.14999999999999858 ) ) ;
#42764 = DIRECTION ( 'NONE',  ( 0.000000000000000000, 0.000000000000000000, 1.000000000000000000 ) ) ;
#42765 = CARTESIAN_POINT ( 'NONE',  ( 61.54865580197261465, 14.09499822944240677, -47.27157924453907611 ) ) ;
#42766 = DIRECTION ( 'NONE',  ( 0.000000000000000000, 0.000000000000000000, 1.000000000000000000 ) ) ;
#42767 = CARTESIAN_POINT ( 'NONE',  ( 43.41850781425760175, -45.38663701516029647, -7.209125745969769739 ) ) ;
#42768 = CARTESIAN_POINT ( 'NONE',  ( 22.23466283676619426, -10.53884220764341251, -61.28681395474006877 ) ) ;
#42769 = CARTESIAN_POINT ( 'NONE',  ( 9.705988999922061211, -20.77992791024760066, -58.29224725099440008 ) ) ;
#42770 = CARTESIAN_POINT ( 'NONE',  ( 21.38252174147899964, -21.31749193139690135, -32.14999999999999858 ) ) ;
#42771 = CARTESIAN_POINT ( 'NONE',  ( 56.43501562198250099, -50.77275378297979813, -74.43358758419878995 ) ) ;
#42773 = CARTESIAN_POINT ( 'NONE',  ( 11.97521368704360967, -10.20490852744658739, -59.74446477439609993 ) ) ;
#42772 = CARTESIAN_POINT ( 'NONE',  ( -10.41134978075270112, 11.60703557408290010, -6.431294820763719500 ) ) ;
#42774 = EDGE_CURVE ( 'NONE', #20020, #21835, #805, .T. ) ;
#42775 = CARTESIAN_POINT ( 'NONE',  ( 47.81335647231890107, -54.39749252969859583, -54.71582838609030119 ) ) ;
#42776 = DIRECTION ( 'NONE',  ( -1.000000000000000000, 0.000000000000000000, 0.000000000000000000 ) ) ;
#42777 = ORIENTED_EDGE ( 'NONE', *, *, #1104, .F. ) ;
#42778 = CARTESIAN_POINT ( 'NONE',  ( 14.90280893508995419, 21.76199782481209510, -76.14999999999999147 ) ) ;
#42779 = EDGE_CURVE ( 'NONE', #6345, #6332, #24823, .T. ) ;
#42780 = VECTOR ( 'NONE', #35241, 1000.000000000000000 ) ;
#42781 = CARTESIAN_POINT ( 'NONE',  ( 47.77676144020560400, 23.19303230712679920, -54.74761805967199990 ) ) ;
#42782 = CARTESIAN_POINT ( 'NONE',  ( 44.76356921293569968, -45.10235736362039916, -7.023953210218369492 ) ) ;
#42783 = CARTESIAN_POINT ( 'NONE',  ( 63.25402410758490390, 0.9098571636355680115, -62.15909090909049439 ) ) ;
#42784 = CARTESIAN_POINT ( 'NONE',  ( 61.09287626159920137, 14.33135539182030094, -47.61635106652619953 ) ) ;
#42785 = CIRCLE ( 'NONE', #12626, 35.00000000000000000 ) ;
#42786 = CARTESIAN_POINT ( 'NONE',  ( 11.28671401888810166, 33.77463329229920674, -16.86100853830619783 ) ) ;
#42787 = ADVANCED_FACE ( 'NONE', ( #11659 ), #19766, .F. ) ;
#42788 = CARTESIAN_POINT ( 'NONE',  ( 51.57064462373369906, 17.81647325063629950, -76.80688255937791098 ) ) ;
#42789 = CARTESIAN_POINT ( 'NONE',  ( 52.83359294848519738, 18.42653244547510027, -48.59872226080710078 ) ) ;
#42790 = CARTESIAN_POINT ( 'NONE',  ( 46.63393739769619373, -36.11618894467930119, -35.14999999999999858 ) ) ;
#42791 = LINE ( 'NONE', #46210, #43486 ) ;
#42792 = CARTESIAN_POINT ( 'NONE',  ( 55.30698993685479792, 16.11823302483700004, -26.47716174366970066 ) ) ;
#42793 = CARTESIAN_POINT ( 'NONE',  ( 50.72687041832384836, 4.467326087330391715, -76.27485697391391284 ) ) ;
#42794 = LINE ( 'NONE', #19700, #33709 ) ;
#42795 = DIRECTION ( 'NONE',  ( -0.8660254037844387076, -0.4999999999999998890, 1.110223024625155678E-16 ) ) ;
#42796 = CARTESIAN_POINT ( 'NONE',  ( 12.14978265628979237, -22.52869892617844272, -76.17435607522669727 ) ) ;
#42797 = CARTESIAN_POINT ( 'NONE',  ( 71.40743923234819590, 0.9234936569010840923, -60.62162712823539579 ) ) ;
#42798 = CARTESIAN_POINT ( 'NONE',  ( 10.77201485400030023, 32.03292712579329304, -45.20473333481510281 ) ) ;
#42799 = CARTESIAN_POINT ( 'NONE',  ( 72.93063970810558772, 1.138495779908299754, -62.11940254112219861 ) ) ;
#42800 = CARTESIAN_POINT ( 'NONE',  ( 65.70572775221249628, -32.85841248749620291, -18.95019544618720175 ) ) ;
#42801 = CARTESIAN_POINT ( 'NONE',  ( 9.799758126153289339, -13.15607537077775646, -65.57083617002002995 ) ) ;
#42802 = ORIENTED_EDGE ( 'NONE', *, *, #24642, .T. ) ;
#42803 = ORIENTED_EDGE ( 'NONE', *, *, #22106, .F. ) ;
#42804 = DIRECTION ( 'NONE',  ( 0.000000000000000000, 0.000000000000000000, -1.000000000000000000 ) ) ;
#42805 = CARTESIAN_POINT ( 'NONE',  ( 76.49486337784722423, -3.223960196710998094, -13.20528376621882671 ) ) ;
#42806 = VERTEX_POINT ( 'NONE', #51490 ) ;
#42807 = ADVANCED_FACE ( 'NONE', ( #21231 ), #15590, .T. ) ;
#42808 = CARTESIAN_POINT ( 'NONE',  ( 10.93389818273009872, -63.58325642793808896, -44.91480761438189973 ) ) ;
#42809 = CARTESIAN_POINT ( 'NONE',  ( 57.47931744391669895, -45.11451192150079947, -25.32996107807690223 ) ) ;
#42810 = CARTESIAN_POINT ( 'NONE',  ( 16.11774638449731967, -23.52717341023336672, -78.00832281184233352 ) ) ;
#42811 = CARTESIAN_POINT ( 'NONE',  ( 16.13393739769620083, -15.61618894467929941, -32.14999999999999858 ) ) ;
#42812 = DIRECTION ( 'NONE',  ( 0.1961161351381840723, -2.713878504639270283E-16, 0.9805806756909202226 ) ) ;
#42813 = ORIENTED_EDGE ( 'NONE', *, *, #32751, .F. ) ;
#42814 = FACE_BOUND ( 'NONE', #49636, .T. ) ;
#42815 = CARTESIAN_POINT ( 'NONE',  ( 44.79206433993918779, 6.785388388300961360, -66.35931098130210160 ) ) ;
#42816 = CARTESIAN_POINT ( 'NONE',  ( 11.97592558356920023, 33.51641353631480058, -24.42566912137219859 ) ) ;
#42817 = ORIENTED_EDGE ( 'NONE', *, *, #43530, .T. ) ;
#42818 = CARTESIAN_POINT ( 'NONE',  ( 23.76387005758689952, -12.49099332496719938, -37.66858791500939674 ) ) ;
#42819 = CARTESIAN_POINT ( 'NONE',  ( 52.10267377313040527, 1.883811054805347496, -20.31845379076632696 ) ) ;
#42820 = CARTESIAN_POINT ( 'NONE',  ( 14.38278649113999919, 19.81652936503730089, -21.89951529875269998 ) ) ;
#42821 = CARTESIAN_POINT ( 'NONE',  ( 22.82186787310235943, -16.68413300609983452, -50.50321592674860938 ) ) ;
#42822 = CARTESIAN_POINT ( 'NONE',  ( 61.79720211019959208, -29.51961015981989789, -16.03830591840080189 ) ) ;
#42823 = VECTOR ( 'NONE', #50831, 1000.000000000000000 ) ;
#42824 =( BOUNDED_CURVE ( )  B_SPLINE_CURVE ( 3, ( #41797, #49679, #13770, #38389 ),
 .UNSPECIFIED., .F., .T. ) 
 B_SPLINE_CURVE_WITH_KNOTS ( ( 4, 4 ),
 ( 1.570796326794896558, 2.356194490192377700 ),
 .UNSPECIFIED. ) 
 CURVE ( )  GEOMETRIC_REPRESENTATION_ITEM ( )  RATIONAL_B_SPLINE_CURVE ( ( 1.000000000000000000, 0.9492530216741870142, 0.9492530216741870142, 1.000000000000000000 ) ) 
 REPRESENTATION_ITEM ( '' )  );
#42825 = DIRECTION ( 'NONE',  ( 0.000000000000000000, 0.000000000000000000, 1.000000000000000000 ) ) ;
#42826 = CARTESIAN_POINT ( 'NONE',  ( 46.73688746986190523, -53.63908013404079611, -75.98233228156729524 ) ) ;
#42827 = AXIS2_PLACEMENT_3D ( 'NONE', #42221, #30143, #15215 ) ;
#42828 = CARTESIAN_POINT ( 'NONE',  ( 49.56322960257909926, 13.74100540729780029, -7.475321071136599826 ) ) ;
#42829 = EDGE_CURVE ( 'NONE', #42328, #814, #17347, .T. ) ;
#42830 = VECTOR ( 'NONE', #21759, 1000.000000000000000 ) ;
#42831 = CARTESIAN_POINT ( 'NONE',  ( 16.13393739769620083, -15.61618894467929941, -81.23899999999999011 ) ) ;
#42832 = DIRECTION ( 'NONE',  ( 0.000000000000000000, 0.000000000000000000, 1.000000000000000000 ) ) ;
#42833 = CARTESIAN_POINT ( 'NONE',  ( 9.678901947420619933, -20.07928830891850325, -80.09494718402959279 ) ) ;
#42834 = VERTEX_POINT ( 'NONE', #25419 ) ;
#42835 = CARTESIAN_POINT ( 'NONE',  ( 56.06469054980239974, -46.69807554794920179, -26.34903941785619708 ) ) ;
#42836 = CARTESIAN_POINT ( 'NONE',  ( -4.162434749930929989, -49.37281588411619992, -7.617592385375469455 ) ) ;
#42837 = CARTESIAN_POINT ( 'NONE',  ( 75.71017558016721694, -8.423768395189359381, -11.72022506976029987 ) ) ;
#42838 = CARTESIAN_POINT ( 'NONE',  ( 75.12127646723587304, 13.76128322658033021, -14.64863796607091473 ) ) ;
#42839 = FACE_OUTER_BOUND ( 'NONE', #30533, .T. ) ;
#42840 = DIRECTION ( 'NONE',  ( -0.3535533905932768950, -0.6123724356957934711, 0.7071067811865469066 ) ) ;
#42841 = VECTOR ( 'NONE', #50233, 1000.000000000000000 ) ;
#42842 = DIRECTION ( 'NONE',  ( 0.000000000000000000, -0.9319748226751538578, -0.3625230060280530409 ) ) ;
#42843 = CARTESIAN_POINT ( 'NONE',  ( 82.13853704237929776, -45.60474347597770617, -47.68296857959820301 ) ) ;
#42844 = FACE_OUTER_BOUND ( 'NONE', #11502, .T. ) ;
#42845 = CARTESIAN_POINT ( 'NONE',  ( 41.00922577670660019, 13.27405061951239951, -4.614727581921130195 ) ) ;
#42846 = ADVANCED_FACE ( 'NONE', ( #47563 ), #8951, .T. ) ;
#42847 = DIRECTION ( 'NONE',  ( -1.000000000000000000, 0.000000000000000000, 0.000000000000000000 ) ) ;
#42848 = CARTESIAN_POINT ( 'NONE',  ( 15.05440318628160057, -53.11618894467930119, -76.14999999999999147 ) ) ;
#42849 = CARTESIAN_POINT ( 'NONE',  ( 70.83745409581581498, -49.21324915459896943, -75.95351669811965678 ) ) ;
#42850 = CARTESIAN_POINT ( 'NONE',  ( 76.38512529972561538, -43.26453402920058977, -13.94652733128153344 ) ) ;
#42851 = CARTESIAN_POINT ( 'NONE',  ( 18.58833069766529889, -51.79024427787479823, -75.14498753491568550 ) ) ;
#42852 = CARTESIAN_POINT ( 'NONE',  ( 60.78568630568080522, -44.33970749964649372, -9.604110006574771319 ) ) ;
#42853 = ORIENTED_EDGE ( 'NONE', *, *, #1535, .T. ) ;
#42854 = AXIS2_PLACEMENT_3D ( 'NONE', #27161, #47364, #3848 ) ;
#42855 = CARTESIAN_POINT ( 'NONE',  ( 13.66038192480450064, -22.64386406956009878, -67.67506889758119826 ) ) ;
#42856 = CARTESIAN_POINT ( 'NONE',  ( 63.57924418363759855, 1.254613999360089993, -61.86253808879629901 ) ) ;
#42857 = ORIENTED_EDGE ( 'NONE', *, *, #26740, .F. ) ;
#42858 = CARTESIAN_POINT ( 'NONE',  ( 22.90111010729205177, -15.61618905465553553, -68.45282213299155671 ) ) ;
#42859 = AXIS2_PLACEMENT_3D ( 'NONE', #45945, #38077, #11079 ) ;
#42860 = DIRECTION ( 'NONE',  ( 0.000000000000000000, 0.000000000000000000, -1.000000000000000000 ) ) ;
#42861 = CARTESIAN_POINT ( 'NONE',  ( 73.09272852564158995, 1.276058558775509999, -68.69062364193268877 ) ) ;
#42862 = CARTESIAN_POINT ( 'NONE',  ( 7.492845759203685674, -61.18022026567161475, -20.13893727953967172 ) ) ;
#42863 = CARTESIAN_POINT ( 'NONE',  ( 9.905352207939319698, -18.56992711498079984, -81.23899999999999011 ) ) ;
#42864 = CARTESIAN_POINT ( 'NONE',  ( 43.16098550650539778, -45.75650059835369632, -7.511432296416719723 ) ) ;
#42865 = ORIENTED_EDGE ( 'NONE', *, *, #2613, .T. ) ;
#42866 = ORIENTED_EDGE ( 'NONE', *, *, #16186, .T. ) ;
#42867 = VERTEX_POINT ( 'NONE', #23675 ) ;
#42868 = CARTESIAN_POINT ( 'NONE',  ( 16.13393739769620083, -15.61618894467929941, -5.966499999999999915 ) ) ;
#42869 = CARTESIAN_POINT ( 'NONE',  ( 23.37832472556300090, -13.25337072732409816, -81.23899999999999011 ) ) ;
#42870 = CARTESIAN_POINT ( 'NONE',  ( 82.48407194341798743, -45.09832794361063435, -46.54736621596860147 ) ) ;
#42871 = EDGE_LOOP ( 'NONE', ( #21365, #41862, #4247, #47541, #2380, #687, #35530, #27155 ) ) ;
#42872 = CARTESIAN_POINT ( 'NONE',  ( 22.26208788750698275, -12.63896016920059218, -80.30869283850560691 ) ) ;
#42873 = ORIENTED_EDGE ( 'NONE', *, *, #1368, .T. ) ;
#42874 = CARTESIAN_POINT ( 'NONE',  ( 11.27230637084539033, -9.289988185851985492, -63.08399882191634589 ) ) ;
#42875 = CARTESIAN_POINT ( 'NONE',  ( 25.63393739769619728, -15.61618894467930119, -18.35000000000000142 ) ) ;
#42876 = ORIENTED_EDGE ( 'NONE', *, *, #41989, .T. ) ;
#42877 = CARTESIAN_POINT ( 'NONE',  ( 13.88455142272560039, 20.94377921756336036, -75.56421430877985301 ) ) ;
#42878 = CARTESIAN_POINT ( 'NONE',  ( 51.20054084488780433, -50.75953116010929733, -76.16661697631359118 ) ) ;
#42879 = CARTESIAN_POINT ( 'NONE',  ( 60.66491735500950000, 14.33979589326570014, -47.29697835118949456 ) ) ;
#42880 = EDGE_CURVE ( 'NONE', #13981, #15078, #26523, .T. ) ;
#42881 = ADVANCED_FACE ( 'NONE', ( #39692 ), #14004, .T. ) ;
#42882 = LINE ( 'NONE', #42097, #17199 ) ;
#42883 = CARTESIAN_POINT ( 'NONE',  ( 40.90236900589889757, -44.69077732174059747, -4.970360716545750179 ) ) ;
#42884 = EDGE_CURVE ( 'NONE', #32800, #44094, #32694, .T. ) ;
#42885 = DIRECTION ( 'NONE',  ( 0.000000000000000000, 0.000000000000000000, -1.000000000000000000 ) ) ;
#42886 = CARTESIAN_POINT ( 'NONE',  ( -3.426429430513819874, 17.54101937228130126, -5.615273139885949227 ) ) ;
#42887 = CIRCLE ( 'NONE', #31958, 34.41780050634729804 ) ;
#42888 = VECTOR ( 'NONE', #8677, 1000.000000000000114 ) ;
#42889 = CARTESIAN_POINT ( 'NONE',  ( 64.66196796819860992, 1.134321519919950116, -70.48604978123970000 ) ) ;
#42890 = CARTESIAN_POINT ( 'NONE',  ( 21.72984300404249680, -19.90902013391950121, -43.05547522733549926 ) ) ;
#42891 = CARTESIAN_POINT ( 'NONE',  ( 17.91327630046971819, -51.14555453227458770, -74.54430098196459653 ) ) ;
#42892 = CARTESIAN_POINT ( 'NONE',  ( 8.353661292524970250, -14.58951864196060022, -56.32926786494370219 ) ) ;
#42893 = ORIENTED_EDGE ( 'NONE', *, *, #25464, .T. ) ;
#42894 = FACE_OUTER_BOUND ( 'NONE', #7615, .T. ) ;
#42895 = CARTESIAN_POINT ( 'NONE',  ( 57.55751162087899786, 18.96618911681419917, -52.70112124855629787 ) ) ;
#42896 = CARTESIAN_POINT ( 'NONE',  ( 71.96892370708050635, 1.258806274518780022, -70.16925935983108786 ) ) ;
#42897 = CARTESIAN_POINT ( 'NONE',  ( 45.11971453824414624, -40.03891821604290158, -61.23139901406670305 ) ) ;
#42898 = CARTESIAN_POINT ( 'NONE',  ( 15.65736449273109976, 19.70849029160099875, -20.65166207265459875 ) ) ;
#42899 = CARTESIAN_POINT ( 'NONE',  ( 20.17759926101160062, -10.17506160504910007, -32.14999999999999858 ) ) ;
#42900 = EDGE_CURVE ( 'NONE', #17894, #19377, #50943, .T. ) ;
#42901 = CARTESIAN_POINT ( 'NONE',  ( 61.31732713205895635, 14.08360349558539149, -47.18610833908295632 ) ) ;
#42902 = CARTESIAN_POINT ( 'NONE',  ( 48.02939153114380133, -54.36963205275340272, -55.28067537372130147 ) ) ;
#42903 = CARTESIAN_POINT ( 'NONE',  ( 24.04464085855207856, -15.54218241719844329, -45.50469856519234924 ) ) ;
#42904 = CARTESIAN_POINT ( 'NONE',  ( -5.159222269204799538, -47.09623647380401934, -4.453993764612231843 ) ) ;
#42905 = CARTESIAN_POINT ( 'NONE',  ( 24.04493740884162634, -16.65171840150751237, -45.83401224397450591 ) ) ;
#42906 = CARTESIAN_POINT ( 'NONE',  ( 47.77546308418779830, 23.20957882008939777, -54.82267176636759842 ) ) ;
#42907 = ORIENTED_EDGE ( 'NONE', *, *, #23527, .T. ) ;
#42908 = CARTESIAN_POINT ( 'NONE',  ( 9.081943790392930538, -15.50689421925920009, -75.85211268767389470 ) ) ;
#42909 = ORIENTED_EDGE ( 'NONE', *, *, #1431, .T. ) ;
#42910 = CARTESIAN_POINT ( 'NONE',  ( 71.25658036288379549, 1.391252479931859964, -70.26382307879899258 ) ) ;
#42911 = CARTESIAN_POINT ( 'NONE',  ( 60.27779889700099147, -45.75868226597979316, -47.23595182050330266 ) ) ;
#42912 = CARTESIAN_POINT ( 'NONE',  ( 56.94228693352650339, -47.50625043831589522, -47.82842110489030318 ) ) ;
#42913 = CARTESIAN_POINT ( 'NONE',  ( 63.93393739769619089, 10.88381105532070059, -62.44999999999999574 ) ) ;
#42915 = CARTESIAN_POINT ( 'NONE',  ( 44.43741329154635622, -33.13124401929711382, -48.95770300930330166 ) ) ;
#42914 = PLANE ( 'NONE',  #30717 ) ;
#42916 = DIRECTION ( 'NONE',  ( 3.556943099846429769E-14, -1.469246684736110336E-14, 1.000000000000000000 ) ) ;
#42917 = CARTESIAN_POINT ( 'NONE',  ( 15.09846545302023557, -23.52719806942911518, -42.04933457646342276 ) ) ;
#42918 = CARTESIAN_POINT ( 'NONE',  ( 24.04507396969289346, -15.61618901627517531, -67.50767071486835391 ) ) ;
#42919 = VERTEX_POINT ( 'NONE', #20395 ) ;
#42920 = FACE_OUTER_BOUND ( 'NONE', #4088, .T. ) ;
#42921 = VERTEX_POINT ( 'NONE', #8110 ) ;
#42922 = ORIENTED_EDGE ( 'NONE', *, *, #21884, .T. ) ;
#42923 = CARTESIAN_POINT ( 'NONE',  ( 12.33251669429900055, -64.64566256145140244, -15.86092359077770020 ) ) ;
#42924 = CARTESIAN_POINT ( 'NONE',  ( 68.13393739769620083, 19.38381105532069881, -75.00000000000000000 ) ) ;
#42925 = CARTESIAN_POINT ( 'NONE',  ( 76.44421473112753063, -24.47276274790905504, -12.98703123328389708 ) ) ;
#42926 = CARTESIAN_POINT ( 'NONE',  ( 9.020077921220060801, -63.39297508468359865, -46.63174122437119706 ) ) ;
#42927 = VECTOR ( 'NONE', #45836, 1000.000000000000000 ) ;
#42928 = ORIENTED_EDGE ( 'NONE', *, *, #41482, .T. ) ;
#42929 = VERTEX_POINT ( 'NONE', #32431 ) ;
#42930 = CARTESIAN_POINT ( 'NONE',  ( 71.57216560976189612, 1.132579237369250036, -60.79187696645490036 ) ) ;
#42931 = CARTESIAN_POINT ( 'NONE',  ( 11.19961559249191474, -65.24734874261105233, -22.25048313876769868 ) ) ;
#42932 = CARTESIAN_POINT ( 'NONE',  ( -1.453061824043200501, -7.771731286528777538, -43.67210485546797827 ) ) ;
#42933 = CARTESIAN_POINT ( 'NONE',  ( 22.90086341797264780, -15.61618933298137790, -46.45282805145726002 ) ) ;
#42934 = CARTESIAN_POINT ( 'NONE',  ( 64.25188488369910544, -0.1060032360258039985, -16.75951320883940099 ) ) ;
#42935 = CARTESIAN_POINT ( 'NONE',  ( 51.75950599516050232, -49.44977665203700212, -76.84761942479970287 ) ) ;
#42936 = CARTESIAN_POINT ( 'NONE',  ( 16.13393739769620083, -15.61618894467929941, -44.64999999999999858 ) ) ;
#42937 = VERTEX_POINT ( 'NONE', #8624 ) ;
#42938 = CARTESIAN_POINT ( 'NONE',  ( 9.351597708753779159, -11.46406213175773914, -32.96709167677747132 ) ) ;
#42939 = DIRECTION ( 'NONE',  ( 0.000000000000000000, 0.000000000000000000, -1.000000000000000000 ) ) ;
#42940 = ORIENTED_EDGE ( 'NONE', *, *, #48917, .T. ) ;
#42941 = CARTESIAN_POINT ( 'NONE',  ( 19.54197222412561530, -9.703303471313775574, -52.11948516037260504 ) ) ;
#42942 = CARTESIAN_POINT ( 'NONE',  ( 59.93898548971230156, -46.07977442274060564, -47.78350827547860291 ) ) ;
#42943 = CARTESIAN_POINT ( 'NONE',  ( 23.86338609116459963, -16.97352843302460101, -44.06782744062260093 ) ) ;
#42944 = EDGE_CURVE ( 'NONE', #8804, #17463, #24571, .T. ) ;
#42945 = CARTESIAN_POINT ( 'NONE',  ( 13.90974566255180100, -51.18269991979300215, -22.51683827224059797 ) ) ;
#42946 = CIRCLE ( 'NONE', #20305, 23.50000000000000000 ) ;
#42947 = DIRECTION ( 'NONE',  ( -1.000000000000000000, 0.000000000000000000, 0.000000000000000000 ) ) ;
#42948 = EDGE_CURVE ( 'NONE', #12281, #32578, #28258, .T. ) ;
#42949 = CARTESIAN_POINT ( 'NONE',  ( 56.71523363900320192, 14.03280086630570089, -17.52449187449219536 ) ) ;
#42950 = CARTESIAN_POINT ( 'NONE',  ( 60.90942164635529821, -45.48565787205490096, -47.35587748028390109 ) ) ;
#42951 = CARTESIAN_POINT ( 'NONE',  ( 56.58636862550530111, -50.60438040973590290, -53.13121941639199974 ) ) ;
#42952 = CARTESIAN_POINT ( 'NONE',  ( 18.19108902640479997, -22.36234980482430146, -39.25296653628179655 ) ) ;
#42953 = CYLINDRICAL_SURFACE ( 'NONE', #33498, 6.766999999999998572 ) ;
#42954 = ORIENTED_EDGE ( 'NONE', *, *, #1873, .T. ) ;
#42955 = CARTESIAN_POINT ( 'NONE',  ( 47.61801188784319550, 23.31248625996650148, -74.17383159519339131 ) ) ;
#42956 = CARTESIAN_POINT ( 'NONE',  ( 65.05887334876679517, 1.388715606738730068, -61.01996879627380110 ) ) ;
#42957 = B_SPLINE_CURVE_WITH_KNOTS ( 'NONE', 3,
 ( #3172, #42497, #22803, #18115, #50868, #50089, #10262, #30671, #19143, #34082, #38824, #14185, #11037, #30157, #38562, #6329, #42757, #30923 ),
 .UNSPECIFIED., .F., .F.,
 ( 4, 2, 2, 2, 2, 2, 2, 2, 4 ),
 ( 0.5000006933586850222, 0.5625006066888493805, 0.6250005200190137389, 0.6875004333491780972, 0.7500003466793425666, 0.8125002600095068139, 0.8750001733396712833, 0.9375000866698356417, 1.000000000000000000 ),
 .UNSPECIFIED. ) ;
#42958 = CARTESIAN_POINT ( 'NONE',  ( 23.61468320491609774, 17.54226184052379978, -35.01184033120630090 ) ) ;
#42959 = AXIS2_PLACEMENT_3D ( 'NONE', #13324, #44766, #37164 ) ;
#42960 = CARTESIAN_POINT ( 'NONE',  ( -0.007164427059776000244, -10.48291004383190028, -34.77269723891829756 ) ) ;
#42961 = CARTESIAN_POINT ( 'NONE',  ( 15.41380670901278194, -50.77307959834621442, -20.47803142984178493 ) ) ;
#42962 = CONICAL_SURFACE ( 'NONE', #38773, 7.500000000000000000, 0.7853981633974476129 ) ;
#42963 = DIRECTION ( 'NONE',  ( -0.5109955813515499878, 0.8595833385072046973, 0.000000000000000000 ) ) ;
#42964 = LINE ( 'NONE', #13880, #40642 ) ;
#42965 = EDGE_CURVE ( 'NONE', #42744, #47075, #13977, .T. ) ;
#42966 = CARTESIAN_POINT ( 'NONE',  ( 82.13853704237929776, 14.12152868491880042, -47.32252334011910477 ) ) ;
#42967 = CARTESIAN_POINT ( 'NONE',  ( 0.09557987621370379883, 19.93481762610629815, -35.07694834390559890 ) ) ;
#42969 = CARTESIAN_POINT ( 'NONE',  ( 83.89200044194980421, -48.61618894467930119, -53.92796738110899923 ) ) ;
#42968 = DIRECTION ( 'NONE',  ( 0.000000000000000000, 0.000000000000000000, -1.000000000000000000 ) ) ;
#42970 = EDGE_CURVE ( 'NONE', #4421, #26368, #28357, .T. ) ;
#42971 = CARTESIAN_POINT ( 'NONE',  ( 9.925381647341668057, -20.56393483659768151, -32.57822336751156200 ) ) ;
#42972 = CARTESIAN_POINT ( 'NONE',  ( 68.13393739769620083, 19.38381105532069881, -71.50000000000000000 ) ) ;
#42973 = CARTESIAN_POINT ( 'NONE',  ( 49.08014769244979902, 22.68967210332029794, -55.22540290251299666 ) ) ;
#42974 = ORIENTED_EDGE ( 'NONE', *, *, #25525, .T. ) ;
#42975 = CARTESIAN_POINT ( 'NONE',  ( 52.78692773688430151, -49.69208888116699541, -48.74514769400369829 ) ) ;
#42976 = VERTEX_POINT ( 'NONE', #742 ) ;
#42977 = CARTESIAN_POINT ( 'NONE',  ( 47.66931075806890306, 8.074467705775857596, -52.52531625216943922 ) ) ;
#42978 = CARTESIAN_POINT ( 'NONE',  ( 15.09848983909765785, -23.52720101742690773, -74.33399818031571726 ) ) ;
#42979 = CARTESIAN_POINT ( 'NONE',  ( 13.68997053979789946, 20.12589560456379800, -23.13969475654330310 ) ) ;
#42980 = FACE_OUTER_BOUND ( 'NONE', #33165, .T. ) ;
#42981 = CARTESIAN_POINT ( 'NONE',  ( 16.72752280990699703, -22.64400617729399912, -58.92599869950339553 ) ) ;
#42982 = CARTESIAN_POINT ( 'NONE',  ( 52.62463376634089940, 18.57086902152009955, -48.47378032971769812 ) ) ;
#42983 = CARTESIAN_POINT ( 'NONE',  ( 56.18245545401309471, -45.53975730964529589, -17.22565076933249983 ) ) ;
#42984 = CYLINDRICAL_SURFACE ( 'NONE', #48227, 9.999999999999998224 ) ;
#42985 = AXIS2_PLACEMENT_3D ( 'NONE', #41866, #5207, #25346 ) ;
#42986 = EDGE_LOOP ( 'NONE', ( #46397, #33370, #23929, #16719 ) ) ;
#42987 = CARTESIAN_POINT ( 'NONE',  ( 14.76533666768029995, -8.292680193320569160, -80.50853572988759765 ) ) ;
#42988 = ORIENTED_EDGE ( 'NONE', *, *, #23964, .F. ) ;
#42989 = CARTESIAN_POINT ( 'NONE',  ( 72.80507874878320251, 1.371509258145890087, -68.88889814452579685 ) ) ;
#42990 = CARTESIAN_POINT ( 'NONE',  ( 9.422115487779029408, 32.29033719602479380, -46.51238083606079954 ) ) ;
#42991 = CARTESIAN_POINT ( 'NONE',  ( 72.74645547301390991, 1.390806392144110060, -62.43047455269960011 ) ) ;
#42992 = DIRECTION ( 'NONE',  ( 0.000000000000000000, 0.000000000000000000, 1.000000000000000000 ) ) ;
#42993 = CARTESIAN_POINT ( 'NONE',  ( 52.90434498377167216, -49.66345680823592090, -49.01850774012503820 ) ) ;
#42994 = DIRECTION ( 'NONE',  ( 0.000000000000000000, 0.000000000000000000, 1.000000000000000000 ) ) ;
#42995 = CARTESIAN_POINT ( 'NONE',  ( 49.70112820465350012, -53.65753597205910097, -55.00786376658719945 ) ) ;
#42996 = ORIENTED_EDGE ( 'NONE', *, *, #10408, .T. ) ;
#42997 = CARTESIAN_POINT ( 'NONE',  ( 64.64302830678690270, 0.9098571636355550218, -70.52991329011150867 ) ) ;
#42998 = ORIENTED_EDGE ( 'NONE', *, *, #41839, .F. ) ;
#42999 = CARTESIAN_POINT ( 'NONE',  ( 10.48761941044149815, -63.17386106513639277, -45.62707961905420717 ) ) ;
#43000 = CARTESIAN_POINT ( 'NONE',  ( 69.22748654599821805, 19.47158195952120963, -71.50000000000200373 ) ) ;
#43001 = EDGE_LOOP ( 'NONE', ( #10154, #1553, #205, #31743 ) ) ;
#43002 = DIRECTION ( 'NONE',  ( 0.000000000000000000, 0.000000000000000000, 1.000000000000000000 ) ) ;
#43003 = CARTESIAN_POINT ( 'NONE',  ( 57.35856958860869526, 18.90358493063820333, -52.61941485291330167 ) ) ;
#43004 = CARTESIAN_POINT ( 'NONE',  ( 53.72303973069330141, 19.38806196010829908, -76.82797360176211043 ) ) ;
#43005 = CIRCLE ( 'NONE', #3637, 30.50439988982899564 ) ;
#43006 = ORIENTED_EDGE ( 'NONE', *, *, #51438, .T. ) ;
#43007 = CIRCLE ( 'NONE', #36276, 7.910999999999997812 ) ;
#43008 = DIRECTION ( 'NONE',  ( -1.000000000000000000, 0.000000000000000000, 0.000000000000000000 ) ) ;
#43009 = CARTESIAN_POINT ( 'NONE',  ( 67.35174094906719233, -47.86618894467930119, -50.14999999999999858 ) ) ;
#43010 = FACE_OUTER_BOUND ( 'NONE', #49957, .T. ) ;
#43011 = CARTESIAN_POINT ( 'NONE',  ( 20.99560049988850352, -9.290011782261316853, -69.50066706253579696 ) ) ;
#43012 = CARTESIAN_POINT ( 'NONE',  ( 18.24066274319899961, -7.644713022709090033, -59.37457502644110008 ) ) ;
#43013 = EDGE_CURVE ( 'NONE', #9287, #14211, #34910, .T. ) ;
#43014 = DIRECTION ( 'NONE',  ( -0.4640893551880601597, 0.8857883891771953788, 0.000000000000000000 ) ) ;
#43015 = DIRECTION ( 'NONE',  ( 0.3569024281753349626, 0.000000000000000000, 0.9341416684649872515 ) ) ;
#43016 = ORIENTED_EDGE ( 'NONE', *, *, #882, .T. ) ;
#43017 = ORIENTED_EDGE ( 'NONE', *, *, #39466, .F. ) ;
#43018 = CARTESIAN_POINT ( 'NONE',  ( -22.71090128286022036, -12.19468477084010871, -54.67917393425321393 ) ) ;
#43019 = CARTESIAN_POINT ( 'NONE',  ( 8.955746707395579875, -13.62112698603560190, -53.31894848452630242 ) ) ;
#43020 = CARTESIAN_POINT ( 'NONE',  ( 54.29943625382440331, 13.88381105524610071, -13.69441485379169876 ) ) ;
#43021 = LINE ( 'NONE', #39848, #9935 ) ;
#43022 = CIRCLE ( 'NONE', #26273, 0.4934432871681592725 ) ;
#43023 = DIRECTION ( 'NONE',  ( 1.000000000000000000, 0.000000000000000000, 0.000000000000000000 ) ) ;
#43024 = FACE_OUTER_BOUND ( 'NONE', #28362, .T. ) ;
#43025 = CARTESIAN_POINT ( 'NONE',  ( 68.13393739769840352, -50.61618894467879670, -73.25000000000220268 ) ) ;
#43026 = CARTESIAN_POINT ( 'NONE',  ( 12.17742765527019877, 33.84218639868790035, -16.46016921338960159 ) ) ;
#43027 = B_SPLINE_CURVE_WITH_KNOTS ( 'NONE', 3,
 ( #26642, #38204, #5978, #21934 ),
 .UNSPECIFIED., .F., .F.,
 ( 4, 4 ),
 ( 3.936509634373229982, 4.045282574772550710 ),
 .UNSPECIFIED. ) ;
#43028 = CARTESIAN_POINT ( 'NONE',  ( 20.33320876516510012, -22.71188064396640272, -63.83757242544770349 ) ) ;
#43029 = CARTESIAN_POINT ( 'NONE',  ( 20.71981744919569834, -21.94173720618249845, -32.14999999999999858 ) ) ;
#43030 = CARTESIAN_POINT ( 'NONE',  ( 53.86687988220850087, -51.12005429169590087, -75.69951437311600273 ) ) ;
#43032 = CARTESIAN_POINT ( 'NONE',  ( 11.07421692656308210, -55.29505889823902010, -44.42833690484276588 ) ) ;
#43031 = CARTESIAN_POINT ( 'NONE',  ( -1.367282239498279983, 19.54806105385790005, -6.357905677808130207 ) ) ;
#43034 = ADVANCED_FACE ( 'NONE', ( #12823 ), #17266, .T. ) ;
#43033 = CARTESIAN_POINT ( 'NONE',  ( 16.13393739769620083, -15.61618894467929941, -14.65000000000000036 ) ) ;
#43035 = CARTESIAN_POINT ( 'NONE',  ( 47.13393739769619373, -36.11618894467930119, -35.14999999999999858 ) ) ;
#43036 = ORIENTED_EDGE ( 'NONE', *, *, #18550, .F. ) ;
#43037 = CARTESIAN_POINT ( 'NONE',  ( 23.36719009671439906, 16.90943255703749770, -48.24693239604849992 ) ) ;
#43038 = CARTESIAN_POINT ( 'NONE',  ( 47.57263996198259548, 23.32900398977909973, -54.92582527468099585 ) ) ;
#43039 = CARTESIAN_POINT ( 'NONE',  ( 41.84490955069979634, -44.86154966424449952, -5.635703470643719903 ) ) ;
#43040 = DIRECTION ( 'NONE',  ( 1.000000000000000000, 2.460964292799963328E-14, 0.000000000000000000 ) ) ;
#43041 = CARTESIAN_POINT ( 'NONE',  ( 60.80565946055000381, 14.31573824510140014, -47.42904253344379839 ) ) ;
#43042 = CARTESIAN_POINT ( 'NONE',  ( 10.52283474022480014, -10.71494210199229968, -79.46119573552070392 ) ) ;
#43043 = CARTESIAN_POINT ( 'NONE',  ( 52.04689645930250208, 18.41021695652339929, -77.05403426700469538 ) ) ;
#43044 = CARTESIAN_POINT ( 'NONE',  ( 52.82121948977260217, 18.43301524717529816, -48.53631916346480324 ) ) ;
#43045 = CARTESIAN_POINT ( 'NONE',  ( 16.13393739769620083, -15.61618894467929941, -643.2998782751060389 ) ) ;
#43046 = CARTESIAN_POINT ( 'NONE',  ( 52.89416330280510437, -49.62717582914000047, -48.70339649242369973 ) ) ;
#43047 = CARTESIAN_POINT ( 'NONE',  ( 53.99942095567629252, 17.28615893591289776, -26.84178626193609674 ) ) ;
#43048 = CARTESIAN_POINT ( 'NONE',  ( 51.41560511219569918, 21.47411202558799914, -53.77857906372980068 ) ) ;
#43049 = B_SPLINE_CURVE_WITH_KNOTS ( 'NONE', 3,
 ( #15845, #43126, #35509, #7983, #11931, #22915, #16099, #39188, #23684, #23935, #35764, #35242, #27633, #51747, #43888, #31806, #43380, #39447, #15075, #3026, #39957, #4051, #20016, #38934, #50976, #7477, #27122, #18999, #51498, #15340, #3548, #23426, #46806, #7218, #42869, #10895, #6964, #36009, #27376, #47571, #124, #11669, #15599, #31551, #26859, #47068, #19518, #47826, #11154, #23171, #3284, #31293, #47323, #11414, #43636, #7739, #39701, #3805, #19777, #21310, #48079, #40984, #13227, #9290, #28652, #24966, #626, #12963, #16885, #40210, #8500, #32831, #40463, #29176, #44920, #4558, #36782, #12698, #5356, #45178, #48598, #44654, #5096, #12177, #24189, #36522, #20527, #16609, #32567, #28915, #25236, #8238, #8761, #9022, #48333, #28136, #33097, #21050, #24709, #40727, #4822, #20790, #890, #41243, #48857, #37312, #37053, #1149, #17146, #49128, #28395, #1412, #32058, #44142, #4299, #20271, #24449, #36264 ),
 .UNSPECIFIED., .F., .F.,
 ( 4, 3, 3, 3, 3, 3, 3, 3, 3, 3, 3, 3, 3, 3, 3, 3, 3, 3, 3, 3, 3, 3, 3, 3, 3, 3, 3, 3, 3, 3, 3, 3, 3, 3, 3, 3, 3, 3, 3, 4 ),
 ( -1.528706106645210117, -1.467014400978620126, -1.462406257103989971, -1.400361489177680108, -1.359972591548769927, -1.338075497077110043, -1.325535052222839960, -1.316390772004420118, -1.255261729574910001, -1.194475196635949921, -1.135862752391179953, -1.120187264403469829, -1.112461740117050013, -1.077250308146409985, -1.017356745748480007, -0.9572232276135819173, -0.8973750758446790154, -0.8492288645832469784, -0.8273183250403219891, -0.8205642567938971066, -0.7619152418095799240, -0.7047902307989519777, -0.6459350209392840103, -0.5874014364452070369, -0.5571792354581740492, -0.5439731168496340086, -0.5366754591832860743, -0.4791547776990519036, -0.4217814619618329708, -0.3651803038717780225, -0.3456238285489399154, -0.3024208499803220374, -0.2835195468565521182, -0.2726001362142098650, -0.2628186310418560989, -0.2067675312773959995, -0.1505665958059829723, -0.09476636028567830827, -0.04010237144085015970, 0.000000000000000000 ),
 .UNSPECIFIED. ) ;
#43050 = CARTESIAN_POINT ( 'NONE',  ( 52.99619512781969632, -49.51755756157847799, -27.70008372195887603 ) ) ;
#43051 = CARTESIAN_POINT ( 'NONE',  ( 12.36324357420019915, -64.54680782163349306, -15.76420532458509882 ) ) ;
#43052 = CARTESIAN_POINT ( 'NONE',  ( 59.09889384191680506, -28.80061074846929969, -15.68544870528650037 ) ) ;
#43053 = CARTESIAN_POINT ( 'NONE',  ( 71.26764986431300031, 0.9952464559119579279, -60.54306244337850273 ) ) ;
#43054 = CARTESIAN_POINT ( 'NONE',  ( 11.13393739769619906, 31.90600321400949824, -43.91241836587330027 ) ) ;
#43055 = CARTESIAN_POINT ( 'NONE',  ( 72.42107927723590421, 1.200163167270710041, -61.48893495576489698 ) ) ;
#43056 = CARTESIAN_POINT ( 'NONE',  ( 51.08833026580700221, -35.06325589799279641, -76.45203734832688269 ) ) ;
#43057 = CARTESIAN_POINT ( 'NONE',  ( 65.01767771978660448, 0.8838110553206759423, -70.77727272727270247 ) ) ;
#43058 = ORIENTED_EDGE ( 'NONE', *, *, #20421, .F. ) ;
#43059 = CONICAL_SURFACE ( 'NONE', #37207, 3.506677339277151084, 0.04995839572194331335 ) ;
#43060 = LINE ( 'NONE', #34651, #16193 ) ;
#43061 = CARTESIAN_POINT ( 'NONE',  ( 50.08086529025462141, -1.257411408365102901, -16.00829333108001151 ) ) ;
#43062 = ORIENTED_EDGE ( 'NONE', *, *, #39829, .F. ) ;
#43063 = CARTESIAN_POINT ( 'NONE',  ( 57.12729451229770206, -45.23260415549869862, -25.71705107423920111 ) ) ;
#43064 = CARTESIAN_POINT ( 'NONE',  ( 37.88393739769619373, -15.61618894467929941, -11.65000000000000036 ) ) ;
#43065 = DIRECTION ( 'NONE',  ( 0.7071067811865461294, -0.7071067811865490160, 0.000000000000000000 ) ) ;
#43066 = CARTESIAN_POINT ( 'NONE',  ( 13.88455093916192951, -52.17615671833033275, -75.56421372420085447 ) ) ;
#43067 = ORIENTED_EDGE ( 'NONE', *, *, #42369, .T. ) ;
#43068 = CARTESIAN_POINT ( 'NONE',  ( -0.3016046179078940015, -20.31737465961040101, -35.02873218748179340 ) ) ;
#43069 = CARTESIAN_POINT ( 'NONE',  ( 44.57438173209401810, 6.759042111859073110, -67.44773831433604983 ) ) ;
#43070 = CARTESIAN_POINT ( 'NONE',  ( 8.222956458069184293, -14.58050192852516957, -34.54933503248848581 ) ) ;
#43071 = ORIENTED_EDGE ( 'NONE', *, *, #11184, .T. ) ;
#43072 = CARTESIAN_POINT ( 'NONE',  ( 24.08898506460380062, -13.44825525616480100, -33.70764136182839366 ) ) ;
#43073 = EDGE_CURVE ( 'NONE', #235, #11148, #40844, .T. ) ;
#43074 = CARTESIAN_POINT ( 'NONE',  ( 16.13393739769620083, -15.61618894467929941, 14.34999999999999964 ) ) ;
#43075 = CIRCLE ( 'NONE', #24579, 1.999999999999997335 ) ;
#43076 = CARTESIAN_POINT ( 'NONE',  ( 23.63709980183327275, -18.22008787322180723, -49.89870660227276744 ) ) ;
#43077 = EDGE_CURVE ( 'NONE', #998, #11471, #36912, .T. ) ;
#43078 = CARTESIAN_POINT ( 'NONE',  ( 59.34570819444679302, -28.11291636370129865, -15.68025305306860062 ) ) ;
#43079 = AXIS2_PLACEMENT_3D ( 'NONE', #36699, #24631, #48256 ) ;
#43080 = EDGE_CURVE ( 'NONE', #7773, #6636, #22333, .T. ) ;
#43081 = CARTESIAN_POINT ( 'NONE',  ( -21.36606260230379917, 30.88381105532059934, 16.35000000000000142 ) ) ;
#43082 = CARTESIAN_POINT ( 'NONE',  ( 47.30620416954869967, -54.71667077003900204, -74.17398805956220542 ) ) ;
#43083 = DIRECTION ( 'NONE',  ( -1.000000000000000000, 0.000000000000000000, 0.000000000000000000 ) ) ;
#43084 = EDGE_CURVE ( 'NONE', #43577, #26724, #41108, .T. ) ;
#43085 = CARTESIAN_POINT ( 'NONE',  ( 14.94606681672440018, 21.73127465433789851, -76.14999999999999147 ) ) ;
#43086 = CARTESIAN_POINT ( 'NONE',  ( 83.16755290732228900, -45.00330858143559709, -46.93255211562899376 ) ) ;
#43087 = CARTESIAN_POINT ( 'NONE',  ( 58.78347454168720532, 13.88381119830360078, -25.62280592735929829 ) ) ;
#43088 = CARTESIAN_POINT ( 'NONE',  ( 12.71325777259860068, -22.74941205225429997, -32.14999999999999858 ) ) ;
#43089 = ORIENTED_EDGE ( 'NONE', *, *, #39124, .F. ) ;
#43090 = CYLINDRICAL_SURFACE ( 'NONE', #7159, 1.999999999999997780 ) ;
#43091 = CIRCLE ( 'NONE', #30531, 38.50000000000001421 ) ;
#43092 = CARTESIAN_POINT ( 'NONE',  ( 3.173549631555339978, -55.55485688747910444, -8.896876761822769097 ) ) ;
#43093 = CARTESIAN_POINT ( 'NONE',  ( 75.04668702423900584, -14.04868477427920048, -11.30405884009489981 ) ) ;
#43095 = EDGE_CURVE ( 'NONE', #8693, #998, #50818, .T. ) ;
#43094 = CARTESIAN_POINT ( 'NONE',  ( 75.43567969634317194, 12.70586975596460277, -13.55812906738603019 ) ) ;
#43096 = CARTESIAN_POINT ( 'NONE',  ( 61.13058997637050851, -45.49867003083084427, -47.51052979104920837 ) ) ;
#43097 = CARTESIAN_POINT ( 'NONE',  ( 14.25914812751967098, 1.264432139860236060, -34.81767276520688625 ) ) ;
#43098 = CARTESIAN_POINT ( 'NONE',  ( 14.06331755925441129, -23.32130431222730138, -38.37566614555674249 ) ) ;
#43099 = CARTESIAN_POINT ( 'NONE',  ( 82.53029411324719433, -45.52163144278929963, -47.58593199419160413 ) ) ;
#43100 = CARTESIAN_POINT ( 'NONE',  ( 57.38208912676239493, -50.61190356253609934, -53.76446502280590067 ) ) ;
#43101 = CARTESIAN_POINT ( 'NONE',  ( 40.47914112739019998, 13.57210277531459930, -4.470311448230490647 ) ) ;
#43102 = CARTESIAN_POINT ( 'NONE',  ( 0.6920486002283754434, -37.06681587484604279, -59.64999999999999147 ) ) ;
#43103 = FACE_OUTER_BOUND ( 'NONE', #46759, .T. ) ;
#43104 = CARTESIAN_POINT ( 'NONE',  ( 58.64232589198999790, -46.61555239613360158, -47.49232833693479705 ) ) ;
#43105 = B_SPLINE_CURVE_WITH_KNOTS ( 'NONE', 3,
 ( #48991, #45043, #9143, #37180, #1277, #20147, #31929, #47950, #12052, #28004, #44010, #45561, #45822, #22202, #21941, #30061, #37953, #9658, #38211, #18030, #50273, #46091 ),
 .UNSPECIFIED., .F., .F.,
 ( 4, 2, 1, 1, 1, 2, 2, 2, 2, 1, 1, 1, 2, 4 ),
 ( 0.000000000000000000, 0.1189054937112668242, 0.1783582405669016657, 0.2080846139947190865, 0.2229478007086256597, 0.2303793940655803063, 0.2378109874225349807, 0.3567164811337855679, 0.4161692279894141366, 0.4458956014172286708, 0.4607587881311373534, 0.4681903814880929438, 0.4719061781665709332, 0.4756219748450489226 ),
 .UNSPECIFIED. ) ;
#43106 = LINE ( 'NONE', #26314, #8891 ) ;
#43107 = FACE_OUTER_BOUND ( 'NONE', #20024, .T. ) ;
#43108 = CARTESIAN_POINT ( 'NONE',  ( 17.79388969624029926, -51.62356816798740056, -75.48775473117470369 ) ) ;
#43109 = CARTESIAN_POINT ( 'NONE',  ( 41.23501660619890430, -45.11618894467940066, -6.199054889248789557 ) ) ;
#43110 = CARTESIAN_POINT ( 'NONE',  ( 23.55933089801509794, -15.00772719258320009, -67.04131744907229518 ) ) ;
#43111 = CARTESIAN_POINT ( 'NONE',  ( 63.54731047306190561, 1.396834109478129804, -62.44999999999999574 ) ) ;
#43112 = ORIENTED_EDGE ( 'NONE', *, *, #26461, .T. ) ;
#43113 = CARTESIAN_POINT ( 'NONE',  ( 8.951553309972659633, 31.89301264151889725, -46.63485964089979774 ) ) ;
#43114 = FACE_OUTER_BOUND ( 'NONE', #13236, .T. ) ;
#43115 = CARTESIAN_POINT ( 'NONE',  ( 73.18334309134590399, 0.9940423591679348192, -68.87653036433009390 ) ) ;
#43116 = CARTESIAN_POINT ( 'NONE',  ( 46.09098740009942219, 8.866406348324682440, -56.51717585894476770 ) ) ;
#43117 = EDGE_CURVE ( 'NONE', #9275, #29825, #41565, .T. ) ;
#43118 = CARTESIAN_POINT ( 'NONE',  ( 9.866497443904730602, -18.50142238704479780, -81.23899999999999011 ) ) ;
#43119 = CARTESIAN_POINT ( 'NONE',  ( 44.12335005272829846, -45.59245195477699752, -7.915725708897361379 ) ) ;
#43120 = ORIENTED_EDGE ( 'NONE', *, *, #47820, .T. ) ;
#43121 = CARTESIAN_POINT ( 'NONE',  ( 17.57188048229909683, 20.96156756881190120, -75.93682688742939035 ) ) ;
#43122 = EDGE_LOOP ( 'NONE', ( #49188, #46882, #10225, #25323 ) ) ;
#43123 = EDGE_LOOP ( 'NONE', ( #44910, #18991, #15349 ) ) ;
#43124 = ORIENTED_EDGE ( 'NONE', *, *, #203, .F. ) ;
#43125 = CARTESIAN_POINT ( 'NONE',  ( 28.13393739769620083, -15.61618894467929941, -22.14999999999999858 ) ) ;
#43126 = CARTESIAN_POINT ( 'NONE',  ( 21.53501286420519989, -9.851163535991840803, -81.23899999999999011 ) ) ;
#43127 =( BOUNDED_CURVE ( )  B_SPLINE_CURVE ( 3, ( #36942, #17037, #32989, #41135 ),
 .UNSPECIFIED., .F., .T. ) 
 B_SPLINE_CURVE_WITH_KNOTS ( ( 4, 4 ),
 ( 5.070260775219124660, 5.428132570053652906 ),
 .UNSPECIFIED. ) 
 CURVE ( )  GEOMETRIC_REPRESENTATION_ITEM ( )  RATIONAL_B_SPLINE_CURVE ( ( 1.000000000000000000, 0.9893557610490306686, 0.9893557610490306686, 1.000000000000000000 ) ) 
 REPRESENTATION_ITEM ( '' )  );
#43128 = DIRECTION ( 'NONE',  ( 0.8090169943749472292, -0.5877852522924734702, 0.000000000000000000 ) ) ;
#43129 = ORIENTED_EDGE ( 'NONE', *, *, #39277, .T. ) ;
#43130 = CARTESIAN_POINT ( 'NONE',  ( 9.221408080047158506, -11.63206808030142092, -52.67433566774367648 ) ) ;
#43131 = ORIENTED_EDGE ( 'NONE', *, *, #12013, .F. ) ;
#43132 = CARTESIAN_POINT ( 'NONE',  ( 17.16952344459745561, -7.705194454623752520, -63.33399937649863887 ) ) ;
#43133 = CIRCLE ( 'NONE', #37277, 1.999999999999999778 ) ;
#43134 = LINE ( 'NONE', #23178, #25121 ) ;
#43135 = AXIS2_PLACEMENT_3D ( 'NONE', #47462, #7625, #43271 ) ;
#43136 = ORIENTED_EDGE ( 'NONE', *, *, #13611, .F. ) ;
#43137 = EDGE_CURVE ( 'NONE', #19523, #19102, #21502, .T. ) ;
#43138 = CARTESIAN_POINT ( 'NONE',  ( 8.222924257981070184, -16.27420347773300691, -50.48118173969053402 ) ) ;
#43139 = CARTESIAN_POINT ( 'NONE',  ( 51.41399413552429820, -50.55426312863379934, -76.23672004883859188 ) ) ;
#43140 = CARTESIAN_POINT ( 'NONE',  ( 61.04997942697320212, 14.17778449832839982, -47.26479615961609682 ) ) ;
#43141 = EDGE_CURVE ( 'NONE', #10825, #50973, #50007, .T. ) ;
#43142 = CARTESIAN_POINT ( 'NONE',  ( 20.64627773545588596, -10.50382045408532505, -40.18285380126813067 ) ) ;
#43143 = CARTESIAN_POINT ( 'NONE',  ( -4.878462934014000218, 16.25210934087710157, -5.225023538751180752 ) ) ;
#43144 = CARTESIAN_POINT ( 'NONE',  ( 46.38667134030966110, 21.75602058146941076, -76.14873014702969556 ) ) ;
#43145 = CARTESIAN_POINT ( 'NONE',  ( 16.13393739769620083, -15.61618894467929941, -24.90346750000000142 ) ) ;
#43146 = CARTESIAN_POINT ( 'NONE',  ( 15.96737325713249867, -23.46214360745049632, -53.79426207090799750 ) ) ;
#43147 = VERTEX_POINT ( 'NONE', #13339 ) ;
#43148 = CARTESIAN_POINT ( 'NONE',  ( 56.76664445297700468, -50.67471734267000016, -53.84360320736509919 ) ) ;
#43149 = CARTESIAN_POINT ( 'NONE',  ( 57.47269723223679705, 19.35962728544430078, -53.60395066395300034 ) ) ;
#43150 = UNCERTAINTY_MEASURE_WITH_UNIT (LENGTH_MEASURE( 1.000000000000000082E-05 ), #32260, 'distance_accuracy_value', 'NONE');
#43152 = EDGE_CURVE ( 'NONE', #51582, #9877, #22200, .T. ) ;
#43151 = CARTESIAN_POINT ( 'NONE',  ( 72.00766661773259614, 1.338417587229379979, -70.07245980288250564 ) ) ;
#43153 = CARTESIAN_POINT ( 'NONE',  ( 44.70959683697221720, -40.00980781633823113, -63.22093828018593342 ) ) ;
#43154 = CARTESIAN_POINT ( 'NONE',  ( 15.45245043279679997, 19.57241326031720163, -20.50565891244509942 ) ) ;
#43155 = FILL_AREA_STYLE ('',( #35005 ) ) ;
#43156 = AXIS2_PLACEMENT_3D ( 'NONE', #6093, #14462, #50112 ) ;
#43157 = DIRECTION ( 'NONE',  ( 0.000000000000000000, 0.000000000000000000, -1.000000000000000000 ) ) ;
#43158 = CARTESIAN_POINT ( 'NONE',  ( 48.50471607674010244, -54.16716192014190057, -55.31622937648399585 ) ) ;
#43159 = AXIS2_PLACEMENT_3D ( 'NONE', #47542, #25586, #42840 ) ;
#43160 = CARTESIAN_POINT ( 'NONE',  ( -29.90025726814942431, -36.14282418732561553, -56.90830752171230245 ) ) ;
#43161 = CARTESIAN_POINT ( 'NONE',  ( 63.58805182154581104, 0.9952259095800390920, -69.56719234871339097 ) ) ;
#43162 = CARTESIAN_POINT ( 'NONE',  ( 47.90440150906960071, 23.11714053132569902, -54.72371951289599679 ) ) ;
#43163 = EDGE_LOOP ( 'NONE', ( #21426, #48526, #39412, #28879 ) ) ;
#43164 = CARTESIAN_POINT ( 'NONE',  ( 14.61213889419929934, -8.323009066753440877, -32.50186350533419954 ) ) ;
#43165 = ORIENTED_EDGE ( 'NONE', *, *, #46807, .T. ) ;
#43166 = CARTESIAN_POINT ( 'NONE',  ( 71.35306154470789863, 1.325839985408290067, -70.42711907493250578 ) ) ;
#43167 = CARTESIAN_POINT ( 'NONE',  ( 60.59785292327919848, -45.59099699431040165, -47.16459466356160135 ) ) ;
#43168 = CARTESIAN_POINT ( 'NONE',  ( 48.61347624589590311, -53.95572845601323309, -54.54157758230553554 ) ) ;
#43169 = CARTESIAN_POINT ( 'NONE',  ( 83.09574697852120551, 13.66248986189807901, -46.39646041021766365 ) ) ;
#43171 = DIRECTION ( 'NONE',  ( -1.000000000000000000, 0.000000000000000000, 0.000000000000000000 ) ) ;
#43170 = CARTESIAN_POINT ( 'NONE',  ( 83.49396592876078671, 14.01990206489290003, -47.52773119087509457 ) ) ;
#43172 = EDGE_CURVE ( 'NONE', #9063, #11865, #51645, .T. ) ;
#43173 = CARTESIAN_POINT ( 'NONE',  ( -5.066062602303800233, -15.61618894467930119, -11.54999999999999893 ) ) ;
#43174 = CARTESIAN_POINT ( 'NONE',  ( 23.04647655710144605, -11.63208733966609820, -67.62566283886621932 ) ) ;
#43175 = CARTESIAN_POINT ( 'NONE',  ( 9.205734167420699166, -27.61618894467930119, -24.15000000000000213 ) ) ;
#43176 = ORIENTED_EDGE ( 'NONE', *, *, #8811, .T. ) ;
#43177 = CARTESIAN_POINT ( 'NONE',  ( -0.03447620312152738231, -22.81072779144790275, -34.79644660940672907 ) ) ;
#43178 = ADVANCED_FACE ( 'NONE', ( #14096 ), #1530, .T. ) ;
#43179 = ORIENTED_EDGE ( 'NONE', *, *, #21241, .F. ) ;
#43180 = LINE ( 'NONE', #20077, #28604 ) ;
#43181 = CARTESIAN_POINT ( 'NONE',  ( 56.55522360613520760, 14.97957722649010037, -26.26695323647559732 ) ) ;
#43182 = CARTESIAN_POINT ( 'NONE',  ( 9.367407790820902136, -15.61608574124520032, -61.84717978381009829 ) ) ;
#43183 = CARTESIAN_POINT ( 'NONE',  ( 9.409749845209210761, -63.48355100517809291, -46.51068098438339860 ) ) ;
#43184 = EDGE_LOOP ( 'NONE', ( #1451, #36225, #3270, #32826 ) ) ;
#43185 = VERTEX_POINT ( 'NONE', #9656 ) ;
#43186 = CARTESIAN_POINT ( 'NONE',  ( 24.04476371124131617, -15.67281232776119460, -55.50994974416185102 ) ) ;
#43187 = AXIS2_PLACEMENT_3D ( 'NONE', #15247, #31198, #47228 ) ;
#43188 = CARTESIAN_POINT ( 'NONE',  ( 56.67708563387860465, -45.29633254537559850, -25.29391797581589785 ) ) ;
#43189 = CARTESIAN_POINT ( 'NONE',  ( 56.41160612050880019, -50.71163893462430394, -53.28620048350840221 ) ) ;
#43190 = CARTESIAN_POINT ( 'NONE',  ( 11.97538441063065306, -10.20477936771429839, -35.74448608333058530 ) ) ;
#43191 = CARTESIAN_POINT ( 'NONE',  ( 59.09559851695989607, -2.441367974390179718, -15.68447099303350178 ) ) ;
#43192 = CARTESIAN_POINT ( 'NONE',  ( 51.91394866954649956, -49.47671654292729926, -77.01723411093288973 ) ) ;
#43193 = CARTESIAN_POINT ( 'NONE',  ( -21.36606260230379917, 31.88381105532059934, 16.35000000000000142 ) ) ;
#43194 = ADVANCED_FACE ( 'NONE', ( #41615 ), #49965, .F. ) ;
#43195 = ORIENTED_EDGE ( 'NONE', *, *, #22695, .T. ) ;
#43196 = B_SPLINE_CURVE_WITH_KNOTS ( 'NONE', 3,
 ( #2337, #18311, #13877, #5756, #2083, #13371, #1563, #37726, #46384, #49785, #41392, #21714, #25135, #50039, #5508, #29837 ),
 .UNSPECIFIED., .F., .F.,
 ( 4, 2, 2, 2, 2, 2, 2, 4 ),
 ( 0.000000000000000000, 0.2171919328280763339, 0.4113453696724681530, 0.5484604928966247961, 0.6170180545087031732, 0.7267101530880277771, 0.9022175108149470546, 1.000000000000000000 ),
 .UNSPECIFIED. ) ;
#43197 = CARTESIAN_POINT ( 'NONE',  ( 9.366647546311250849, -15.61604444486649967, -65.84717978381009118 ) ) ;
#43198 = CARTESIAN_POINT ( 'NONE',  ( 22.90017504350882760, -16.53861086495556165, -50.89058099898073806 ) ) ;
#43199 = DIRECTION ( 'NONE',  ( -0.3502816565540492477, 0.000000000000000000, 0.9366444154970182678 ) ) ;
#43200 = CARTESIAN_POINT ( 'NONE',  ( 15.09846568087331775, -23.52719809933467587, -54.04933655904326173 ) ) ;
#43201 = CIRCLE ( 'NONE', #47396, 1.000000000000000888 ) ;
#43202 = EDGE_CURVE ( 'NONE', #5111, #23033, #21939, .T. ) ;
#43203 = CARTESIAN_POINT ( 'NONE',  ( 23.90878591523479813, -14.54919404267139882, -45.96908178614960150 ) ) ;
#43204 = B_SPLINE_CURVE_WITH_KNOTS ( 'NONE', 3,
 ( #38395, #14030, #1975, #38922, #50196, #3014, #10102, #34447, #14806, #25793, #50963, #34966, #46793, #30255, #2494, #26848 ),
 .UNSPECIFIED., .F., .F.,
 ( 4, 2, 2, 2, 2, 2, 2, 4 ),
 ( 12.41746251024190073, 14.15001006772948955, 23.85327782795553730, 28.70491170806860382, 32.58621881215907479, 36.46752591624945694, 42.67761728279422329, 46.65082938388610501 ),
 .UNSPECIFIED. ) ;
#43205 = VECTOR ( 'NONE', #7198, 1000.000000000000114 ) ;
#43206 = CARTESIAN_POINT ( 'NONE',  ( 13.02865871864519853, -50.32049581721639697, -21.18330777480309735 ) ) ;
#43207 = CARTESIAN_POINT ( 'NONE',  ( 14.13393739769619906, -37.52509124488599923, -54.64999999999999858 ) ) ;
#43208 = CARTESIAN_POINT ( 'NONE',  ( 56.54446371377569847, 13.89738154011810067, -15.75405245971630031 ) ) ;
#43209 = CARTESIAN_POINT ( 'NONE',  ( 61.05628860138500613, -45.35080969805910200, -46.88525996552779418 ) ) ;
#43210 = CARTESIAN_POINT ( 'NONE',  ( 56.45963719500250022, -50.66310011266489255, -53.16982888481129521 ) ) ;
#43211 = CARTESIAN_POINT ( 'NONE',  ( 18.21162691092170149, -8.876325039444729725, -48.44236253966159467 ) ) ;
#43212 = CARTESIAN_POINT ( 'NONE',  ( 17.01967013855468380, -8.849179591706896275, -43.99445488068004551 ) ) ;
#43213 = ORIENTED_EDGE ( 'NONE', *, *, #1370, .T. ) ;
#43214 = CARTESIAN_POINT ( 'NONE',  ( 14.35463486013270007, -51.14554741935889837, -74.54427505470819426 ) ) ;
#43215 = CARTESIAN_POINT ( 'NONE',  ( 64.84946247134770658, 1.186701509386330011, -60.73797667709650483 ) ) ;
#43216 = CARTESIAN_POINT ( 'NONE',  ( 3.277530937145240131, -5.884138137110399569, -34.64999999999999858 ) ) ;
#43217 = FACE_OUTER_BOUND ( 'NONE', #28404, .T. ) ;
#43218 = CARTESIAN_POINT ( 'NONE',  ( 22.21935039506094967, 22.72579217771971827, -34.76477869314942382 ) ) ;
#43219 = CARTESIAN_POINT ( 'NONE',  ( 9.807838715921571193, -10.75442553347946451, -46.71600211399567826 ) ) ;
#43220 = CIRCLE ( 'NONE', #1356, 2.999999999999999112 ) ;
#43221 = CARTESIAN_POINT ( 'NONE',  ( 10.81643727139639921, -64.95351341576260040, -17.63284883035869655 ) ) ;
#43222 = AXIS2_PLACEMENT_3D ( 'NONE', #47940, #43998, #4161 ) ;
#43223 = CARTESIAN_POINT ( 'NONE',  ( 82.13853704237929776, 14.30143299382709898, -47.59887875144359981 ) ) ;
#43224 = CARTESIAN_POINT ( 'NONE',  ( 63.66068354842749244, 0.9098571636355720083, -68.84999999999999432 ) ) ;
#43226 = CARTESIAN_POINT ( 'NONE',  ( 11.50961124680121728, 33.46337070016348747, -23.96126768911706861 ) ) ;
#43225 = CARTESIAN_POINT ( 'NONE',  ( 16.13393739769620083, -15.61618894467929941, -28.45282021618999835 ) ) ;
#43227 = CARTESIAN_POINT ( 'NONE',  ( 13.09030777569590676, -22.94849230994849520, -32.41764226196748666 ) ) ;
#43228 = CARTESIAN_POINT ( 'NONE',  ( 49.48559182206740559, 22.51696836342139818, -55.18124709514480486 ) ) ;
#43229 = EDGE_LOOP ( 'NONE', ( #11091, #40397, #13273, #12633 ) ) ;
#43230 = CARTESIAN_POINT ( 'NONE',  ( 52.80437713202650230, -49.69361475838819331, -48.85649632429790046 ) ) ;
#43231 = ORIENTED_EDGE ( 'NONE', *, *, #3266, .T. ) ;
#43232 = CARTESIAN_POINT ( 'NONE',  ( 45.14469185402641926, 7.879481261360513855, -65.05625649667543087 ) ) ;
#43233 = CIRCLE ( 'NONE', #524, 16.33504667647529729 ) ;
#43234 = DIRECTION ( 'NONE',  ( 0.05355673475992397264, -0.9985648081931662867, 0.000000000000000000 ) ) ;
#43235 = CARTESIAN_POINT ( 'NONE',  ( 14.13996207071689959, 19.81020116829009936, -21.96868406873839774 ) ) ;
#43236 = CARTESIAN_POINT ( 'NONE',  ( 51.85719039531000618, -49.29163377067489904, -77.06876493040969933 ) ) ;
#43237 = EDGE_CURVE ( 'NONE', #28919, #39247, #48278, .T. ) ;
#43238 = CARTESIAN_POINT ( 'NONE',  ( 21.35923182362840222, -20.35315599744080117, -50.68722986888699467 ) ) ;
#43239 = CARTESIAN_POINT ( 'NONE',  ( 52.72599990135299919, 18.50994649268380243, -48.79685834802910449 ) ) ;
#43240 = CARTESIAN_POINT ( 'NONE',  ( 55.76563889033010213, -45.58887186001610559, -16.42694171794889968 ) ) ;
#43241 = CARTESIAN_POINT ( 'NONE',  ( 55.63848436370909667, 15.03490499964270022, -25.39977966304109813 ) ) ;
#43242 = CIRCLE ( 'NONE', #28999, 0.5000000000000004441 ) ;
#43243 = EDGE_CURVE ( 'NONE', #22490, #28125, #1321, .T. ) ;
#43244 = ORIENTED_EDGE ( 'NONE', *, *, #2728, .F. ) ;
#43245 = CARTESIAN_POINT ( 'NONE',  ( 10.00581152974459798, -19.85325857441549857, -79.87478428137869457 ) ) ;
#43246 = B_SPLINE_CURVE_WITH_KNOTS ( 'NONE', 3,
 ( #7578, #48896, #3390, #27730, #43980, #19097, #44951, #24031, #11249, #40053, #36820, #4856, #47418, #35338, #12997, #9051, #27211, #3643, #15438, #51078 ),
 .UNSPECIFIED., .F., .F.,
 ( 4, 2, 2, 2, 2, 2, 2, 2, 2, 4 ),
 ( -1.826192301619919967, -1.710015269441619967, -1.458000257336709904, -1.209852399823200031, -1.027233169661200041, -0.9130961508099589841, -0.6848221131074689882, -0.4130753771317612344, -0.1614840352128998902, 0.000000000000000000 ),
 .UNSPECIFIED. ) ;
#43247 = ORIENTED_EDGE ( 'NONE', *, *, #40678, .T. ) ;
#43248 = ADVANCED_FACE ( 'NONE', ( #2832 ), #7311, .T. ) ;
#43249 = CARTESIAN_POINT ( 'NONE',  ( 11.51020352941140068, -65.19111653312340593, -17.03655004557180064 ) ) ;
#43250 = CARTESIAN_POINT ( 'NONE',  ( 11.55432588269150074, 33.99546521010679356, -47.20121379407340356 ) ) ;
#43251 = CARTESIAN_POINT ( 'NONE',  ( 73.09245838956729813, 1.096153228089730147, -62.34242842016499964 ) ) ;
#43252 = CARTESIAN_POINT ( 'NONE',  ( 8.428791536887311864, -17.68670186955939272, -40.70900208874113702 ) ) ;
#43253 = DIRECTION ( 'NONE',  ( 0.8090169943749478954, 0.5877852522924724710, 0.000000000000000000 ) ) ;
#43254 = CARTESIAN_POINT ( 'NONE',  ( 0.5716597375277996385, -15.61618894467929941, -6.649999999999999467 ) ) ;
#43255 = CARTESIAN_POINT ( 'NONE',  ( 51.19787128922300212, -52.90300504561889738, -54.04781962224119951 ) ) ;
#43256 = ORIENTED_EDGE ( 'NONE', *, *, #10774, .T. ) ;
#43257 = DIRECTION ( 'NONE',  ( 0.000000000000000000, 0.000000000000000000, -1.000000000000000000 ) ) ;
#43258 = CARTESIAN_POINT ( 'NONE',  ( 10.14147138814020010, -63.21765883073391024, -45.99379265408919792 ) ) ;
#43259 = FACE_OUTER_BOUND ( 'NONE', #33511, .T. ) ;
#43260 = ORIENTED_EDGE ( 'NONE', *, *, #42774, .T. ) ;
#43261 = CARTESIAN_POINT ( 'NONE',  ( 68.38970072013677282, -30.34057458802632823, -18.15384971058606922 ) ) ;
#43262 = CARTESIAN_POINT ( 'NONE',  ( 56.91872540556310156, 19.41123227373739724, -53.86107397134590258 ) ) ;
#43263 = DIRECTION ( 'NONE',  ( 0.000000000000000000, 0.000000000000000000, 1.000000000000000000 ) ) ;
#43264 = EDGE_LOOP ( 'NONE', ( #17052, #26791, #37181, #38390 ) ) ;
#43265 = CARTESIAN_POINT ( 'NONE',  ( 52.20740535868762322, 20.17246182719578584, -75.93239680710105688 ) ) ;
#43266 = CARTESIAN_POINT ( 'NONE',  ( 11.27985751389227609, -20.39062183032262254, -33.20531548096091967 ) ) ;
#43267 = CARTESIAN_POINT ( 'NONE',  ( 57.32828653034319899, -50.41406207962300812, -53.00038473087199975 ) ) ;
#43268 = EDGE_CURVE ( 'NONE', #30849, #32691, #37768, .T. ) ;
#43269 = CARTESIAN_POINT ( 'NONE',  ( 14.70217909044999871, -7.496288193711560410, -65.23677592514890478 ) ) ;
#43270 = CARTESIAN_POINT ( 'NONE',  ( 63.02123093760216221, 0.4193442080440759612, -17.11446765124405900 ) ) ;
#43271 = DIRECTION ( 'NONE',  ( 1.000000000000000000, 2.460964292799963328E-14, 0.000000000000000000 ) ) ;
#43272 = DIRECTION ( 'NONE',  ( 0.000000000000000000, 0.000000000000000000, 1.000000000000000000 ) ) ;
#43273 = ORIENTED_EDGE ( 'NONE', *, *, #15367, .F. ) ;
#43274 = ORIENTED_EDGE ( 'NONE', *, *, #18506, .F. ) ;
#43275 = CARTESIAN_POINT ( 'NONE',  ( -22.73277434335082603, -12.47272083566619649, -54.68865740790490548 ) ) ;
#43276 = CARTESIAN_POINT ( 'NONE',  ( 9.313614695934589349, -18.61450381289790101, -51.10081841474490005 ) ) ;
#43277 = AXIS2_PLACEMENT_3D ( 'NONE', #40332, #20144, #48719 ) ;
#43278 = CARTESIAN_POINT ( 'NONE',  ( 50.77828552747439517, -50.74762180099740050, -76.14999999999999147 ) ) ;
#43279 = CARTESIAN_POINT ( 'NONE',  ( 16.13393739769620083, -15.61618894467929941, -35.14999999999999858 ) ) ;
#43280 = CARTESIAN_POINT ( 'NONE',  ( 46.76524959757980326, 22.46046862905859598, -75.96071349691810326 ) ) ;
#43281 = CARTESIAN_POINT ( 'NONE',  ( 50.03007040746459921, 17.38381105532069881, -78.14999999999999147 ) ) ;
#43282 = FACE_OUTER_BOUND ( 'NONE', #34869, .T. ) ;
#43283 = CARTESIAN_POINT ( 'NONE',  ( 42.39660149645209941, -44.97461146731200898, -5.990492802273720940 ) ) ;
#43284 = CARTESIAN_POINT ( 'NONE',  ( 12.00693377043790022, 33.56613978031089118, -16.09314495738659900 ) ) ;
#43285 = CARTESIAN_POINT ( 'NONE',  ( 24.33302514535889927, -16.48663757332040092, -69.54133546202839966 ) ) ;
#43286 = CARTESIAN_POINT ( 'NONE',  ( 55.91596500572619277, -45.90464019914170279, -25.32542830939949852 ) ) ;
#43287 = CIRCLE ( 'NONE', #1421, 7.599999999999996092 ) ;
#43288 = CARTESIAN_POINT ( 'NONE',  ( 55.34927123575489816, -50.61618894660580281, -76.48225957491609961 ) ) ;
#43290 = CARTESIAN_POINT ( 'NONE',  ( 31.59596111684529518, -35.98598576688283401, -84.65000000000001990 ) ) ;
#43289 = CARTESIAN_POINT ( 'NONE',  ( -6.318914795328239187, 14.68237235522740036, -4.813384506477039970 ) ) ;
#43291 = CARTESIAN_POINT ( 'NONE',  ( 24.04516176800591865, -15.61618872104648226, -63.79232972929064971 ) ) ;
#43292 = DIRECTION ( 'NONE',  ( -0.8320502943378438321, 0.000000000000000000, 0.5547001962252288143 ) ) ;
#43293 = ORIENTED_EDGE ( 'NONE', *, *, #8678, .F. ) ;
#43294 = DIRECTION ( 'NONE',  ( -0.9200120562340502461, 0.3918900565005380976, 0.000000000000000000 ) ) ;
#43295 = CARTESIAN_POINT ( 'NONE',  ( 47.74202631360270033, 23.20359536699950098, -54.70726247055279856 ) ) ;
#43296 = CARTESIAN_POINT ( 'NONE',  ( 60.02121333775870227, -45.19777382224889806, -26.54063133662459961 ) ) ;
#43297 = CARTESIAN_POINT ( 'NONE',  ( 16.15069521921704165, -51.05177107958204630, -15.66900421577824254 ) ) ;
#43298 = CARTESIAN_POINT ( 'NONE',  ( 13.22845487704439904, 19.37063177541839920, -21.36464768999449859 ) ) ;
#43299 = CARTESIAN_POINT ( 'NONE',  ( 61.02913797987469735, 14.29490916149900137, -47.53473330658249552 ) ) ;
#43300 = CARTESIAN_POINT ( 'NONE',  ( 22.19445665721740113, -19.94940946873740018, -70.43023759426799302 ) ) ;
#43301 = CARTESIAN_POINT ( 'NONE',  ( 51.29313473418520175, 18.26623787800760113, -76.46030551589480240 ) ) ;
#43302 = CARTESIAN_POINT ( 'NONE',  ( 52.96420269150630844, 18.35810234167090016, -48.77461993677670193 ) ) ;
#43303 = DIRECTION ( 'NONE',  ( 8.462868000000000073E-18, -1.066343000000000058E-17, 1.000000000000000000 ) ) ;
#43304 = EDGE_CURVE ( 'NONE', #23386, #26529, #19320, .T. ) ;
#43305 = CARTESIAN_POINT ( 'NONE',  ( 50.11664719554170944, 5.483622036391903265, -76.15000000000003411 ) ) ;
#43306 = CARTESIAN_POINT ( 'NONE',  ( 23.98964259220293371, -16.68387156175795383, -61.55060845666147884 ) ) ;
#43307 = CARTESIAN_POINT ( 'NONE',  ( 20.99560800870527899, -9.290017777483981831, -37.50066705834722569 ) ) ;
#43308 = CARTESIAN_POINT ( 'NONE',  ( 71.33393739769628894, 1.383811055320669947, -61.44999999999999574 ) ) ;
#43309 = CARTESIAN_POINT ( 'NONE',  ( 64.35623192390551139, -32.08291323696330011, -17.59133921123940070 ) ) ;
#43310 = CARTESIAN_POINT ( 'NONE',  ( 71.13601697155240799, 1.385888765344509999, -60.99577487439199786 ) ) ;
#43311 = CARTESIAN_POINT ( 'NONE',  ( -18.86606260230360022, -50.61618894467959962, 11.34999999999999964 ) ) ;
#43312 = CARTESIAN_POINT ( 'NONE',  ( 72.17449546179830122, 1.458407608744489936, -61.54081785568290286 ) ) ;
#43313 = CARTESIAN_POINT ( 'NONE',  ( 20.15227385440210028, -21.41235416792470048, -41.15422088180869054 ) ) ;
#43314 = CARTESIAN_POINT ( 'NONE',  ( 61.12526931739070335, -45.25414475714967466, -27.63398140488572352 ) ) ;
#43315 = VERTEX_POINT ( 'NONE', #42924 ) ;
#43316 = ORIENTED_EDGE ( 'NONE', *, *, #50815, .F. ) ;
#43317 = CARTESIAN_POINT ( 'NONE',  ( 10.16236763787109432, -19.36890979467511187, -37.66858791500941805 ) ) ;
#43318 = CARTESIAN_POINT ( 'NONE',  ( 49.91571640700792756, -29.72640275947340172, -15.91623881425632447 ) ) ;
#43319 = ORIENTED_EDGE ( 'NONE', *, *, #31076, .T. ) ;
#43320 = CARTESIAN_POINT ( 'NONE',  ( 56.23014233047970123, -45.81748423697870010, -25.89964805919260016 ) ) ;
#43321 = CARTESIAN_POINT ( 'NONE',  ( 0.9261640637176550284, -8.686430247967809493, -34.65800258959620095 ) ) ;
#43322 = LINE ( 'NONE', #18424, #28132 ) ;
#43323 = VERTEX_POINT ( 'NONE', #3859 ) ;
#43324 = CARTESIAN_POINT ( 'NONE',  ( 16.13393739769620083, -15.61618894467929941, -5.740514720465080600 ) ) ;
#43325 = CARTESIAN_POINT ( 'NONE',  ( 42.99776018868912075, 6.545124476837784755, -75.33088594088501111 ) ) ;
#43326 = CARTESIAN_POINT ( 'NONE',  ( 41.99203386431830154, -44.88537213046480190, -5.712673480947970006 ) ) ;
#43327 = ORIENTED_EDGE ( 'NONE', *, *, #51008, .T. ) ;
#43328 = EDGE_CURVE ( 'NONE', #39742, #37859, #20742, .T. ) ;
#43329 = CARTESIAN_POINT ( 'NONE',  ( 50.44516630538529967, -45.11618894467940066, -10.60027150187420020 ) ) ;
#43330 = CARTESIAN_POINT ( 'NONE',  ( 51.88785155891503109, 1.541422455399617419, -18.83071984855998338 ) ) ;
#43331 = CARTESIAN_POINT ( 'NONE',  ( 13.22332444824007780, -22.99680140878987444, -50.41190558083048501 ) ) ;
#43332 = EDGE_CURVE ( 'NONE', #29113, #3072, #17371, .T. ) ;
#43333 = CARTESIAN_POINT ( 'NONE',  ( 60.21673368439580543, -28.82193623653779824, -15.80468577411680009 ) ) ;
#43334 = CARTESIAN_POINT ( 'NONE',  ( 20.29259151353744883, -10.20485656652930118, -64.16115512084347472 ) ) ;
#43335 = CARTESIAN_POINT ( 'NONE',  ( 47.30620416954869967, -54.71667077003900204, -74.14999999999999147 ) ) ;
#43336 = CARTESIAN_POINT ( 'NONE',  ( 23.60639345834430358, -18.01392704823980040, -72.11132903714400300 ) ) ;
#43337 = FACE_OUTER_BOUND ( 'NONE', #4469, .T. ) ;
#43338 = CARTESIAN_POINT ( 'NONE',  ( 43.92206853057700044, 14.74641057201809957, -8.176270959481939826 ) ) ;
#43339 = B_SPLINE_CURVE_WITH_KNOTS ( 'NONE', 3,
 ( #13380, #29340, #13634, #45597, #46128, #41142, #45342, #50312, #9447, #41397, #37993, #49542, #5515, #49283, #50045, #14138 ),
 .UNSPECIFIED., .F., .F.,
 ( 4, 2, 2, 2, 2, 2, 2, 4 ),
 ( -4.551914000000000309E-15, 0.07319275283555799760, 0.1391693187718399949, 0.1804046724820149994, 0.2061767685508749948, 0.2577209606885960125, 0.3401916681089480199, 0.4123535371017559847 ),
 .UNSPECIFIED. ) ;
#43340 = DIRECTION ( 'NONE',  ( -1.000000000000000000, 0.000000000000000000, 0.000000000000000000 ) ) ;
#43341 = CARTESIAN_POINT ( 'NONE',  ( 84.17895764879889953, -44.08298806148399507, -47.20739533566359825 ) ) ;
#43342 = AXIS2_PLACEMENT_3D ( 'NONE', #32318, #20533, #8765 ) ;
#43343 = CARTESIAN_POINT ( 'NONE',  ( 57.48924594623639450, 13.88381125482189837, -25.32904884043690075 ) ) ;
#43344 = CARTESIAN_POINT ( 'NONE',  ( 20.08350565795849718, -22.39760913111329899, -79.61963359764799009 ) ) ;
#43345 = VERTEX_POINT ( 'NONE', #51552 ) ;
#43346 = DIRECTION ( 'NONE',  ( 0.000000000000000000, -0.7071067811865492381, -0.7071067811865457964 ) ) ;
#43347 = CARTESIAN_POINT ( 'NONE',  ( 6.660026050685900145, -59.99599272703940045, -12.48570139134749901 ) ) ;
#43348 = CARTESIAN_POINT ( 'NONE',  ( 76.33997785262350533, -14.06269230294210004, -12.53642027154039873 ) ) ;
#43349 = CIRCLE ( 'NONE', #2335, 28.31678667024650409 ) ;
#43350 = CARTESIAN_POINT ( 'NONE',  ( 75.29505756514645043, 13.38913129781163391, -14.04565979207876936 ) ) ;
#43351 = CARTESIAN_POINT ( 'NONE',  ( 2.419685150592632006, -5.395387223103724317, -35.06583844469683697 ) ) ;
#43352 = CARTESIAN_POINT ( 'NONE',  ( -30.36606260230379917, -53.11618894467940066, 16.35000000000000142 ) ) ;
#43353 = CARTESIAN_POINT ( 'NONE',  ( 20.99564373225254599, -21.94233159712619852, -38.08400039168056850 ) ) ;
#43354 = CARTESIAN_POINT ( 'NONE',  ( 7.492845759203720313, 29.94784237631284896, -20.13893727953968948 ) ) ;
#43355 = CARTESIAN_POINT ( 'NONE',  ( 82.71798245299019925, -45.49268626692509798, -47.55440761962790219 ) ) ;
#43356 = CARTESIAN_POINT ( 'NONE',  ( 57.39790738242900403, -50.56072618960909892, -53.44821462976450732 ) ) ;
#43357 = CARTESIAN_POINT ( 'NONE',  ( 42.42327895389549752, 12.56836077726920031, -4.706996716866660435 ) ) ;
#43358 = LINE ( 'NONE', #23149, #36772 ) ;
#43359 = CARTESIAN_POINT ( 'NONE',  ( 63.86181505067941089, 1.033004162168289941, -61.43684260791479801 ) ) ;
#43360 = CARTESIAN_POINT ( 'NONE',  ( 16.13393739769620083, -15.61618894467929941, 5.856814007409659517 ) ) ;
#43361 = CARTESIAN_POINT ( 'NONE',  ( 70.83393739769717001, -48.11618894467422081, -70.54999999999975557 ) ) ;
#43362 = EDGE_CURVE ( 'NONE', #39834, #30210, #11508, .T. ) ;
#43363 = CARTESIAN_POINT ( 'NONE',  ( 66.98669698734040878, -1.154848256152869901, -17.21849850612139576 ) ) ;
#43364 = CARTESIAN_POINT ( 'NONE',  ( 17.73938417335649831, -51.76348103900169662, -75.62474771911479365 ) ) ;
#43365 = CARTESIAN_POINT ( 'NONE',  ( 53.57599294125679990, -43.78057387862440208, -7.454646995071700033 ) ) ;
#43366 = CARTESIAN_POINT ( 'NONE',  ( 22.52917233249549867, -19.43818638934929766, -63.23880875801850010 ) ) ;
#43367 = CARTESIAN_POINT ( 'NONE',  ( 17.16957802224845864, -7.705202244497520780, -41.04933447065145202 ) ) ;
#43368 = CARTESIAN_POINT ( 'NONE',  ( 63.35923387292240250, 1.230946250268760034, -62.19265059571660004 ) ) ;
#43369 = ORIENTED_EDGE ( 'NONE', *, *, #39154, .F. ) ;
#43370 = CARTESIAN_POINT ( 'NONE',  ( 59.49262858449159808, 17.38381105532069881, -53.92796738110899923 ) ) ;
#43371 = CARTESIAN_POINT ( 'NONE',  ( 22.89996330215964804, -15.74029339777422543, -34.45865469882935628 ) ) ;
#43372 = CARTESIAN_POINT ( 'NONE',  ( 72.82137280411760116, 1.383928098097870096, -68.54761322559109260 ) ) ;
#43373 = CARTESIAN_POINT ( 'NONE',  ( 10.72266900401992196, -11.45745232604984842, -73.66115355198333248 ) ) ;
#43374 = CARTESIAN_POINT ( 'NONE',  ( 11.78849808412049960, -9.293787752828999160, -81.23899999999999011 ) ) ;
#43375 = ORIENTED_EDGE ( 'NONE', *, *, #35434, .T. ) ;
#43376 = CARTESIAN_POINT ( 'NONE',  ( 17.79805963255870083, 20.61263520652270032, -75.69337827730609547 ) ) ;
#43377 = ORIENTED_EDGE ( 'NONE', *, *, #15289, .F. ) ;
#43378 = VERTEX_POINT ( 'NONE', #38994 ) ;
#43379 = LINE ( 'NONE', #15074, #14330 ) ;
#43380 = CARTESIAN_POINT ( 'NONE',  ( 22.56774556973750023, -11.25265918193379910, -81.23899999999999011 ) ) ;
#43381 = CARTESIAN_POINT ( 'NONE',  ( 18.20469914615897977, -7.911112079811677411, -73.37566484845835646 ) ) ;
#43382 = AXIS2_PLACEMENT_3D ( 'NONE', #13107, #36395, #49257 ) ;
#43383 = VERTEX_POINT ( 'NONE', #27430 ) ;
#43384 = CARTESIAN_POINT ( 'NONE',  ( 13.46657045245495432, -9.346956680139966167, -79.82493874763157748 ) ) ;
#43385 = ORIENTED_EDGE ( 'NONE', *, *, #16968, .F. ) ;
#43386 = FACE_OUTER_BOUND ( 'NONE', #38564, .T. ) ;
#43387 = EDGE_CURVE ( 'NONE', #31052, #32053, #12359, .T. ) ;
#43388 = CARTESIAN_POINT ( 'NONE',  ( 10.47406283454438203, -63.11543068638779630, -45.62066736167659542 ) ) ;
#43389 = ORIENTED_EDGE ( 'NONE', *, *, #25958, .T. ) ;
#43390 = CARTESIAN_POINT ( 'NONE',  ( 72.80768847294999091, 1.384447124000270035, -62.70866005236110396 ) ) ;
#43391 = CARTESIAN_POINT ( 'NONE',  ( 51.02815224764380275, -50.88300054698879649, -76.14999943445839392 ) ) ;
#43392 = CARTESIAN_POINT ( 'NONE',  ( 60.96828345175140385, 14.29541988433120103, -47.49580120907970127 ) ) ;
#43393 = CARTESIAN_POINT ( 'NONE',  ( 19.96336983191040559, -9.970646423659596636, -40.14281403636497458 ) ) ;
#43394 = CARTESIAN_POINT ( 'NONE',  ( 40.53658481618179366, -44.74595000644689691, -4.211756420469699336 ) ) ;
#43395 = CARTESIAN_POINT ( 'NONE',  ( -10.89069801029419970, 11.10586477277349893, -6.229949705787969805 ) ) ;
#43396 = CARTESIAN_POINT ( 'NONE',  ( 47.11356721804862246, 23.41744796771036263, -74.95177798119966894 ) ) ;
#43397 = CARTESIAN_POINT ( 'NONE',  ( 9.366395830200795913, -16.73520444579738253, -43.79452874782144534 ) ) ;
#43398 = CARTESIAN_POINT ( 'NONE',  ( 17.51060849981909939, -7.890159896082458602, -52.84363489814449366 ) ) ;
#43399 = VERTEX_POINT ( 'NONE', #19575 ) ;
#43400 = CYLINDRICAL_SURFACE ( 'NONE', #15456, 7.910999999999997812 ) ;
#43401 = CARTESIAN_POINT ( 'NONE',  ( 44.39988805235839919, 14.85962372618369898, -8.567279085052819099 ) ) ;
#43402 = CARTESIAN_POINT ( 'NONE',  ( 71.76028641513160267, 1.321111291667659948, -70.24077000692989259 ) ) ;
#43403 = CARTESIAN_POINT ( 'NONE',  ( 44.78235668084641219, -40.01503934400871287, -62.86839404953338573 ) ) ;
#43404 = CARTESIAN_POINT ( 'NONE',  ( 13.75381683890269890, 19.05415068650080102, -20.97887788433579814 ) ) ;
#43405 = CARTESIAN_POINT ( 'NONE',  ( 16.13393739769620083, -15.61618894467929941, 14.62639320225000006 ) ) ;
#43406 = CARTESIAN_POINT ( 'NONE',  ( 12.69621343537160207, 18.74918025219870188, -21.09935757674490020 ) ) ;
#43407 = VECTOR ( 'NONE', #26988, 1000.000000000000000 ) ;
#43408 = CARTESIAN_POINT ( 'NONE',  ( 63.25162284297759641, 1.007912009470870229, -69.12629645913949616 ) ) ;
#43409 = CARTESIAN_POINT ( 'NONE',  ( 48.80641172512370218, -53.96751462272040101, -54.78053361341569882 ) ) ;
#43410 = CARTESIAN_POINT ( 'NONE',  ( 24.04486360762935604, -15.57925695708305014, -45.50619014287734387 ) ) ;
#43411 = ADVANCED_FACE ( 'NONE', ( #11211 ), #24028, .F. ) ;
#43412 = CYLINDRICAL_SURFACE ( 'NONE', #34245, 7.910999999999997812 ) ;
#43413 = CARTESIAN_POINT ( 'NONE',  ( 15.09847269682518878, -23.52719894729639449, -38.04933652063846239 ) ) ;
#43414 = CARTESIAN_POINT ( 'NONE',  ( 47.77489297752619990, 23.22910854708220185, -54.94508266598730017 ) ) ;
#43415 = VERTEX_POINT ( 'NONE', #38735 ) ;
#43416 = CARTESIAN_POINT ( 'NONE',  ( 9.825858312949119266, -19.58038275917900251, -37.88875081766039443 ) ) ;
#43417 =( BOUNDED_CURVE ( )  B_SPLINE_CURVE ( 3, ( #47859, #32604, #28949, #16645 ),
 .UNSPECIFIED., .F., .T. ) 
 B_SPLINE_CURVE_WITH_KNOTS ( ( 4, 4 ),
 ( 3.141592653589793116, 3.487830450619280320 ),
 .UNSPECIFIED. ) 
 CURVE ( )  GEOMETRIC_REPRESENTATION_ITEM ( )  RATIONAL_B_SPLINE_CURVE ( ( 1.000000000000000000, 0.9900348743600094759, 0.9900348743600094759, 1.000000000000000000 ) ) 
 REPRESENTATION_ITEM ( '' )  );
#43418 = EDGE_CURVE ( 'NONE', #38586, #20094, #2774, .T. ) ;
#43419 = ORIENTED_EDGE ( 'NONE', *, *, #38896, .T. ) ;
#43420 = CARTESIAN_POINT ( 'NONE',  ( 71.42907483962369497, 1.326134026835569912, -70.39062084647959239 ) ) ;
#43421 = CARTESIAN_POINT ( 'NONE',  ( 60.47410467199969730, -45.68409708816510317, -47.42171235821720643 ) ) ;
#43422 = CARTESIAN_POINT ( 'NONE',  ( 58.64232589199010448, -46.61555239613360158, -47.49232833693479705 ) ) ;
#43423 = CARTESIAN_POINT ( 'NONE',  ( 10.47406283454438203, 8.337936262032100032, -45.62066736167659542 ) ) ;
#43425 = CARTESIAN_POINT ( 'NONE',  ( 14.63183004845009982, 0.9274771370715009233, -34.65000333055159842 ) ) ;
#43424 = CARTESIAN_POINT ( 'NONE',  ( 83.07525583555450055, 14.27202569750270023, -47.60489434516649965 ) ) ;
#43426 = EDGE_CURVE ( 'NONE', #17470, #10051, #34026, .T. ) ;
#43427 = CARTESIAN_POINT ( 'NONE',  ( 5.741632552282950108, -21.61618894467929763, -22.14999999999999858 ) ) ;
#43428 = CARTESIAN_POINT ( 'NONE',  ( 68.13393739769620083, -43.11618894467930119, -65.65000000000000568 ) ) ;
#43429 = ORIENTED_EDGE ( 'NONE', *, *, #22003, .F. ) ;
#43430 = CARTESIAN_POINT ( 'NONE',  ( -0.4410626023037970689, -22.87636857973879856, -35.14999999999999858 ) ) ;
#43431 = VERTEX_POINT ( 'NONE', #44714 ) ;
#43432 = VERTEX_POINT ( 'NONE', #16948 ) ;
#43433 = DIRECTION ( 'NONE',  ( 1.000000000000000000, 2.460964292799963328E-14, 0.000000000000000000 ) ) ;
#43434 = CARTESIAN_POINT ( 'NONE',  ( 76.50875310644418903, -28.83273956145659156, -13.26513667399496832 ) ) ;
#43435 = CARTESIAN_POINT ( 'NONE',  ( 11.75059328717480156, -65.32411396726729436, -47.38109070371250908 ) ) ;
#43436 = EDGE_CURVE ( 'NONE', #36534, #41357, #40784, .T. ) ;
#43437 = ORIENTED_EDGE ( 'NONE', *, *, #37388, .T. ) ;
#43438 = ORIENTED_EDGE ( 'NONE', *, *, #49883, .T. ) ;
#43439 = CARTESIAN_POINT ( 'NONE',  ( 23.04644915753889833, -19.60034241002689726, -55.67430029654918400 ) ) ;
#43440 = CARTESIAN_POINT ( 'NONE',  ( -21.26982224466123839, -4.540630827726737095, -53.50719499581953897 ) ) ;
#43441 = CARTESIAN_POINT ( 'NONE',  ( 56.47485811939319689, -50.74143557146020100, -53.50470819900189667 ) ) ;
#43442 = CARTESIAN_POINT ( 'NONE',  ( 18.71923009779332503, -9.337457873371985073, -46.07711848848515501 ) ) ;
#43443 = CARTESIAN_POINT ( 'NONE',  ( 61.39813329574750611, -1.033231316043849768, -16.14322717339910085 ) ) ;
#43444 = EDGE_CURVE ( 'NONE', #15377, #42024, #13200, .T. ) ;
#43445 = CARTESIAN_POINT ( 'NONE',  ( 51.68229834213279617, -48.76553687035409723, -77.01558403215359760 ) ) ;
#43446 = LINE ( 'NONE', #20800, #13729 ) ;
#43447 = ORIENTED_EDGE ( 'NONE', *, *, #18905, .T. ) ;
#43448 = CARTESIAN_POINT ( 'NONE',  ( 63.18115153217100755, 0.8966068345641480253, -69.03681046574699565 ) ) ;
#43449 = CARTESIAN_POINT ( 'NONE',  ( 10.93327293485905471, -20.38018394046732595, -51.61111978222447050 ) ) ;
#43450 = CARTESIAN_POINT ( 'NONE',  ( 21.54530235781215453, -11.45757796651336768, -52.24448483740684424 ) ) ;
#43451 = VECTOR ( 'NONE', #33580, 1000.000000000000000 ) ;
#43452 = CARTESIAN_POINT ( 'NONE',  ( 16.68946024236489833, -7.788153305987209229, -57.53504572143799578 ) ) ;
#43453 = CARTESIAN_POINT ( 'NONE',  ( 13.61751436023210005, -50.16766667186070094, -20.94898426184690265 ) ) ;
#43454 = CARTESIAN_POINT ( 'NONE',  ( 55.38096894651479829, 19.39060553094100214, -76.22684432684179967 ) ) ;
#43455 = CARTESIAN_POINT ( 'NONE',  ( -18.86606260230390220, 19.38381105532060289, 16.85000000000000142 ) ) ;
#43456 = CARTESIAN_POINT ( 'NONE',  ( 56.36309497301279947, 13.88381105532070059, -15.20458750986569996 ) ) ;
#43457 = CARTESIAN_POINT ( 'NONE',  ( 61.01756443532780594, -45.37431638178470195, -47.00084460110949891 ) ) ;
#43458 = CARTESIAN_POINT ( 'NONE',  ( 47.64143405402000297, -54.53488714544439375, -55.14905519569939685 ) ) ;
#43459 = EDGE_CURVE ( 'NONE', #13362, #21835, #47789, .T. ) ;
#43460 = CARTESIAN_POINT ( 'NONE',  ( 16.84831893358350285, -22.63275635300900035, -57.31488281878699098 ) ) ;
#43461 = CARTESIAN_POINT ( 'NONE',  ( 46.81105700171560358, -39.69772926811019431, -54.41163925913020449 ) ) ;
#43462 = ORIENTED_EDGE ( 'NONE', *, *, #18905, .F. ) ;
#43463 = CARTESIAN_POINT ( 'NONE',  ( 46.40621397470390264, 21.74426214990070250, -76.14873014702980925 ) ) ;
#43464 = CARTESIAN_POINT ( 'NONE',  ( 64.86758340617990370, 0.9945465939392541532, -60.62606712929739672 ) ) ;
#43465 = CARTESIAN_POINT ( 'NONE',  ( 23.83903791948154094, -13.54551468052735963, -51.42433247511532102 ) ) ;
#43466 = CARTESIAN_POINT ( 'NONE',  ( 86.75761129539397132, 18.79802461769378397, -60.02031173921621132 ) ) ;
#43467 = B_SPLINE_CURVE_WITH_KNOTS ( 'NONE', 3,
 ( #10530, #26489, #42503, #30680, #46705, #2664, #10789, #6311, #34062, #50591, #33556, #26202, #26460, #46674, #6565, #13659, #37762, #50336, #49821, #10760, #38019, #6833, #26719, #1598, #38541, #41953, #2368, #42213, #1858, #6052, #17836, #2114, #22269, #17586, #38279, #42737, #18346 ),
 .UNSPECIFIED., .F., .F.,
 ( 4, 2, 2, 2, 2, 2, 2, 2, 2, 2, 2, 2, 2, 2, 1, 1, 1, 1, 1, 2, 4 ),
 ( 0.000000000000000000, 0.06250093636191540736, 0.1250018727238308147, 0.1875028090857462082, 0.2500037454476616294, 0.2812542136286192984, 0.3125046818095770229, 0.3437551499905348584, 0.3750056181714926384, 0.4062560863524504740, 0.4375065545334082540, 0.4687570227143661450, 0.4843822568048449240, 0.4921948738500844245, 0.4961011823727041747, 0.4980543366340139944, 0.4990309137646689042, 0.4995192023299963036, 0.4997633466126600310, 0.4998854187539919502, 0.5000074908953238140 ),
 .UNSPECIFIED. ) ;
#43468 = CARTESIAN_POINT ( 'NONE',  ( 83.89200044194980421, 18.85811933572209753, -52.57651812407429759 ) ) ;
#43469 = CARTESIAN_POINT ( 'NONE',  ( 17.90512170467987474, -9.025297858467601131, -76.03613063694051277 ) ) ;
#43470 = CARTESIAN_POINT ( 'NONE',  ( 10.97864148259309935, 33.91456773539839986, -18.17421237882080476 ) ) ;
#43471 = DIRECTION ( 'NONE',  ( -0.9200120562340476926, -0.3918900565005438708, 0.000000000000000000 ) ) ;
#43473 = CARTESIAN_POINT ( 'NONE',  ( 47.13098424738270609, -38.11658957897590483, -54.64686075001500143 ) ) ;
#43472 = CARTESIAN_POINT ( 'NONE',  ( 63.02123093760216221, 0.4193442080440759612, -17.11446765124405900 ) ) ;
#43474 = CARTESIAN_POINT ( 'NONE',  ( 24.04493509668306572, -15.60920340738896606, -71.50739165550209009 ) ) ;
#43475 = CARTESIAN_POINT ( 'NONE',  ( 49.22498099147649953, 22.62797864033339934, -55.23666898610220244 ) ) ;
#43476 = EDGE_LOOP ( 'NONE', ( #6588, #19742, #14673, #23109, #3147 ) ) ;
#43477 = EDGE_CURVE ( 'NONE', #39182, #814, #23988, .T. ) ;
#43478 = AXIS2_PLACEMENT_3D ( 'NONE', #28274, #13108, #29059 ) ;
#43479 = CARTESIAN_POINT ( 'NONE',  ( 52.60258585013299637, -49.82394164341149434, -48.51135465991440299 ) ) ;
#43480 = ORIENTED_EDGE ( 'NONE', *, *, #16566, .F. ) ;
#43481 = VECTOR ( 'NONE', #11372, 1000.000000000000000 ) ;
#43482 = CARTESIAN_POINT ( 'NONE',  ( 47.12305569550148476, 6.751649648232654677, -54.63870115556262874 ) ) ;
#43483 = CARTESIAN_POINT ( 'NONE',  ( 14.55219274796575313, 20.46959765477225091, -75.56421372419544014 ) ) ;
#43484 = CARTESIAN_POINT ( 'NONE',  ( 8.133937397696209715, -54.80802482921019703, -21.14999999999999858 ) ) ;
#43485 = CARTESIAN_POINT ( 'NONE',  ( 51.67587649748560352, -48.69064075877850684, -77.01363636363639387 ) ) ;
#43486 = VECTOR ( 'NONE', #1650, 1000.000000000000000 ) ;
#43487 = CARTESIAN_POINT ( 'NONE',  ( 18.02732184005409977, -22.41013139733979997, -56.86630649184920117 ) ) ;
#43488 = VECTOR ( 'NONE', #37679, 1000.000000000000000 ) ;
#43490 = EDGE_CURVE ( 'NONE', #2299, #25155, #596, .T. ) ;
#43489 = DIRECTION ( 'NONE',  ( 0.000000000000000000, -1.000000000000000000, 0.000000000000000000 ) ) ;
#43491 = CARTESIAN_POINT ( 'NONE',  ( 56.63382897851940356, -45.18506093673340018, -16.44084196791180119 ) ) ;
#43492 = CARTESIAN_POINT ( 'NONE',  ( 55.85841962760110135, 14.74773305113219912, -25.34033445086470238 ) ) ;
#43493 = EDGE_LOOP ( 'NONE', ( #16962, #21965, #20802, #5929 ) ) ;
#43494 = CIRCLE ( 'NONE', #11695, 5.251829701412229490 ) ;
#43495 = CARTESIAN_POINT ( 'NONE',  ( 23.52146105081359906, -18.26406402817810104, -45.39705537816429626 ) ) ;
#43496 = ORIENTED_EDGE ( 'NONE', *, *, #41819, .F. ) ;
#43497 = CARTESIAN_POINT ( 'NONE',  ( 11.61081910261030004, -65.23863181566240144, -17.07039304614280084 ) ) ;
#43498 = CARTESIAN_POINT ( 'NONE',  ( 11.02897443665469979, 33.86259216482670098, -47.16934780673829408 ) ) ;
#43499 = CARTESIAN_POINT ( 'NONE',  ( 73.11007580172049813, 0.9281439705311369526, -62.29764659744859756 ) ) ;
#43500 = CARTESIAN_POINT ( 'NONE',  ( 19.13393739769600188, 18.38381105532069881, -35.14999999999999858 ) ) ;
#43501 = CARTESIAN_POINT ( 'NONE',  ( 11.54127901367117914, -65.34045536701110279, -22.61052249223064692 ) ) ;
#43502 = DIRECTION ( 'NONE',  ( 0.000000000000000000, 0.000000000000000000, -1.000000000000000000 ) ) ;
#43503 = EDGE_LOOP ( 'NONE', ( #39588, #31610, #8246, #33629 ) ) ;
#43504 = CARTESIAN_POINT ( 'NONE',  ( 44.11147024075970080, -33.11640768660669920, -54.64999999999999858 ) ) ;
#43505 = CARTESIAN_POINT ( 'NONE',  ( 10.97782631398749942, -63.13468953106429638, -44.74264417585560238 ) ) ;
#43506 = CARTESIAN_POINT ( 'NONE',  ( 66.23540447448930024, 18.72622661238430553, -73.39853292320987066 ) ) ;
#43507 = ORIENTED_EDGE ( 'NONE', *, *, #4296, .F. ) ;
#43508 = LINE ( 'NONE', #47957, #41765 ) ;
#43509 = CARTESIAN_POINT ( 'NONE',  ( 56.68249757595900462, 19.21262946785479997, -52.87688493478909635 ) ) ;
#43510 = CARTESIAN_POINT ( 'NONE',  ( 24.04635993889370127, -15.33348728407727712, -49.49630671588138142 ) ) ;
#43511 = ORIENTED_EDGE ( 'NONE', *, *, #45336, .F. ) ;
#43512 = CARTESIAN_POINT ( 'NONE',  ( 24.04487853986463008, -15.61618860033810030, -61.79233400586811342 ) ) ;
#43513 = PLANE ( 'NONE',  #32548 ) ;
#43514 = CARTESIAN_POINT ( 'NONE',  ( 10.35043018118175695, -19.20900750040789262, -33.27603111959778914 ) ) ;
#43515 = DIRECTION ( 'NONE',  ( 0.3863301728269248891, -0.9223605572461988089, 0.000000000000000000 ) ) ;
#43516 = CARTESIAN_POINT ( 'NONE',  ( 23.80510751029979843, -18.63874897884280202, -77.91180489532798958 ) ) ;
#43517 = DIRECTION ( 'NONE',  ( 0.000000000000000000, 0.000000000000000000, -1.000000000000000000 ) ) ;
#43518 = AXIS2_PLACEMENT_3D ( 'NONE', #33713, #37923, #2538 ) ;
#43519 = CARTESIAN_POINT ( 'NONE',  ( 46.42406059160111198, -38.19600863765170828, -58.19938352928596714 ) ) ;
#43520 = DIRECTION ( 'NONE',  ( 1.000000000000000000, 0.000000000000000000, 0.000000000000000000 ) ) ;
#43521 = EDGE_LOOP ( 'NONE', ( #15830, #40458, #7104, #11840, #27850, #39587 ) ) ;
#43522 = ORIENTED_EDGE ( 'NONE', *, *, #23858, .F. ) ;
#43523 = AXIS2_PLACEMENT_3D ( 'NONE', #28917, #22085, #29441 ) ;
#43524 = VECTOR ( 'NONE', #35839, 1000.000000000000114 ) ;
#43525 = CARTESIAN_POINT ( 'NONE',  ( 19.43693194943929825, -22.29428154633589898, -54.58645138154409437 ) ) ;
#43526 = AXIS2_PLACEMENT_3D ( 'NONE', #24498, #20579, #3595 ) ;
#43527 = EDGE_CURVE ( 'NONE', #22043, #10696, #4616, .T. ) ;
#43528 = CARTESIAN_POINT ( 'NONE',  ( 24.04493739769619864, -15.61618894467929941, -32.14999999999999858 ) ) ;
#43529 = CARTESIAN_POINT ( 'NONE',  ( 9.818495732055460223, -19.87888382093819928, -32.14999999999999858 ) ) ;
#43530 = EDGE_CURVE ( 'NONE', #45901, #24962, #12800, .T. ) ;
#43531 = CARTESIAN_POINT ( 'NONE',  ( 47.15820541288359635, 23.35149450075520150, -75.00623917109859917 ) ) ;
#43532 = CIRCLE ( 'NONE', #20914, 15.56227766016840164 ) ;
#43533 = CARTESIAN_POINT ( 'NONE',  ( 18.14758755231450493, -4.788411538692897373, -34.79644660940672907 ) ) ;
#43534 = ADVANCED_FACE ( 'NONE', ( #17714 ), #36584, .T. ) ;
#43535 = CARTESIAN_POINT ( 'NONE',  ( 9.937051593247810288, 22.47179399159399793, -34.65604926186119172 ) ) ;
#43536 = CARTESIAN_POINT ( 'NONE',  ( 11.76101335023730066, 33.66270366472770803, -16.31614116035649786 ) ) ;
#43537 = CARTESIAN_POINT ( 'NONE',  ( 8.416037913024730699, -18.51735220335379850, -72.39321698031869801 ) ) ;
#43538 = CARTESIAN_POINT ( 'NONE',  ( 21.78353651810359892, -20.85666229875000255, -32.14999999999999858 ) ) ;
#43539 = CARTESIAN_POINT ( 'NONE',  ( 55.05482395368899518, -50.61618894681969749, -76.63544833123130218 ) ) ;
#43541 = CARTESIAN_POINT ( 'NONE',  ( 11.13393739769620616, -55.30245861064820190, -44.08754233725599647 ) ) ;
#43540 = CARTESIAN_POINT ( 'NONE',  ( -9.688667659886910144, 11.02459018896860066, -4.264896373567980348 ) ) ;
#43542 = CARTESIAN_POINT ( 'NONE',  ( 63.06339012708429692, 0.9214125008369580261, -68.85787081529349507 ) ) ;
#43543 = CARTESIAN_POINT ( 'NONE',  ( 61.39882506316129707, 13.96060197418889892, -46.69637642908890030 ) ) ;
#43544 = DIRECTION ( 'NONE',  ( -8.660081000000000658E-17, -2.123755000000000144E-17, -1.000000000000000000 ) ) ;
#43545 = DIRECTION ( 'NONE',  ( 0.000000000000000000, 0.000000000000000000, -1.000000000000000000 ) ) ;
#43546 = ORIENTED_EDGE ( 'NONE', *, *, #6084, .F. ) ;
#43547 = CARTESIAN_POINT ( 'NONE',  ( 52.79375803185560301, -49.68041131509039587, -48.48716100244389793 ) ) ;
#43548 = CARTESIAN_POINT ( 'NONE',  ( 47.74808848842369713, 23.19578408484800036, -54.68947420106290025 ) ) ;
#43549 = CARTESIAN_POINT ( 'NONE',  ( 8.728929033786567260, -12.74017886842098335, -64.91034747281507578 ) ) ;
#43550 = CARTESIAN_POINT ( 'NONE',  ( 24.04468322966528859, -15.61618861995729013, -71.79233702014498419 ) ) ;
#43551 = CARTESIAN_POINT ( 'NONE',  ( 61.48324830189730505, 14.13192806243720057, -47.33702467829240135 ) ) ;
#43552 = CARTESIAN_POINT ( 'NONE',  ( 8.687638548776371650, -15.37261707081270146, -77.24306566573929445 ) ) ;
#43553 = CARTESIAN_POINT ( 'NONE',  ( 51.79788809998749599, 18.93511776858189677, -76.50613236165939668 ) ) ;
#43555 = EDGE_CURVE ( 'NONE', #50266, #38136, #45502, .T. ) ;
#43554 = CARTESIAN_POINT ( 'NONE',  ( 52.76444409924949497, 18.46836548807459977, -48.64233343848459867 ) ) ;
#43556 = DIRECTION ( 'NONE',  ( 1.000000000000000000, 0.000000000000000000, 0.000000000000000000 ) ) ;
#43557 = CARTESIAN_POINT ( 'NONE',  ( 52.84731369148330060, -49.65172165314799457, -48.60966827451719752 ) ) ;
#43558 = CARTESIAN_POINT ( 'NONE',  ( 16.13393739769620083, -15.61618894467919816, -82.14319696191608955 ) ) ;
#43559 = VECTOR ( 'NONE', #46500, 1000.000000000000000 ) ;
#43560 = CARTESIAN_POINT ( 'NONE',  ( 47.66631869268250199, -54.51824591515769924, -54.99485691796319742 ) ) ;
#43561 = CYLINDRICAL_SURFACE ( 'NONE', #5273, 1.999999999999997113 ) ;
#43562 = CARTESIAN_POINT ( 'NONE',  ( 17.01976930770689833, -22.38318413455865397, -70.91115524790816949 ) ) ;
#43563 = CARTESIAN_POINT ( 'NONE',  ( 65.05499895842218905, -32.25244862226109888, -17.84090853625750128 ) ) ;
#43564 = CARTESIAN_POINT ( 'NONE',  ( 71.15549028777350316, 1.383161449028130097, -60.96613084263369586 ) ) ;
#43565 = CARTESIAN_POINT ( 'NONE',  ( 16.13393739769620083, -1.700401765863659209, -34.89146800830129536 ) ) ;
#43566 = CARTESIAN_POINT ( 'NONE',  ( 72.46066273947089087, 1.275252243133929930, -61.58318855245290280 ) ) ;
#43567 = CIRCLE ( 'NONE', #30971, 0.5000000000000004441 ) ;
#43568 = LINE ( 'NONE', #7668, #30969 ) ;
#43569 = CARTESIAN_POINT ( 'NONE',  ( 59.52869410915831594, -45.48984219772450643, -26.73579121603098585 ) ) ;
#43570 = VERTEX_POINT ( 'NONE', #9600 ) ;
#43571 = ORIENTED_EDGE ( 'NONE', *, *, #15221, .T. ) ;
#43572 = CARTESIAN_POINT ( 'NONE',  ( 11.27219963446819229, -9.290068936367397612, -55.08398911216916360 ) ) ;
#43573 = DIRECTION ( 'NONE',  ( 0.000000000000000000, 0.000000000000000000, -1.000000000000000000 ) ) ;
#43574 = VERTEX_POINT ( 'NONE', #1731 ) ;
#43575 = CARTESIAN_POINT ( 'NONE',  ( 16.13393739769620083, -15.61618894467929941, 6.072546842075589701 ) ) ;
#43576 = CARTESIAN_POINT ( 'NONE',  ( 21.71415593298656788, -21.22378504329634552, -77.75844095104929465 ) ) ;
#43577 = VERTEX_POINT ( 'NONE', #17204 ) ;
#43578 = CARTESIAN_POINT ( 'NONE',  ( 10.98127921298129728, 33.58944323623821049, -23.21470234273132149 ) ) ;
#43579 = CARTESIAN_POINT ( 'NONE',  ( 43.43225333442439506, 6.607470992752627836, -73.15836440129699270 ) ) ;
#43580 = CARTESIAN_POINT ( 'NONE',  ( 13.02068638423840063, 34.28679101843700039, -23.33284745141469685 ) ) ;
#43581 = B_SPLINE_CURVE_WITH_KNOTS ( 'NONE', 3,
 ( #36835, #8284, #24494, #16403, #48645, #24759, #13010, #40512, #4870, #28700 ),
 .UNSPECIFIED., .F., .F.,
 ( 4, 2, 2, 2, 4 ),
 ( 0.1813467805151689483, 0.3860100853863767112, 0.5906733902575844741, 0.7953366951287922371, 1.000000000000000000 ),
 .UNSPECIFIED. ) ;
#43582 = CARTESIAN_POINT ( 'NONE',  ( 23.04746735250069989, -11.12332531222269871, -35.60889570735529475 ) ) ;
#43583 = DIRECTION ( 'NONE',  ( 0.8660254037844379305, -0.5000000000000011102, 0.000000000000000000 ) ) ;
#43584 = CARTESIAN_POINT ( 'NONE',  ( 24.04470982567631410, -15.68103954860247740, -49.79493908758399101 ) ) ;
#43585 = LINE ( 'NONE', #14511, #43559 ) ;
#43586 = CARTESIAN_POINT ( 'NONE',  ( 62.40084614537109786, -29.97498645692460073, -16.17177386113289828 ) ) ;
#43587 = CARTESIAN_POINT ( 'NONE',  ( 14.34417029198830029, 19.88381105532299742, -74.14999999999999147 ) ) ;
#43588 = CARTESIAN_POINT ( 'NONE',  ( 47.07018870238729846, -54.05275391524939721, -75.65465545553870186 ) ) ;
#43589 = CARTESIAN_POINT ( 'NONE',  ( 8.380768790010019842, -14.40164206111660050, -73.06195620990739314 ) ) ;
#43590 = CARTESIAN_POINT ( 'NONE',  ( 54.67236884565690502, 14.97126989199350078, -15.88466681443639850 ) ) ;
#43591 = CARTESIAN_POINT ( 'NONE',  ( 42.10987924529349868, 14.38172689610610000, -6.748859080943129918 ) ) ;
#43592 = ADVANCED_FACE ( 'NONE', ( #13789 ), #10116, .T. ) ;
#43593 = CARTESIAN_POINT ( 'NONE',  ( 14.98932716411379928, 21.70054973260339892, -76.14999999999999147 ) ) ;
#43594 = EDGE_CURVE ( 'NONE', #49564, #48985, #48430, .T. ) ;
#43595 = VECTOR ( 'NONE', #15252, 1000.000000000000114 ) ;
#43596 = CIRCLE ( 'NONE', #87, 28.27108544675919788 ) ;
#43597 = CARTESIAN_POINT ( 'NONE',  ( 84.38939444912799104, -43.48290221131350108, -47.32729711157580255 ) ) ;
#43598 = CARTESIAN_POINT ( 'NONE',  ( 65.36617461242161653, -30.59625171506405295, -16.64867345289078671 ) ) ;
#43599 = CARTESIAN_POINT ( 'NONE',  ( 18.04724510464590281, -7.596090795186240641, -43.08221248677949688 ) ) ;
#43600 = ORIENTED_EDGE ( 'NONE', *, *, #19045, .T. ) ;
#43601 = CARTESIAN_POINT ( 'NONE',  ( 54.75372257292519862, -47.88473616892759566, -26.64369953896449772 ) ) ;
#43602 = CARTESIAN_POINT ( 'NONE',  ( 14.70125025179870093, -50.53285427156319543, -20.74420046562639897 ) ) ;
#43603 = CARTESIAN_POINT ( 'NONE',  ( 75.70738177086290932, 12.17974452044730072, -13.47559339050390115 ) ) ;
#43604 = B_SPLINE_CURVE_WITH_KNOTS ( 'NONE', 3,
 ( #49405, #29458, #4575, #48881, #45463, #12986, #20547, #9561, #36542, #28936 ),
 .UNSPECIFIED., .F., .F.,
 ( 4, 2, 2, 2, 4 ),
 ( 0.000000000000000000, 0.2643499294688712031, 0.4734939176322996990, 0.8917818939591528604, 1.000000000000000000 ),
 .UNSPECIFIED. ) ;
#43605 = CARTESIAN_POINT ( 'NONE',  ( 75.45398146315633880, 12.53648618435466133, -13.49434368755179747 ) ) ;
#43606 = DIRECTION ( 'NONE',  ( 0.000000000000000000, 0.000000000000000000, -1.000000000000000000 ) ) ;
#43607 = EDGE_LOOP ( 'NONE', ( #25189, #1375, #6902, #26676 ) ) ;
#43608 = CARTESIAN_POINT ( 'NONE',  ( -8.352801854373527846, -44.78526516041389982, -5.739504211299600200 ) ) ;
#43609 = CARTESIAN_POINT ( 'NONE',  ( 23.83903723949826414, -17.68686655609902658, -37.87566771034045132 ) ) ;
#43610 = DIRECTION ( 'NONE',  ( 0.000000000000000000, -1.000000000000000000, 0.000000000000000000 ) ) ;
#43611 = CARTESIAN_POINT ( 'NONE',  ( 63.23767253740619765, 1.267233196669030004, -62.48314610740069242 ) ) ;
#43612 = CARTESIAN_POINT ( 'NONE',  ( 57.33945454586879720, -50.32221370019689743, -52.87108245925089989 ) ) ;
#43613 = CARTESIAN_POINT ( 'NONE',  ( 41.94994391832800318, 12.69230833618010124, -4.524181473528510189 ) ) ;
#43615 = ADVANCED_FACE ( 'NONE', ( #5673 ), #42493, .T. ) ;
#43614 = CARTESIAN_POINT ( 'NONE',  ( 61.32247977517523907, -45.56437718414176175, -47.63520364883854086 ) ) ;
#43616 = CARTESIAN_POINT ( 'NONE',  ( 0.2602139982834061338, 14.91936600910487343, -34.65037388166341259 ) ) ;
#43617 = DIRECTION ( 'NONE',  ( 0.000000000000000000, 0.000000000000000000, 1.000000000000000000 ) ) ;
#43618 = CARTESIAN_POINT ( 'NONE',  ( -0.2133638169075534607, -20.52615564361606815, -34.95200341233793750 ) ) ;
#43619 = CARTESIAN_POINT ( 'NONE',  ( 30.68460988201149320, -15.41618894467931611, -103.0993275156849762 ) ) ;
#43620 = CARTESIAN_POINT ( 'NONE',  ( 18.17012112126710122, -52.29987767205400218, -75.77396328158869210 ) ) ;
#43621 = EDGE_CURVE ( 'NONE', #11158, #12367, #41883, .T. ) ;
#43622 = CARTESIAN_POINT ( 'NONE',  ( 17.31586692445079834, -22.97212103600040223, -67.51663103545399736 ) ) ;
#43623 = CARTESIAN_POINT ( 'NONE',  ( 11.27237412149550977, -9.289936927475686446, -40.79933478808754188 ) ) ;
#43624 = CARTESIAN_POINT ( 'NONE',  ( 63.31978226060338955, 1.136600705754869933, -62.14534926897810152 ) ) ;
#43625 = VERTEX_POINT ( 'NONE', #45762 ) ;
#43626 = DIRECTION ( 'NONE',  ( 0.5720614028176831400, -0.4156269377774557405, -0.7071067811865470176 ) ) ;
#43627 = CARTESIAN_POINT ( 'NONE',  ( 10.52996152801476093, -19.45088358834182074, -35.26171248262056679 ) ) ;
#43628 = CARTESIAN_POINT ( 'NONE',  ( 73.08075677931830683, 1.188042061556800144, -68.87465088918141021 ) ) ;
#43629 = DIRECTION ( 'NONE',  ( 0.000000000000000000, 0.000000000000000000, 1.000000000000000000 ) ) ;
#43630 = CARTESIAN_POINT ( 'NONE',  ( 8.974641593888140534, -14.92660264788080049, -81.23899999999999011 ) ) ;
#43631 = ORIENTED_EDGE ( 'NONE', *, *, #47308, .T. ) ;
#43632 = CARTESIAN_POINT ( 'NONE',  ( 18.02088350666679872, 20.74698410172580054, -75.72128529899769944 ) ) ;
#43633 = ORIENTED_EDGE ( 'NONE', *, *, #48629, .T. ) ;
#43634 = ORIENTED_EDGE ( 'NONE', *, *, #16093, .F. ) ;
#43635 = FACE_OUTER_BOUND ( 'NONE', #42019, .T. ) ;
#43636 = CARTESIAN_POINT ( 'NONE',  ( 23.52286796769300281, -16.13183659920250079, -81.23899999999999011 ) ) ;
#43637 = CARTESIAN_POINT ( 'NONE',  ( -110.3642515470889975, -33.11618894529460277, -112.3286729284269967 ) ) ;
#43638 = TOROIDAL_SURFACE ( 'NONE', #32704, 18.00000000000000000, 2.000000000000000000 ) ;
#43639 = CARTESIAN_POINT ( 'NONE',  ( 61.64525490299610766, 13.96903739949059897, -46.95128602980910415 ) ) ;
#43640 = AXIS2_PLACEMENT_3D ( 'NONE', #3996, #8699, #15784 ) ;
#43641 = ORIENTED_EDGE ( 'NONE', *, *, #3144, .F. ) ;
#43642 = AXIS2_PLACEMENT_3D ( 'NONE', #48995, #17018, #24322 ) ;
#43643 = CARTESIAN_POINT ( 'NONE',  ( 16.13393739769579582, -15.61618894467939889, -10.44999999999980034 ) ) ;
#43644 = ORIENTED_EDGE ( 'NONE', *, *, #16834, .F. ) ;
#43645 = CARTESIAN_POINT ( 'NONE',  ( 83.89200044194980421, -50.61618894467930119, -53.92796738110899923 ) ) ;
#43646 = CARTESIAN_POINT ( 'NONE',  ( 16.13393739769620083, -15.61618894467929941, -7.101316701949489385 ) ) ;
#43647 = ORIENTED_EDGE ( 'NONE', *, *, #8316, .F. ) ;
#43648 = CARTESIAN_POINT ( 'NONE',  ( 44.66728565622769054, 1.931601751605777073, -44.70166766796090485 ) ) ;
#43649 = CARTESIAN_POINT ( 'NONE',  ( 52.46419972536169496, -51.19626386910670135, -75.99844944557069937 ) ) ;
#43650 = CARTESIAN_POINT ( 'NONE',  ( 60.56461264277469780, 14.52689081580879993, -47.69384697653629956 ) ) ;
#43651 = EDGE_CURVE ( 'NONE', #46747, #17157, #42083, .T. ) ;
#43652 = CARTESIAN_POINT ( 'NONE',  ( 11.89321892218980103, 34.20364954172580241, -22.25048313876769868 ) ) ;
#43653 = CARTESIAN_POINT ( 'NONE',  ( -9.419262753694910728, 12.55375140257260114, -5.879062740130000186 ) ) ;
#43654 = CARTESIAN_POINT ( 'NONE',  ( 46.70834501317497001, 22.49584756229791083, -75.96332490896284639 ) ) ;
#43655 = CARTESIAN_POINT ( 'NONE',  ( 12.28756344725089988, -21.52786946782889999, -43.53078881371720144 ) ) ;
#43656 = CARTESIAN_POINT ( 'NONE',  ( 9.206818668722608123, -19.30424728178379823, -60.13177655599749727 ) ) ;
#43657 = EDGE_LOOP ( 'NONE', ( #34253, #47150, #45362, #13728, #5023 ) ) ;
#43658 = CARTESIAN_POINT ( 'NONE',  ( 41.20098873942420425, 14.32627756744839864, -6.156279893315419471 ) ) ;
#43659 = CARTESIAN_POINT ( 'NONE',  ( 71.90239294763270550, 0.9973858971030851173, -70.31979469916329606 ) ) ;
#43660 = CARTESIAN_POINT ( 'NONE',  ( 44.31273514806447622, -39.97978406752861247, -65.14464952758170568 ) ) ;
#43661 = CARTESIAN_POINT ( 'NONE',  ( 13.94847430742629868, 19.04672674949359745, -20.89779807318980076 ) ) ;
#43662 = VECTOR ( 'NONE', #24739, 999.9999999999998863 ) ;
#43663 = VECTOR ( 'NONE', #11420, 1000.000000000000114 ) ;
#43664 = CYLINDRICAL_SURFACE ( 'NONE', #15492, 1.999999999999970246 ) ;
#43665 = VECTOR ( 'NONE', #13796, 1000.000000000000000 ) ;
#43666 = CARTESIAN_POINT ( 'NONE',  ( 63.25144821230251324, 0.9425424353906030062, -69.13730826794480322 ) ) ;
#43667 = CARTESIAN_POINT ( 'NONE',  ( 48.73678662100309822, -53.88539940205489387, -54.49010856789290358 ) ) ;
#43668 = FACE_OUTER_BOUND ( 'NONE', #12791, .T. ) ;
#43669 = CARTESIAN_POINT ( 'NONE',  ( 63.32231416895070453, 0.9254875393589929722, -69.23491771966379815 ) ) ;
#43670 = CARTESIAN_POINT ( 'NONE',  ( 12.14989696424939147, -22.52876359041865229, -38.17433614912694395 ) ) ;
#43671 = ADVANCED_FACE ( 'NONE', ( #37115 ), #45241, .F. ) ;
#43672 = CARTESIAN_POINT ( 'NONE',  ( 47.66548848826279539, 23.29226298427809638, -55.16185052358790131 ) ) ;
#43673 = VERTEX_POINT ( 'NONE', #37371 ) ;
#43674 = CARTESIAN_POINT ( 'NONE',  ( 8.916825887739390666, -17.46551200763889966, -35.98749647213350045 ) ) ;
#43675 = CARTESIAN_POINT ( 'NONE',  ( 64.74323834027561020, 1.229084191802120030, -60.83585027030739667 ) ) ;
#43676 = EDGE_LOOP ( 'NONE', ( #47200, #39184, #8772, #36259 ) ) ;
#43677 = CARTESIAN_POINT ( 'NONE',  ( 18.70688454841999970, -48.06418385137889970, -35.14999999999999858 ) ) ;
#43678 = CARTESIAN_POINT ( 'NONE',  ( 60.24866557976200454, -45.78236623157710028, -47.36885438232280165 ) ) ;
#43679 = DIRECTION ( 'NONE',  ( 0.000000000000000000, 0.000000000000000000, -1.000000000000000000 ) ) ;
#43680 = CARTESIAN_POINT ( 'NONE',  ( 62.09157612670949788, -33.11618894467940066, -65.34607522167520699 ) ) ;
#43682 = CARTESIAN_POINT ( 'NONE',  ( 45.07858682377059978, -46.11248607424209922, -9.026855431852869316 ) ) ;
#43681 = CARTESIAN_POINT ( 'NONE',  ( 41.49957317341533525, 8.476577171076462136, -78.74628940708531388 ) ) ;
#43683 = DIRECTION ( 'NONE',  ( 0.000000000000000000, 0.000000000000000000, -1.000000000000000000 ) ) ;
#43684 = CARTESIAN_POINT ( 'NONE',  ( 18.13393739769620083, -41.61618894467930119, -35.14999999999999858 ) ) ;
#43685 = ORIENTED_EDGE ( 'NONE', *, *, #12114, .F. ) ;
#43686 = CARTESIAN_POINT ( 'NONE',  ( 0.1124364628814909922, 19.94096921249579779, -35.13980537375690005 ) ) ;
#43687 = ORIENTED_EDGE ( 'NONE', *, *, #30622, .F. ) ;
#43688 = DIRECTION ( 'NONE',  ( 0.000000000000000000, 0.000000000000000000, -1.000000000000000000 ) ) ;
#43689 = CARTESIAN_POINT ( 'NONE',  ( 20.11803275322282758, -8.703644260883391937, -39.45899364610082216 ) ) ;
#43690 = DIRECTION ( 'NONE',  ( 0.000000000000000000, 0.000000000000000000, 1.000000000000000000 ) ) ;
#43691 = CARTESIAN_POINT ( 'NONE',  ( 11.67521959659690012, -65.26890461106869168, -47.24652687432000420 ) ) ;
#43692 = VERTEX_POINT ( 'NONE', #17459 ) ;
#43693 = CARTESIAN_POINT ( 'NONE',  ( 19.31296351478360052, 18.65448050664020130, -82.14319696191608955 ) ) ;
#43694 = CARTESIAN_POINT ( 'NONE',  ( 56.75573796874090249, -45.26196802996069835, -25.29489359144389837 ) ) ;
#43695 = CARTESIAN_POINT ( 'NONE',  ( 56.40078553072530099, -50.54434665457389997, -52.89577359589869587 ) ) ;
#43696 = CARTESIAN_POINT ( 'NONE',  ( 22.90093225693778223, -15.60714275223250525, -46.45240273082318794 ) ) ;
#43697 = CARTESIAN_POINT ( 'NONE',  ( 61.06650679487360378, -1.429311427220590014, -16.00487319935590236 ) ) ;
#43698 = CARTESIAN_POINT ( 'NONE',  ( 52.02482082126720542, -49.78138960277850344, -76.90588669317190806 ) ) ;
#43699 = CARTESIAN_POINT ( 'NONE',  ( 68.13393739769618662, -5.818188944679350882, -65.65000000000000568 ) ) ;
#43700 = ORIENTED_EDGE ( 'NONE', *, *, #6371, .T. ) ;
#43701 = CARTESIAN_POINT ( 'NONE',  ( 64.43393739769608430, 11.38381105532050519, -61.94999999999998863 ) ) ;
#43703 = CARTESIAN_POINT ( 'NONE',  ( 75.82138965228800487, 12.11553555588150921, -13.50018836794542487 ) ) ;
#43702 = AXIS2_PLACEMENT_3D ( 'NONE', #14866, #35294, #30830 ) ;
#43704 = CARTESIAN_POINT ( 'NONE',  ( 1.058369240368409958, -22.58802147093010149, -34.64999999999999858 ) ) ;
#43705 = CARTESIAN_POINT ( 'NONE',  ( 22.90106509282977854, -15.61618896609811458, -36.45282238757207693 ) ) ;
#43706 = CARTESIAN_POINT ( 'NONE',  ( 9.932201140091338587, -20.42505731288110127, -58.80254861845589431 ) ) ;
#43707 = CARTESIAN_POINT ( 'NONE',  ( 13.13410622190690091, -50.32702805021810377, -21.17378955277370167 ) ) ;
#43708 = CARTESIAN_POINT ( 'NONE',  ( 55.24231505161220213, 19.39098015012699960, -76.29834687610690480 ) ) ;
#43709 = EDGE_CURVE ( 'NONE', #16578, #34913, #51682, .T. ) ;
#43710 = PLANE ( 'NONE',  #6713 ) ;
#43711 = CARTESIAN_POINT ( 'NONE',  ( 10.72853615272882699, -64.94170179444019197, -18.17421237897245945 ) ) ;
#43713 = EDGE_CURVE ( 'NONE', #41820, #29784, #2290, .T. ) ;
#43712 = CARTESIAN_POINT ( 'NONE',  ( 60.80565956584559473, -45.54811607624679937, -47.42904258599709522 ) ) ;
#43714 = EDGE_CURVE ( 'NONE', #17827, #9229, #38294, .T. ) ;
#43715 = CARTESIAN_POINT ( 'NONE',  ( 9.543089160664727899, -17.38752728827747163, -39.36948714365400548 ) ) ;
#43716 = CARTESIAN_POINT ( 'NONE',  ( 11.30419729876839874, -10.47652263729510125, -58.10707212942319444 ) ) ;
#43717 = FACE_OUTER_BOUND ( 'NONE', #47263, .T. ) ;
#43718 = ADVANCED_FACE ( 'NONE', ( #339 ), #17111, .T. ) ;
#43719 = ORIENTED_EDGE ( 'NONE', *, *, #1668, .F. ) ;
#43720 = CARTESIAN_POINT ( 'NONE',  ( 13.63143226142920028, -51.46210362308260500, -74.58518005236030035 ) ) ;
#43721 = FACE_OUTER_BOUND ( 'NONE', #17393, .T. ) ;
#43722 = CARTESIAN_POINT ( 'NONE',  ( 23.83903529911903618, -13.54550174322651657, -37.42433788284738938 ) ) ;
#43723 = LINE ( 'NONE', #12019, #18743 ) ;
#43724 =( BOUNDED_CURVE ( )  B_SPLINE_CURVE ( 3, ( #10452, #39259, #22734, #3107 ),
 .UNSPECIFIED., .F., .T. ) 
 B_SPLINE_CURVE_WITH_KNOTS ( ( 4, 4 ),
 ( 0.07448749837916979200, 0.3185623355031764192 ),
 .UNSPECIFIED. ) 
 CURVE ( )  GEOMETRIC_REPRESENTATION_ITEM ( )  RATIONAL_B_SPLINE_CURVE ( ( 1.000000000000000000, 0.9950417810258930240, 0.9950417810258930240, 1.000000000000000000 ) ) 
 REPRESENTATION_ITEM ( '' )  );
#43725 = CARTESIAN_POINT ( 'NONE',  ( 46.27112185534480204, 13.88381105532070059, -7.639051677656230055 ) ) ;
#43726 = CARTESIAN_POINT ( 'NONE',  ( 46.64206449348299799, -53.27165255397410704, -76.10218428122850298 ) ) ;
#43727 = DIRECTION ( 'NONE',  ( -0.7071067811865475727, 0.000000000000000000, 0.7071067811865475727 ) ) ;
#43728 = DIRECTION ( 'NONE',  ( -0.2517544074889974115, -0.9677911542837451808, 0.000000000000000000 ) ) ;
#43730 = CARTESIAN_POINT ( 'NONE',  ( 12.14991080221749087, -22.52877141676245998, -58.45899808055179392 ) ) ;
#43729 = DIRECTION ( 'NONE',  ( 1.000000000000000000, 0.000000000000000000, 0.000000000000000000 ) ) ;
#43731 = DIRECTION ( 'NONE',  ( 0.000000000000000000, 0.000000000000000000, -1.000000000000000000 ) ) ;
#43732 = CARTESIAN_POINT ( 'NONE',  ( 8.222339619445261150, -15.61627490117209938, -70.79233150823699816 ) ) ;
#43733 = ADVANCED_FACE ( 'NONE', ( #20494 ), #41209, .T. ) ;
#43734 = CARTESIAN_POINT ( 'NONE',  ( 49.62716556310740401, 22.41720408324059832, -54.74430167493610355 ) ) ;
#43735 = ORIENTED_EDGE ( 'NONE', *, *, #30270, .F. ) ;
#43736 = CARTESIAN_POINT ( 'NONE',  ( 52.62812534184670454, -49.80011865873639465, -48.49159685222129923 ) ) ;
#43737 = ORIENTED_EDGE ( 'NONE', *, *, #945, .F. ) ;
#43738 = CARTESIAN_POINT ( 'NONE',  ( 43.29114022628257885, 7.693946413374631810, -74.22886101434919226 ) ) ;
#43739 = DIRECTION ( 'NONE',  ( 0.000000000000000000, 1.000000000000000000, 0.000000000000000000 ) ) ;
#43740 = CARTESIAN_POINT ( 'NONE',  ( 16.13393739769639623, 7.383811055320659733, -84.65000000000000568 ) ) ;
#43741 = CARTESIAN_POINT ( 'NONE',  ( 52.15298860272049808, -49.68190537283830110, -77.15976494802958996 ) ) ;
#43742 = CARTESIAN_POINT ( 'NONE',  ( 14.46176406050670060, -8.764445004118037730, -59.87662587226679278 ) ) ;
#43743 = DIRECTION ( 'NONE',  ( 0.8090169943749515591, 0.000000000000000000, 0.5877852522924675860 ) ) ;
#43744 = CARTESIAN_POINT ( 'NONE',  ( 56.71583985100659930, -45.26515517447770520, -17.53022232124200031 ) ) ;
#43745 = DIRECTION ( 'NONE',  ( 0.000000000000000000, 0.000000000000000000, -1.000000000000000000 ) ) ;
#43746 = ORIENTED_EDGE ( 'NONE', *, *, #19457, .T. ) ;
#43747 = CARTESIAN_POINT ( 'NONE',  ( 22.37504268966269905, -10.85852639698109989, -45.08017965390980208 ) ) ;
#43748 = EDGE_LOOP ( 'NONE', ( #36654, #14029, #3743, #22849, #30383, #25673 ) ) ;
#43749 = CARTESIAN_POINT ( 'NONE',  ( 11.99376944390879984, -65.35897423492339442, -17.21195683420090106 ) ) ;
#43750 = CARTESIAN_POINT ( 'NONE',  ( 10.06009413933740149, 32.63977898893389806, -46.27041880991490075 ) ) ;
#43751 = CARTESIAN_POINT ( 'NONE',  ( 73.08495881288720852, 1.096305581841160004, -62.33061120451039727 ) ) ;
#43752 = CARTESIAN_POINT ( 'NONE',  ( 50.70646051152439782, -52.15942487423860285, -52.42739074807799682 ) ) ;
#43753 = CARTESIAN_POINT ( 'NONE',  ( 10.97093567021087068, -64.80530225377253828, -23.22645367378097703 ) ) ;
#43754 = CYLINDRICAL_SURFACE ( 'NONE', #22479, 2.000000000000000888 ) ;
#43755 = EDGE_CURVE ( 'NONE', #34702, #8909, #30867, .T. ) ;
#43756 = ORIENTED_EDGE ( 'NONE', *, *, #2738, .T. ) ;
#43757 = CARTESIAN_POINT ( 'NONE',  ( 64.66447934098378880, 0.9065823421260920112, -70.54525856488079683 ) ) ;
#43758 = CARTESIAN_POINT ( 'NONE',  ( 10.97869545187629825, -63.24704946791390370, -44.74208737706349837 ) ) ;
#43759 = CARTESIAN_POINT ( 'NONE',  ( 68.13393739769769297, 18.72622661238600017, -69.60146707679309941 ) ) ;
#43760 = ORIENTED_EDGE ( 'NONE', *, *, #19864, .F. ) ;
#43761 = CARTESIAN_POINT ( 'NONE',  ( 11.14351459429726177, -63.74727234195290748, -43.82532805256368391 ) ) ;
#43762 = CARTESIAN_POINT ( 'NONE',  ( 18.79008633813485574, -8.139399684649680111, -77.11640214972752005 ) ) ;
#43763 = CARTESIAN_POINT ( 'NONE',  ( 20.98332165578556285, -9.344388009994190725, -49.21715238545373694 ) ) ;
#43764 = EDGE_LOOP ( 'NONE', ( #27986, #17424 ) ) ;
#43765 = SURFACE_STYLE_USAGE ( .BOTH. , #15218 ) ;
#43766 = CARTESIAN_POINT ( 'NONE',  ( -8.866062602303902196, -15.61618894467929941, 7.919999999999963514 ) ) ;
#43767 = CARTESIAN_POINT ( 'NONE',  ( 8.428888865400255170, -13.54532213638748317, -56.59100174228039748 ) ) ;
#43768 = CARTESIAN_POINT ( 'NONE',  ( 53.63393739769619373, 30.88381105532059934, 17.35000000000000142 ) ) ;
#43769 = CARTESIAN_POINT ( 'NONE',  ( 17.77623415669070184, -7.536239600077499823, -69.35616034045709455 ) ) ;
#43770 = DIRECTION ( 'NONE',  ( 0.000000000000000000, 0.000000000000000000, -1.000000000000000000 ) ) ;
#43771 = CARTESIAN_POINT ( 'NONE',  ( 46.75053292986431330, -38.22714621137214408, -56.56697207775517455 ) ) ;
#43772 = ORIENTED_EDGE ( 'NONE', *, *, #22315, .T. ) ;
#43773 = EDGE_CURVE ( 'NONE', #19102, #30849, #32278, .T. ) ;
#43774 = AXIS2_PLACEMENT_3D ( 'NONE', #14468, #2162, #30185 ) ;
#43775 = CARTESIAN_POINT ( 'NONE',  ( 22.89605187407040177, -18.74356829703729943, -68.37054538661389813 ) ) ;
#43776 = CIRCLE ( 'NONE', #37075, 0.9999999999999991118 ) ;
#43777 = CARTESIAN_POINT ( 'NONE',  ( 53.05493175928820193, -49.60024593468599363, -49.10911682558059965 ) ) ;
#43778 = DIRECTION ( 'NONE',  ( 0.000000000000000000, 0.000000000000000000, -1.000000000000000000 ) ) ;
#43779 = CARTESIAN_POINT ( 'NONE',  ( 11.60083912566800102, -21.98623894961669833, -32.14999999999999858 ) ) ;
#43780 = ADVANCED_FACE ( 'NONE', ( #28883 ), #45144, .T. ) ;
#43781 = CARTESIAN_POINT ( 'NONE',  ( 46.93934609751799769, 22.89847016650290001, -75.65554799883719284 ) ) ;
#43782 = DIRECTION ( 'NONE',  ( -0.3863301728269312174, 0.9223605572461961444, 1.110223024625156294E-16 ) ) ;
#43783 = DIRECTION ( 'NONE',  ( 0.000000000000000000, 1.000000000000000000, 0.000000000000000000 ) ) ;
#43784 = CARTESIAN_POINT ( 'NONE',  ( 41.94962124040690554, -44.91063985297350314, -5.752304926970420063 ) ) ;
#43785 = CARTESIAN_POINT ( 'NONE',  ( 12.06856799516559953, 33.91524600913400178, -16.61922514010409913 ) ) ;
#43786 = CARTESIAN_POINT ( 'NONE',  ( 10.52982223945920026, -9.568328661720299166, -74.76978491222729417 ) ) ;
#43787 = CARTESIAN_POINT ( 'NONE',  ( 22.23384466866859910, -12.16604687330790213, -32.14999999999999858 ) ) ;
#43788 = AXIS2_PLACEMENT_3D ( 'NONE', #44845, #40905, #8950 ) ;
#43789 = CARTESIAN_POINT ( 'NONE',  ( 55.86072899227769994, -50.68028847179019891, -75.53713797333620050 ) ) ;
#43791 = DIRECTION ( 'NONE',  ( 0.7071067811865475727, 0.000000000000000000, 0.7071067811865475727 ) ) ;
#43790 = CARTESIAN_POINT ( 'NONE',  ( 0.3088433006440429729, 21.43104923585109844, -7.323220502269159660 ) ) ;
#43792 = CARTESIAN_POINT ( 'NONE',  ( 63.02029346573409185, 0.8838110553206759423, -68.78868353141480441 ) ) ;
#43793 = CARTESIAN_POINT ( 'NONE',  ( 61.22799349397990198, 14.06250502558359905, -47.02344481981909752 ) ) ;
#43794 = B_SPLINE_CURVE_WITH_KNOTS ( 'NONE', 3,
 ( #21260, #1623, #33582, #32518, #49080, #12648, #28347, #28609, #40676, #37006, #41200, #9244, #24405, #16835, #29394, #32783, #8715, #9501 ),
 .UNSPECIFIED., .F., .F.,
 ( 4, 2, 2, 2, 2, 2, 2, 2, 4 ),
 ( 0.000000000000000000, 0.06249999303177191518, 0.1249999860635438304, 0.1874999790953157386, 0.2499999721270876607, 0.3124999651588598049, 0.3749999581906319213, 0.4374999512224040932, 0.4999999442541762096 ),
 .UNSPECIFIED. ) ;
#43795 = EDGE_CURVE ( 'NONE', #49183, #34590, #19862, .T. ) ;
#43796 = CARTESIAN_POINT ( 'NONE',  ( 8.133937397696209715, 8.337936262032100032, -43.74348518090240390 ) ) ;
#43797 = VERTEX_POINT ( 'NONE', #24935 ) ;
#43798 = CARTESIAN_POINT ( 'NONE',  ( 52.83783599233930062, -49.65668728527659681, -48.61330445836559733 ) ) ;
#43799 = CARTESIAN_POINT ( 'NONE',  ( 59.86146244909460279, -45.44095901954209893, -26.83847763191949909 ) ) ;
#43800 = CARTESIAN_POINT ( 'NONE',  ( 16.27309551684129829, -23.60625643615314573, -66.28644551406529217 ) ) ;
#43801 = CARTESIAN_POINT ( 'NONE',  ( 56.57264709847169826, 14.96115542950509969, -26.26398226818550086 ) ) ;
#43802 = CARTESIAN_POINT ( 'NONE',  ( 11.16483992176100060, -10.06508418258009918, -75.50024918233970084 ) ) ;
#43803 = CARTESIAN_POINT ( 'NONE',  ( 52.02481131427630601, 18.54900204977309741, -76.90588458405230199 ) ) ;
#43804 = CARTESIAN_POINT ( 'NONE',  ( 52.72694658191860384, 18.49028550864479925, -48.50421737598679783 ) ) ;
#43805 = CARTESIAN_POINT ( 'NONE',  ( 0.3209249304026170480, -4.754491132419490285, -34.64999999999999858 ) ) ;
#43806 = DIRECTION ( 'NONE',  ( 1.000000000000000000, 0.000000000000000000, 0.000000000000000000 ) ) ;
#43807 = ORIENTED_EDGE ( 'NONE', *, *, #17095, .T. ) ;
#43808 = CIRCLE ( 'NONE', #21192, 22.00000000000000000 ) ;
#43809 = CARTESIAN_POINT ( 'NONE',  ( -11.39236625349550103, 2.585530954890270294, -54.64999999999999858 ) ) ;
#43810 = VECTOR ( 'NONE', #51792, 1000.000000000000000 ) ;
#43811 = CARTESIAN_POINT ( 'NONE',  ( 47.71580729225940587, -54.48068309477200444, -54.87186394391349609 ) ) ;
#43812 = CARTESIAN_POINT ( 'NONE',  ( -18.86606260230360022, -50.61618894467959962, 10.84999999999999964 ) ) ;
#43813 = CARTESIAN_POINT ( 'NONE',  ( 48.42521416700790127, 25.14253336855949783, -60.76348542011150045 ) ) ;
#43814 = CARTESIAN_POINT ( 'NONE',  ( 59.15983391655790058, -28.73665177021000261, -15.68167984968010131 ) ) ;
#43815 = CARTESIAN_POINT ( 'NONE',  ( 71.34424925767550008, 1.265401080857980087, -60.77621068871049204 ) ) ;
#43816 = CARTESIAN_POINT ( 'NONE',  ( -0.4123484725610440105, -45.29119327467250145, -35.12503119152799513 ) ) ;
#43817 = CARTESIAN_POINT ( 'NONE',  ( 72.43519100933379207, 1.033013263524900083, -61.46596897695270201 ) ) ;
#43818 = EDGE_CURVE ( 'NONE', #32526, #11866, #15687, .T. ) ;
#43819 = CARTESIAN_POINT ( 'NONE',  ( 68.13393739769620083, -48.11618894467930119, -73.25000000000000000 ) ) ;
#43820 = CARTESIAN_POINT ( 'NONE',  ( -3.175079596678700433, -15.61618894467929941, 16.85000000000000142 ) ) ;
#43821 = ORIENTED_EDGE ( 'NONE', *, *, #51310, .T. ) ;
#43822 = EDGE_CURVE ( 'NONE', #32096, #17323, #19007, .T. ) ;
#43823 = VERTEX_POINT ( 'NONE', #4789 ) ;
#43824 = DIRECTION ( 'NONE',  ( 0.000000000000000000, 0.000000000000000000, -1.000000000000000000 ) ) ;
#43825 = CARTESIAN_POINT ( 'NONE',  ( 21.08268135459507420, 0.3115492626563509115, -75.56421356237308373 ) ) ;
#43826 = EDGE_LOOP ( 'NONE', ( #18024, #25445, #6542, #16039, #45755 ) ) ;
#43827 = DIRECTION ( 'NONE',  ( 1.000000000000000000, 0.000000000000000000, 0.000000000000000000 ) ) ;
#43828 = CARTESIAN_POINT ( 'NONE',  ( 19.66452008112446492, -22.72169927725052574, -77.86093795788831073 ) ) ;
#43829 = ORIENTED_EDGE ( 'NONE', *, *, #5051, .T. ) ;
#43830 = CARTESIAN_POINT ( 'NONE',  ( 11.02024616950667557, 33.64882680616562993, -23.17060109525836964 ) ) ;
#43831 = CARTESIAN_POINT ( 'NONE',  ( 43.79971744381874998, 6.658519618423869524, -71.32108293267019405 ) ) ;
#43832 = CARTESIAN_POINT ( 'NONE',  ( 60.85636071390069901, 14.48090769567980018, -47.74754960808709825 ) ) ;
#43833 = CARTESIAN_POINT ( 'NONE',  ( 21.51895211384039897, -21.85993273849760143, -46.06579460775299140 ) ) ;
#43834 = TOROIDAL_SURFACE ( 'NONE', #275, 17.39999999999999858, 3.799999999999999822 ) ;
#43835 = CARTESIAN_POINT ( 'NONE',  ( 12.14982466399041705, -22.52872268964002700, -68.17433422315620817 ) ) ;
#43836 = CARTESIAN_POINT ( 'NONE',  ( 14.95255119587064208, -23.45945773958777636, -50.33991548539275129 ) ) ;
#43837 =( NAMED_UNIT ( * ) SI_UNIT ( $, .STERADIAN. ) SOLID_ANGLE_UNIT ( ) );
#43838 = CARTESIAN_POINT ( 'NONE',  ( 60.83746312569630277, -29.08971170939889817, -15.89330470500829939 ) ) ;
#43839 = EDGE_CURVE ( 'NONE', #15227, #3359, #27170, .T. ) ;
#43840 = B_SPLINE_CURVE_WITH_KNOTS ( 'NONE', 3,
 ( #5445, #21402, #41849, #37403, #45791, #9880, #5953, #21911, #14326, #23451, #42375, #30809, #26621, #51010, #34743, #51270, #47347, #11445, #26888, #35271, #19290, #42638, #14586, #27402, #39476, #6472, #50751, #46576, #15368, #35002, #6735, #19026, #22690, #15107, #38709, #14846, #50495, #50239, #2800, #7503, #23195, #31067, #42897, #47094, #18250, #11182, #3312, #39211, #38963, #27148, #46837, #30552, #31322, #10665, #3056, #43403, #30297, #46315, #18771, #34219, #43153, #6992, #10405, #26357, #10923, #7247, #22428, #38438, #2537, #22945, #18516, #34492, #43660, #31834, #16126, #32602, #28165, #23713, #43915, #12728, #20301, #23965, #4333, #51524, #32343, #19803, #35537, #4585, #48362, #27659, #15625, #32087, #35793, #401, #8790, #20556, #3576, #12206, #39985, #8010, #48107, #51776, #44170, #16640, #48628, #657, #20049, #28684, #12458, #44686, #44430, #4077, #36291, #8535, #36553, #40492, #8264, #24743, #36040, #16387, #148, #7765, #24217, #11957, #28427, #40242, #19544, #31577, #47597, #24479, #11697, #39726, #3830, #15880, #47851, #27914, #36817, #22566, #22047, #42251, #10281, #13950, #6350, #45927, #22308, #10017, #38060, #21794, #20820, #25979, #30694, #46456, #33845, #922, #13697, #30431, #10544, #10801, #26243, #46716, #4854, #2155, #1897, #26500, #49861, #38316, #18649, #16916, #32861, #41993, #42516, #34361, #40753, #38582, #50378, #50627, #2676, #48894, #30177 ),
 .UNSPECIFIED., .F., .F.,
 ( 4, 2, 2, 2, 1, 1, 2, 2, 2, 2, 1, 2, 2, 2, 2, 2, 2, 2, 1, 1, 2, 2, 2, 2, 1, 2, 1, 2, 2, 2, 2, 2, 1, 2, 2, 2, 2, 1, 2, 2, 2, 2, 2, 2, 1, 2, 2, 2, 2, 1, 1, 2, 2, 2, 2, 2, 1, 2, 2, 2, 2, 1, 2, 2, 2, 2, 2, 2, 1, 1, 2, 2, 2, 2, 1, 2, 2, 2, 2, 2, 2, 2, 1, 1, 2, 2, 2, 2, 1, 2, 2, 2, 2, 2, 2, 2, 1, 2, 2, 4 ),
 ( 0.000000000000000000, 0.03124999999998254174, 0.04687499999997373629, 0.05468749999996957295, 0.05859374999996754679, 0.06054687499996654065, 0.06152343749996577044, 0.06249999999996499328, 0.09374999999994663991, 0.1093749999999377581, 0.1171874999999337197, 0.1210937499999317768, 0.1230468749999313466, 0.1240234374999307637, 0.1249999999999301947, 0.1562499999999337474, 0.1718749999999354960, 0.1796874999999364675, 0.1835937499999372446, 0.1855468749999378275, 0.1865234374999381883, 0.1874999999999385214, 0.2187499999999658606, 0.2343749999999794609, 0.2421874999999861777, 0.2460937499999892031, 0.2480468749999906741, 0.2490234374999909794, 0.2499999999999912847, 0.2812499999999738542, 0.2968749999999648059, 0.3046874999999603650, 0.3085937499999580891, 0.3105468749999574785, 0.3124999999999568123, 0.3437499999999511502, 0.3593749999999475975, 0.3671874999999458766, 0.3710937499999448774, 0.3730468749999434896, 0.3749999999999420464, 0.4062499999999429345, 0.4218749999999433786, 0.4296874999999437117, 0.4335937499999432676, 0.4355468749999431011, 0.4374999999999428790, 0.4687499999999381051, 0.4843749999999358291, 0.4921874999999355516, 0.4960937499999345524, 0.4980468749999351630, 0.4999999999999357181, 0.5312499999999212852, 0.5468749999999139577, 0.5546874999999096278, 0.5585937499999079625, 0.5605468749999077405, 0.5624999999999075184, 0.5937499999999158451, 0.6093749999999200639, 0.6171874999999220623, 0.6210937499999231726, 0.6230468749999237277, 0.6249999999999242828, 0.6562499999999480416, 0.6718749999999598099, 0.6796874999999658051, 0.6835937499999686917, 0.6855468749999705791, 0.6865234374999714673, 0.6874999999999723554, 0.7187500000000116573, 0.7343750000000320854, 0.7421875000000422995, 0.7460937500000467404, 0.7480468750000479616, 0.7490234375000487388, 0.7500000000000495159, 0.7812500000000650591, 0.7968750000000727196, 0.8046875000000766054, 0.8085937500000784928, 0.8105468750000793809, 0.8115234375000792699, 0.8125000000000791589, 0.8437500000000712763, 0.8593750000000673905, 0.8671875000000652811, 0.8710937500000650591, 0.8730468750000650591, 0.8740234375000658362, 0.8750000000000666134, 0.9062500000000518474, 0.9218750000000451861, 0.9296875000000413003, 0.9335937500000387468, 0.9355468750000369704, 0.9375000000000351941, 1.000000000000000000 ),
 .UNSPECIFIED. ) ;
#43841 = CARTESIAN_POINT ( 'NONE',  ( 63.08005232011709751, 0.8859637708054499683, -62.41593972647849853 ) ) ;
#43842 = CARTESIAN_POINT ( 'NONE',  ( 16.38271474186759846, -23.06229203135920258, -32.72202640798520434 ) ) ;
#43843 = CARTESIAN_POINT ( 'NONE',  ( 10.72260735920611907, -19.77484646530637846, -37.24448631176660740 ) ) ;
#43844 = CARTESIAN_POINT ( 'NONE',  ( 41.12836154737230032, 13.96087487792660120, -5.806220427399999551 ) ) ;
#43845 = ADVANCED_FACE ( 'NONE', ( #14461 ), #38720, .T. ) ;
#43846 = CIRCLE ( 'NONE', #12057, 0.9999999999568487397 ) ;
#43847 = CARTESIAN_POINT ( 'NONE',  ( -0.9360626029568490658, -15.61618894436409732, -14.69000000030820985 ) ) ;
#43848 = CARTESIAN_POINT ( 'NONE',  ( 84.13361756236649569, -43.99383155051249616, -46.96659941728370313 ) ) ;
#43849 = CARTESIAN_POINT ( 'NONE',  ( 63.62896973943209389, 1.416241615474740145, -69.07296579632759403 ) ) ;
#43850 = CARTESIAN_POINT ( 'NONE',  ( 11.21911071231070167, -8.995977515910739797, -38.80439020934399252 ) ) ;
#43851 = ORIENTED_EDGE ( 'NONE', *, *, #8119, .F. ) ;
#43852 = CARTESIAN_POINT ( 'NONE',  ( 52.88967915934290431, -49.60939747366519725, -27.87881832530509740 ) ) ;
#43853 = CARTESIAN_POINT ( 'NONE',  ( 15.78755803685880110, -51.00425289770759463, -20.74412215666150061 ) ) ;
#43854 = CARTESIAN_POINT ( 'NONE',  ( 24.04790590996992705, -15.78420839348370208, -39.51442343626069231 ) ) ;
#43855 = CARTESIAN_POINT ( 'NONE',  ( 22.04683847007901321, -19.02420019749379065, -56.61945810151985370 ) ) ;
#43856 = DIRECTION ( 'NONE',  ( 1.000000000000000000, 0.000000000000000000, 0.000000000000000000 ) ) ;
#43857 = ORIENTED_EDGE ( 'NONE', *, *, #23985, .F. ) ;
#43858 = CARTESIAN_POINT ( 'NONE',  ( -5.701502996861630201, -46.97469897207449918, -5.417034474275260081 ) ) ;
#43859 = DIRECTION ( 'NONE',  ( -1.000000000000000000, 0.000000000000000000, 0.000000000000000000 ) ) ;
#43860 = DIRECTION ( 'NONE',  ( 0.6888026391158329487, 0.7071067811865494601, 0.1598465650148944150 ) ) ;
#43861 = CARTESIAN_POINT ( 'NONE',  ( 63.06902243323368396, 0.9940695285616559795, -62.44811160372290004 ) ) ;
#43862 = CARTESIAN_POINT ( 'NONE',  ( 57.37674695049749829, -50.61618894467930119, -53.87125040983160318 ) ) ;
#43863 = CARTESIAN_POINT ( 'NONE',  ( 40.74969953824990654, 13.47525508662189964, -4.809312831994500215 ) ) ;
#43864 = CARTESIAN_POINT ( 'NONE',  ( 20.29261341095602944, -21.02750385110190834, -64.74448845417677489 ) ) ;
#43865 = CARTESIAN_POINT ( 'NONE',  ( 64.00995881370980101, 1.028300555801489935, -61.29114157291949994 ) ) ;
#43866 = DIRECTION ( 'NONE',  ( -0.8732394366197182567, 0.4872913772396111343, 0.000000000000000000 ) ) ;
#43867 = CARTESIAN_POINT ( 'NONE',  ( 11.27215316695904335, -9.290104087649041276, -75.08404200567380826 ) ) ;
#43868 = AXIS2_PLACEMENT_3D ( 'NONE', #23704, #3569, #4323 ) ;
#43869 = DIRECTION ( 'NONE',  ( 1.000000000000000000, 0.000000000000000000, 0.000000000000000000 ) ) ;
#43870 = CARTESIAN_POINT ( 'NONE',  ( 17.37473796128360348, -52.76520172820870158, -76.12661215459480957 ) ) ;
#43871 = AXIS2_PLACEMENT_3D ( 'NONE', #48548, #21524, #25193 ) ;
#43872 = CARTESIAN_POINT ( 'NONE',  ( 13.37557373594179921, -8.695341868789380868, -62.44661944738240322 ) ) ;
#43873 = CARTESIAN_POINT ( 'NONE',  ( 15.00527006812512987, 19.40301060417740686, -20.65452753591024759 ) ) ;
#43874 =( BOUNDED_CURVE ( )  B_SPLINE_CURVE ( 3, ( #48839, #44383, #45611, #25670 ),
 .UNSPECIFIED., .F., .T. ) 
 B_SPLINE_CURVE_WITH_KNOTS ( ( 4, 4 ),
 ( 5.497787143782140618, 6.283185307179584456 ),
 .UNSPECIFIED. ) 
 CURVE ( )  GEOMETRIC_REPRESENTATION_ITEM ( )  RATIONAL_B_SPLINE_CURVE ( ( 1.000000000000000000, 0.9492530216741915661, 0.9492530216741915661, 1.000000000000000000 ) ) 
 REPRESENTATION_ITEM ( '' )  );
#43875 = CARTESIAN_POINT ( 'NONE',  ( 63.29959049205589849, 1.031491003832160080, -62.11015851666019927 ) ) ;
#43876 = ORIENTED_EDGE ( 'NONE', *, *, #10592, .F. ) ;
#43877 = CARTESIAN_POINT ( 'NONE',  ( 8.807322927776979782, 32.00291607516390258, -46.67042760097810117 ) ) ;
#43878 = CARTESIAN_POINT ( 'NONE',  ( 22.74436002974624671, -17.09899314720811248, -34.52302736558711160 ) ) ;
#43879 = CARTESIAN_POINT ( 'NONE',  ( 9.311115770169109851, -12.88060009992239863, -81.23899999999999011 ) ) ;
#43880 = VERTEX_POINT ( 'NONE', #39859 ) ;
#43881 = CARTESIAN_POINT ( 'NONE',  ( 17.49786823416480175, 21.15196775986840194, -76.02269426304029309 ) ) ;
#43882 = EDGE_CURVE ( 'NONE', #26463, #21257, #50863, .T. ) ;
#43883 = ORIENTED_EDGE ( 'NONE', *, *, #20038, .F. ) ;
#43884 = AXIS2_PLACEMENT_3D ( 'NONE', #27597, #47539, #11635 ) ;
#43885 = MANIFOLD_SOLID_BREP ( 'Stock-MAS-691-1', #26822 ) ;
#43886 = ORIENTED_EDGE ( 'NONE', *, *, #34037, .T. ) ;
#43887 = DIRECTION ( 'NONE',  ( 1.000000000000000000, 0.000000000000000000, 0.000000000000000000 ) ) ;
#43888 = CARTESIAN_POINT ( 'NONE',  ( 22.50961056586849907, -11.15336966704510147, -81.23899999999999011 ) ) ;
#43889 = EDGE_CURVE ( 'NONE', #29281, #17323, #8366, .T. ) ;
#43890 = AXIS2_PLACEMENT_3D ( 'NONE', #43558, #12613, #4480 ) ;
#43891 = CARTESIAN_POINT ( 'NONE',  ( 11.27236315750194784, -9.289945223521018036, -73.08399817834765599 ) ) ;
#43892 = ORIENTED_EDGE ( 'NONE', *, *, #984, .T. ) ;
#43893 = CARTESIAN_POINT ( 'NONE',  ( 12.36320305029179956, 33.31445045633500257, -15.76422791923680045 ) ) ;
#43894 = ORIENTED_EDGE ( 'NONE', *, *, #157, .F. ) ;
#43895 = PLANE ( 'NONE',  #7694 ) ;
#43896 = AXIS2_PLACEMENT_3D ( 'NONE', #28479, #8067, #28216 ) ;
#43897 = ORIENTED_EDGE ( 'NONE', *, *, #29898, .F. ) ;
#43898 = ORIENTED_EDGE ( 'NONE', *, *, #24481, .F. ) ;
#43899 = CARTESIAN_POINT ( 'NONE',  ( 44.67500051388495308, 1.933004323653375156, -44.55553664676357073 ) ) ;
#43900 = CARTESIAN_POINT ( 'NONE',  ( 46.53687296277449548, -53.33479509908829641, -76.10218428122850298 ) ) ;
#43901 = CARTESIAN_POINT ( 'NONE',  ( 61.23319982858129862, 14.25045713433570072, -47.51874276278900311 ) ) ;
#43902 = EDGE_CURVE ( 'NONE', #14173, #40777, #28292, .T. ) ;
#43903 = CARTESIAN_POINT ( 'NONE',  ( 22.83044329432877362, -14.62138923286050840, -40.40589576860565302 ) ) ;
#43904 = AXIS2_PLACEMENT_3D ( 'NONE', #4772, #11879, #31497 ) ;
#43905 = CARTESIAN_POINT ( 'NONE',  ( 41.38588534151550391, -44.01253888900150457, -3.641004148972040166 ) ) ;
#43906 = CARTESIAN_POINT ( 'NONE',  ( -3.204312279287770515, 17.11425786164920027, -4.550063412008999997 ) ) ;
#43907 = CARTESIAN_POINT ( 'NONE',  ( 0.8044204053657370013, -22.50679809325820102, -34.68801049095919353 ) ) ;
#43908 = CARTESIAN_POINT ( 'NONE',  ( 58.32293069149620379, 14.27849980386080020, -26.32855658276989885 ) ) ;
#43909 = CARTESIAN_POINT ( 'NONE',  ( 16.10092966880469945, -7.768535876849650634, -66.78616676534149121 ) ) ;
#43910 = ORIENTED_EDGE ( 'NONE', *, *, #19555, .T. ) ;
#43911 = AXIS2_PLACEMENT_3D ( 'NONE', #144, #30805, #15622 ) ;
#43912 = CARTESIAN_POINT ( 'NONE',  ( 23.32430482491560042, -49.33365190531349498, -34.64999999999999858 ) ) ;
#43913 = CARTESIAN_POINT ( 'NONE',  ( 11.83825639606079960, 33.81473130967069807, -45.42565952151209530 ) ) ;
#43914 = CARTESIAN_POINT ( 'NONE',  ( 72.63216195444580592, 1.261444690199509999, -69.51221393975839646 ) ) ;
#43915 = CARTESIAN_POINT ( 'NONE',  ( 44.04477319376010769, -39.95831334196088847, -66.44292113288734924 ) ) ;
#43916 = VECTOR ( 'NONE', #12418, 1000.000000000000000 ) ;
#43917 = FACE_OUTER_BOUND ( 'NONE', #50971, .T. ) ;
#43918 = CARTESIAN_POINT ( 'NONE',  ( 13.04450223014749888, 18.79195992918549862, -21.04428000939609689 ) ) ;
#43919 = CARTESIAN_POINT ( 'NONE',  ( -0.4410626023037880206, -27.49517073325580085, -35.14999999999999858 ) ) ;
#43920 = CARTESIAN_POINT ( 'NONE',  ( 48.46825551001710153, -54.10363359004039552, -54.77876380330509676 ) ) ;
#43921 = CARTESIAN_POINT ( 'NONE',  ( 16.13393739769620083, -15.61618894467929941, -32.14999999999999858 ) ) ;
#43922 = DIRECTION ( 'NONE',  ( 0.000000000000000000, 0.000000000000000000, -1.000000000000000000 ) ) ;
#43923 = FACE_BOUND ( 'NONE', #31869, .T. ) ;
#43924 = CARTESIAN_POINT ( 'NONE',  ( 22.90093739769620029, -15.61618894467913243, -28.45282021618999835 ) ) ;
#43925 = ORIENTED_EDGE ( 'NONE', *, *, #5846, .F. ) ;
#43926 = CARTESIAN_POINT ( 'NONE',  ( 13.04303129394959981, -22.06172762676530041, -31.70967419469809201 ) ) ;
#43927 = CARTESIAN_POINT ( 'NONE',  ( 22.90101955563642733, -15.61618902498797290, -36.84717743668400658 ) ) ;
#43928 = EDGE_LOOP ( 'NONE', ( #17200, #37120, #48797, #22795 ) ) ;
#43929 = CARTESIAN_POINT ( 'NONE',  ( 71.54199927891758648, 1.099344084866040072, -70.54350063839000029 ) ) ;
#43930 = CARTESIAN_POINT ( 'NONE',  ( 60.99523858508899821, -45.40662299616879949, -47.17226579437180334 ) ) ;
#43931 = CARTESIAN_POINT ( 'NONE',  ( 47.81335647231890107, -54.39749252969859583, -54.71582838609030119 ) ) ;
#43932 = FACE_OUTER_BOUND ( 'NONE', #2430, .T. ) ;
#43934 = CARTESIAN_POINT ( 'NONE',  ( 22.46012340461659917, -10.75453950994439722, -35.58399600476455760 ) ) ;
#43933 = CARTESIAN_POINT ( 'NONE',  ( 42.21125607557041803, 8.554746773914486013, -75.31133717877361278 ) ) ;
#43935 = DIRECTION ( 'NONE',  ( 0.000000000000000000, 0.000000000000000000, 1.000000000000000000 ) ) ;
#43936 = CARTESIAN_POINT ( 'NONE',  ( 56.52536539877749533, 19.51942783438209972, -53.84278118897309895 ) ) ;
#43937 = ORIENTED_EDGE ( 'NONE', *, *, #48216, .T. ) ;
#43938 = CARTESIAN_POINT ( 'NONE',  ( 28.13393739769619728, -22.54439217495490055, -35.14999999999999858 ) ) ;
#43939 = CONICAL_SURFACE ( 'NONE', #388, 0.7349999999999987654, 0.06981317007977388966 ) ;
#43940 = EDGE_CURVE ( 'NONE', #37903, #38406, #4990, .T. ) ;
#43941 = VERTEX_POINT ( 'NONE', #4207 ) ;
#43942 = DIRECTION ( 'NONE',  ( 0.000000000000000000, 0.000000000000000000, 1.000000000000000000 ) ) ;
#43943 = CARTESIAN_POINT ( 'NONE',  ( 53.55317832401189548, -49.41998711946010303, -49.22667755100069797 ) ) ;
#43944 = CARTESIAN_POINT ( 'NONE',  ( 55.92234169269686106, 14.66394275432020144, -25.39467821330401165 ) ) ;
#43945 = CARTESIAN_POINT ( 'NONE',  ( 76.39108789613560191, -16.41352413642167818, -12.75810673299934628 ) ) ;
#43946 = ORIENTED_EDGE ( 'NONE', *, *, #4116, .T. ) ;
#43947 = ORIENTED_EDGE ( 'NONE', *, *, #5512, .T. ) ;
#43948 = CARTESIAN_POINT ( 'NONE',  ( -0.1840543581862938427, 14.24433273476873829, -34.92644969713277447 ) ) ;
#43949 = AXIS2_PLACEMENT_3D ( 'NONE', #43145, #19537, #19283 ) ;
#43950 = CARTESIAN_POINT ( 'NONE',  ( 57.25641887048840317, -45.13136270895589774, -25.31435934810820143 ) ) ;
#43951 = CARTESIAN_POINT ( 'NONE',  ( 56.51998432061900246, -50.75157408873379694, -53.72896419663980083 ) ) ;
#43952 = CARTESIAN_POINT ( 'NONE',  ( 15.16221966815624889, -8.902689794812856050, -45.90713210071369588 ) ) ;
#43953 = CARTESIAN_POINT ( 'NONE',  ( 59.93368784167530805, -1.201354282306859922, -16.01185523896749885 ) ) ;
#43954 = ORIENTED_EDGE ( 'NONE', *, *, #10213, .F. ) ;
#43955 = DIRECTION ( 'NONE',  ( 0.000000000000000000, 0.000000000000000000, 1.000000000000000000 ) ) ;
#43956 = CARTESIAN_POINT ( 'NONE',  ( 53.72304193977469566, -50.62044000525840204, -76.82797321725880124 ) ) ;
#43957 = LINE ( 'NONE', #36333, #19310 ) ;
#43958 = CARTESIAN_POINT ( 'NONE',  ( 69.73393739769620936, 11.23736444591397543, -61.59644660940672622 ) ) ;
#43959 = CARTESIAN_POINT ( 'NONE',  ( 11.20381621344150069, -9.510400486163490541, -49.29627689082150255 ) ) ;
#43960 = EDGE_CURVE ( 'NONE', #42020, #32963, #21540, .T. ) ;
#43961 = CARTESIAN_POINT ( 'NONE',  ( 12.53340094288019912, -50.34701036924130335, -21.18850769734029882 ) ) ;
#43962 = EDGE_CURVE ( 'NONE', #33996, #22272, #48491, .T. ) ;
#43963 = CARTESIAN_POINT ( 'NONE',  ( -18.86606260230360022, -50.61618894467959962, 16.85000000000000142 ) ) ;
#43964 = CARTESIAN_POINT ( 'NONE',  ( 66.23540447448814916, -49.95860450174473044, -71.35146707679193412 ) ) ;
#43965 = CARTESIAN_POINT ( 'NONE',  ( 61.04011644851190255, -45.35928274206209920, -46.86308394475349814 ) ) ;
#43966 = CARTESIAN_POINT ( 'NONE',  ( 9.366488261363459245, -15.61629045172390029, -39.45282021618999835 ) ) ;
#43967 = CARTESIAN_POINT ( 'NONE',  ( 21.96868942811769898, -19.57828787301799878, -53.03706054135149373 ) ) ;
#43968 = AXIS2_PLACEMENT_3D ( 'NONE', #2925, #20950, #17040 ) ;
#43969 = DIRECTION ( 'NONE',  ( 0.000000000000000000, 0.000000000000000000, 1.000000000000000000 ) ) ;
#43970 = ORIENTED_EDGE ( 'NONE', *, *, #40051, .F. ) ;
#43971 = AXIS2_PLACEMENT_3D ( 'NONE', #28152, #31823, #19791 ) ;
#43972 = CARTESIAN_POINT ( 'NONE',  ( 13.48116118032930011, -51.59709463796549755, -74.36013246831049628 ) ) ;
#43973 = CARTESIAN_POINT ( 'NONE',  ( 47.38854743227360444, -54.66225796327380237, -54.75946254694029847 ) ) ;
#43974 = CARTESIAN_POINT ( 'NONE',  ( 0.2321907996226789950, 19.54381078690260054, -34.65604112956820160 ) ) ;
#43975 = AXIS2_PLACEMENT_3D ( 'NONE', #47095, #3313, #11446 ) ;
#43976 = DIRECTION ( 'NONE',  ( 0.000000000000000000, 0.000000000000000000, -1.000000000000000000 ) ) ;
#43977 = CARTESIAN_POINT ( 'NONE',  ( 60.87559839016541474, -45.45153674070272842, -47.11203263457593948 ) ) ;
#43978 = CARTESIAN_POINT ( 'NONE',  ( 17.01966338078927876, -8.849178626785063173, -75.99446377898397031 ) ) ;
#43979 = CARTESIAN_POINT ( 'NONE',  ( 11.74201408115419909, 34.19078560508950204, -18.09919823649679671 ) ) ;
#43980 = CARTESIAN_POINT ( 'NONE',  ( 72.83009333885360093, 0.9561296872639739597, -69.38553930450309792 ) ) ;
#43982 = CARTESIAN_POINT ( 'NONE',  ( 8.222958677519082826, -16.65189219951969690, -74.46600179554452836 ) ) ;
#43981 = CARTESIAN_POINT ( 'NONE',  ( 83.89200044194980421, -48.61618894467930119, -53.92796738110899923 ) ) ;
#43983 = CARTESIAN_POINT ( 'NONE',  ( 4.773435940454120008, -58.71549427862700554, -13.16255389817539978 ) ) ;
#43984 = FACE_OUTER_BOUND ( 'NONE', #8756, .T. ) ;
#43985 = CARTESIAN_POINT ( 'NONE',  ( 49.69686147736450010, 22.42393137654260116, -54.99388098410930326 ) ) ;
#43986 = VERTEX_POINT ( 'NONE', #16007 ) ;
#43987 = CARTESIAN_POINT ( 'NONE',  ( 52.89232551375209113, -49.65864638672599796, -48.97387503448329937 ) ) ;
#43988 = ORIENTED_EDGE ( 'NONE', *, *, #44165, .T. ) ;
#43989 = AXIS2_PLACEMENT_3D ( 'NONE', #14611, #26128, #22195 ) ;
#43990 = CARTESIAN_POINT ( 'NONE',  ( 41.86227561628311378, 6.227911795772825165, -80.99113711912313818 ) ) ;
#43991 = CARTESIAN_POINT ( 'NONE',  ( -18.49575789335964515, 19.89349176177682210, 16.21999999999999886 ) ) ;
#43992 = CARTESIAN_POINT ( 'NONE',  ( 56.84932596551109185, -50.65659107673559447, -53.85230338955700091 ) ) ;
#43994 = CARTESIAN_POINT ( 'NONE',  ( 54.97499875616310305, 15.98981385143299860, -26.07547149580530288 ) ) ;
#43993 = CARTESIAN_POINT ( 'NONE',  ( 82.68714621053810276, 13.87897394514460103, -46.76937705306080062 ) ) ;
#43995 = CARTESIAN_POINT ( 'NONE',  ( 13.21370044366810070, -9.196315516880730456, -57.81693366461269079 ) ) ;
#43996 = CARTESIAN_POINT ( 'NONE',  ( 53.27384017177119802, 18.28364788282440045, -49.18478595043859514 ) ) ;
#43997 = CARTESIAN_POINT ( 'NONE',  ( 56.98602350126559912, -45.17932659337360235, -17.71533550764939591 ) ) ;
#43998 = DIRECTION ( 'NONE',  ( -1.000000000000000000, 0.000000000000000000, 0.000000000000000000 ) ) ;
#43999 = VECTOR ( 'NONE', #48242, 1000.000000000000000 ) ;
#44000 = ORIENTED_EDGE ( 'NONE', *, *, #35243, .T. ) ;
#44001 = ADVANCED_FACE ( 'NONE', ( #12595 ), #24091, .T. ) ;
#44002 = CARTESIAN_POINT ( 'NONE',  ( 23.15260118800880207, -12.10547580035419912, -47.13987186156389697 ) ) ;
#44003 = ORIENTED_EDGE ( 'NONE', *, *, #31307, .T. ) ;
#44004 = ADVANCED_FACE ( 'NONE', ( #36169 ), #4463, .T. ) ;
#44005 = CARTESIAN_POINT ( 'NONE',  ( 11.11465761659180096, -65.15671412701409793, -17.59315288542880040 ) ) ;
#44006 = CARTESIAN_POINT ( 'NONE',  ( 11.05731942293660097, 33.25945548349249492, -45.88168350577869603 ) ) ;
#44007 = CARTESIAN_POINT ( 'NONE',  ( 18.51615658030550904, 20.07812231642038370, -15.71022044314043775 ) ) ;
#44008 = CARTESIAN_POINT ( 'NONE',  ( 48.16430552237229534, -54.25377568305749776, -54.81723493473039355 ) ) ;
#44009 = CARTESIAN_POINT ( 'NONE',  ( 11.62036812317445822, -65.37374231276770331, -22.52863453705835894 ) ) ;
#44010 = CARTESIAN_POINT ( 'NONE',  ( 51.29176633094323279, 3.460026447682412964, -76.59668190568126533 ) ) ;
#44011 = AXIS2_PLACEMENT_3D ( 'NONE', #39853, #3959, #24604 ) ;
#44012 = EDGE_LOOP ( 'NONE', ( #39979, #2877, #7019, #8300 ) ) ;
#44013 = CARTESIAN_POINT ( 'NONE',  ( 12.16981617636350066, 18.81688479155219795, -21.14999999999999858 ) ) ;
#44014 = AXIS2_PLACEMENT_3D ( 'NONE', #19355, #47159, #11246 ) ;
#44015 = CARTESIAN_POINT ( 'NONE',  ( 11.13393739769619906, -63.49867051491490599, -43.75823411798670293 ) ) ;
#44016 = CARTESIAN_POINT ( 'NONE',  ( 68.13393739769814772, 19.38381105532029736, -71.50000000000200373 ) ) ;
#44017 = ORIENTED_EDGE ( 'NONE', *, *, #39671, .T. ) ;
#44018 = CARTESIAN_POINT ( 'NONE',  ( 11.32941444270682751, -64.39195768723817537, -44.31826145974155651 ) ) ;
#44019 = CARTESIAN_POINT ( 'NONE',  ( 56.89024914083419304, 19.26467303738039760, -53.06448611529630455 ) ) ;
#44020 = FACE_OUTER_BOUND ( 'NONE', #38517, .T. ) ;
#44021 = LINE ( 'NONE', #15724, #29591 ) ;
#44022 = ORIENTED_EDGE ( 'NONE', *, *, #46527, .F. ) ;
#44023 = CARTESIAN_POINT ( 'NONE',  ( 23.04646110145052873, -19.60031946873696995, -35.67433263960586487 ) ) ;
#44024 = CARTESIAN_POINT ( 'NONE',  ( 16.13393739769620083, -45.61618894467940066, -62.64999999999999858 ) ) ;
#44025 = DIRECTION ( 'NONE',  ( 0.000000000000000000, 0.000000000000000000, 1.000000000000000000 ) ) ;
#44026 = CARTESIAN_POINT ( 'NONE',  ( 51.49741897520730305, 20.33382311736169967, -51.82318133733109988 ) ) ;
#44027 = CARTESIAN_POINT ( 'NONE',  ( 23.98482941094870213, -18.13535838165310210, -71.89116613449300530 ) ) ;
#44028 = FACE_OUTER_BOUND ( 'NONE', #8825, .T. ) ;
#44029 = DIRECTION ( 'NONE',  ( 1.000000000000000000, 0.000000000000000000, 0.000000000000000000 ) ) ;
#44030 = EDGE_CURVE ( 'NONE', #23138, #8243, #4795, .T. ) ;
#44031 = ORIENTED_EDGE ( 'NONE', *, *, #12481, .F. ) ;
#44032 = CARTESIAN_POINT ( 'NONE',  ( 20.96026664345949797, -21.29185981398060079, -62.50834448790610054 ) ) ;
#44033 = LINE ( 'NONE', #31693, #38112 ) ;
#44034 = CARTESIAN_POINT ( 'NONE',  ( 11.44367971890009983, -21.85319165794779650, -32.14999999999999858 ) ) ;
#44035 = CIRCLE ( 'NONE', #22162, 16.00000000000000000 ) ;
#44036 = CARTESIAN_POINT ( 'NONE',  ( 47.21535380273969906, 23.31245928922829691, -75.00416199656089589 ) ) ;
#44037 = CARTESIAN_POINT ( 'NONE',  ( 71.33393739769650210, 1.396834109478129804, -61.06337307536569625 ) ) ;
#44038 = CARTESIAN_POINT ( 'NONE',  ( 22.90079931266048874, -15.61618915558698184, -42.84717230777439312 ) ) ;
#44039 = CARTESIAN_POINT ( 'NONE',  ( 11.95767227754359929, 33.76040311825810392, -16.37738641794519978 ) ) ;
#44040 = CONICAL_SURFACE ( 'NONE', #29766, 55.50000000000000711, 1.262743545771120246 ) ;
#44041 = CARTESIAN_POINT ( 'NONE',  ( 15.09046434425009942, -7.437320765297320335, -70.96727622117339251 ) ) ;
#44042 = VECTOR ( 'NONE', #1413, 1000.000000000000000 ) ;
#44043 = CARTESIAN_POINT ( 'NONE',  ( 56.23763027956269411, -50.62070442378890078, -75.67790624608100813 ) ) ;
#44045 = CYLINDRICAL_SURFACE ( 'NONE', #23042, 1.999999999999998224 ) ;
#44044 = FILL_AREA_STYLE ('',( #12863 ) ) ;
#44046 = CARTESIAN_POINT ( 'NONE',  ( 63.10653712364238999, 0.8879664753683469414, -68.92499589875220067 ) ) ;
#44047 = CARTESIAN_POINT ( 'NONE',  ( 61.36576913129360378, 13.98029824516259900, -46.78307081367769626 ) ) ;
#44048 = CARTESIAN_POINT ( 'NONE',  ( 64.08038400710292137, 11.23736444591397543, -64.04999999999999716 ) ) ;
#44049 = VERTEX_POINT ( 'NONE', #24352 ) ;
#44050 = CARTESIAN_POINT ( 'NONE',  ( 53.26660255314480708, -49.43204447085090436, -48.79175800379049832 ) ) ;
#44051 = CARTESIAN_POINT ( 'NONE',  ( 57.35811193301260147, -45.61648094041229484, -26.19463098886150476 ) ) ;
#44052 = CARTESIAN_POINT ( 'NONE',  ( 57.55751162049570269, -50.09049722528730086, -52.57651812429949700 ) ) ;
#44053 = CARTESIAN_POINT ( 'NONE',  ( 56.93939532337000031, 14.49262922001920018, -26.16865613188059925 ) ) ;
#44054 = CARTESIAN_POINT ( 'NONE',  ( 9.705356321231780825, -19.38182821955269830, -71.06398904277699557 ) ) ;
#44055 = CARTESIAN_POINT ( 'NONE',  ( 50.87835696893989734, 18.59755892215100204, -76.22533640045350012 ) ) ;
#44056 = CARTESIAN_POINT ( 'NONE',  ( 52.79145156329050081, 18.45098357012509993, -48.63146327739730168 ) ) ;
#44057 = CARTESIAN_POINT ( 'NONE',  ( 71.21254218222989607, 1.330484379554840002, -70.49093568668439502 ) ) ;
#44058 = CARTESIAN_POINT ( 'NONE',  ( 68.13393739769620083, 16.88381105532069881, -71.50000000000000000 ) ) ;
#44059 = ORIENTED_EDGE ( 'NONE', *, *, #35261, .F. ) ;
#44060 = ADVANCED_FACE ( 'NONE', ( #40366 ), #8202, .F. ) ;
#44061 = DIRECTION ( 'NONE',  ( 0.2771081164311154366, 0.6505467637364714673, -0.7071067811865496822 ) ) ;
#44062 = EDGE_CURVE ( 'NONE', #2875, #19986, #49245, .T. ) ;
#44063 = CARTESIAN_POINT ( 'NONE',  ( 47.65526630185220114, -54.48436720726729732, -54.69071458794790175 ) ) ;
#44064 = DIRECTION ( 'NONE',  ( 0.000000000000000000, 0.000000000000000000, -1.000000000000000000 ) ) ;
#44065 = PLANE ( 'NONE',  #22731 ) ;
#44066 = CARTESIAN_POINT ( 'NONE',  ( 59.16375522681380517, -28.11079332067949821, -15.65965516856539885 ) ) ;
#44068 = EDGE_CURVE ( 'NONE', #16929, #51296, #43339, .T. ) ;
#44067 = CARTESIAN_POINT ( 'NONE',  ( 71.47612964547808190, 0.8925687589132640376, -60.66703147076970737 ) ) ;
#44069 = CARTESIAN_POINT ( 'NONE',  ( 2.557755973795889926, -25.18888510921449964, -34.65000333055159842 ) ) ;
#44070 = CARTESIAN_POINT ( 'NONE',  ( 72.43412257677050547, 1.117804454683279936, -61.47169494157739678 ) ) ;
#44071 = AXIS2_PLACEMENT_3D ( 'NONE', #39159, #27091, #49217 ) ;
#44072 = FACE_OUTER_BOUND ( 'NONE', #14760, .T. ) ;
#44073 = EDGE_CURVE ( 'NONE', #20360, #16042, #33782, .T. ) ;
#44074 = CARTESIAN_POINT ( 'NONE',  ( 65.02006347151939281, 1.101170701158060039, -70.72594205704909598 ) ) ;
#44075 = ORIENTED_EDGE ( 'NONE', *, *, #19768, .T. ) ;
#44076 = ORIENTED_EDGE ( 'NONE', *, *, #50994, .T. ) ;
#44077 = CARTESIAN_POINT ( 'NONE',  ( 71.33393739769799424, 10.88381105532070059, -61.45000000000079865 ) ) ;
#44078 = CARTESIAN_POINT ( 'NONE',  ( 0.1375253771463843255, -45.94887013623939964, -34.68482877647384299 ) ) ;
#44079 = ORIENTED_EDGE ( 'NONE', *, *, #4651, .T. ) ;
#44081 = B_SPLINE_CURVE_WITH_KNOTS ( 'NONE', 3,
 ( #4291, #36254, #365, #31542, #19508, #32302, #19248, #43371, #3795, #51488, #51237, #16346, #39948, #43878, #7975, #28384, #7463, #31797, #44133, #15328, #31281, #28127, #51737, #23417, #35498, #39438, #15588, #43627, #7730, #23673, #19764, #35755, #15832 ),
 .UNSPECIFIED., .F., .F.,
 ( 4, 2, 1, 1, 1, 1, 1, 2, 2, 2, 2, 2, 2, 2, 2, 2, 2, 2, 4 ),
 ( 0.4999976081416900864, 0.5002417499345896967, 0.5004858917274892516, 0.5009741753132884723, 0.5019507424848870247, 0.5039038768280834635, 0.5078101455144765630, 0.5156226828872626511, 0.5312477576328348272, 0.5624979071239791795, 0.6249982061062677730, 0.6874985050885564775, 0.7499988040708451820, 0.8124991030531336644, 0.8749994020354223689, 0.9062495515265667212, 0.9374997010177110734, 0.9687498505088556477, 1.000000000000000000 ),
 .UNSPECIFIED. ) ;
#44080 = CARTESIAN_POINT ( 'NONE',  ( 11.93218508669420075, -65.12546966291930062, -45.62051050307170641 ) ) ;
#44082 = CARTESIAN_POINT ( 'NONE',  ( 56.40194557720492696, 19.55619987700153217, -74.41780141112559477 ) ) ;
#44083 = VERTEX_POINT ( 'NONE', #29593 ) ;
#44084 = CARTESIAN_POINT ( 'NONE',  ( 10.97815053533537544, 33.58448697120250870, -23.21825472827888959 ) ) ;
#44085 = CARTESIAN_POINT ( 'NONE',  ( 17.96595504107426677, 1.226104548012931339, -34.77490583097451804 ) ) ;
#44086 = CIRCLE ( 'NONE', #28156, 4.649999999999999467 ) ;
#44087 = CARTESIAN_POINT ( 'NONE',  ( 23.52669840957137026, -18.53768046102651468, -65.62753320149030856 ) ) ;
#44088 = CARTESIAN_POINT ( 'NONE',  ( 20.71434839502420289, -22.47202989612290125, -42.10484805457200252 ) ) ;
#44089 = AXIS2_PLACEMENT_3D ( 'NONE', #17866, #26491, #33837 ) ;
#44090 = CARTESIAN_POINT ( 'NONE',  ( 45.15012441416580202, 2.064121025657089881, -35.08176457245370017 ) ) ;
#44091 = CARTESIAN_POINT ( 'NONE',  ( 14.37168384308351676, -23.35179302556277037, -50.36354003200006701 ) ) ;
#44092 = DIRECTION ( 'NONE',  ( 0.000000000000000000, 0.000000000000000000, 1.000000000000000000 ) ) ;
#44093 = EDGE_CURVE ( 'NONE', #42488, #50414, #32405, .T. ) ;
#44094 = VERTEX_POINT ( 'NONE', #10215 ) ;
#44095 = CARTESIAN_POINT ( 'NONE',  ( 12.35403558730510021, -65.44380354427669033, -23.29258724847819906 ) ) ;
#44096 = CARTESIAN_POINT ( 'NONE',  ( 19.68464592544490088, -9.066443701053138682, -35.89078365052999686 ) ) ;
#44097 = CARTESIAN_POINT ( 'NONE',  ( 42.22416114274249566, 14.21574947835240010, -6.646926284411279973 ) ) ;
#44098 = CIRCLE ( 'NONE', #45789, 17.06999999999999673 ) ;
#44099 = CARTESIAN_POINT ( 'NONE',  ( 14.79004452048550000, 21.13934752900200209, -76.01805773991210913 ) ) ;
#44100 = CARTESIAN_POINT ( 'NONE',  ( 11.85758210885778574, -22.34943485980089761, -60.47261281821599255 ) ) ;
#44101 = CARTESIAN_POINT ( 'NONE',  ( 84.42643369580130752, -43.29356274104110724, -47.38360074682189804 ) ) ;
#44102 = CIRCLE ( 'NONE', #8127, 2.499999999999998668 ) ;
#44103 = CARTESIAN_POINT ( 'NONE',  ( 63.54731047306190561, 1.396834109478129804, -68.84999999999999432 ) ) ;
#44104 = EDGE_CURVE ( 'NONE', #45507, #12281, #50892, .T. ) ;
#44105 = CARTESIAN_POINT ( 'NONE',  ( 20.38268442930850100, -22.68236679202650308, -47.83534835059659684 ) ) ;
#44106 = ORIENTED_EDGE ( 'NONE', *, *, #14566, .F. ) ;
#44107 = CARTESIAN_POINT ( 'NONE',  ( 53.17482295840940054, -49.26994467858509097, -27.24576603800480257 ) ) ;
#44108 = CARTESIAN_POINT ( 'NONE',  ( 15.67955243735410065, -50.86262981146630580, -20.14992656220979939 ) ) ;
#44109 = CARTESIAN_POINT ( 'NONE',  ( 76.78794120290260139, 10.77102507788350039, -14.46667607172110159 ) ) ;
#44110 = DIRECTION ( 'NONE',  ( 0.000000000000000000, 0.000000000000000000, -1.000000000000000000 ) ) ;
#44111 = DIRECTION ( 'NONE',  ( 0.000000000000000000, 0.000000000000000000, 1.000000000000000000 ) ) ;
#44112 = EDGE_LOOP ( 'NONE', ( #41486, #51801, #38921, #31540, #14858, #32876 ) ) ;
#44113 = CARTESIAN_POINT ( 'NONE',  ( 9.366543050370410128, -15.61630854221780140, -53.84717978381009829 ) ) ;
#44114 = B_SPLINE_CURVE_WITH_KNOTS ( 'NONE', 3,
 ( #34883, #15748, #42513, #22563, #47478, #19162, #38579, #30691, #27531, #2673, #43029, #39350, #14975, #27277, #47223, #46713, #10798, #26757, #7375, #23325, #3449, #35401, #42770, #39094, #50883, #43538, #30941, #3189, #7638, #46972, #11055, #35139, #51144, #4920, #988, #13313, #13567, #7889, #16986, #45275, #27792, #49479, #9385, #8858, #9115, #37406, #37152, #44752, #24810, #25330, #29271, #28754, #29530, #32935, #48961, #41592, #13064, #41334, #40820, #12797, #47726, #21147, #29019, #5447, #45534, #23835, #1761, #20891, #21404, #9630, #1507, #36888, #17491, #33457, #25585, #5701, #45015, #25065, #719, #40560, #21654, #37659, #31702, #4653, #36614, #41082, #5194, #20626, #1250, #17238, #33200, #49219, #11832, #43787, #16709, #32667, #48695, #50755, #50241, #18520, #46839, #34494, #38440, #2539, #26892, #21915, #26359, #38711, #14848, #10925, #6737, #22172, #30811, #18000, #49728, #42113, #42899, #38965 ),
 .UNSPECIFIED., .F., .F.,
 ( 4, 3, 3, 3, 3, 3, 3, 3, 3, 3, 3, 3, 3, 3, 3, 3, 3, 3, 3, 3, 3, 3, 3, 3, 3, 3, 3, 3, 3, 3, 3, 3, 3, 3, 3, 3, 3, 3, 3, 4 ),
 ( -1.528706106645139950, -1.467014403968580183, -1.462406257103959994, -1.400361489047440067, -1.359972591434809974, -1.338075497632319921, -1.325535015073280087, -1.316390772988770053, -1.255261730263310005, -1.194475198410479999, -1.135862753278430004, -1.120187266468789966, -1.112461743370449785, -1.077250308146380009, -1.017356746704059844, -0.9572232250175689572, -0.8973750609027659753, -0.8492288533768060921, -0.8273183019162870799, -0.8205642526347601828, -0.7619152277339599211, -0.7047902307989259985, -0.6459350262605879633, -0.5874014674332818098, -0.5571792625727400861, -0.5439733099578959452, -0.5366754859262510280, -0.4791548101318530151, -0.4217815166465830323, -0.3651804039304868965, -0.3456238285489439122, -0.3024208499803260342, -0.2835195468565561150, -0.2726001364230170587, -0.2628186309613229632, -0.2067675508394690720, -0.1505665974598759949, -0.09476632463357703706, -0.04010227761605178465, 0.000000000000000000 ),
 .UNSPECIFIED. ) ;
#44115 = CARTESIAN_POINT ( 'NONE',  ( 47.32063939835540367, 23.47154167609649988, -54.65735503397459638 ) ) ;
#44116 = AXIS2_PLACEMENT_3D ( 'NONE', #47817, #31544, #7732 ) ;
#44117 = CARTESIAN_POINT ( 'NONE',  ( 17.50631664302402513, 18.38378960604975632, -83.19923667293778635 ) ) ;
#44118 = CARTESIAN_POINT ( 'NONE',  ( 63.30967889250540992, 1.328674444234399843, -62.53373279716100086 ) ) ;
#44119 = CARTESIAN_POINT ( 'NONE',  ( 57.42729054907940167, -50.31136290499970443, -52.86014444765240938 ) ) ;
#44120 = CARTESIAN_POINT ( 'NONE',  ( 41.02582444074300128, 13.36974427871779980, -4.878402571444859781 ) ) ;
#44121 = CARTESIAN_POINT ( 'NONE',  ( 12.14984836808695512, -8.703641790031165115, -61.12566380759824369 ) ) ;
#44122 = CARTESIAN_POINT ( 'NONE',  ( 72.51559007951500746, 1.439519383694849886, -61.97453994048029813 ) ) ;
#44123 = CARTESIAN_POINT ( 'NONE',  ( 56.24757573095129715, -47.87022910182560054, -48.07122818578029921 ) ) ;
#44124 = CARTESIAN_POINT ( 'NONE',  ( 69.22748654599971019, -50.70395984888047991, -72.15645085170115181 ) ) ;
#44125 = CARTESIAN_POINT ( 'NONE',  ( 104.6856170952499809, -2.032350560839140119, -65.65000000000000568 ) ) ;
#44126 = CARTESIAN_POINT ( 'NONE',  ( 17.93047854176909794, -52.54005950962240235, -75.96018872839380265 ) ) ;
#44127 = ADVANCED_FACE ( 'NONE', ( #33267 ), #49791, .T. ) ;
#44128 = CARTESIAN_POINT ( 'NONE',  ( 8.428860946447588987, -13.54542364617790007, -76.87566458011686166 ) ) ;
#44129 = CARTESIAN_POINT ( 'NONE',  ( 11.89321892218980103, 34.20364954172580241, -22.25048313876769868 ) ) ;
#44130 = ORIENTED_EDGE ( 'NONE', *, *, #15718, .F. ) ;
#44131 = CARTESIAN_POINT ( 'NONE',  ( 30.63393739769620083, -15.61618894467929941, -6.928362978644219794 ) ) ;
#44132 = CARTESIAN_POINT ( 'NONE',  ( 31.69621505786460247, -15.61618894467929763, -8.050000000000000711 ) ) ;
#44133 = CARTESIAN_POINT ( 'NONE',  ( 19.64202710409484354, -21.45867595000445149, -34.78082310848400738 ) ) ;
#44134 = CARTESIAN_POINT ( 'NONE',  ( 12.45061392682710100, -8.818281481913160746, -81.23899999999999011 ) ) ;
#44135 = ADVANCED_FACE ( 'NONE', ( #34296 ), #48349, .T. ) ;
#44136 = VERTEX_POINT ( 'NONE', #45077 ) ;
#44137 = CARTESIAN_POINT ( 'NONE',  ( 17.96618083103230035, 21.24161264671329974, -75.93682688742939035 ) ) ;
#44138 = ORIENTED_EDGE ( 'NONE', *, *, #27836, .T. ) ;
#44139 = B_SPLINE_CURVE_WITH_KNOTS ( 'NONE', 3,
 ( #8770, #36793, #32840, #48867, #12974, #28927 ),
 .UNSPECIFIED., .F., .F.,
 ( 4, 2, 4 ),
 ( 0.4969483822624109481, 0.7484741911312053908, 1.000000000000000000 ),
 .UNSPECIFIED. ) ;
#44140 = EDGE_LOOP ( 'NONE', ( #38807, #4971 ) ) ;
#44141 = CARTESIAN_POINT ( 'NONE',  ( 56.50458353480760110, -46.26559983311960167, -26.27572163198150079 ) ) ;
#44142 = CARTESIAN_POINT ( 'NONE',  ( 18.94624808374599922, -21.82521411516110277, -81.23899999999999011 ) ) ;
#44143 = DIRECTION ( 'NONE',  ( -0.8857883891771956009, -0.4640893551880597157, 0.000000000000000000 ) ) ;
#44144 = CARTESIAN_POINT ( 'NONE',  ( 71.33393739769628894, 10.88381105532070059, -61.44999999999999574 ) ) ;
#44145 = LINE ( 'NONE', #8241, #4197 ) ;
#44146 = FACE_OUTER_BOUND ( 'NONE', #45383, .T. ) ;
#44147 = ORIENTED_EDGE ( 'NONE', *, *, #11741, .F. ) ;
#44148 = DIRECTION ( 'NONE',  ( -0.4808500020228050897, -0.3493579760610313611, 0.8041966675616158966 ) ) ;
#44149 = CARTESIAN_POINT ( 'NONE',  ( 5.133937397847174289, -15.61618894439989802, -19.08999999999999986 ) ) ;
#44150 = ORIENTED_EDGE ( 'NONE', *, *, #18084, .T. ) ;
#44151 = ORIENTED_EDGE ( 'NONE', *, *, #34697, .T. ) ;
#44152 = CARTESIAN_POINT ( 'NONE',  ( 5.741632552282950108, -21.61618894467929763, -22.14999999999999858 ) ) ;
#44153 = CARTESIAN_POINT ( 'NONE',  ( 46.35275103504449845, -52.90993241930539881, -76.14999999999999147 ) ) ;
#44154 = CARTESIAN_POINT ( 'NONE',  ( 60.79127206636130154, 14.45127149603970018, -47.68528058551200388 ) ) ;
#44155 = FACE_OUTER_BOUND ( 'NONE', #16910, .T. ) ;
#44156 = CIRCLE ( 'NONE', #27426, 3.500000000000003109 ) ;
#44157 = DIRECTION ( 'NONE',  ( -0.7071067811865475727, 0.7071067811865475727, 0.000000000000000000 ) ) ;
#44158 = CARTESIAN_POINT ( 'NONE',  ( -11.32734370190460105, 10.64934056395049922, -6.430192534648650593 ) ) ;
#44159 = CARTESIAN_POINT ( 'NONE',  ( 47.18324198357289845, 23.57489020266570279, -74.14999999999999147 ) ) ;
#44160 = CARTESIAN_POINT ( 'NONE',  ( 59.14587251186409844, 14.19052952610539897, -26.50944264180050070 ) ) ;
#44161 = ADVANCED_FACE ( 'NONE', ( #9947 ), #21725, .T. ) ;
#44162 = CARTESIAN_POINT ( 'NONE',  ( 12.64206891719070036, -22.64424718988719931, -63.93428524705129234 ) ) ;
#44163 = VERTEX_POINT ( 'NONE', #9187 ) ;
#44165 = EDGE_CURVE ( 'NONE', #8693, #43345, #37732, .T. ) ;
#44164 = CARTESIAN_POINT ( 'NONE',  ( 16.13393739769620083, -15.61618894467929941, -20.15000000000000213 ) ) ;
#44166 = CARTESIAN_POINT ( 'NONE',  ( 23.32493948456750132, -49.33243882768289978, -34.64999999999999858 ) ) ;
#44167 = CARTESIAN_POINT ( 'NONE',  ( 53.64461521333896599, -51.26703787289181236, -75.63087492057186978 ) ) ;
#44168 = CARTESIAN_POINT ( 'NONE',  ( 72.29280397036849592, 1.443019669817199979, -69.67232717175519952 ) ) ;
#44169 = EDGE_CURVE ( 'NONE', #4309, #46086, #3977, .T. ) ;
#44170 = CARTESIAN_POINT ( 'NONE',  ( 43.29584607586762246, -39.89359886923165988, -70.06847773017847203 ) ) ;
#44171 = CARTESIAN_POINT ( 'NONE',  ( 8.223571189834400386, -15.61612039429540033, -78.79233150823698395 ) ) ;
#44172 = CARTESIAN_POINT ( 'NONE',  ( 46.85494769317200081, 22.79310794512280225, -75.76537854031029440 ) ) ;
#44173 = CARTESIAN_POINT ( 'NONE',  ( 48.51671518355920654, -54.02387269257750546, -54.61093961119340179 ) ) ;
#44174 = CARTESIAN_POINT ( 'NONE',  ( 52.01928042579915257, -32.98329962954817063, -19.49272405259882390 ) ) ;
#44175 = DIRECTION ( 'NONE',  ( 1.000000000000000000, 0.000000000000000000, 0.000000000000000000 ) ) ;
#44176 = CARTESIAN_POINT ( 'NONE',  ( 79.93393739769618378, -31.81618894467930403, -65.65000000000000568 ) ) ;
#44177 = CARTESIAN_POINT ( 'NONE',  ( 57.04834586696819798, 13.88381105532070059, -16.05449549621770089 ) ) ;
#44178 = ORIENTED_EDGE ( 'NONE', *, *, #41417, .F. ) ;
#44179 = CARTESIAN_POINT ( 'NONE',  ( 9.186759353120089955, -12.92497237842379931, -32.18498778107969116 ) ) ;
#44180 = CARTESIAN_POINT ( 'NONE',  ( 64.81872023251169423, 1.368315088675869928, -60.99398296987489942 ) ) ;
#44181 = ORIENTED_EDGE ( 'NONE', *, *, #45187, .T. ) ;
#44182 = CARTESIAN_POINT ( 'NONE',  ( 71.57861930639089110, 0.9369374701296400154, -70.56272516144490226 ) ) ;
#44183 = CARTESIAN_POINT ( 'NONE',  ( 60.74338974301230110, -45.55518699895110046, -47.36711274165079999 ) ) ;
#44184 = CARTESIAN_POINT ( 'NONE',  ( 56.86634278361329820, 19.42073994026870309, -53.85427493997759285 ) ) ;
#44185 = AXIS2_PLACEMENT_3D ( 'NONE', #40046, #40303, #208 ) ;
#44186 = DIRECTION ( 'NONE',  ( 0.000000000000000000, 0.000000000000000000, 1.000000000000000000 ) ) ;
#44188 = DIRECTION ( 'NONE',  ( 0.8263629291053389281, -0.3519990991164029803, -0.4395690430656890024 ) ) ;
#44187 = CARTESIAN_POINT ( 'NONE',  ( 41.70001785874607947, 8.499530765254291964, -77.77813295808087446 ) ) ;
#44189 = CARTESIAN_POINT ( 'NONE',  ( 31.79224979287389985, 4.883811055320679273, -84.65000000000000568 ) ) ;
#44190 = DIRECTION ( 'NONE',  ( 0.000000000000000000, 0.000000000000000000, 1.000000000000000000 ) ) ;
#44191 = EDGE_CURVE ( 'NONE', #40265, #50827, #37499, .T. ) ;
#44192 = ORIENTED_EDGE ( 'NONE', *, *, #23964, .T. ) ;
#44193 = CARTESIAN_POINT ( 'NONE',  ( 84.44784216359251161, -43.11618894467930119, -47.47585302082339354 ) ) ;
#44194 = VERTEX_POINT ( 'NONE', #21983 ) ;
#44195 = ORIENTED_EDGE ( 'NONE', *, *, #27017, .T. ) ;
#44196 = ORIENTED_EDGE ( 'NONE', *, *, #47943, .F. ) ;
#44197 = LINE ( 'NONE', #27173, #38698 ) ;
#44198 = DIRECTION ( 'NONE',  ( 0.000000000000000000, 0.000000000000000000, -1.000000000000000000 ) ) ;
#44199 = CARTESIAN_POINT ( 'NONE',  ( 76.42339056421366195, -22.53537624654720162, -12.89730100488529274 ) ) ;
#44200 = CARTESIAN_POINT ( 'NONE',  ( 53.17454399592740089, -51.89736142002809771, -53.32454619227790005 ) ) ;
#44201 = ORIENTED_EDGE ( 'NONE', *, *, #45674, .F. ) ;
#44202 = ORIENTED_EDGE ( 'NONE', *, *, #15071, .F. ) ;
#44203 = CARTESIAN_POINT ( 'NONE',  ( 48.71617454467180153, 22.66482838071829775, -54.49917290083569554 ) ) ;
#44204 = CARTESIAN_POINT ( 'NONE',  ( 56.87859880284599967, -45.21741274165630387, -25.29773968820679997 ) ) ;
#44205 = CARTESIAN_POINT ( 'NONE',  ( 56.52383276625679542, -50.75240083704239424, -53.80484218896539517 ) ) ;
#44206 = CARTESIAN_POINT ( 'NONE',  ( 68.13393739769618662, -29.66618894467940137, -65.65000000000000568 ) ) ;
#44207 = CARTESIAN_POINT ( 'NONE',  ( 24.04487537504365591, -15.58383510252001791, -59.79102400322322808 ) ) ;
#44208 = DIRECTION ( 'NONE',  ( 1.000000000000000000, 0.000000000000000000, 0.000000000000000000 ) ) ;
#44209 = VERTEX_POINT ( 'NONE', #1315 ) ;
#44210 = B_SPLINE_CURVE_WITH_KNOTS ( 'NONE', 3,
 ( #20216, #4246, #24126, #8700, #32769, #565, #314, #33039, #3997, #71, #13171, #44082, #5031, #12903 ),
 .UNSPECIFIED., .F., .F.,
 ( 4, 2, 2, 2, 2, 2, 4 ),
 ( 0.000000000000000000, 0.03186051038564466364, 0.1779947729689404512, 0.2693286870835011615, 0.4519965153126213053, 0.7442650404792127139, 1.000000000000000000 ),
 .UNSPECIFIED. ) ;
#44211 = DIRECTION ( 'NONE',  ( -1.000000000000000000, 0.000000000000000000, 0.000000000000000000 ) ) ;
#44212 = CARTESIAN_POINT ( 'NONE',  ( 54.08403600473499750, -50.62655576154210024, -76.77913599446510773 ) ) ;
#44213 = CARTESIAN_POINT ( 'NONE',  ( 8.222678474964419948, -15.61600660124389961, -50.79233150823699816 ) ) ;
#44214 = DIRECTION ( 'NONE',  ( 0.000000000000000000, 1.000000000000000000, 0.000000000000000000 ) ) ;
#44215 = CARTESIAN_POINT ( 'NONE',  ( 20.86355735167390080, -21.87857209189399654, -52.30659627123909416 ) ) ;
#44216 = CARTESIAN_POINT ( 'NONE',  ( 12.94869328597129865, -50.11097969449580347, -21.09867881371670251 ) ) ;
#44217 = CYLINDRICAL_SURFACE ( 'NONE', #28777, 1.999999999999997113 ) ;
#44218 = CARTESIAN_POINT ( 'NONE',  ( -22.70381420151059615, -12.10940840177920563, -54.67624860166066725 ) ) ;
#44219 = CYLINDRICAL_SURFACE ( 'NONE', #17629, 6.766999999999998572 ) ;
#44220 = CARTESIAN_POINT ( 'NONE',  ( 65.43393739769584272, -48.11618894467832064, -70.54999999999975557 ) ) ;
#44221 = CARTESIAN_POINT ( 'NONE',  ( 3.987490788289483667, -22.62894316431776787, -34.79644660940672907 ) ) ;
#44222 = LINE ( 'NONE', #23769, #35464 ) ;
#44223 = AXIS2_PLACEMENT_3D ( 'NONE', #33176, #44211, #25309 ) ;
#44224 = CARTESIAN_POINT ( 'NONE',  ( 10.93327293488309948, -20.38018394044530268, -51.61111978220640140 ) ) ;
#44225 = CARTESIAN_POINT ( 'NONE',  ( -23.86606260230375298, 4.515865522462924275, -53.92777777777781978 ) ) ;
#44226 = ORIENTED_EDGE ( 'NONE', *, *, #11827, .T. ) ;
#44228 = EDGE_CURVE ( 'NONE', #18800, #23355, #18067, .T. ) ;
#44227 = CARTESIAN_POINT ( 'NONE',  ( 14.39527773360719820, -51.26000396899650013, -74.91994212301220557 ) ) ;
#44229 = CARTESIAN_POINT ( 'NONE',  ( 47.30647391031549631, -54.71510682645079982, -54.67548368043780016 ) ) ;
#44230 = DIRECTION ( 'NONE',  ( -1.000000000000000000, 0.000000000000000000, 0.000000000000000000 ) ) ;
#44231 = ADVANCED_FACE ( 'NONE', ( #43721 ), #4137, .T. ) ;
#44232 = CARTESIAN_POINT ( 'NONE',  ( 22.90093739478795598, -14.73038937777455892, -38.41115654869280860 ) ) ;
#44233 = DIRECTION ( 'NONE',  ( 1.000000000000000000, 0.000000000000000000, 0.000000000000000000 ) ) ;
#44234 = CARTESIAN_POINT ( 'NONE',  ( 60.89898296291905666, -45.44660769381673049, -47.15703363117398794 ) ) ;
#44235 = CARTESIAN_POINT ( 'NONE',  ( 11.89321892218980103, 34.20364954172580241, -18.17421237893020347 ) ) ;
#44236 = CARTESIAN_POINT ( 'NONE',  ( 23.04647429551237536, -19.60029476399586557, -73.67433456739328790 ) ) ;
#44237 = CARTESIAN_POINT ( 'NONE',  ( 14.58586965385978296, -51.79680896048888172, -75.65449996337102334 ) ) ;
#44238 = CARTESIAN_POINT ( 'NONE',  ( 48.74056688299980777, 22.69703636651660261, -54.59336294021409941 ) ) ;
#44239 = VERTEX_POINT ( 'NONE', #4395 ) ;
#44240 = CARTESIAN_POINT ( 'NONE',  ( 53.05460986333120132, -49.56517142501709827, -48.99361254808879806 ) ) ;
#44241 = ORIENTED_EDGE ( 'NONE', *, *, #15203, .T. ) ;
#44242 = CARTESIAN_POINT ( 'NONE',  ( 24.04493739769619864, -15.61618894467929941, -32.14999999999999858 ) ) ;
#44243 = CARTESIAN_POINT ( 'NONE',  ( 11.97538973034304455, -21.02760254491551350, -75.16115355296736311 ) ) ;
#44244 = CARTESIAN_POINT ( 'NONE',  ( 56.86634279045120621, -50.65311782823120268, -53.85427494076709820 ) ) ;
#44246 = CARTESIAN_POINT ( 'NONE',  ( 53.47797947282749931, 17.67580957532919683, -26.84483267738330170 ) ) ;
#44245 = CARTESIAN_POINT ( 'NONE',  ( 83.85202357338320667, 13.12642060550550127, -46.78691132286910204 ) ) ;
#44247 = CARTESIAN_POINT ( 'NONE',  ( 21.32600670501789963, -20.38954992040629932, -66.68945394373800184 ) ) ;
#44248 = CARTESIAN_POINT ( 'NONE',  ( 52.62851231361270266, 18.57686390552120059, -48.67161502741990375 ) ) ;
#44249 = CARTESIAN_POINT ( 'NONE',  ( 56.80367323221330622, -45.12899470519759859, -16.17916504339369865 ) ) ;
#44250 = EDGE_CURVE ( 'NONE', #6450, #29628, #39149, .T. ) ;
#44251 = CARTESIAN_POINT ( 'NONE',  ( 11.27236363464668401, -21.94243302856639843, -80.50066552057984381 ) ) ;
#44252 = ORIENTED_EDGE ( 'NONE', *, *, #34697, .F. ) ;
#44253 = CARTESIAN_POINT ( 'NONE',  ( 11.85406245721990004, -22.19413837265960154, -43.97111461901920393 ) ) ;
#44254 = EDGE_CURVE ( 'NONE', #5735, #42976, #46722, .T. ) ;
#44255 = ORIENTED_EDGE ( 'NONE', *, *, #11709, .F. ) ;
#44256 = CARTESIAN_POINT ( 'NONE',  ( 11.94685996674130024, -65.31805379620070084, -17.08231279504250111 ) ) ;
#44257 = CARTESIAN_POINT ( 'NONE',  ( 10.67951312630159855, 33.37294054514710240, -46.54192847483160023 ) ) ;
#44258 = CARTESIAN_POINT ( 'NONE',  ( 18.78952938989682053, 20.37315169409249194, -15.76902864060759590 ) ) ;
#44259 = CARTESIAN_POINT ( 'NONE',  ( 48.78564399443680344, -53.86781325685030453, -54.49562672282650055 ) ) ;
#44260 = CARTESIAN_POINT ( 'NONE',  ( 8.794764235947729603, 31.93474649087269768, -46.67042062406039804 ) ) ;
#44261 = CARTESIAN_POINT ( 'NONE',  ( 0.07463975747345250045, -10.49561525072540036, -34.71188928912359728 ) ) ;
#44262 = CIRCLE ( 'NONE', #25827, 13.50000000000000178 ) ;
#44263 = CIRCLE ( 'NONE', #30026, 2.999999999999999112 ) ;
#44264 = ORIENTED_EDGE ( 'NONE', *, *, #26411, .F. ) ;
#44265 = CARTESIAN_POINT ( 'NONE',  ( 53.59003930803689997, -49.40628012469949937, -49.22510501142529904 ) ) ;
#44266 = CARTESIAN_POINT ( 'NONE',  ( 11.13393739769619906, -63.29577390112070390, -43.91524999462519929 ) ) ;
#44267 = DIRECTION ( 'NONE',  ( -0.3535533905932738974, 0.6123724356957941373, 0.7071067811865477948 ) ) ;
#44268 = EDGE_LOOP ( 'NONE', ( #7924, #33102 ) ) ;
#44269 = CARTESIAN_POINT ( 'NONE',  ( 71.55691549992010891, 1.416242794300029972, -70.15496246767990840 ) ) ;
#44270 = CARTESIAN_POINT ( 'NONE',  ( 50.04022686061209413, -48.91488563423410341, -76.14999999999999147 ) ) ;
#44271 = DIRECTION ( 'NONE',  ( -0.3294064756441168473, -0.9441882088883136737, 0.000000000000000000 ) ) ;
#44272 = ORIENTED_EDGE ( 'NONE', *, *, #10533, .T. ) ;
#44273 = CARTESIAN_POINT ( 'NONE',  ( 21.39066400359539699, -9.703911137440838885, -81.23899999999999011 ) ) ;
#44274 = CARTESIAN_POINT ( 'NONE',  ( 11.67619942398487609, 33.65927571709751476, -46.39999999999999858 ) ) ;
#44275 = CARTESIAN_POINT ( 'NONE',  ( 16.13393739769620083, -38.61618894467930119, -84.65000000000000568 ) ) ;
#44276 = DIRECTION ( 'NONE',  ( 0.000000000000000000, 0.000000000000000000, 1.000000000000000000 ) ) ;
#44277 = CARTESIAN_POINT ( 'NONE',  ( 11.87246112257180108, -22.67469728656620021, -70.46522537534779929 ) ) ;
#44278 = CARTESIAN_POINT ( 'NONE',  ( 18.59784447790332251, -9.007730646818817632, -38.46077722564568546 ) ) ;
#44279 = CYLINDRICAL_SURFACE ( 'NONE', #4105, 5.499999999999998224 ) ;
#44280 = SHAPE_DEFINITION_REPRESENTATION ( #39852, #50919 ) ;
#44281 = ORIENTED_EDGE ( 'NONE', *, *, #10843, .F. ) ;
#44282 = CARTESIAN_POINT ( 'NONE',  ( 10.48872632231780067, -10.75426692560380104, -63.45897166066949069 ) ) ;
#44283 = CARTESIAN_POINT ( 'NONE',  ( 52.82328078765490176, -49.70102997746409557, -48.95193629136059599 ) ) ;
#44284 = DIRECTION ( 'NONE',  ( 0.000000000000000000, 0.000000000000000000, -1.000000000000000000 ) ) ;
#44285 = LINE ( 'NONE', #28808, #19515 ) ;
#44287 = EDGE_CURVE ( 'NONE', #37740, #47321, #1506, .T. ) ;
#44286 = CARTESIAN_POINT ( 'NONE',  ( 46.98204976736620608, 22.87102341606869871, -75.65359354181590845 ) ) ;
#44288 = CARTESIAN_POINT ( 'NONE',  ( 14.63393739769630031, 1.354373803797940035, -35.14999999999999858 ) ) ;
#44289 = CARTESIAN_POINT ( 'NONE',  ( 61.28610861176739633, -45.23040055550220018, -28.15000000000000213 ) ) ;
#44290 = AXIS2_PLACEMENT_3D ( 'NONE', #32505, #48533, #14180 ) ;
#44291 = DIRECTION ( 'NONE',  ( 0.000000000000000000, 1.000000000000000000, 0.000000000000000000 ) ) ;
#44292 = AXIS2_PLACEMENT_3D ( 'NONE', #33527, #13881, #45861 ) ;
#44294 = AXIS2_PLACEMENT_3D ( 'NONE', #42584, #51476, #47548 ) ;
#44293 = CARTESIAN_POINT ( 'NONE',  ( 8.829104702642069924, -19.44007963430999908, -76.35416353349960161 ) ) ;
#44295 = CARTESIAN_POINT ( 'NONE',  ( 54.36664156623190536, -50.61618894733009455, -76.93804975441300087 ) ) ;
#44297 = DIRECTION ( 'NONE',  ( -0.8660254037844381525, -0.5000000000000007772, 0.000000000000000000 ) ) ;
#44296 = DIRECTION ( 'NONE',  ( 1.000000000000000000, 2.460964292799963328E-14, 0.000000000000000000 ) ) ;
#44298 = VECTOR ( 'NONE', #27620, 1000.000000000000114 ) ;
#44299 = MANIFOLD_SOLID_BREP ( 'Stock-MAS-691-1', #18449 ) ;
#44300 = CARTESIAN_POINT ( 'NONE',  ( 63.25550833076970747, 1.336371993404959824, -68.64083569922701145 ) ) ;
#44301 = CARTESIAN_POINT ( 'NONE',  ( 61.37776962238909562, 13.97314662197880075, -46.75431274365950429 ) ) ;
#44302 = CARTESIAN_POINT ( 'NONE',  ( -0.4147641054085740020, -62.74225160656001066, -49.23002488738299576 ) ) ;
#44303 = ORIENTED_EDGE ( 'NONE', *, *, #7470, .F. ) ;
#44304 = CARTESIAN_POINT ( 'NONE',  ( 52.92965940600010555, -49.60857842614319679, -48.75165690212650560 ) ) ;
#44305 = CARTESIAN_POINT ( 'NONE',  ( 61.43378182061679382, -45.16646909839339941, -28.04045001510230151 ) ) ;
#44306 = CARTESIAN_POINT ( 'NONE',  ( 11.27215347255375555, -21.94227403160163448, -72.50068352509246949 ) ) ;
#44307 = CARTESIAN_POINT ( 'NONE',  ( 57.38853962498540540, 14.21080702799810069, -26.07334594942189909 ) ) ;
#44308 = CARTESIAN_POINT ( 'NONE',  ( 17.23033643585230124, -22.58328789946420301, -36.90313586381709854 ) ) ;
#44309 = CARTESIAN_POINT ( 'NONE',  ( 50.30621308613430642, 17.38380720298980009, -76.16272939236809236 ) ) ;
#44310 = CARTESIAN_POINT ( 'NONE',  ( 52.95762501200700001, 18.36394703063159994, -48.83320043447420034 ) ) ;
#44311 = CARTESIAN_POINT ( 'NONE',  ( 71.11795458202399800, 1.382840740411490188, -70.34664320112889868 ) ) ;
#44312 = CARTESIAN_POINT ( 'NONE',  ( 85.38000601716228743, 17.38381105532069881, -60.34000486924599471 ) ) ;
#44313 = CARTESIAN_POINT ( 'NONE',  ( 43.40604938376139899, -43.84278571223109822, -5.039288310186040398 ) ) ;
#44314 = VERTEX_POINT ( 'NONE', #8078 ) ;
#44315 = DIRECTION ( 'NONE',  ( 0.000000000000000000, -1.000000000000000000, 0.000000000000000000 ) ) ;
#44316 = EDGE_CURVE ( 'NONE', #17150, #15443, #45014, .T. ) ;
#44317 = CARTESIAN_POINT ( 'NONE',  ( 47.77491216306469823, -54.41753965447119867, -54.70980729587230229 ) ) ;
#44318 = PLANE ( 'NONE',  #37092 ) ;
#44319 = CARTESIAN_POINT ( 'NONE',  ( 34.99574079657120507, -15.61618894467929763, 17.07360679774999923 ) ) ;
#44320 = CARTESIAN_POINT ( 'NONE',  ( 60.62314454574009659, 14.26357126862269986, -47.31713781460809543 ) ) ;
#44321 = CARTESIAN_POINT ( 'NONE',  ( 71.37118938927949330, 1.325715844996850024, -60.88145737504000010 ) ) ;
#44322 = DIRECTION ( 'NONE',  ( 0.000000000000000000, -1.000000000000000000, 0.000000000000000000 ) ) ;
#44323 = CARTESIAN_POINT ( 'NONE',  ( 71.63858812870320492, 1.136600705753829876, -60.83584486289709758 ) ) ;
#44324 = CARTESIAN_POINT ( 'NONE',  ( 9.807676993354524697, -20.47774494272987056, -72.29929351537433035 ) ) ;
#44325 = CARTESIAN_POINT ( 'NONE',  ( 65.11099717020638877, 1.370937308141410238, -70.40667188452549397 ) ) ;
#44326 = ORIENTED_EDGE ( 'NONE', *, *, #43555, .T. ) ;
#44327 = ORIENTED_EDGE ( 'NONE', *, *, #5964, .F. ) ;
#44328 = DIRECTION ( 'NONE',  ( 1.224646799147353207E-16, 1.000000000000000000, -0.000000000000000000 ) ) ;
#44329 = AXIS2_PLACEMENT_3D ( 'NONE', #6473, #38182, #50496 ) ;
#44330 = CARTESIAN_POINT ( 'NONE',  ( 0.1457839871805953758, -45.96255801450852374, -34.68167748489142355 ) ) ;
#44331 = ORIENTED_EDGE ( 'NONE', *, *, #38684, .F. ) ;
#44332 = CARTESIAN_POINT ( 'NONE',  ( 38.67452568954060155, -15.61618894467929941, -81.65000000000000568 ) ) ;
#44333 = CARTESIAN_POINT ( 'NONE',  ( 11.72329413022380074, -64.94052275741300662, -45.18478288877960836 ) ) ;
#44334 = LINE ( 'NONE', #9225, #51299 ) ;
#44335 = AXIS2_PLACEMENT_3D ( 'NONE', #28502, #35860, #216 ) ;
#44336 = CIRCLE ( 'NONE', #47714, 1.999999999999998224 ) ;
#44337 = ORIENTED_EDGE ( 'NONE', *, *, #50747, .T. ) ;
#44338 = CARTESIAN_POINT ( 'NONE',  ( 22.90067702240739322, -15.61618873416334807, -54.84718332859007006 ) ) ;
#44339 = CIRCLE ( 'NONE', #34249, 10.00000000000000888 ) ;
#44340 = LINE ( 'NONE', #40153, #22627 ) ;
#44341 = AXIS2_PLACEMENT_3D ( 'NONE', #50457, #2495, #11141 ) ;
#44342 = CARTESIAN_POINT ( 'NONE',  ( 19.63779757108790136, -8.152564895917599586, -45.43204315924410253 ) ) ;
#44343 = CARTESIAN_POINT ( 'NONE',  ( 65.27736602627911111, 1.383811055320669947, -60.94999999999999574 ) ) ;
#44344 = CIRCLE ( 'NONE', #30070, 1.500000000000001332 ) ;
#44345 = CARTESIAN_POINT ( 'NONE',  ( 41.88850923412460503, -37.60571807051355364, -80.87708175111015407 ) ) ;
#44346 =( LENGTH_UNIT ( ) NAMED_UNIT ( * ) SI_UNIT ( .MILLI., .METRE. ) );
#44347 = ORIENTED_EDGE ( 'NONE', *, *, #47166, .F. ) ;
#44348 = CARTESIAN_POINT ( 'NONE',  ( 11.74606379632330011, -63.66956124298060615, -24.76212639862699660 ) ) ;
#44349 = CARTESIAN_POINT ( 'NONE',  ( 12.57041540415229974, -9.073406294472009748, -35.57390792627550269 ) ) ;
#44350 = CARTESIAN_POINT ( 'NONE',  ( 42.00758169699690114, 14.56552422315210116, -6.830508309558650737 ) ) ;
#44351 = ADVANCED_FACE ( 'NONE', ( #16448 ), #34979, .T. ) ;
#44352 = CARTESIAN_POINT ( 'NONE',  ( 14.07159887855190128, 21.04516553096049947, -75.75221093576890041 ) ) ;
#44353 = ADVANCED_FACE ( 'NONE', ( #8330 ), #12525, .T. ) ;
#44354 = CARTESIAN_POINT ( 'NONE',  ( 51.88872868351670320, 18.11352286612800100, -77.07840643951000459 ) ) ;
#44355 = EDGE_CURVE ( 'NONE', #8604, #26370, #38313, .T. ) ;
#44356 = CARTESIAN_POINT ( 'NONE',  ( 83.24078296369461327, -44.82564673796089494, -46.48094294253990455 ) ) ;
#44357 = CARTESIAN_POINT ( 'NONE',  ( 0.4371248283888460318, -8.845792823550640449, -35.02873218748179340 ) ) ;
#44358 = ADVANCED_FACE ( 'NONE', ( #35770 ), #19904, .F. ) ;
#44359 = CARTESIAN_POINT ( 'NONE',  ( 16.01653867706220069, -23.86051658551030030, -38.01220089870790275 ) ) ;
#44360 = ORIENTED_EDGE ( 'NONE', *, *, #49842, .T. ) ;
#44361 = CARTESIAN_POINT ( 'NONE',  ( 52.98187407645789904, -49.51877675916850308, -27.67813261086740084 ) ) ;
#44362 = CARTESIAN_POINT ( 'NONE',  ( 15.78591284856750043, -50.92509110356280644, -20.28298178678319985 ) ) ;
#44363 = CARTESIAN_POINT ( 'NONE',  ( 57.28991729228510366, 19.34649676830889931, -53.44461810997239581 ) ) ;
#44364 = CARTESIAN_POINT ( 'NONE',  ( 22.68450356906678422, -17.37076425861442175, -56.53614005759181538 ) ) ;
#44365 = CARTESIAN_POINT ( 'NONE',  ( 10.13393739769619906, -54.15188668067469990, -35.14999999999999858 ) ) ;
#44366 = AXIS2_PLACEMENT_3D ( 'NONE', #41246, #1416, #21832 ) ;
#44367 = VERTEX_POINT ( 'NONE', #34720 ) ;
#44368 = AXIS2_PLACEMENT_3D ( 'NONE', #3217, #47504, #39378 ) ;
#44369 = CARTESIAN_POINT ( 'NONE',  ( -10.40242566545200020, -42.83441872489630242, -6.165522616775290565 ) ) ;
#44370 = TOROIDAL_SURFACE ( 'NONE', #23438, 16.60961179679779676, 0.5000000000000000000 ) ;
#44371 = CARTESIAN_POINT ( 'NONE',  ( 47.29084618877600121, 23.49490054074589906, -54.73149148133969533 ) ) ;
#44373 = AXIS2_PLACEMENT_3D ( 'NONE', #37302, #37553, #49373 ) ;
#44372 = CARTESIAN_POINT ( 'NONE',  ( 19.13393739769600188, 18.38381105532069881, -83.01107220193038927 ) ) ;
#44374 = CARTESIAN_POINT ( 'NONE',  ( 63.03382193542370260, 0.9209334348186318797, -62.48938310929649731 ) ) ;
#44375 = CARTESIAN_POINT ( 'NONE',  ( 16.13393739769620083, -15.61618894467929941, -18.35000000000000142 ) ) ;
#44376 = VECTOR ( 'NONE', #2195, 1000.000000000000000 ) ;
#44377 = CARTESIAN_POINT ( 'NONE',  ( 42.50318722711249819, 12.76421688433049972, -4.913421252035550246 ) ) ;
#44378 = CARTESIAN_POINT ( 'NONE',  ( 12.86517331568619937, 17.88381105532060289, -34.64999999999999858 ) ) ;
#44379 = CARTESIAN_POINT ( 'NONE',  ( -18.32056709076243450, -10.29233614124584761, -50.69739520735547700 ) ) ;
#44380 = CARTESIAN_POINT ( 'NONE',  ( 71.59408232549860429, 1.419970371292400113, -61.16051820649249748 ) ) ;
#44381 = CARTESIAN_POINT ( 'NONE',  ( 57.08291034350739324, -47.57583641667570618, -48.30715737835689794 ) ) ;
#44382 = DIRECTION ( 'NONE',  ( 0.1961161351368100048, 0.000000000000000000, 0.9805806756911950028 ) ) ;
#44383 = CARTESIAN_POINT ( 'NONE',  ( 46.82538613462320143, 3.332619105128364012, -54.61944740401203546 ) ) ;
#44384 = CARTESIAN_POINT ( 'NONE',  ( 17.69336951584759987, -52.55982454884319566, -76.04476946176040997 ) ) ;
#44385 = EDGE_CURVE ( 'NONE', #8558, #11901, #35513, .T. ) ;
#44386 = DIRECTION ( 'NONE',  ( 0.000000000000000000, 0.000000000000000000, 1.000000000000000000 ) ) ;
#44387 = CARTESIAN_POINT ( 'NONE',  ( 46.03122142033570441, 13.88381105532070059, -7.582879021622040305 ) ) ;
#44388 = EDGE_LOOP ( 'NONE', ( #21616, #51295 ) ) ;
#44389 = CARTESIAN_POINT ( 'NONE',  ( -0.2164510085826325259, -10.71251607911394288, -34.95468620319246611 ) ) ;
#44390 = CARTESIAN_POINT ( 'NONE',  ( 9.727929673803711097, 31.89460007113610018, -46.30184689934900177 ) ) ;
#44391 = FACE_OUTER_BOUND ( 'NONE', #45881, .T. ) ;
#44392 = CARTESIAN_POINT ( 'NONE',  ( 67.36984938551290725, -30.01295387514729995, -17.47394132841339598 ) ) ;
#44393 = ORIENTED_EDGE ( 'NONE', *, *, #45734, .F. ) ;
#44395 = B_SPLINE_CURVE_WITH_KNOTS ( 'NONE', 3,
 ( #23806, #47694, #19385, #39821 ),
 .UNSPECIFIED., .F., .F.,
 ( 4, 4 ),
 ( 0.000000000000000000, 1.000000000000000000 ),
 .UNSPECIFIED. ) ;
#44394 = CARTESIAN_POINT ( 'NONE',  ( 18.55689598211829860, 20.32289363718000175, -74.92517623884199907 ) ) ;
#44396 = ORIENTED_EDGE ( 'NONE', *, *, #28953, .F. ) ;
#44397 = VERTEX_POINT ( 'NONE', #27383 ) ;
#44398 = ORIENTED_EDGE ( 'NONE', *, *, #6446, .F. ) ;
#44399 = FACE_OUTER_BOUND ( 'NONE', #27769, .T. ) ;
#44400 = DIRECTION ( 'NONE',  ( -0.8224686640529097481, 0.3976080002595595575, -0.4067593573362710546 ) ) ;
#44401 = LINE ( 'NONE', #20528, #36474 ) ;
#44402 = CARTESIAN_POINT ( 'NONE',  ( 61.50409081826520463, 14.14169698785779872, -47.35439638855399380 ) ) ;
#44403 = ORIENTED_EDGE ( 'NONE', *, *, #9872, .F. ) ;
#44404 = EDGE_CURVE ( 'NONE', #45770, #8243, #40819, .T. ) ;
#44405 = CARTESIAN_POINT ( 'NONE',  ( -21.36606260230379917, -62.11618894467930119, 11.84999999999999964 ) ) ;
#44406 = CARTESIAN_POINT ( 'NONE',  ( 11.98643035757825892, 34.18553736260165010, -17.50083510588233793 ) ) ;
#44407 = ORIENTED_EDGE ( 'NONE', *, *, #23034, .F. ) ;
#44408 = CARTESIAN_POINT ( 'NONE',  ( 11.60073034461098551, -64.80729423298977565, -23.92052759426241337 ) ) ;
#44409 = CARTESIAN_POINT ( 'NONE',  ( 14.13393739769619195, -34.76920587678100105, -43.67210485810500842 ) ) ;
#44411 = VERTEX_POINT ( 'NONE', #11157 ) ;
#44410 = CIRCLE ( 'NONE', #33512, 8.000000000000000000 ) ;
#44412 = ORIENTED_EDGE ( 'NONE', *, *, #38703, .T. ) ;
#44413 = DIRECTION ( 'NONE',  ( 0.7800418122827239564, 0.000000000000000000, -0.6257273935913973961 ) ) ;
#44414 = CARTESIAN_POINT ( 'NONE',  ( 64.93393739769619799, 1.883811055320669947, -60.94999999999999574 ) ) ;
#44415 = VECTOR ( 'NONE', #4753, 1000.000000000000000 ) ;
#44416 = CARTESIAN_POINT ( 'NONE',  ( 60.63142620721699672, 14.43203532425889968, -47.55417844658280302 ) ) ;
#44417 = AXIS2_PLACEMENT_3D ( 'NONE', #25611, #26134, #21430 ) ;
#44418 = CARTESIAN_POINT ( 'NONE',  ( 45.64758709548550542, 13.96552996563729998, -8.164367127537008884 ) ) ;
#44419 = CARTESIAN_POINT ( 'NONE',  ( 17.63393739769620083, -42.11618894467939356, -34.64999999999999858 ) ) ;
#44420 = CARTESIAN_POINT ( 'NONE',  ( -8.924323233903118435, 12.96044049061340075, -5.352796887738729303 ) ) ;
#44421 = CARTESIAN_POINT ( 'NONE',  ( 64.08038400710292137, 11.23736444591397543, -68.84999999999999432 ) ) ;
#44422 = CARTESIAN_POINT ( 'NONE',  ( 55.12914169688411192, 14.86070934991266590, -16.25648467340654335 ) ) ;
#44423 = EDGE_CURVE ( 'NONE', #19697, #26146, #50724, .T. ) ;
#44424 = CARTESIAN_POINT ( 'NONE',  ( 18.80162467749480015, -22.99658139768499865, -65.67710173045091437 ) ) ;
#44425 = ORIENTED_EDGE ( 'NONE', *, *, #22759, .F. ) ;
#44426 = DIRECTION ( 'NONE',  ( 1.000000000000000000, 2.460964292799963328E-14, 0.000000000000000000 ) ) ;
#44427 = CARTESIAN_POINT ( 'NONE',  ( 41.31928349002789957, 14.36833702740849894, -6.259994320181990091 ) ) ;
#44428 = DIRECTION ( 'NONE',  ( 1.000000000000000000, 0.000000000000000000, 0.000000000000000000 ) ) ;
#44429 = CARTESIAN_POINT ( 'NONE',  ( 72.24967035273689930, 1.113948672550079788, -70.00993265641670860 ) ) ;
#44430 = CARTESIAN_POINT ( 'NONE',  ( 42.95314063166655671, -39.86164201837387822, -71.72600535252449561 ) ) ;
#44431 =( NAMED_UNIT ( * ) SI_UNIT ( $, .STERADIAN. ) SOLID_ANGLE_UNIT ( ) );
#44432 = CARTESIAN_POINT ( 'NONE',  ( 49.39942642721219812, -53.75096344194059128, -54.82511225024550328 ) ) ;
#44433 = CARTESIAN_POINT ( 'NONE',  ( -7.973795448866470181, 13.91176078833520080, -5.720958296299230028 ) ) ;
#44434 = FACE_OUTER_BOUND ( 'NONE', #28282, .T. ) ;
#44435 = CARTESIAN_POINT ( 'NONE',  ( 18.12828521207283217, 1.371102756008170109, -35.06583844469729172 ) ) ;
#44437 = EDGE_CURVE ( 'NONE', #37692, #13888, #8057, .T. ) ;
#44436 = CARTESIAN_POINT ( 'NONE',  ( 22.64011532494543388, -18.06274401070583835, -70.96223323988861864 ) ) ;
#44438 = VERTEX_POINT ( 'NONE', #15851 ) ;
#44439 = VECTOR ( 'NONE', #51349, 1000.000000000000000 ) ;
#44440 = CARTESIAN_POINT ( 'NONE',  ( 12.07081295223539996, -21.86100392024429695, -43.75095171636819913 ) ) ;
#44441 = CARTESIAN_POINT ( 'NONE',  ( 65.03603135424580728, -29.76883965895079953, -19.52361391316370032 ) ) ;
#44442 = VERTEX_POINT ( 'NONE', #31810 ) ;
#44443 = DIRECTION ( 'NONE',  ( -1.000000000000000000, 0.000000000000000000, 0.000000000000000000 ) ) ;
#44444 = CARTESIAN_POINT ( 'NONE',  ( 60.79250979228859819, -45.50810424805050758, -47.25467579807390450 ) ) ;
#44445 = DIRECTION ( 'NONE',  ( 1.000000000000000000, 0.000000000000000000, 0.000000000000000000 ) ) ;
#44446 = CARTESIAN_POINT ( 'NONE',  ( 67.50570755965968317, -43.40455556736388587, -11.14108988509339326 ) ) ;
#44448 = CARTESIAN_POINT ( 'NONE',  ( 0.1457841021255935343, -22.91266753744946527, -34.68167779225149161 ) ) ;
#44447 = CARTESIAN_POINT ( 'NONE',  ( 42.81535512389526588, 8.615775408760638854, -72.39296071868187710 ) ) ;
#44449 = AXIS2_PLACEMENT_3D ( 'NONE', #20728, #817, #49059 ) ;
#44450 = DIRECTION ( 'NONE',  ( -1.065814103640149870E-16, 1.000000000000000000, 0.000000000000000000 ) ) ;
#44451 = VERTEX_POINT ( 'NONE', #6967 ) ;
#44452 = CARTESIAN_POINT ( 'NONE',  ( 83.91175033285890095, -44.80491236700709834, -47.46627397093730139 ) ) ;
#44453 = EDGE_LOOP ( 'NONE', ( #22368, #35922, #18675, #18493, #14541 ) ) ;
#44454 = ORIENTED_EDGE ( 'NONE', *, *, #25836, .F. ) ;
#44455 = ORIENTED_EDGE ( 'NONE', *, *, #51277, .F. ) ;
#44456 = DIRECTION ( 'NONE',  ( -1.000000000000000000, 0.000000000000000000, 0.000000000000000000 ) ) ;
#44457 = CARTESIAN_POINT ( 'NONE',  ( 53.48381752779376086, -50.52032509664712734, -77.13953785887332515 ) ) ;
#44458 = CARTESIAN_POINT ( 'NONE',  ( 76.39938456792719990, -19.35446345062952744, -12.79389377502640102 ) ) ;
#44459 = CARTESIAN_POINT ( 'NONE',  ( 50.21208614976480078, -53.15602288804570463, -53.95043619330500206 ) ) ;
#44460 = ORIENTED_EDGE ( 'NONE', *, *, #33825, .F. ) ;
#44461 = EDGE_CURVE ( 'NONE', #40749, #32305, #17064, .T. ) ;
#44462 = ORIENTED_EDGE ( 'NONE', *, *, #44068, .T. ) ;
#44463 = CARTESIAN_POINT ( 'NONE',  ( 48.89501045483829955, 22.56229972626200109, -54.41963477494619639 ) ) ;
#44464 = CARTESIAN_POINT ( 'NONE',  ( 0.6045892726184849408, -22.44175889786657763, -34.79644291222908237 ) ) ;
#44465 = EDGE_CURVE ( 'NONE', #41357, #18363, #41685, .T. ) ;
#44466 = FACE_OUTER_BOUND ( 'NONE', #13903, .T. ) ;
#44467 = DIRECTION ( 'NONE',  ( 0.8090169943749478954, 0.5877852522924724710, 0.000000000000000000 ) ) ;
#44468 = CARTESIAN_POINT ( 'NONE',  ( 44.12711257345860361, -33.11618894467940066, -54.38706558040979644 ) ) ;
#44469 = LINE ( 'NONE', #48668, #13419 ) ;
#44470 = ADVANCED_FACE ( 'NONE', ( #8507 ), #48340, .T. ) ;
#44471 = ORIENTED_EDGE ( 'NONE', *, *, #20038, .T. ) ;
#44472 = DIRECTION ( 'NONE',  ( -1.000000000000000000, 0.000000000000000000, 0.000000000000000000 ) ) ;
#44473 = CARTESIAN_POINT ( 'NONE',  ( 54.66064891145139626, -45.76208697842928785, 10.84999999999999964 ) ) ;
#44474 = CARTESIAN_POINT ( 'NONE',  ( 15.02108337061823740, -8.917202890402387894, -33.90037646791326864 ) ) ;
#44475 = CARTESIAN_POINT ( 'NONE',  ( 82.75389963950320293, -45.59493862562369770, -47.67227237921210303 ) ) ;
#44476 = CARTESIAN_POINT ( 'NONE',  ( 9.868248963658528439, -10.89094862918750017, -57.21816999718339503 ) ) ;
#44477 = CARTESIAN_POINT ( 'NONE',  ( 41.70176439649490163, -44.27974353495149984, -4.832746683949399547 ) ) ;
#44478 = CARTESIAN_POINT ( 'NONE',  ( 57.00722761779879733, 13.88381105532070059, -15.97596069844019873 ) ) ;
#44479 = LINE ( 'NONE', #24533, #18176 ) ;
#44480 = ADVANCED_FACE ( 'NONE', ( #4562 ), #44661, .T. ) ;
#44481 = AXIS2_PLACEMENT_3D ( 'NONE', #41588, #17996, #9626 ) ;
#44482 =( BOUNDED_CURVE ( )  B_SPLINE_CURVE ( 3, ( #44507, #15448, #40062, #35867 ),
 .UNSPECIFIED., .F., .T. ) 
 B_SPLINE_CURVE_WITH_KNOTS ( ( 4, 4 ),
 ( 3.323007232337010119, 3.540281829795995261 ),
 .UNSPECIFIED. ) 
 CURVE ( )  GEOMETRIC_REPRESENTATION_ITEM ( )  RATIONAL_B_SPLINE_CURVE ( ( 1.000000000000000000, 0.9960698467165439718, 0.9960698467165439718, 1.000000000000000000 ) ) 
 REPRESENTATION_ITEM ( '' )  );
#44483 = B_SPLINE_CURVE_WITH_KNOTS ( 'NONE', 3,
 ( #47657, #47915, #20112, #40557, #209, #36106, #51841, #716, #16706, #48692, #32663, #40816, #12794, #16190, #48426, #43722, #24540, #23776 ),
 .UNSPECIFIED., .F., .F.,
 ( 4, 2, 2, 2, 2, 2, 2, 2, 4 ),
 ( 0.000000000000000000, 0.06250018575575970459, 0.1250003715115194092, 0.1875005572672791276, 0.2500007430230388183, 0.3125009287787984258, 0.3750011145345580332, 0.4375013002903175852, 0.5000014860460771926 ),
 .UNSPECIFIED. ) ;
#44484 = AXIS2_PLACEMENT_3D ( 'NONE', #48233, #16510, #12329 ) ;
#44485 = CARTESIAN_POINT ( 'NONE',  ( 16.51210842463260065, -8.573494442655439585, -56.36425564602360083 ) ) ;
#44486 = CARTESIAN_POINT ( 'NONE',  ( 18.30487665358372240, -52.23919279727024190, -75.65449996337102334 ) ) ;
#44487 = AXIS2_PLACEMENT_3D ( 'NONE', #11482, #27439, #39004 ) ;
#44488 = EDGE_CURVE ( 'NONE', #19762, #43431, #25842, .T. ) ;
#44489 = ORIENTED_EDGE ( 'NONE', *, *, #25958, .F. ) ;
#44490 = CARTESIAN_POINT ( 'NONE',  ( 13.61616881089470077, -51.88814251562879321, -75.11575902016450357 ) ) ;
#44491 = CARTESIAN_POINT ( 'NONE',  ( 47.23304785971389919, -54.76875619474640189, -54.67497879625340573 ) ) ;
#44492 = SURFACE_STYLE_USAGE ( .BOTH. , #3894 ) ;
#44493 = CARTESIAN_POINT ( 'NONE',  ( 10.79909669266985617, 33.81695037846098018, -47.18321592281282761 ) ) ;
#44494 = DIRECTION ( 'NONE',  ( 1.000000000000000000, 0.000000000000000000, 0.000000000000000000 ) ) ;
#44495 = CARTESIAN_POINT ( 'NONE',  ( 23.33463543114514849, -12.22107770882397482, -55.36731066630095910 ) ) ;
#44496 = CARTESIAN_POINT ( 'NONE',  ( 57.36082898843075384, 14.38365649012001768, -26.19484475583911021 ) ) ;
#44497 = DIRECTION ( 'NONE',  ( 0.000000000000000000, 0.000000000000000000, -1.000000000000000000 ) ) ;
#44499 = CARTESIAN_POINT ( 'NONE',  ( 11.18117724951066094, 32.79411394922273359, -24.11551136640916582 ) ) ;
#44498 = CARTESIAN_POINT ( 'NONE',  ( 47.29473060385306837, 22.86193303853967151, -75.51963295297495904 ) ) ;
#44500 = CARTESIAN_POINT ( 'NONE',  ( 24.04493739635935512, -15.61397715763259164, -71.50758368266318143 ) ) ;
#44501 = CARTESIAN_POINT ( 'NONE',  ( 48.76908445385270596, 22.82217318232579828, -55.30112621652450144 ) ) ;
#44502 = VERTEX_POINT ( 'NONE', #36789 ) ;
#44503 = CARTESIAN_POINT ( 'NONE',  ( 21.21177448402870169, -10.72148469425540007, -64.60302447664000169 ) ) ;
#44504 = ORIENTED_EDGE ( 'NONE', *, *, #11071, .T. ) ;
#44505 = DIRECTION ( 'NONE',  ( 0.000000000000000000, 1.000000000000000000, 0.000000000000000000 ) ) ;
#44506 = CARTESIAN_POINT ( 'NONE',  ( 65.02936113742819657, 1.390208944942409985, -61.02997314496759884 ) ) ;
#44507 = CARTESIAN_POINT ( 'NONE',  ( 11.93174526809839975, 34.20691394249479345, -17.93019253464870033 ) ) ;
#44509 = CARTESIAN_POINT ( 'NONE',  ( 54.60893606919109544, 16.53358082662880335, -26.40962254079889959 ) ) ;
#44508 = CARTESIAN_POINT ( 'NONE',  ( 83.45793240077850328, 13.44987206900269960, -46.53859470524319875 ) ) ;
#44510 = CARTESIAN_POINT ( 'NONE',  ( 9.240841536127231137, -14.12361126166039860, -63.52069670119340827 ) ) ;
#44511 = CARTESIAN_POINT ( 'NONE',  ( 52.63952980978569940, 18.56936772728549911, -48.69585515676859444 ) ) ;
#44512 = CARTESIAN_POINT ( 'NONE',  ( 55.16770328537340617, -45.48138187130849985, -15.50413919957330044 ) ) ;
#44513 = CARTESIAN_POINT ( 'NONE',  ( 8.222732946675209931, -15.61637358666110131, -80.79233150823698395 ) ) ;
#44514 = ORIENTED_EDGE ( 'NONE', *, *, #41390, .F. ) ;
#44515 = ORIENTED_EDGE ( 'NONE', *, *, #1215, .F. ) ;
#44516 = CARTESIAN_POINT ( 'NONE',  ( 11.90855646482620145, -65.23144919529680408, -16.85546526173629900 ) ) ;
#44517 = CARTESIAN_POINT ( 'NONE',  ( 12.36168672466449969, 34.19959952941539427, -47.41183413623420506 ) ) ;
#44518 = CARTESIAN_POINT ( 'NONE',  ( 61.31733475858135307, -45.31597754466083927, -47.18612592330886457 ) ) ;
#44519 = AXIS2_PLACEMENT_3D ( 'NONE', #23980, #24233, #40004 ) ;
#44520 = CARTESIAN_POINT ( 'NONE',  ( 52.94338268357279986, -49.52467429185519876, -48.62015017847210174 ) ) ;
#44521 = CARTESIAN_POINT ( 'NONE',  ( 11.59132828503483026, -65.36240846161591378, -22.55862962361555546 ) ) ;
#44522 = CARTESIAN_POINT ( 'NONE',  ( 61.51122975691189509, -45.14516155341349446, -28.15000000000000213 ) ) ;
#44523 = AXIS2_PLACEMENT_3D ( 'NONE', #25020, #44190, #5151 ) ;
#44524 = ORIENTED_EDGE ( 'NONE', *, *, #22383, .T. ) ;
#44525 = DIRECTION ( 'NONE',  ( 0.000000000000000000, 1.000000000000000000, 0.000000000000000000 ) ) ;
#44526 = CARTESIAN_POINT ( 'NONE',  ( 10.97826455356500119, -63.19059205414950497, -44.74194573736729552 ) ) ;
#44527 = EDGE_CURVE ( 'NONE', #12539, #37063, #5828, .T. ) ;
#44528 = CARTESIAN_POINT ( 'NONE',  ( 17.16947398661607593, -23.52719049786522376, -59.96602729019871703 ) ) ;
#44529 = CARTESIAN_POINT ( 'NONE',  ( 72.40210087067039524, 1.451792515613489876, -69.49977495595670973 ) ) ;
#44530 = CARTESIAN_POINT ( 'NONE',  ( 50.20000625561069540, -49.66915949483620096, -76.14999999999999147 ) ) ;
#44531 = EDGE_CURVE ( 'NONE', #33105, #44858, #36015, .T. ) ;
#44532 = CARTESIAN_POINT ( 'NONE',  ( 8.222262383277058717, -15.61618471288229948, -44.50766849176299900 ) ) ;
#44533 = B_SPLINE_CURVE_WITH_KNOTS ( 'NONE', 3,
 ( #42171, #10462, #35059, #42435 ),
 .UNSPECIFIED., .F., .F.,
 ( 4, 4 ),
 ( 0.000000000000000000, 1.000000000000000000 ),
 .UNSPECIFIED. ) ;
#44534 = ORIENTED_EDGE ( 'NONE', *, *, #5712, .F. ) ;
#44535 = CARTESIAN_POINT ( 'NONE',  ( 17.25678305769739751, -43.96113075119600211, -62.64999999999999858 ) ) ;
#44536 = CARTESIAN_POINT ( 'NONE',  ( 47.13393739769619373, -39.28050807707779768, -35.14999999999999858 ) ) ;
#44537 = CARTESIAN_POINT ( 'NONE',  ( 2.428024600086250206, -25.79661907562860179, -34.95504743437649608 ) ) ;
#44538 = CARTESIAN_POINT ( 'NONE',  ( 18.29186039705039946, -23.57395800295140020, -72.20804185874750658 ) ) ;
#44539 = CARTESIAN_POINT ( 'NONE',  ( 13.81959240756670049, -51.26308380449479785, -23.06522851520879769 ) ) ;
#44540 = CARTESIAN_POINT ( 'NONE',  ( 54.72927025131360068, 19.84196400840209762, -75.36035929567221103 ) ) ;
#44541 = SHAPE_DEFINITION_REPRESENTATION ( #14437, #28088 ) ;
#44542 = CARTESIAN_POINT ( 'NONE',  ( 47.44049510014409776, -54.50743786567679905, -74.80726814568210159 ) ) ;
#44543 = ORIENTED_EDGE ( 'NONE', *, *, #45907, .T. ) ;
#44544 = CARTESIAN_POINT ( 'NONE',  ( 14.84020896475909979, -8.279094114505989310, -65.67710173045101385 ) ) ;
#44545 = FACE_OUTER_BOUND ( 'NONE', #23169, .T. ) ;
#44546 = CARTESIAN_POINT ( 'NONE',  ( 54.17308945056809932, 21.38381105532069881, -77.01198594424270993 ) ) ;
#44547 = EDGE_CURVE ( 'NONE', #9596, #17738, #47854, .T. ) ;
#44548 = CARTESIAN_POINT ( 'NONE',  ( 47.27157656634140181, 23.02640076397910107, -75.35698732394219235 ) ) ;
#44549 = ADVANCED_FACE ( 'NONE', ( #44146 ), #12182, .T. ) ;
#44550 = CARTESIAN_POINT ( 'NONE',  ( 71.09849264842429761, 1.384887413063060180, -60.98363600610959878 ) ) ;
#44551 = CARTESIAN_POINT ( 'NONE',  ( 75.04939620295753855, -19.22741391667048561, -11.30491871076487875 ) ) ;
#44552 = VECTOR ( 'NONE', #2189, 1000.000000000000000 ) ;
#44553 = VECTOR ( 'NONE', #7357, 1000.000000000000000 ) ;
#44554 = CARTESIAN_POINT ( 'NONE',  ( -5.066062602303800233, -15.61618894467930119, -10.44999999999999929 ) ) ;
#44555 = AXIS2_PLACEMENT_3D ( 'NONE', #38370, #18959, #18447 ) ;
#44556 = CARTESIAN_POINT ( 'NONE',  ( 14.76155815278458405, -49.61616749541425975, -83.19923667295616099 ) ) ;
#44557 = CARTESIAN_POINT ( 'NONE',  ( 57.24934407037070372, -50.61618894527409651, -74.14876594678160870 ) ) ;
#44559 = DIRECTION ( 'NONE',  ( 1.000000000000000000, 0.000000000000000000, 0.000000000000000000 ) ) ;
#44558 = CARTESIAN_POINT ( 'NONE',  ( 16.13393739769620083, -15.61618894467929941, 14.62639320225000006 ) ) ;
#44560 = CARTESIAN_POINT ( 'NONE',  ( 63.14473109323350286, 1.096110717717199812, -68.90857121967530929 ) ) ;
#44561 = CARTESIAN_POINT ( 'NONE',  ( 61.36075333576579993, 13.96751052759550049, -46.61068689941740217 ) ) ;
#44562 = CARTESIAN_POINT ( 'NONE',  ( -12.15512026601220086, -55.59619837851330004, -51.32444474606690221 ) ) ;
#44563 = ORIENTED_EDGE ( 'NONE', *, *, #34960, .F. ) ;
#44564 = CARTESIAN_POINT ( 'NONE',  ( 52.84703211352019991, -49.65186917973220204, -48.63862332596730198 ) ) ;
#44565 = CARTESIAN_POINT ( 'NONE',  ( 57.50445365671880182, -45.11618913266270425, -25.33159055575459817 ) ) ;
#44566 = CARTESIAN_POINT ( 'NONE',  ( 28.63393739769619728, -22.83306730954970121, -34.64999999999999858 ) ) ;
#44567 = CARTESIAN_POINT ( 'NONE',  ( 56.48403040235340455, 14.55542443240409867, -26.04784922081150000 ) ) ;
#44568 = CARTESIAN_POINT ( 'NONE',  ( 16.22658542707289797, -23.06590471877949966, -80.72869863253859535 ) ) ;
#44569 = CARTESIAN_POINT ( 'NONE',  ( 51.01627429428619820, 19.33079967119669718, -76.16510837308341308 ) ) ;
#44570 = CARTESIAN_POINT ( 'NONE',  ( 53.10865791236649613, 18.28620130409879962, -48.88762731574559695 ) ) ;
#44571 = CARTESIAN_POINT ( 'NONE',  ( 70.99050876911339003, 1.383811055320669947, -70.34999999999999432 ) ) ;
#44572 = CARTESIAN_POINT ( 'NONE',  ( 42.93197233849399908, -42.55807683903039162, -3.187564294433600232 ) ) ;
#44573 = CARTESIAN_POINT ( 'NONE',  ( 74.94086307074489639, -45.11618894467940066, -15.31398699537819930 ) ) ;
#44574 = ORIENTED_EDGE ( 'NONE', *, *, #46767, .F. ) ;
#44575 = CARTESIAN_POINT ( 'NONE',  ( 22.90093475162459313, -15.62310159663111619, -40.45314972491761552 ) ) ;
#44576 = CARTESIAN_POINT ( 'NONE',  ( 72.98500336837570046, 1.331842543267529821, -68.70530175958410268 ) ) ;
#44577 = CARTESIAN_POINT ( 'NONE',  ( 47.60865874083440019, -54.51384904987570224, -54.69368874373819978 ) ) ;
#44578 = FACE_BOUND ( 'NONE', #48775, .T. ) ;
#44579 = CARTESIAN_POINT ( 'NONE',  ( 72.92981560451809742, 1.375383258925270136, -62.73515566246579311 ) ) ;
#44580 = CARTESIAN_POINT ( 'NONE',  ( 40.92757333388370000, 13.18145061293710008, -3.805844904963549880 ) ) ;
#44581 = CARTESIAN_POINT ( 'NONE',  ( 58.92073642956109580, -28.10798705511860263, -15.65000675586140311 ) ) ;
#44582 = CARTESIAN_POINT ( 'NONE',  ( 71.19761362482960010, 1.388189907116970101, -61.01613942410280345 ) ) ;
#44583 = CARTESIAN_POINT ( 'NONE',  ( 46.98749101202549383, 7.998570365497442936, -34.79644638567071269 ) ) ;
#44584 = CARTESIAN_POINT ( 'NONE',  ( 71.98371235365300436, 1.451792515613489876, -61.38183652702590365 ) ) ;
#44585 = LINE ( 'NONE', #5021, #36851 ) ;
#44586 = CARTESIAN_POINT ( 'NONE',  ( 65.11238450761909746, 1.383161449028130097, -70.33386915736640788 ) ) ;
#44587 = EDGE_LOOP ( 'NONE', ( #46120, #21562 ) ) ;
#44588 = ORIENTED_EDGE ( 'NONE', *, *, #3544, .F. ) ;
#44589 = CARTESIAN_POINT ( 'NONE',  ( 57.35590716318880311, 18.90417298996780104, -52.61987026769980247 ) ) ;
#44590 = EDGE_CURVE ( 'NONE', #10013, #19286, #20019, .T. ) ;
#44591 = CARTESIAN_POINT ( 'NONE',  ( 16.06904196025218567, -51.02878819236820362, -15.66677487260436230 ) ) ;
#44592 = ORIENTED_EDGE ( 'NONE', *, *, #37680, .F. ) ;
#44593 = FACE_OUTER_BOUND ( 'NONE', #42479, .T. ) ;
#44594 = CARTESIAN_POINT ( 'NONE',  ( 29.99034385824719706, -15.61618894467929941, -32.14999999999999858 ) ) ;
#44595 = DIRECTION ( 'NONE',  ( -0.2260571801428149230, 0.000000000000000000, 0.9741140340359946137 ) ) ;
#44596 = CARTESIAN_POINT ( 'NONE',  ( 52.36900551255840242, 19.49169383700370162, -76.35261119704479427 ) ) ;
#44597 = ORIENTED_EDGE ( 'NONE', *, *, #29453, .F. ) ;
#44598 = CARTESIAN_POINT ( 'NONE',  ( 16.13393739769629676, -15.61618894467929941, -20.75000000000000000 ) ) ;
#44599 = CARTESIAN_POINT ( 'NONE',  ( 41.97094584064922174, 6.386695846697909573, -80.46488821210131448 ) ) ;
#44600 = CARTESIAN_POINT ( 'NONE',  ( 60.77958717670829714, 14.50249311732349966, -47.75277892092170617 ) ) ;
#44601 = CARTESIAN_POINT ( 'NONE',  ( 7.890219331288808924, -15.46181116932459965, -44.79829171073519944 ) ) ;
#44602 = DIRECTION ( 'NONE',  ( 0.000000000000000000, -5.782411586589432581E-16, 1.000000000000000000 ) ) ;
#44603 = CARTESIAN_POINT ( 'NONE',  ( 42.96119562966075733, -37.77193556298957589, -75.51370607938744683 ) ) ;
#44604 = ORIENTED_EDGE ( 'NONE', *, *, #16854, .T. ) ;
#44605 = CARTESIAN_POINT ( 'NONE',  ( 23.04647467197195354, -19.60029406037446620, -41.95899769523001765 ) ) ;
#44606 = CARTESIAN_POINT ( 'NONE',  ( 11.41311105421049987, -9.852467598734330423, -33.51421571862140070 ) ) ;
#44607 = CARTESIAN_POINT ( 'NONE',  ( 40.92585300945609816, 14.21241371935070141, -5.903596487906789925 ) ) ;
#44608 = ADVANCED_FACE ( 'NONE', ( #28141 ), #47531, .T. ) ;
#44609 = AXIS2_PLACEMENT_3D ( 'NONE', #11304, #35660, #31440 ) ;
#44610 = EDGE_CURVE ( 'NONE', #25200, #19643, #10853, .T. ) ;
#44611 = CARTESIAN_POINT ( 'NONE',  ( 14.12708840369279883, 20.99064699730730155, -75.77237669558989808 ) ) ;
#44612 = CARTESIAN_POINT ( 'NONE',  ( 24.04492352372650998, -15.63331151564256416, -59.79301433380418018 ) ) ;
#44613 = DIRECTION ( 'NONE',  ( 0.000000000000000000, 0.000000000000000000, -1.000000000000000000 ) ) ;
#44614 = CARTESIAN_POINT ( 'NONE',  ( 63.92800470363879839, 1.456055302763120007, -69.58268673945899252 ) ) ;
#44615 = CARTESIAN_POINT ( 'NONE',  ( 19.48597052431479781, -23.14922250540550053, -43.87440179741569324 ) ) ;
#44616 = VERTEX_POINT ( 'NONE', #42224 ) ;
#44617 = CARTESIAN_POINT ( 'NONE',  ( 54.15165173585579339, -48.25669691649810034, -26.60605610731790094 ) ) ;
#44618 = CARTESIAN_POINT ( 'NONE',  ( 14.40169973177160045, -50.85784981463910270, -21.38758215361159998 ) ) ;
#44619 = DIRECTION ( 'NONE',  ( 0.2260571801428161165, -1.387778780781444597E-17, -0.9741140340359943917 ) ) ;
#44620 = CARTESIAN_POINT ( 'NONE',  ( 50.76363268875235235, -50.10650823822278710, 11.97999999999999865 ) ) ;
#44621 = DIRECTION ( 'NONE',  ( 0.000000000000000000, 0.7371541402007423249, 0.6757246285173452716 ) ) ;
#44622 = AXIS2_PLACEMENT_3D ( 'NONE', #6879, #29916, #6099 ) ;
#44623 = ORIENTED_EDGE ( 'NONE', *, *, #35057, .T. ) ;
#44624 = CARTESIAN_POINT ( 'NONE',  ( -9.502204115007360841, -43.71455336852960016, -5.942533345529509958 ) ) ;
#44625 = VECTOR ( 'NONE', #45305, 1000.000000000000000 ) ;
#44626 = CARTESIAN_POINT ( 'NONE',  ( 47.24676140008929082, 23.52564688271890248, -54.63827976033719835 ) ) ;
#44627 = CARTESIAN_POINT ( 'NONE',  ( 57.24929578595760660, 21.38381105532069881, -74.14999999999999147 ) ) ;
#44628 = CARTESIAN_POINT ( 'NONE',  ( 63.02016742692980245, 0.9209567800143640959, -62.51152384389749272 ) ) ;
#44629 = CARTESIAN_POINT ( 'NONE',  ( 57.27629350501299399, -50.59351780024810097, -53.60235144059989665 ) ) ;
#44630 = CARTESIAN_POINT ( 'NONE',  ( 10.90442930760440099, 33.77248995292200107, -17.54871770534860076 ) ) ;
#44631 = DIRECTION ( 'NONE',  ( -1.000000000000000000, -4.829924999999999738E-13, 7.800438000000000694E-12 ) ) ;
#44632 = CARTESIAN_POINT ( 'NONE',  ( -13.73674066540299954, -0.6797460008306699386, -46.71145918530370267 ) ) ;
#44633 = CARTESIAN_POINT ( 'NONE',  ( 71.51437757259260763, 1.412203896155519889, -61.12765129660999719 ) ) ;
#44634 = CARTESIAN_POINT ( 'NONE',  ( 53.97718803714800373, -49.20306630607990428, -49.10491108831829621 ) ) ;
#44635 = CARTESIAN_POINT ( 'NONE',  ( 68.13393739769840352, -50.61618894467879670, -73.25000000000220268 ) ) ;
#44636 = CARTESIAN_POINT ( 'NONE',  ( 11.68549127948460153, -10.14317847777680015, -80.12993496510929958 ) ) ;
#44637 = CARTESIAN_POINT ( 'NONE',  ( 17.21347160910390173, -53.11618894467930119, -76.14999999999999147 ) ) ;
#44638 = CARTESIAN_POINT ( 'NONE',  ( 24.04526354826459666, -15.61618910718878794, -73.50766907743336276 ) ) ;
#44639 = CARTESIAN_POINT ( 'NONE',  ( 71.33393739769628894, 1.883811055320669947, -70.34999999999999432 ) ) ;
#44640 = DIRECTION ( 'NONE',  ( 0.000000000000000000, 0.000000000000000000, -1.000000000000000000 ) ) ;
#44641 = ORIENTED_EDGE ( 'NONE', *, *, #4669, .T. ) ;
#44642 = CARTESIAN_POINT ( 'NONE',  ( 20.06565654289127210, 23.98759296397042462, -19.24283188815232037 ) ) ;
#44643 = CARTESIAN_POINT ( 'NONE',  ( 8.965489388580479613, 31.97191824437770080, -46.63273652527719548 ) ) ;
#44644 = DIRECTION ( 'NONE',  ( 0.000000000000000000, 0.000000000000000000, -1.000000000000000000 ) ) ;
#44645 = CARTESIAN_POINT ( 'NONE',  ( 66.89371529141759254, -30.40426478165719715, -17.19079369877330166 ) ) ;
#44646 = ORIENTED_EDGE ( 'NONE', *, *, #10659, .F. ) ;
#44647 = CARTESIAN_POINT ( 'NONE',  ( 18.45802431067919969, 20.88378464714680049, -75.46937177410659103 ) ) ;
#44648 = ORIENTED_EDGE ( 'NONE', *, *, #14607, .T. ) ;
#44649 = ORIENTED_EDGE ( 'NONE', *, *, #49271, .T. ) ;
#44650 = EDGE_CURVE ( 'NONE', #12905, #13888, #10718, .T. ) ;
#44651 = VERTEX_POINT ( 'NONE', #30917 ) ;
#44652 = CARTESIAN_POINT ( 'NONE',  ( 11.15446670767390103, -64.60906199386440107, -45.98375597346589672 ) ) ;
#44653 = DIRECTION ( 'NONE',  ( 0.000000000000000000, 0.000000000000000000, -1.000000000000000000 ) ) ;
#44654 = CARTESIAN_POINT ( 'NONE',  ( 22.23872575654229777, -19.32696879987259919, -81.23899999999999011 ) ) ;
#44655 = EDGE_CURVE ( 'NONE', #7182, #1986, #50084, .T. ) ;
#44656 = CARTESIAN_POINT ( 'NONE',  ( 61.48332870919479376, 13.96258771565810086, -46.85782488637240562 ) ) ;
#44657 = ADVANCED_FACE ( 'NONE', ( #6324 ), #30783, .F. ) ;
#44658 = ORIENTED_EDGE ( 'NONE', *, *, #32152, .T. ) ;
#44659 = CARTESIAN_POINT ( 'NONE',  ( 75.24807542847500486, 3.017609241400042386, -12.28055750973653737 ) ) ;
#44660 = ADVANCED_FACE ( 'NONE', ( #14694 ), #18877, .F. ) ;
#44661 = PLANE ( 'NONE',  #43342 ) ;
#44662 = ORIENTED_EDGE ( 'NONE', *, *, #2171, .T. ) ;
#44663 = CARTESIAN_POINT ( 'NONE',  ( 51.61134830314709632, -46.21250895552949345, -13.62813625026690012 ) ) ;
#44664 = DIRECTION ( 'NONE',  ( 0.9752630547764096214, 0.2208726751083120443, 0.008788366098654002215 ) ) ;
#44665 = LINE ( 'NONE', #7991, #26816 ) ;
#44666 = ORIENTED_EDGE ( 'NONE', *, *, #452, .F. ) ;
#44667 = VECTOR ( 'NONE', #49738, 1000.000000000000000 ) ;
#44668 = ORIENTED_EDGE ( 'NONE', *, *, #12004, .T. ) ;
#44669 = CARTESIAN_POINT ( 'NONE',  ( 57.55751162049570269, -50.48013859002959691, -53.20292136905285929 ) ) ;
#44671 = CARTESIAN_POINT ( 'NONE',  ( 68.38971107296249841, -30.11618894467929763, -18.15384911730639672 ) ) ;
#44670 = VECTOR ( 'NONE', #32903, 1000.000000000000000 ) ;
#44672 = CARTESIAN_POINT ( 'NONE',  ( 60.85636071390069901, 14.48090769567980018, -47.74754960808709825 ) ) ;
#44673 = CARTESIAN_POINT ( 'NONE',  ( 50.61935581471210099, 13.97259095194099920, -11.61330938592119999 ) ) ;
#44674 = EDGE_CURVE ( 'NONE', #39247, #28919, #51709, .T. ) ;
#44675 = CARTESIAN_POINT ( 'NONE',  ( -9.882013117715120032, -40.49932216338130075, -21.14999999999999858 ) ) ;
#44676 = CARTESIAN_POINT ( 'NONE',  ( -5.346827492566250228, 15.73560381583549628, -4.480328055642280205 ) ) ;
#44677 = CARTESIAN_POINT ( 'NONE',  ( 47.13393739769619373, -39.28050807707779768, -35.14999999999999858 ) ) ;
#44678 = DIRECTION ( 'NONE',  ( 0.000000000000000000, 0.000000000000000000, -1.000000000000000000 ) ) ;
#44679 = CARTESIAN_POINT ( 'NONE',  ( 13.22842670730820025, -8.326143964624399985, -62.66678235003330144 ) ) ;
#44680 = ORIENTED_EDGE ( 'NONE', *, *, #18450, .T. ) ;
#44681 = CARTESIAN_POINT ( 'NONE',  ( 18.02855964079333972, 1.282173023328747608, -34.84133294386911217 ) ) ;
#44682 = AXIS2_PLACEMENT_3D ( 'NONE', #43699, #23753, #16621 ) ;
#44683 = CARTESIAN_POINT ( 'NONE',  ( 23.43760361721939844, -49.11659379690700433, -34.68023162149790295 ) ) ;
#44684 = DIRECTION ( 'NONE',  ( 6.127627000000000503E-13, 6.320986000000000022E-13, -1.000000000000000000 ) ) ;
#44685 = CARTESIAN_POINT ( 'NONE',  ( 72.51142765151010394, 1.054781932184780002, -69.75391249758430945 ) ) ;
#44686 = CARTESIAN_POINT ( 'NONE',  ( 42.97066549866231355, -39.86336681541309446, -71.64106045580271598 ) ) ;
#44687 = ADVANCED_FACE ( 'NONE', ( #46687 ), #6579, .T. ) ;
#44688 = CARTESIAN_POINT ( 'NONE',  ( -0.1437508118503130761, -27.26413697273960679, -34.89146800830132378 ) ) ;
#44689 = CARTESIAN_POINT ( 'NONE',  ( 49.69686147736390325, -53.65630926590149841, -54.99388098410970116 ) ) ;
#44690 = CARTESIAN_POINT ( 'NONE',  ( -7.099872940393900045, 14.68218975379929958, -5.638321079196820129 ) ) ;
#44691 = AXIS2_PLACEMENT_3D ( 'NONE', #27282, #23330, #31197 ) ;
#44692 = CARTESIAN_POINT ( 'NONE',  ( 23.67181263347827525, -18.06420660938224998, -33.60759600576869843 ) ) ;
#44693 = CARTESIAN_POINT ( 'NONE',  ( 11.13393739769619906, 32.28996931002959769, -24.14942631645369886 ) ) ;
#44694 = CARTESIAN_POINT ( 'NONE',  ( 9.807823418024582907, -20.47793272903095030, -54.58399883035956890 ) ) ;
#44695 = VERTEX_POINT ( 'NONE', #13927 ) ;
#44696 = CIRCLE ( 'NONE', #16235, 1.000000000000000888 ) ;
#44697 = CARTESIAN_POINT ( 'NONE',  ( 23.40224892329179696, -17.25275299940979679, -49.13783902869439402 ) ) ;
#44698 = CARTESIAN_POINT ( 'NONE',  ( 64.54901150452390368, 0.9254890127232510144, -60.83838280017310041 ) ) ;
#44699 = EDGE_LOOP ( 'NONE', ( #11282, #15183, #15856, #32956 ) ) ;
#44700 = CARTESIAN_POINT ( 'NONE',  ( 16.00572161013059969, -8.564513971789514457, -34.34139281033760227 ) ) ;
#44701 = CARTESIAN_POINT ( 'NONE',  ( 60.43738122508229793, -45.77296434314530416, -47.62750683704569354 ) ) ;
#44702 = DIRECTION ( 'NONE',  ( 0.7071067811865470176, -8.659560562354926695E-17, 0.7071067811865480168 ) ) ;
#44703 = CARTESIAN_POINT ( 'NONE',  ( 50.47459370284350655, 19.05485954424960227, -76.14999999999999147 ) ) ;
#44705 = CARTESIAN_POINT ( 'NONE',  ( 44.62611405146211752, -33.15679615701111516, -45.47822973459005169 ) ) ;
#44704 = CARTESIAN_POINT ( 'NONE',  ( 42.57256523677698112, 8.591912734483669212, -73.56571430690956959 ) ) ;
#44706 = DIRECTION ( 'NONE',  ( 0.000000000000000000, 0.000000000000000000, 1.000000000000000000 ) ) ;
#44707 = CARTESIAN_POINT ( 'NONE',  ( -5.079266037900150188, -4.302480445694469857, -59.64999999999999147 ) ) ;
#44708 = ORIENTED_EDGE ( 'NONE', *, *, #3477, .F. ) ;
#44709 = CARTESIAN_POINT ( 'NONE',  ( 83.89463082533569604, -44.78225339558859730, -47.42987625071230440 ) ) ;
#44710 = ORIENTED_EDGE ( 'NONE', *, *, #48165, .F. ) ;
#44711 = ORIENTED_EDGE ( 'NONE', *, *, #28118, .F. ) ;
#44712 = VERTEX_POINT ( 'NONE', #26732 ) ;
#44713 = CARTESIAN_POINT ( 'NONE',  ( 61.73642837792289839, -45.13062012120709454, -46.64899561561870200 ) ) ;
#44714 = CARTESIAN_POINT ( 'NONE',  ( 11.93174526809839975, 34.20691394249479345, -17.93019253464870033 ) ) ;
#44715 = ADVANCED_FACE ( 'NONE', ( #14436 ), #30407, .T. ) ;
#44716 = CARTESIAN_POINT ( 'NONE',  ( 76.39394475779087657, -13.67985447755458850, -12.77041102619445923 ) ) ;
#44717 = CARTESIAN_POINT ( 'NONE',  ( 53.36408652092959670, -52.07595258546250250, -53.95637823904670682 ) ) ;
#44718 = ADVANCED_FACE ( 'NONE', ( #46429, #26473 ), #42490, .T. ) ;
#44719 = ORIENTED_EDGE ( 'NONE', *, *, #13913, .T. ) ;
#44720 = ORIENTED_EDGE ( 'NONE', *, *, #16902, .T. ) ;
#44721 = EDGE_CURVE ( 'NONE', #31721, #7977, #38034, .T. ) ;
#44722 = CARTESIAN_POINT ( 'NONE',  ( 60.70500520956166923, 28.95487886718607484, 16.35000000000000142 ) ) ;
#44723 = CARTESIAN_POINT ( 'NONE',  ( -5.866062602303812490, -15.61618894467929941, -54.64999999999999858 ) ) ;
#44724 = CARTESIAN_POINT ( 'NONE',  ( 12.74054237723616900, -9.433355499570044600, -66.18740309792794108 ) ) ;
#44725 = AXIS2_PLACEMENT_3D ( 'NONE', #20223, #51698, #24397 ) ;
#44726 = LINE ( 'NONE', #1224, #41153 ) ;
#44727 = CARTESIAN_POINT ( 'NONE',  ( 23.64088819150179077, -13.06712943445810104, -59.68817848589910824 ) ) ;
#44728 = DIRECTION ( 'NONE',  ( 0.000000000000000000, 1.000000000000000000, 0.000000000000000000 ) ) ;
#44729 = ORIENTED_EDGE ( 'NONE', *, *, #945, .T. ) ;
#44730 = DIRECTION ( 'NONE',  ( -6.958217999999999866E-13, 1.000000000000000000, -3.004664999999999799E-13 ) ) ;
#44731 = CARTESIAN_POINT ( 'NONE',  ( 53.96532960447419924, -50.61809440848099939, -76.95223789022560368 ) ) ;
#44732 = CARTESIAN_POINT ( 'NONE',  ( 60.33694438359644607, 14.62750282847424899, -47.70890968787152531 ) ) ;
#44733 = CARTESIAN_POINT ( 'NONE',  ( 60.48811175542340379, 14.41611557752919914, -47.17639167819340429 ) ) ;
#44734 = VECTOR ( 'NONE', #12795, 1000.000000000000000 ) ;
#44735 = CARTESIAN_POINT ( 'NONE',  ( 23.91605131074399893, -14.60354357934630087, -61.97130586100059446 ) ) ;
#44736 = DIRECTION ( 'NONE',  ( -1.000000000000000000, -7.841349000000000539E-12, -8.551771000000000195E-12 ) ) ;
#44737 = CARTESIAN_POINT ( 'NONE',  ( 68.13393739769618662, -28.66618894467939782, -65.65000000000000568 ) ) ;
#44738 = EDGE_CURVE ( 'NONE', #1196, #12484, #13267, .T. ) ;
#44739 = CARTESIAN_POINT ( 'NONE',  ( 42.88515050504339854, -43.77470902807130670, -4.897272209519029751 ) ) ;
#44740 = DIRECTION ( 'NONE',  ( -0.8660254037844387076, 0.4999999999999998890, 1.942890293094024439E-16 ) ) ;
#44741 = CARTESIAN_POINT ( 'NONE',  ( 57.50723902594879888, 13.88381105532070059, -17.67941225248179649 ) ) ;
#44742 = CARTESIAN_POINT ( 'NONE',  ( 68.03757084111694553, 0.7700511936776454069, -18.68196744858373037 ) ) ;
#44743 = CARTESIAN_POINT ( 'NONE',  ( 64.03570111260079045, 1.347758383967160078, -69.88143807632219762 ) ) ;
#44744 = CARTESIAN_POINT ( 'NONE',  ( 9.221496542177588296, -11.63191685418159693, -40.95899807896893918 ) ) ;
#44745 = CARTESIAN_POINT ( 'NONE',  ( 66.89373992269190694, -0.8281018005762210699, -17.19081051937810045 ) ) ;
#44746 = ORIENTED_EDGE ( 'NONE', *, *, #44753, .T. ) ;
#44747 = CARTESIAN_POINT ( 'NONE',  ( 14.48971970689060029, -51.52596624575240725, -75.36996982820370761 ) ) ;
#44748 = CARTESIAN_POINT ( 'NONE',  ( 47.29014113061550262, -54.72776004820889995, -54.71595221509849694 ) ) ;
#44749 = CARTESIAN_POINT ( 'NONE',  ( 22.90095859539430379, -15.61618916398383661, -38.45281773784812174 ) ) ;
#44750 = LINE ( 'NONE', #48427, #12952 ) ;
#44751 = CYLINDRICAL_SURFACE ( 'NONE', #26475, 7.910999999999997812 ) ;
#44753 = EDGE_CURVE ( 'NONE', #50005, #24458, #1547, .T. ) ;
#44752 = CARTESIAN_POINT ( 'NONE',  ( 23.20507000855700142, -18.04245328055489850, -32.14999999999999858 ) ) ;
#44754 = CARTESIAN_POINT ( 'NONE',  ( 29.11900864776890074, -4.497910611074960485, -35.02873218748179340 ) ) ;
#44756 = EDGE_CURVE ( 'NONE', #31721, #15986, #1464, .T. ) ;
#44755 = CARTESIAN_POINT ( 'NONE',  ( 47.76731554892809584, -54.45608225251359613, -54.88059270044120552 ) ) ;
#44757 = AXIS2_PLACEMENT_3D ( 'NONE', #33443, #16438, #41317 ) ;
#44759 = CARTESIAN_POINT ( 'NONE',  ( 18.20464644555056921, -23.32128070152664634, -52.20899666773274106 ) ) ;
#44758 = CARTESIAN_POINT ( 'NONE',  ( 47.26610112325450075, 22.82567072896360116, -75.56421356201970241 ) ) ;
#44760 = DIRECTION ( 'NONE',  ( 1.000000000000000000, 0.000000000000000000, 0.000000000000000000 ) ) ;
#44761 = CARTESIAN_POINT ( 'NONE',  ( 42.48652067987293179, 13.02449555953472426, -5.094659060785825311 ) ) ;
#44762 = CARTESIAN_POINT ( 'NONE',  ( 48.63180645979579708, 22.87900943640810070, -55.21523209561640044 ) ) ;
#44763 = EDGE_LOOP ( 'NONE', ( #10957, #30328, #1752 ) ) ;
#44764 = CARTESIAN_POINT ( 'NONE',  ( 12.99575412164399779, -21.93238755621440106, -63.49395944174919748 ) ) ;
#44765 = VERTEX_POINT ( 'NONE', #11289 ) ;
#44766 = DIRECTION ( 'NONE',  ( 1.000000000000000000, 0.000000000000000000, 0.000000000000000000 ) ) ;
#44767 = DIRECTION ( 'NONE',  ( -0.7286256507163790808, -0.6849121557675359462, 0.000000000000000000 ) ) ;
#44768 = DIRECTION ( 'NONE',  ( 0.000000000000000000, 0.000000000000000000, -1.000000000000000000 ) ) ;
#44770 = CARTESIAN_POINT ( 'NONE',  ( 53.19086730767300253, 17.98371808565390140, -27.08903680673190095 ) ) ;
#44769 = CARTESIAN_POINT ( 'NONE',  ( 83.93595989616819963, 13.02949184870690047, -46.83273212233100224 ) ) ;
#44771 = CARTESIAN_POINT ( 'NONE',  ( 12.88757487121280043, -21.87747388015940331, -65.10507532246559492 ) ) ;
#44772 = FACE_OUTER_BOUND ( 'NONE', #25805, .T. ) ;
#44773 = CARTESIAN_POINT ( 'NONE',  ( 57.39657356000389399, -45.11618894467940066, -17.44506318542070034 ) ) ;
#44774 = B_SPLINE_SURFACE_WITH_KNOTS ( 'NONE', 3, 3, ( 
 ( #33133, #49158, #37347, #13254 ),
 ( #21340, #51472, #15312, #38909 ),
 ( #22637, #10349, #30758, #42581 ),
 ( #46523, #31264, #39421, #38655 ),
 ( #3521, #26308, #22377, #35481 ),
 ( #27349, #35215, #2743, #31015 ),
 ( #26834, #15571, #10869, #11127 ),
 ( #2999, #31527, #51218, #26566 ),
 ( #3256, #42321, #2476, #14790 ),
 ( #34690, #46780, #43099, #43355 ),
 ( #42843, #23146, #6419, #39162 ),
 ( #18714, #18969, #47297, #15048 ) ),
 .UNSPECIFIED., .F., .F., .F.,
 ( 4, 1, 1, 1, 1, 1, 1, 1, 1, 4 ),
 ( 4, 4 ),
 ( 0.000000000000000000, 0.1111111111111110078, 0.2222222222222219878, 0.3333333333333329818, 0.4444444444444439757, 0.5555555555555560243, 0.6666666666666670737, 0.7777777777777779011, 0.8888888888888889506, 1.000000000000000000 ),
 ( -0.2043272503186320255, -0.05091814332707400581 ),
 .UNSPECIFIED. ) ;
#44775 = DIRECTION ( 'NONE',  ( 0.5685928097855380559, -0.5944782866685500711, -0.5685928097855370567 ) ) ;
#44776 = ORIENTED_EDGE ( 'NONE', *, *, #24084, .F. ) ;
#44777 = ORIENTED_EDGE ( 'NONE', *, *, #43436, .T. ) ;
#44778 = CARTESIAN_POINT ( 'NONE',  ( 12.06706412657270100, -65.03706746763299407, -16.41672221715840152 ) ) ;
#44779 = CARTESIAN_POINT ( 'NONE',  ( 12.01677611816480074, 34.07027331508780321, -47.05243182101040134 ) ) ;
#44780 = CARTESIAN_POINT ( 'NONE',  ( 18.54927880441067956, 20.10353310518733139, -15.71463296250362518 ) ) ;
#44781 = EDGE_CURVE ( 'NONE', #51621, #47003, #48212, .T. ) ;
#44782 = DIRECTION ( 'NONE',  ( -0.7052114458104683514, 0.7089970498513439301, 0.000000000000000000 ) ) ;
#44783 = CARTESIAN_POINT ( 'NONE',  ( 12.14992628989387313, -22.52878017980526693, -64.17433570710899460 ) ) ;
#44784 = AXIS2_PLACEMENT_3D ( 'NONE', #5901, #30249, #21601 ) ;
#44785 = ORIENTED_EDGE ( 'NONE', *, *, #11364, .F. ) ;
#44786 = EDGE_CURVE ( 'NONE', #40766, #22439, #42117, .T. ) ;
#44787 = CARTESIAN_POINT ( 'NONE',  ( 13.61938558678000000, 20.19483563406610216, -23.15000000000000213 ) ) ;
#44788 = CARTESIAN_POINT ( 'NONE',  ( 52.82975638541582697, 18.42854252836027484, -28.09160094008685604 ) ) ;
#44789 = CARTESIAN_POINT ( 'NONE',  ( -11.32734370190460105, -41.88171845330919751, -19.14999999999999858 ) ) ;
#44790 = CARTESIAN_POINT ( 'NONE',  ( 18.41199818135587307, -48.25922751448980819, -34.79644660940672907 ) ) ;
#44791 = CARTESIAN_POINT ( 'NONE',  ( 50.46752464413489747, -49.58022540544509837, -76.16325466874729955 ) ) ;
#44792 = CARTESIAN_POINT ( 'NONE',  ( 14.13393739769619906, -41.61618894467930119, -54.64999999999999858 ) ) ;
#44793 =( BOUNDED_CURVE ( )  B_SPLINE_CURVE ( 3, ( #39089, #23313, #15232, #33897 ),
 .UNSPECIFIED., .F., .T. ) 
 B_SPLINE_CURVE_WITH_KNOTS ( ( 4, 4 ),
 ( 5.936250502017659691, 6.279745795443859357 ),
 .UNSPECIFIED. ) 
 CURVE ( )  GEOMETRIC_REPRESENTATION_ITEM ( )  RATIONAL_B_SPLINE_CURVE ( ( 1.000000000000000000, 0.9901917273091168648, 0.9901917273091168648, 1.000000000000000000 ) ) 
 REPRESENTATION_ITEM ( '' )  );
#44794 = ORIENTED_EDGE ( 'NONE', *, *, #20385, .F. ) ;
#44795 = CARTESIAN_POINT ( 'NONE',  ( 54.34775236769140605, -47.86158002624119945, -25.94360105443890063 ) ) ;
#44796 = CARTESIAN_POINT ( 'NONE',  ( -18.86606260230360022, -50.61618894467959962, 11.97999999999999865 ) ) ;
#44797 = VERTEX_POINT ( 'NONE', #44273 ) ;
#44798 = CYLINDRICAL_SURFACE ( 'NONE', #28464, 1.999999999999999112 ) ;
#44799 = CARTESIAN_POINT ( 'NONE',  ( 0.3209249304026040028, 15.01904124785189865, -34.64999999999999858 ) ) ;
#44800 = CARTESIAN_POINT ( 'NONE',  ( 21.98482826927030231, -20.84627725470230075, -34.24467998873379315 ) ) ;
#44801 = AXIS2_PLACEMENT_3D ( 'NONE', #32204, #7881, #8647 ) ;
#44802 = CARTESIAN_POINT ( 'NONE',  ( 14.16335351432319989, -51.13178799427510768, -22.70850811651479972 ) ) ;
#44803 = CARTESIAN_POINT ( 'NONE',  ( 56.46547423300169299, 19.54384849142039826, -74.28346178225240237 ) ) ;
#44804 = CARTESIAN_POINT ( 'NONE',  ( 47.05561704033240034, -53.94108635855520362, -75.73967526752529977 ) ) ;
#44805 = ORIENTED_EDGE ( 'NONE', *, *, #42422, .T. ) ;
#44806 = CARTESIAN_POINT ( 'NONE',  ( 63.88393739769619373, 4.883811055320659733, -61.44999999999999574 ) ) ;
#44807 = CARTESIAN_POINT ( 'NONE',  ( 8.862687950201170395, -17.23964983963449882, -69.16273469725010159 ) ) ;
#44808 = DIRECTION ( 'NONE',  ( 0.000000000000000000, 0.000000000000000000, -1.000000000000000000 ) ) ;
#44809 = DIRECTION ( 'NONE',  ( 0.000000000000000000, 0.000000000000000000, -1.000000000000000000 ) ) ;
#44810 = CARTESIAN_POINT ( 'NONE',  ( 47.50309827252019801, 23.36724551378910064, -74.17369128426381053 ) ) ;
#44811 = CARTESIAN_POINT ( 'NONE',  ( 18.86789271272390067, -51.78678247029300508, -15.81497036395479761 ) ) ;
#44812 = CARTESIAN_POINT ( 'NONE',  ( 68.13393739769620083, -43.11618894467930119, -73.25000000000000000 ) ) ;
#44813 = CARTESIAN_POINT ( 'NONE',  ( 61.28610861176739633, 13.99802266614350010, -28.15000000000000213 ) ) ;
#44814 = EDGE_CURVE ( 'NONE', #7703, #26641, #14072, .T. ) ;
#44815 = DIRECTION ( 'NONE',  ( -0.9441882088883087887, 0.3294064756441308917, 0.000000000000000000 ) ) ;
#44817 = EDGE_CURVE ( 'NONE', #45450, #20524, #6690, .T. ) ;
#44816 = PLANE ( 'NONE',  #4947 ) ;
#44818 = CARTESIAN_POINT ( 'NONE',  ( 68.13393739769618662, -1.166188944679350081, -65.65000000000000568 ) ) ;
#44820 = DIRECTION ( 'NONE',  ( -3.532868000000000128E-12, 2.963302999999999818E-13, 1.000000000000000000 ) ) ;
#44819 = CARTESIAN_POINT ( 'NONE',  ( 61.13393739769620083, 1.883811055320649963, -84.38499399519520239 ) ) ;
#44821 = MANIFOLD_SOLID_BREP ( 'Stock-MAS-691-1', #40188 ) ;
#44822 = CARTESIAN_POINT ( 'NONE',  ( 63.11679429741250402, 0.8888742037077569380, -68.94068779328439689 ) ) ;
#44823 = CARTESIAN_POINT ( 'NONE',  ( 61.32721378439150328, 13.97792828797489939, -46.50571435523870178 ) ) ;
#44824 = CARTESIAN_POINT ( 'NONE',  ( -32.51565489538130294, -20.32396912357229724, -55.84912116621229927 ) ) ;
#44825 = ADVANCED_FACE ( 'NONE', ( #17280, #49000 ), #19901, .T. ) ;
#44826 = ORIENTED_EDGE ( 'NONE', *, *, #921, .T. ) ;
#44827 = CARTESIAN_POINT ( 'NONE',  ( 52.99768783924589854, -49.57341479806719775, -48.81581856325809810 ) ) ;
#44828 = B_SPLINE_CURVE_WITH_KNOTS ( 'NONE', 3,
 ( #40118, #11838, #27798, #27283, #36173, #16265, #281, #26306, #34430, #5259, #28297, #16517, #36682, #20692, #4727, #32732, #21211, #13384 ),
 .UNSPECIFIED., .F., .F.,
 ( 4, 2, 2, 2, 2, 2, 2, 2, 4 ),
 ( 0.000000000000000000, 0.06250011819343853636, 0.1250002363868770727, 0.1875003545803156091, 0.2500004727737541455, 0.3125005909671927928, 0.3750007091606314402, 0.4375008273540700876, 0.5000009455475087350 ),
 .UNSPECIFIED. ) ;
#44829 = CARTESIAN_POINT ( 'NONE',  ( 61.41965047412389822, -45.13055029907879856, -27.46561386188539799 ) ) ;
#44830 = AXIS2_PLACEMENT_3D ( 'NONE', #44812, #28288, #1047 ) ;
#44831 = CARTESIAN_POINT ( 'NONE',  ( 8.223247527389670353, -15.61637340300369914, -74.79233150823711185 ) ) ;
#44832 = CARTESIAN_POINT ( 'NONE',  ( 13.50712872756970029, 19.81166641576820098, -21.90151629162349778 ) ) ;
#44833 = CARTESIAN_POINT ( 'NONE',  ( 57.21513657066689973, 14.40326995541390076, -26.18061821942099954 ) ) ;
#44834 = CARTESIAN_POINT ( 'NONE',  ( 21.92791489578599951, -19.63767914711110052, -38.64595234721679162 ) ) ;
#44835 = CARTESIAN_POINT ( 'NONE',  ( 50.39203494153080243, 18.10371503980149654, -76.16300746228739627 ) ) ;
#44836 = CARTESIAN_POINT ( 'NONE',  ( 52.73806344804810209, 18.48670660044059844, -48.65316599148000165 ) ) ;
#44837 = CARTESIAN_POINT ( 'NONE',  ( 71.29497000743199919, 0.8840451408750739093, -70.74985906855570761 ) ) ;
#44838 = CARTESIAN_POINT ( 'NONE',  ( 67.22839177940861077, -44.96269340666319891, -12.13170577700170050 ) ) ;
#44839 = TOROIDAL_SURFACE ( 'NONE', #51533, 39.99999906195129995, 1.999999997951819930 ) ;
#44840 = ORIENTED_EDGE ( 'NONE', *, *, #24673, .F. ) ;
#44841 = FACE_OUTER_BOUND ( 'NONE', #17753, .T. ) ;
#44842 = CARTESIAN_POINT ( 'NONE',  ( 23.26606227162260154, -17.77013627947239982, -71.16070186438059864 ) ) ;
#44843 = CARTESIAN_POINT ( 'NONE',  ( 72.75396425272869294, 1.390208944942409985, -68.75457626026799574 ) ) ;
#44844 = CARTESIAN_POINT ( 'NONE',  ( 47.47423769629730117, -54.59780520654420144, -54.66828950685410149 ) ) ;
#44845 = CARTESIAN_POINT ( 'NONE',  ( 16.13393739769620083, -15.61618894467929941, 17.07360679774999923 ) ) ;
#44846 = CARTESIAN_POINT ( 'NONE',  ( 16.13393739769620083, -15.61618894467929941, -31.39999999999999858 ) ) ;
#44847 = CARTESIAN_POINT ( 'NONE',  ( 60.64534134237799634, 14.90352494164799957, -48.24433635901220185 ) ) ;
#44848 = CARTESIAN_POINT ( 'NONE',  ( 71.43836573789050703, 0.9955677559369568996, -60.65081522799539471 ) ) ;
#44849 = DIRECTION ( 'NONE',  ( -1.000000000000000000, 0.000000000000000000, 0.000000000000000000 ) ) ;
#44850 = CARTESIAN_POINT ( 'NONE',  ( 71.59128680196450034, 1.230946250268210029, -60.87529647521710530 ) ) ;
#44851 = CARTESIAN_POINT ( 'NONE',  ( 24.03381973957637285, -16.06908004449718419, -71.52589682854927844 ) ) ;
#44852 = EDGE_CURVE ( 'NONE', #11156, #37266, #15854, .T. ) ;
#44853 = CARTESIAN_POINT ( 'NONE',  ( 64.92925538503580185, 1.097085799869280009, -70.67221403600389351 ) ) ;
#44854 = ORIENTED_EDGE ( 'NONE', *, *, #38639, .F. ) ;
#44855 = ORIENTED_EDGE ( 'NONE', *, *, #5517, .T. ) ;
#44856 = CARTESIAN_POINT ( 'NONE',  ( 8.964272521377070646, -63.19719428634219582, -46.63279896585060413 ) ) ;
#44857 = CARTESIAN_POINT ( 'NONE',  ( 16.13393739769620083, -15.61618894467929941, 4.450000000000000178 ) ) ;
#44858 = VERTEX_POINT ( 'NONE', #24586 ) ;
#44859 = DIRECTION ( 'NONE',  ( 0.000000000000000000, 0.000000000000000000, -1.000000000000000000 ) ) ;
#44860 = CARTESIAN_POINT ( 'NONE',  ( 12.72591284326311190, -9.703296205089767312, -69.78615459468322513 ) ) ;
#44861 = CARTESIAN_POINT ( 'NONE',  ( 21.80687142448134352, -11.85343762274402124, -50.26656186468857612 ) ) ;
#44862 = CARTESIAN_POINT ( 'NONE',  ( 51.82414486449059865, 18.95706542269019579, -76.50963458223939995 ) ) ;
#44863 = ORIENTED_EDGE ( 'NONE', *, *, #26844, .T. ) ;
#44864 = DIRECTION ( 'NONE',  ( 9.209768215203483886E-28, -6.141198660767589922E-12, -1.000000000000000000 ) ) ;
#44866 = CARTESIAN_POINT ( 'NONE',  ( 42.10651587289341080, 6.408251961395291296, -79.78705605499216347 ) ) ;
#44865 = VECTOR ( 'NONE', #40839, 1000.000000000000000 ) ;
#44867 = CARTESIAN_POINT ( 'NONE',  ( 20.99564994467235479, -9.290051249912700371, -35.21599968409613268 ) ) ;
#44868 = CARTESIAN_POINT ( 'NONE',  ( 24.25483720920119879, -17.04226969534990133, -43.84766453797169561 ) ) ;
#44869 = CARTESIAN_POINT ( 'NONE',  ( 22.90070561427262064, -15.61618657793558818, -56.45282510079097449 ) ) ;
#44870 = CARTESIAN_POINT ( 'NONE',  ( 42.64634278043503457, -37.72488185585652332, -77.08790612488995464 ) ) ;
#44871 = EDGE_LOOP ( 'NONE', ( #45333, #36425, #29999, #33364, #664 ) ) ;
#44872 = CARTESIAN_POINT ( 'NONE',  ( 11.02107559592020003, -63.90702541208909082, -23.99273296026720104 ) ) ;
#44873 = CARTESIAN_POINT ( 'NONE',  ( 8.729467296546598476, -16.44112522791030173, -33.19733999436699889 ) ) ;
#44874 = CARTESIAN_POINT ( 'NONE',  ( 11.19819258504769977, -10.83938507832420051, -32.14999999999999858 ) ) ;
#44875 = B_SPLINE_CURVE_WITH_KNOTS ( 'NONE', 3,
 ( #21460, #37983, #1558, #42174 ),
 .UNSPECIFIED., .F., .F.,
 ( 4, 4 ),
 ( 0.000000000000000000, 1.000000000000000000 ),
 .UNSPECIFIED. ) ;
#44876 = VECTOR ( 'NONE', #51026, 1000.000000000000000 ) ;
#44877 = CARTESIAN_POINT ( 'NONE',  ( 14.30169396435220008, 21.24161264671329974, -75.93682688742939035 ) ) ;
#44878 = FACE_OUTER_BOUND ( 'NONE', #28976, .T. ) ;
#44879 = CARTESIAN_POINT ( 'NONE',  ( 83.53868183867639630, -44.62159407410370449, -46.56548196350899360 ) ) ;
#44880 = CARTESIAN_POINT ( 'NONE',  ( 21.21552280508710098, -22.10927838317979877, -51.79629490377759993 ) ) ;
#44881 = ORIENTED_EDGE ( 'NONE', *, *, #41647, .T. ) ;
#44882 = CARTESIAN_POINT ( 'NONE',  ( 52.77203259569630234, -49.67394356405169731, -27.82577599984929861 ) ) ;
#44883 = ADVANCED_FACE ( 'NONE', ( #4696 ), #13352, .F. ) ;
#44884 = CARTESIAN_POINT ( 'NONE',  ( 16.13393739769620083, -15.61618894467929941, -44.64999999999999858 ) ) ;
#44885 = CARTESIAN_POINT ( 'NONE',  ( 23.83903856107666641, -17.68686005063226574, -63.87566687503874618 ) ) ;
#44886 = CARTESIAN_POINT ( 'NONE',  ( 17.01966273183835199, -22.38319939417082338, -56.91109783820547108 ) ) ;
#44887 = CYLINDRICAL_SURFACE ( 'NONE', #48293, 10.00000000000000888 ) ;
#44888 = ORIENTED_EDGE ( 'NONE', *, *, #12550, .F. ) ;
#44889 = CARTESIAN_POINT ( 'NONE',  ( -10.41395375019419944, -42.81708513381939696, -6.102688242772109639 ) ) ;
#44890 = CARTESIAN_POINT ( 'NONE',  ( 47.35959481792740178, 23.44442529656140195, -54.67024274119960126 ) ) ;
#44891 = CIRCLE ( 'NONE', #49067, 6.100000000000001421 ) ;
#44892 = CARTESIAN_POINT ( 'NONE',  ( 55.92134356540361040, -45.89757597650480392, -25.32475626239351740 ) ) ;
#44893 = CARTESIAN_POINT ( 'NONE',  ( 63.20402522475220053, 1.187237555532410171, -62.39609834743819761 ) ) ;
#44894 = CARTESIAN_POINT ( 'NONE',  ( 18.13393739769599833, 14.38381105532070059, -35.14999999999999858 ) ) ;
#44895 = CARTESIAN_POINT ( 'NONE',  ( 10.89208540626749944, 33.76849045686219597, -17.57297890437990162 ) ) ;
#44896 = CARTESIAN_POINT ( 'NONE',  ( 63.43393739769620510, 0.8838110553206759423, -68.50657137141709541 ) ) ;
#44897 = CARTESIAN_POINT ( 'NONE',  ( 72.27703085588929355, 1.458412159422780130, -61.64333151374460584 ) ) ;
#44898 = CARTESIAN_POINT ( 'NONE',  ( 53.94120575207560364, -49.17518334734650409, -49.03324901303680150 ) ) ;
#44899 = AXIS2_PLACEMENT_3D ( 'NONE', #29859, #14929, #26193 ) ;
#44900 = CARTESIAN_POINT ( 'NONE',  ( 52.83863466997060243, 18.42092259931630238, -28.03264406027369660 ) ) ;
#44901 = CARTESIAN_POINT ( 'NONE',  ( 17.32335564108290171, -52.96147345225150360, -76.14999999999999147 ) ) ;
#44902 = EDGE_CURVE ( 'NONE', #31815, #21944, #39620, .T. ) ;
#44903 = CARTESIAN_POINT ( 'NONE',  ( 17.92370450339669929, -52.11618894467930119, -74.14999999999999147 ) ) ;
#44904 = CARTESIAN_POINT ( 'NONE',  ( 9.638313984568736004, -18.10068106752252604, -61.73034261279407531 ) ) ;
#44905 = VERTEX_POINT ( 'NONE', #40596 ) ;
#44906 = DIRECTION ( 'NONE',  ( 0.000000000000000000, 0.000000000000000000, 1.000000000000000000 ) ) ;
#44907 = CARTESIAN_POINT ( 'NONE',  ( 8.966094888256401774, 31.97546849540949765, -46.63271503358079428 ) ) ;
#44908 = FACE_OUTER_BOUND ( 'NONE', #20198, .T. ) ;
#44909 = DIRECTION ( 'NONE',  ( 0.000000000000000000, 0.000000000000000000, 1.000000000000000000 ) ) ;
#44910 = ORIENTED_EDGE ( 'NONE', *, *, #14498, .F. ) ;
#44911 = EDGE_CURVE ( 'NONE', #13981, #51663, #9882, .T. ) ;
#44912 = CARTESIAN_POINT ( 'NONE',  ( 18.42162172276690058, 20.91303491124869751, -75.51792558472189398 ) ) ;
#44913 = AXIS2_PLACEMENT_3D ( 'NONE', #27272, #27785, #15236 ) ;
#44914 = EDGE_LOOP ( 'NONE', ( #14038, #39759, #593, #10417 ) ) ;
#44915 = ORIENTED_EDGE ( 'NONE', *, *, #14061, .F. ) ;
#44916 = EDGE_CURVE ( 'NONE', #26391, #9424, #42567, .T. ) ;
#44917 = EDGE_LOOP ( 'NONE', ( #38118, #29675, #11791, #50716, #37558 ) ) ;
#44918 = CARTESIAN_POINT ( 'NONE',  ( 11.54287861353399869, -64.87899921766438638, -45.94746754196619776 ) ) ;
#44919 = CARTESIAN_POINT ( 'NONE',  ( 57.31690520220239193, -45.30894883373459692, -25.91066051893669808 ) ) ;
#44920 = CARTESIAN_POINT ( 'NONE',  ( 22.61477114348110007, -18.74635927958349768, -81.23899999999999011 ) ) ;
#44921 = CARTESIAN_POINT ( 'NONE',  ( 8.222953192759320018, -14.58052584272395436, -62.54933522701458770 ) ) ;
#44922 = CARTESIAN_POINT ( 'NONE',  ( 61.69575994152130249, 13.91829368062330019, -46.74341057651110276 ) ) ;
#44923 = CARTESIAN_POINT ( 'NONE',  ( 64.36679430080839381, 1.446932438105809737, -61.32315308161489753 ) ) ;
#44924 = ORIENTED_EDGE ( 'NONE', *, *, #42495, .T. ) ;
#44925 = ORIENTED_EDGE ( 'NONE', *, *, #3906, .F. ) ;
#44926 = DIRECTION ( 'NONE',  ( 0.000000000000000000, -1.000000000000000000, 0.000000000000000000 ) ) ;
#44927 = ORIENTED_EDGE ( 'NONE', *, *, #43073, .T. ) ;
#44928 = CARTESIAN_POINT ( 'NONE',  ( 53.39341508398250369, -46.23762566829479681, -14.95068794128250111 ) ) ;
#44929 = AXIS2_PLACEMENT_3D ( 'NONE', #30757, #41789, #14276 ) ;
#44930 = DIRECTION ( 'NONE',  ( 0.3863301728269178947, 0.9223605572462016955, 0.000000000000000000 ) ) ;
#44931 = CARTESIAN_POINT ( 'NONE',  ( 22.90066504558609850, -15.61618132107965984, -48.84717678326153845 ) ) ;
#44932 = ORIENTED_EDGE ( 'NONE', *, *, #29324, .T. ) ;
#44933 = ORIENTED_EDGE ( 'NONE', *, *, #39955, .F. ) ;
#44934 = CARTESIAN_POINT ( 'NONE',  ( 72.77636315587029969, 1.387131204727290124, -62.61203846038919352 ) ) ;
#44935 = CARTESIAN_POINT ( 'NONE',  ( 46.69262628625429556, -53.66646348021690471, -75.98411709232810551 ) ) ;
#44936 = DIRECTION ( 'NONE',  ( 1.000000000000000000, 0.000000000000000000, 0.000000000000000000 ) ) ;
#44937 = AXIS2_PLACEMENT_3D ( 'NONE', #38379, #2469, #47540 ) ;
#44938 = CARTESIAN_POINT ( 'NONE',  ( 53.44281326324379933, 14.78227628659979942, -14.85152119988429931 ) ) ;
#44939 = CARTESIAN_POINT ( 'NONE',  ( 29.13393739769619728, -26.76363820448759867, -35.14999999999999858 ) ) ;
#44940 = CARTESIAN_POINT ( 'NONE',  ( -10.89446219731619969, 11.10192921922270060, -6.214546411156319117 ) ) ;
#44941 = CARTESIAN_POINT ( 'NONE',  ( 61.04001029137710077, 14.12696047140060074, -46.86320535112459851 ) ) ;
#44942 = CARTESIAN_POINT ( 'NONE',  ( 58.54030351516670549, 14.35265200861150170, -26.43833219818329638 ) ) ;
#44943 = CARTESIAN_POINT ( 'NONE',  ( 18.06150950593789872, -8.008875755996218260, -74.86649773383069828 ) ) ;
#44944 = ORIENTED_EDGE ( 'NONE', *, *, #47966, .F. ) ;
#44945 = CARTESIAN_POINT ( 'NONE',  ( 56.64869691665980156, 16.52354571958140284, -48.31614736825900280 ) ) ;
#44946 = EDGE_CURVE ( 'NONE', #1406, #9498, #20196, .T. ) ;
#44947 = CARTESIAN_POINT ( 'NONE',  ( -8.885774327477038881, -44.39634378508870327, -6.080198097671999591 ) ) ;
#44948 = CARTESIAN_POINT ( 'NONE',  ( 13.00893739769619906, 34.28605925116850273, -47.75434321273180416 ) ) ;
#44949 = CARTESIAN_POINT ( 'NONE',  ( 72.26003265285929444, 1.443555314919450216, -69.70765349352710416 ) ) ;
#44950 = DIRECTION ( 'NONE',  ( -0.2517544074889974115, -0.9677911542837451808, 0.000000000000000000 ) ) ;
#44951 = CARTESIAN_POINT ( 'NONE',  ( 72.65863549626330098, 1.000506532484680022, -69.59146369456030357 ) ) ;
#44952 = FACE_OUTER_BOUND ( 'NONE', #458, .T. ) ;
#44953 = CARTESIAN_POINT ( 'NONE',  ( 49.32346266582219840, -53.57041216484680035, -54.24688575054349826 ) ) ;
#44954 = CARTESIAN_POINT ( 'NONE',  ( 14.06314123691665507, -23.32125865919739738, -56.37568259043300856 ) ) ;
#44955 = CARTESIAN_POINT ( 'NONE',  ( 9.243065035284324438, -19.52181753121742247, -34.34351632011016164 ) ) ;
#44956 = CARTESIAN_POINT ( 'NONE',  ( 14.63393739769620083, -32.15793020853440254, -34.64999999999999858 ) ) ;
#44957 = DIRECTION ( 'NONE',  ( 0.000000000000000000, 1.000000000000000000, 0.000000000000000000 ) ) ;
#44958 = ORIENTED_EDGE ( 'NONE', *, *, #22963, .T. ) ;
#44959 = CARTESIAN_POINT ( 'NONE',  ( 13.32728455275639945, -8.714783714848721274, -46.44439537253129657 ) ) ;
#44960 = CARTESIAN_POINT ( 'NONE',  ( 64.26074781679190551, 1.176186365485389906, -61.10801278039449613 ) ) ;
#44961 = ORIENTED_EDGE ( 'NONE', *, *, #46447, .T. ) ;
#44962 = CARTESIAN_POINT ( 'NONE',  ( 83.84453607992982427, -44.32824044336482672, -46.66650892480838309 ) ) ;
#44963 = CARTESIAN_POINT ( 'NONE',  ( 61.12529890362679907, -45.61997541134829248, -47.68695910954430417 ) ) ;
#44964 = DIRECTION ( 'NONE',  ( 1.000000000000000000, 0.000000000000000000, 0.000000000000000000 ) ) ;
#44965 = CARTESIAN_POINT ( 'NONE',  ( 61.75019796695541885, 13.88381105532069881, -46.62077719375000129 ) ) ;
#44967 = CARTESIAN_POINT ( 'NONE',  ( 23.04645612045855785, -19.60032880246072651, -77.95899556036906120 ) ) ;
#44966 = CARTESIAN_POINT ( 'NONE',  ( 44.61601407454162427, 8.770664997500155380, -63.67412486887144496 ) ) ;
#44968 = B_SPLINE_CURVE_WITH_KNOTS ( 'NONE', 3,
 ( #34837, #6553, #14413, #30381 ),
 .UNSPECIFIED., .F., .F.,
 ( 4, 4 ),
 ( 0.000000000000000000, 1.000000000000000000 ),
 .UNSPECIFIED. ) ;
#44969 = DIRECTION ( 'NONE',  ( -1.000000000000000000, 0.000000000000000000, 0.000000000000000000 ) ) ;
#44970 = CARTESIAN_POINT ( 'NONE',  ( 24.04493738312996243, -16.65173602022645838, -51.54933235314647533 ) ) ;
#44971 = EDGE_LOOP ( 'NONE', ( #5361, #30205, #22826, #14610 ) ) ;
#44972 = CARTESIAN_POINT ( 'NONE',  ( 83.76205119356160367, -44.99354611814039373, -47.48604701470450351 ) ) ;
#44973 = ORIENTED_EDGE ( 'NONE', *, *, #45865, .T. ) ;
#44974 = VERTEX_POINT ( 'NONE', #38224 ) ;
#44975 = EDGE_CURVE ( 'NONE', #47941, #41326, #6476, .T. ) ;
#44976 = ORIENTED_EDGE ( 'NONE', *, *, #7688, .T. ) ;
#44977 = CARTESIAN_POINT ( 'NONE',  ( 16.13393739769620083, -15.61618894467929941, -47.64999999999999858 ) ) ;
#44978 = CARTESIAN_POINT ( 'NONE',  ( 50.03007040746459921, -48.61618894467930119, -78.14999999999999147 ) ) ;
#44979 = CARTESIAN_POINT ( 'NONE',  ( 76.39895413544020641, -19.27255048218861688, -12.79204002819740538 ) ) ;
#44980 = CARTESIAN_POINT ( 'NONE',  ( 53.97000432569529949, -51.81786419676419797, -53.85145765957989283 ) ) ;
#44981 = COLOUR_RGB ( '', 0.40784314, 0.44705882, 0.49803922) ;
#44982 = ORIENTED_EDGE ( 'NONE', *, *, #8555, .T. ) ;
#44983 = ORIENTED_EDGE ( 'NONE', *, *, #17177, .T. ) ;
#44984 = CARTESIAN_POINT ( 'NONE',  ( -30.36606260230379917, 8.133811055320650851, 16.35000000000000142 ) ) ;
#44985 = CARTESIAN_POINT ( 'NONE',  ( 56.61697313468700798, 19.46285310884560005, -53.47849945241240022 ) ) ;
#44986 = CARTESIAN_POINT ( 'NONE',  ( 12.73487495346794240, -55.47150669537813883, -75.56421462368682285 ) ) ;
#44987 = CARTESIAN_POINT ( 'NONE',  ( 14.12660287920414959, 18.38375430241896780, -83.14624708882956838 ) ) ;
#44988 = DIRECTION ( 'NONE',  ( 0.000000000000000000, -1.000000000000000000, 0.000000000000000000 ) ) ;
#44989 = B_SPLINE_CURVE_WITH_KNOTS ( 'NONE', 3,
 ( #30045, #49739, #22185, #22444, #2291, #26635, #50770, #9894, #33726, #26119 ),
 .UNSPECIFIED., .F., .F.,
 ( 4, 2, 2, 2, 4 ),
 ( 0.4999997377388590292, 0.5624999999911143300, 0.6624999999941543205, 0.8224999999990194599, 1.000000000000000000 ),
 .UNSPECIFIED. ) ;
#44990 = CARTESIAN_POINT ( 'NONE',  ( 10.22100544393300581, -12.20823257830125463, -53.61948740722137074 ) ) ;
#44991 = B_SPLINE_CURVE_WITH_KNOTS ( 'NONE', 3,
 ( #13096, #744, #8626, #16742, #5221, #28261, #40846, #8369, #24317, #24574, #28784, #44783, #20656, #8887, #25098, #29047, #24059, #40336 ),
 .UNSPECIFIED., .F., .F.,
 ( 4, 2, 2, 2, 2, 2, 2, 2, 4 ),
 ( 0.5000008230189937342, 0.5625007201416195590, 0.6250006172642452729, 0.6875005143868710977, 0.7500004115094969226, 0.8125003086321226364, 0.8750002057547484613, 0.9375001028773741751, 1.000000000000000000 ),
 .UNSPECIFIED. ) ;
#44992 = ORIENTED_EDGE ( 'NONE', *, *, #30270, .T. ) ;
#44993 = DIRECTION ( 'NONE',  ( -1.000000000000000000, 0.000000000000000000, 0.000000000000000000 ) ) ;
#44994 = CARTESIAN_POINT ( 'NONE',  ( 52.66506590845860103, -50.10307196442919775, -77.26054838597460162 ) ) ;
#44995 = CARTESIAN_POINT ( 'NONE',  ( 22.10690976917388539, -18.81397998849861253, -46.60927541014969222 ) ) ;
#44996 = CARTESIAN_POINT ( 'NONE',  ( 14.14886614762350092, -32.59522544870679894, -35.02873218748179340 ) ) ;
#44997 = CARTESIAN_POINT ( 'NONE',  ( 23.73362326446910231, -13.65876147017249842, -65.93225241418160465 ) ) ;
#44998 = LINE ( 'NONE', #8585, #32197 ) ;
#44999 = B_SPLINE_CURVE_WITH_KNOTS ( 'NONE', 3,
 ( #33048, #573, #8709, #9496, #28340, #16830, #12644, #40413, #32777, #36467, #44345, #41193, #16559, #25443, #33317, #4253, #32511, #322, #20224, #16306, #37265, #5045, #24919, #25188, #28602, #17352, #29128, #1361, #4506, #835, #20477, #45127, #40929, #48541, #5304, #17097, #44870, #37000, #49330, #13432, #12378, #45391, #36213, #44603, #29388, #32259, #24661, #1098, #48805, #40671, #49074, #48284, #4773, #20739, #36728, #12912, #10782, #1616, #17857, #38298, #30672, #9742, #46695, #41703, #37783, #1877, #34083, #2387, #22291, #41445, #29890, #42498, #45909, #29639, #22547, #17609, #25963, #18362, #37517, #34346, #33577, #33829, #18116, #46435, #46176, #6586, #50357, #50610, #14444, #42231, #38563, #21520, #14186, #30413, #2659, #10525, #49591, #26481, #13681, #18628, #50090, #34607, #5563, #14701, #45645, #30158, #9995, #41974, #2137, #25701, #21777, #5811, #10263, #49841, #13935, #6071, #22031, #26222, #38042, #6330, #35902, #31689, #7877, #11816, #30924, #27006, #19406, #17, #31178, #35384, #43519, #47208, #15482, #47711, #6853, #31946, #15995, #27778, #7112, #11297, #43771, #23062, #22804, #26738, #38825, #23823 ),
 .UNSPECIFIED., .F., .F.,
 ( 4, 2, 2, 2, 2, 2, 1, 2, 2, 2, 2, 1, 1, 1, 2, 2, 2, 2, 1, 1, 1, 2, 2, 2, 2, 1, 1, 2, 2, 2, 2, 1, 1, 2, 2, 2, 2, 2, 2, 2, 2, 2, 2, 2, 2, 2, 2, 2, 2, 2, 2, 2, 1, 2, 2, 2, 2, 2, 2, 2, 2, 2, 1, 2, 2, 2, 2, 2, 2, 2, 2, 1, 2, 2, 2, 2, 2, 2, 2, 4 ),
 ( 0.000000000000000000, 0.007812500000003518019, 0.01562500000000703604, 0.03125000000001407208, 0.04687500000002110812, 0.05468750000002399470, 0.05859375000002597228, 0.06054687500002690903, 0.06250000000002783884, 0.09375000000003770595, 0.1093750000000434236, 0.1171875000000472677, 0.1210937500000481976, 0.1230468750000496547, 0.1240234375000502515, 0.1250000000000508482, 0.1562500000000302258, 0.1718750000000191791, 0.1796875000000143774, 0.1835937500000114353, 0.1855468750000099920, 0.1865234375000099087, 0.1875000000000098255, 0.2187500000000126843, 0.2343750000000148215, 0.2421875000000159039, 0.2460937500000155431, 0.2480468750000153488, 0.2500000000000151545, 0.2812500000000131561, 0.2968750000000121014, 0.3046875000000122125, 0.3085937500000128231, 0.3105468750000131561, 0.3125000000000134892, 0.3437500000000138223, 0.3593750000000133782, 0.3750000000000129341, 0.4062500000000099365, 0.4218750000000083822, 0.4375000000000068279, 0.4687500000000035527, 0.4843750000000026645, 0.4921875000000013878, 0.5000000000000000000, 0.5312500000000000000, 0.5468749999999998890, 0.5546874999999998890, 0.5585937499999998890, 0.5624999999999997780, 0.5937499999999973355, 0.6093749999999962252, 0.6171874999999955591, 0.6210937499999953371, 0.6249999999999951150, 0.6562499999999987788, 0.6718750000000013323, 0.6796875000000027756, 0.6835937500000028866, 0.6875000000000028866, 0.7187500000000064393, 0.7343750000000078826, 0.7421875000000085487, 0.7460937500000093259, 0.7500000000000101030, 0.7812500000000117684, 0.7968750000000125455, 0.8046875000000129896, 0.8125000000000133227, 0.8437500000000145439, 0.8593750000000148770, 0.8671875000000148770, 0.8710937500000145439, 0.8750000000000142109, 0.9062500000000092149, 0.9218750000000069944, 0.9296875000000062172, 0.9335937500000058842, 0.9375000000000054401, 1.000000000000000000 ),
 .UNSPECIFIED. ) ;
#45000 = CARTESIAN_POINT ( 'NONE',  ( 42.68710801524959919, -43.36600712485200404, -4.456284347537809332 ) ) ;
#45001 = DIRECTION ( 'NONE',  ( 0.3535533905932784493, 0.6123724356957970238, 0.7071067811865430208 ) ) ;
#45002 = CARTESIAN_POINT ( 'NONE',  ( 68.13393739769841773, -50.61618894467878960, -73.25000000000220268 ) ) ;
#45003 = DIRECTION ( 'NONE',  ( 1.000000000000000000, 0.000000000000000000, 0.000000000000000000 ) ) ;
#45004 = CARTESIAN_POINT ( 'NONE',  ( 63.83374159272360515, 1.117803980320120072, -69.82829407303259472 ) ) ;
#45005 = CARTESIAN_POINT ( 'NONE',  ( 65.03565846499330405, 1.015012278467199991, -17.83341330082179965 ) ) ;
#45006 = EDGE_LOOP ( 'NONE', ( #32841, #20847, #34242, #4548, #1740 ) ) ;
#45007 = CARTESIAN_POINT ( 'NONE',  ( 14.20086869850939948, -51.63908721605620400, -75.44171726276898937 ) ) ;
#45008 = ADVANCED_FACE ( 'NONE', ( #18811 ), #10707, .T. ) ;
#45009 = CARTESIAN_POINT ( 'NONE',  ( 57.35314493057190077, 19.08815642815629587, -52.86947157453059987 ) ) ;
#45010 = CARTESIAN_POINT ( 'NONE',  ( 16.13393739769620083, -15.61618894467929941, -32.14999999999999858 ) ) ;
#45011 = DIRECTION ( 'NONE',  ( 0.000000000000000000, 1.000000000000000000, 0.000000000000000000 ) ) ;
#45012 = EDGE_CURVE ( 'NONE', #50827, #29283, #50072, .T. ) ;
#45013 = CARTESIAN_POINT ( 'NONE',  ( 56.52536539877740296, -50.75180572374080157, -53.84278118897309895 ) ) ;
#45014 = CIRCLE ( 'NONE', #44185, 13.50000000000000178 ) ;
#45015 = CARTESIAN_POINT ( 'NONE',  ( 23.20978547387309732, -14.32984258838409986, -32.14999999999999858 ) ) ;
#45016 = SPHERICAL_SURFACE ( 'NONE', #10541, 2.000000000000000000 ) ;
#45017 = EDGE_CURVE ( 'NONE', #20864, #37366, #34009, .T. ) ;
#45018 = CARTESIAN_POINT ( 'NONE',  ( 47.66581657685510010, -54.52382939817299956, -55.09436269531810382 ) ) ;
#45020 = CARTESIAN_POINT ( 'NONE',  ( 11.28911561387254636, 33.06253056614959718, -24.06342471125372739 ) ) ;
#45019 = DIRECTION ( 'NONE',  ( 0.9441882088883221114, 0.3294064756440927000, 0.000000000000000000 ) ) ;
#45021 = TOROIDAL_SURFACE ( 'NONE', #42532, 34.47562460986249988, 0.5000000000000000000 ) ;
#45022 = CARTESIAN_POINT ( 'NONE',  ( 18.68117707985434706, -55.53437412588283451, -76.07908087643973261 ) ) ;
#45023 = CARTESIAN_POINT ( 'NONE',  ( 48.85376873155860267, 22.78610090897890217, -55.25797120370700100 ) ) ;
#45024 = ORIENTED_EDGE ( 'NONE', *, *, #7623, .T. ) ;
#45025 = CARTESIAN_POINT ( 'NONE',  ( 9.127021151536109045, -16.41973352573810274, -63.81083516600379113 ) ) ;
#45026 = ORIENTED_EDGE ( 'NONE', *, *, #3499, .F. ) ;
#45027 = CARTESIAN_POINT ( 'NONE',  ( 13.00893739761190027, -65.51843714052189682, -47.75434321210310173 ) ) ;
#45028 = CARTESIAN_POINT ( 'NONE',  ( 19.16157989668716866, -49.56476373416713699, -34.89146800830127404 ) ) ;
#45029 = DIRECTION ( 'NONE',  ( -1.000000000000000000, 0.000000000000000000, 0.000000000000000000 ) ) ;
#45031 = CARTESIAN_POINT ( 'NONE',  ( 54.51447658024279974, 16.52301143147950313, -26.25507474854270029 ) ) ;
#45030 = CARTESIAN_POINT ( 'NONE',  ( 84.42287661217579853, 12.05518195546730098, -47.36827274406740429 ) ) ;
#45032 = CARTESIAN_POINT ( 'NONE',  ( 14.90922390191370006, -8.670497074903209977, -65.89726463310188365 ) ) ;
#45033 = CARTESIAN_POINT ( 'NONE',  ( 11.41271396217753065, 33.75416681246611716, -16.69425700585250993 ) ) ;
#45034 = CARTESIAN_POINT ( 'NONE',  ( 72.80030139158668590, 1.384887413063060180, -68.61455525072810246 ) ) ;
#45035 = DIRECTION ( 'NONE',  ( 1.000000000000000000, 2.460964292799963328E-14, 0.000000000000000000 ) ) ;
#45036 = ORIENTED_EDGE ( 'NONE', *, *, #22929, .F. ) ;
#45037 = ADVANCED_FACE ( 'NONE', ( #14630 ), #46102, .T. ) ;
#45038 = VERTEX_POINT ( 'NONE', #45832 ) ;
#45039 = CARTESIAN_POINT ( 'NONE',  ( 12.14166061495349958, -65.10571081234380131, -16.52221827438259893 ) ) ;
#45040 = CARTESIAN_POINT ( 'NONE',  ( 13.00893739769619906, 34.28605925116850273, -47.75434321273180416 ) ) ;
#45041 = CARTESIAN_POINT ( 'NONE',  ( 61.08967272334363230, -45.33611584009540962, -46.92974945990184210 ) ) ;
#45042 = CARTESIAN_POINT ( 'NONE',  ( 50.54558668919739972, -52.16494804883890168, -52.27649567391959806 ) ) ;
#45043 = CARTESIAN_POINT ( 'NONE',  ( 51.63120318262737385, 2.821641822706145497, -76.94893558361998487 ) ) ;
#45044 = ORIENTED_EDGE ( 'NONE', *, *, #33851, .T. ) ;
#45045 = CARTESIAN_POINT ( 'NONE',  ( 12.35956436673935954, 18.99725813312436884, -21.15000000013027659 ) ) ;
#45046 = CARTESIAN_POINT ( 'NONE',  ( 57.26919357480770145, 14.59258250881100061, -26.26282533821949983 ) ) ;
#45047 = CARTESIAN_POINT ( 'NONE',  ( 64.93393739769619799, 1.883811055320669947, -70.34999999999999432 ) ) ;
#45048 = CARTESIAN_POINT ( 'NONE',  ( 72.65628610108569774, 1.412203896155640015, -69.03044017489760620 ) ) ;
#45049 = DIRECTION ( 'NONE',  ( 0.5897727341282554825, -0.3900873262218120252, 0.7071067811865473507 ) ) ;
#45050 = CARTESIAN_POINT ( 'NONE',  ( -21.36606260230379917, -53.11618894467930119, 11.84999999999999964 ) ) ;
#45051 = ORIENTED_EDGE ( 'NONE', *, *, #43651, .F. ) ;
#45052 = CARTESIAN_POINT ( 'NONE',  ( 9.543104041351597289, -13.84479649607203733, -67.53615334925251545 ) ) ;
#45053 = CARTESIAN_POINT ( 'NONE',  ( 17.98749448546710994, -32.47778390180250341, -34.79644291222910368 ) ) ;
#45054 = ORIENTED_EDGE ( 'NONE', *, *, #26191, .F. ) ;
#45055 = CARTESIAN_POINT ( 'NONE',  ( 12.57402232428822764, -55.45745225559931413, -75.39120620928086680 ) ) ;
#45056 = AXIS2_PLACEMENT_3D ( 'NONE', #22542, #3166, #50859 ) ;
#45057 = FACE_OUTER_BOUND ( 'NONE', #10221, .T. ) ;
#45058 = EDGE_CURVE ( 'NONE', #20846, #25261, #24929, .T. ) ;
#45059 = CARTESIAN_POINT ( 'NONE',  ( 24.36162650863650114, -16.15271744766720019, -79.81305924085479830 ) ) ;
#45060 = CARTESIAN_POINT ( 'NONE',  ( 11.87323508190820931, -21.23659595403887934, -65.55365164941011358 ) ) ;
#45061 = CARTESIAN_POINT ( 'NONE',  ( 9.205734167420709824, -3.616188944679339823, -32.14999999999999858 ) ) ;
#45062 = CARTESIAN_POINT ( 'NONE',  ( 47.21823810954259670, -54.28882551123370348, -75.35585495399020317 ) ) ;
#45063 = EDGE_LOOP ( 'NONE', ( #48594, #46534, #31038, #9173 ) ) ;
#45064 = CARTESIAN_POINT ( 'NONE',  ( 55.72808153907849515, 14.53141219772050086, -16.72868168772430053 ) ) ;
#45065 = CARTESIAN_POINT ( 'NONE',  ( 57.28991729228579288, -50.57887465766769708, -53.44461810997250240 ) ) ;
#45066 = CARTESIAN_POINT ( 'NONE',  ( 19.38808262899609858, -9.358945304426239176, -34.49983067246459001 ) ) ;
#45067 = CARTESIAN_POINT ( 'NONE',  ( 16.13393739769620083, 30.88381105532059934, 11.84999999999999964 ) ) ;
#45068 = ORIENTED_EDGE ( 'NONE', *, *, #1174, .F. ) ;
#45069 = CARTESIAN_POINT ( 'NONE',  ( 46.57616577472359864, 22.03317133735550115, -76.11243514202939764 ) ) ;
#45070 = CARTESIAN_POINT ( 'NONE',  ( 47.13393739769619373, -38.26167638829240047, -54.64999999999999858 ) ) ;
#45071 = CARTESIAN_POINT ( 'NONE',  ( -11.36606260230380094, -15.61618894467929941, -54.64999999999999858 ) ) ;
#45072 = CARTESIAN_POINT ( 'NONE',  ( 12.24959214049200007, 33.48392698190040306, -15.94651421638729971 ) ) ;
#45073 = CARTESIAN_POINT ( 'NONE',  ( 18.77108585709959954, -23.07469878264739904, -81.89948870795299740 ) ) ;
#45074 = ADVANCED_FACE ( 'NONE', ( #7037 ), #23494, .F. ) ;
#45075 = DIRECTION ( 'NONE',  ( 8.402539340422011355E-12, -1.000000000000000000, -1.365304166073849981E-11 ) ) ;
#45076 = CARTESIAN_POINT ( 'NONE',  ( 72.92981560451809742, 1.375383258925270136, -68.56484433753419694 ) ) ;
#45078 = CARTESIAN_POINT ( 'NONE',  ( 30.26695094089093629, -35.61719269261135423, -84.60820949069447749 ) ) ;
#45077 = CARTESIAN_POINT ( 'NONE',  ( 56.63393739769620083, 19.38381105532069881, 16.85000000000000142 ) ) ;
#45079 = CARTESIAN_POINT ( 'NONE',  ( 24.04493739769619864, -15.61618894467929941, -32.14999999999999858 ) ) ;
#45080 = B_SPLINE_CURVE_WITH_KNOTS ( 'NONE', 3,
 ( #37019, #24936, #10018, #21275, #25980, #33065, #5580, #1898, #48822, #22048 ),
 .UNSPECIFIED., .F., .F.,
 ( 4, 1, 1, 1, 1, 1, 1, 4 ),
 ( 0.000000000000000000, 0.04040786132540063330, 0.1196267923890341062, 0.1988457234526539996, 0.2780646545162693273, 0.3572835855798892069, 0.4365025166435069215, 0.4999960598860723193 ),
 .UNSPECIFIED. ) ;
#45081 = CARTESIAN_POINT ( 'NONE',  ( 12.77400604982020127, -63.78156501761489494, -45.78449089158930008 ) ) ;
#45082 = ORIENTED_EDGE ( 'NONE', *, *, #5385, .T. ) ;
#45083 = CARTESIAN_POINT ( 'NONE',  ( 53.18775749951439735, -49.47422114125170367, -48.84930875881670431 ) ) ;
#45084 = CIRCLE ( 'NONE', #51777, 3.500000000000003109 ) ;
#45085 = CARTESIAN_POINT ( 'NONE',  ( 17.71568183981793609, 20.46959823935371503, -75.56421430877649925 ) ) ;
#45086 = CARTESIAN_POINT ( 'NONE',  ( 9.807863465693298366, -20.47798411401742058, -74.58399817736376747 ) ) ;
#45087 = CARTESIAN_POINT ( 'NONE',  ( 13.55381709587100048, 19.79410389518359992, -21.89021442387040040 ) ) ;
#45088 = CARTESIAN_POINT ( 'NONE',  ( 57.45067094067109537, 14.37644489360019939, -26.20528765251999559 ) ) ;
#45089 = VECTOR ( 'NONE', #5372, 1000.000000000000000 ) ;
#45090 = CARTESIAN_POINT ( 'NONE',  ( 12.97538624507340010, -21.92223780171290315, -33.10062717276339583 ) ) ;
#45091 = CARTESIAN_POINT ( 'NONE',  ( 50.65831132946720317, 18.03884146108959996, -76.22116164240389935 ) ) ;
#45092 = CARTESIAN_POINT ( 'NONE',  ( 53.25072070970590232, 18.25720078509660027, -49.09191088899479638 ) ) ;
#45093 = CARTESIAN_POINT ( 'NONE',  ( 71.10413293483961183, 1.338092079250050137, -70.53694914618849054 ) ) ;
#45094 = CARTESIAN_POINT ( 'NONE',  ( 40.50275677532349761, -44.77423425411610225, -4.148922563335220026 ) ) ;
#45095 = CARTESIAN_POINT ( 'NONE',  ( 47.11719193592726640, 22.63726203549512661, -75.76637087366511025 ) ) ;
#45096 = ORIENTED_EDGE ( 'NONE', *, *, #18899, .T. ) ;
#45097 = CARTESIAN_POINT ( 'NONE',  ( 16.35471799615400101, -23.06319825774929910, -79.55790855712409382 ) ) ;
#45098 = ORIENTED_EDGE ( 'NONE', *, *, #46075, .T. ) ;
#45099 = CARTESIAN_POINT ( 'NONE',  ( 72.80287646850260330, 1.383922910988889976, -68.71460001914260829 ) ) ;
#45100 = CARTESIAN_POINT ( 'NONE',  ( 47.41980604789990394, -54.64426992894529889, -54.80792317606589847 ) ) ;
#45101 = CARTESIAN_POINT ( 'NONE',  ( 20.89221387562904297, -9.278317313805978017, -49.49732490764383641 ) ) ;
#45102 = CARTESIAN_POINT ( 'NONE',  ( 9.366937397696199596, -15.61618894467949836, -28.45282021618999835 ) ) ;
#45103 =( BOUNDED_CURVE ( )  B_SPLINE_CURVE ( 3, ( #44632, #44379, #3782, #4533 ),
 .UNSPECIFIED., .F., .F. ) 
 B_SPLINE_CURVE_WITH_KNOTS ( ( 4, 4 ),
 ( 2.696998093256683937, 3.586187213922897410 ),
 .UNSPECIFIED. ) 
 CURVE ( )  GEOMETRIC_REPRESENTATION_ITEM ( )  RATIONAL_B_SPLINE_CURVE ( ( 1.000000000000000000, 0.9351900772698563680, 0.9351900772698563680, 1.000000000000000000 ) ) 
 REPRESENTATION_ITEM ( '' )  );
#45104 = CARTESIAN_POINT ( 'NONE',  ( 58.51098925350719782, 17.50221282658370114, -51.08149774042820468 ) ) ;
#45105 = CARTESIAN_POINT ( 'NONE',  ( 53.13663690894949809, 18.26775922387509965, -48.80285956119419666 ) ) ;
#45106 = FACE_OUTER_BOUND ( 'NONE', #2958, .T. ) ;
#45107 = CARTESIAN_POINT ( 'NONE',  ( 72.00360496390891285, 1.017423949637090042, -61.06375415878460444 ) ) ;
#45108 = CARTESIAN_POINT ( 'NONE',  ( 23.04644961876633502, -19.60034157972581070, -71.67430252639809396 ) ) ;
#45109 = ORIENTED_EDGE ( 'NONE', *, *, #43073, .F. ) ;
#45110 = CARTESIAN_POINT ( 'NONE',  ( 65.02205492013339949, 0.9960089569207349891, -70.77007079217121088 ) ) ;
#45111 = ORIENTED_EDGE ( 'NONE', *, *, #27493, .F. ) ;
#45112 = ORIENTED_EDGE ( 'NONE', *, *, #26420, .T. ) ;
#45113 = CARTESIAN_POINT ( 'NONE',  ( 8.966097822182190313, -63.20784705743349718, -46.63270530499050182 ) ) ;
#45114 = LINE ( 'NONE', #28590, #36932 ) ;
#45115 = ORIENTED_EDGE ( 'NONE', *, *, #16303, .F. ) ;
#45116 = CARTESIAN_POINT ( 'NONE',  ( 16.13393739769620083, -15.61618894467929941, -2.149999999999999911 ) ) ;
#45117 = FACE_OUTER_BOUND ( 'NONE', #39549, .T. ) ;
#45118 = LINE ( 'NONE', #29120, #47930 ) ;
#45119 = CARTESIAN_POINT ( 'NONE',  ( 51.19067547918189831, 19.52102757408819755, -76.16618596938450025 ) ) ;
#45120 = EDGE_LOOP ( 'NONE', ( #20140, #48992, #16531, #38257 ) ) ;
#45121 = CARTESIAN_POINT ( 'NONE',  ( 41.99526469904490966, 6.390604947338678343, -80.34329386236483117 ) ) ;
#45122 = CARTESIAN_POINT ( 'NONE',  ( 23.98146874757331659, -14.58313711796746404, -43.75066625850210045 ) ) ;
#45123 = EDGE_CURVE ( 'NONE', #8693, #24585, #2369, .T. ) ;
#45124 = CARTESIAN_POINT ( 'NONE',  ( 20.11402673884080272, -8.395274259375058890, -51.45268192007909391 ) ) ;
#45125 = EDGE_CURVE ( 'NONE', #44451, #30791, #31632, .T. ) ;
#45126 = FACE_OUTER_BOUND ( 'NONE', #12968, .T. ) ;
#45127 = CARTESIAN_POINT ( 'NONE',  ( 42.56729540932941092, -37.71296202124863584, -77.48315337116866885 ) ) ;
#45128 = ADVANCED_FACE ( 'NONE', ( #47896 ), #38366, .F. ) ;
#45129 = ORIENTED_EDGE ( 'NONE', *, *, #47758, .T. ) ;
#45130 = CARTESIAN_POINT ( 'NONE',  ( 12.19807860417640022, -9.290391812094439317, -45.55549324029149716 ) ) ;
#45131 = CARTESIAN_POINT ( 'NONE',  ( 52.59026075507060227, -49.83798095265300532, -48.57069100191419864 ) ) ;
#45132 = CIRCLE ( 'NONE', #49335, 7.000000000000000000 ) ;
#45133 = CARTESIAN_POINT ( 'NONE',  ( 11.88110451476120133, -10.30869569151619913, -32.14999999999999858 ) ) ;
#45134 = AXIS2_PLACEMENT_3D ( 'NONE', #45116, #29377, #45378 ) ;
#45135 = CIRCLE ( 'NONE', #31706, 1.000000000000000444 ) ;
#45136 = CARTESIAN_POINT ( 'NONE',  ( 14.45708746590530147, 21.37421319461290281, -76.02269426304029309 ) ) ;
#45137 = LINE ( 'NONE', #9248, #17195 ) ;
#45138 = CARTESIAN_POINT ( 'NONE',  ( 83.25003658253979211, -44.84236030505880422, -46.59700837026780107 ) ) ;
#45139 = CARTESIAN_POINT ( 'NONE',  ( 18.56287218994199861, -7.736912551253769088, -49.10285124761459485 ) ) ;
#45140 = EDGE_CURVE ( 'NONE', #13573, #10379, #27445, .T. ) ;
#45141 = ORIENTED_EDGE ( 'NONE', *, *, #28482, .F. ) ;
#45142 = CARTESIAN_POINT ( 'NONE',  ( 55.24793159653169994, -47.06280844521510431, -26.19812636028400021 ) ) ;
#45143 = FACE_OUTER_BOUND ( 'NONE', #13946, .T. ) ;
#45144 = CYLINDRICAL_SURFACE ( 'NONE', #3125, 1.999999999999997113 ) ;
#45145 = CARTESIAN_POINT ( 'NONE',  ( 16.13393739769620083, -15.61618894467929941, 4.450000000000000178 ) ) ;
#45146 = CARTESIAN_POINT ( 'NONE',  ( 51.02727426391909660, 14.97163178983270093, -13.20164647346950026 ) ) ;
#45147 = ORIENTED_EDGE ( 'NONE', *, *, #40931, .F. ) ;
#45148 = CARTESIAN_POINT ( 'NONE',  ( -7.441429056736700076, -45.44001222700619991, -5.170794712822120331 ) ) ;
#45149 = CARTESIAN_POINT ( 'NONE',  ( 47.30810002566669681, 23.48187059465450233, -54.68911926312569705 ) ) ;
#45150 = FACE_OUTER_BOUND ( 'NONE', #7421, .T. ) ;
#45151 = CARTESIAN_POINT ( 'NONE',  ( 63.17939165373819321, 0.9307121176571839793, -62.26576483763439995 ) ) ;
#45152 = CARTESIAN_POINT ( 'NONE',  ( 10.10517893431049963, -55.15925497894330931, -21.14999999999999858 ) ) ;
#45153 = CARTESIAN_POINT ( 'NONE',  ( 11.22168587317799826, 33.99689325987720423, -17.68872783567740115 ) ) ;
#45154 = CYLINDRICAL_SURFACE ( 'NONE', #15872, 21.50000000000000000 ) ;
#45155 = CARTESIAN_POINT ( 'NONE',  ( 16.13393739769620083, -15.61618894467929941, -35.14999999999999858 ) ) ;
#45156 = CARTESIAN_POINT ( 'NONE',  ( 58.76827139312189985, -46.69333694941190060, -47.97482660407749933 ) ) ;
#45157 = CARTESIAN_POINT ( 'NONE',  ( 52.41358714188920231, 21.24840881348460186, -54.13676513255019529 ) ) ;
#45158 = VECTOR ( 'NONE', #30801, 1000.000000000000114 ) ;
#45159 = CARTESIAN_POINT ( 'NONE',  ( 9.366403394718119557, -15.61612932825470068, -61.45282021618999124 ) ) ;
#45160 = DIRECTION ( 'NONE',  ( 1.000000000000000000, 2.460964292799963328E-14, 0.000000000000000000 ) ) ;
#45161 = ORIENTED_EDGE ( 'NONE', *, *, #16012, .F. ) ;
#45162 = CARTESIAN_POINT ( 'NONE',  ( 22.90121638405171467, -15.61618906730874734, -72.84718036870921765 ) ) ;
#45163 = CARTESIAN_POINT ( 'NONE',  ( 8.963664087775370604, 31.96126547328639944, -46.63283018613729780 ) ) ;
#45164 = CARTESIAN_POINT ( 'NONE',  ( 28.37540540599747274, -22.68380379454831441, -34.70142521051217699 ) ) ;
#45165 = VECTOR ( 'NONE', #43782, 999.9999999999998863 ) ;
#45166 = CIRCLE ( 'NONE', #34251, 6.999999999999999112 ) ;
#45167 = AXIS2_PLACEMENT_3D ( 'NONE', #14533, #35218, #19236 ) ;
#45168 = CARTESIAN_POINT ( 'NONE',  ( 68.36214372925699934, -30.78933952734989887, -18.19623527655679851 ) ) ;
#45169 = ORIENTED_EDGE ( 'NONE', *, *, #38896, .F. ) ;
#45170 = CARTESIAN_POINT ( 'NONE',  ( 18.86790871750899967, 20.55443427335040241, -74.33583724502659607 ) ) ;
#45171 = ORIENTED_EDGE ( 'NONE', *, *, #3600, .F. ) ;
#45172 = ORIENTED_EDGE ( 'NONE', *, *, #26592, .F. ) ;
#45173 = DIRECTION ( 'NONE',  ( 0.000000000000000000, 0.000000000000000000, -1.000000000000000000 ) ) ;
#45174 = AXIS2_PLACEMENT_3D ( 'NONE', #43311, #7403, #31989 ) ;
#45175 = ORIENTED_EDGE ( 'NONE', *, *, #51108, .T. ) ;
#45176 = CARTESIAN_POINT ( 'NONE',  ( 10.92970840452719905, -64.58899151715630182, -46.27302159251959779 ) ) ;
#45177 = CARTESIAN_POINT ( 'NONE',  ( 56.37838042625359947, -46.11745970339239875, -26.19141323752749884 ) ) ;
#45178 = CARTESIAN_POINT ( 'NONE',  ( 22.45577387985110107, -19.01145220004960024, -81.23899999999999011 ) ) ;
#45179 = CARTESIAN_POINT ( 'NONE',  ( 23.04647095553203684, -11.63207687756748676, -63.34100319679465940 ) ) ;
#45180 = CARTESIAN_POINT ( 'NONE',  ( 61.37276932190779632, 14.04312170586010033, -47.09682269328109783 ) ) ;
#45181 = DIRECTION ( 'NONE',  ( 0.000000000000000000, 1.000000000000000000, 0.000000000000000000 ) ) ;
#45182 = VERTEX_POINT ( 'NONE', #7805 ) ;
#45183 = ORIENTED_EDGE ( 'NONE', *, *, #26025, .F. ) ;
#45184 = EDGE_LOOP ( 'NONE', ( #23785, #6761, #34549, #37519 ) ) ;
#45185 = CARTESIAN_POINT ( 'NONE',  ( 50.30625828053950244, -45.11618894460909956, -10.79703776619339983 ) ) ;
#45186 = B_SPLINE_CURVE_WITH_KNOTS ( 'NONE', 3,
 ( #51256, #15350, #27388, #43390, #7485, #23436, #15608, #44934, #21321, #49141, #9034, #9305, #13237, #8248, #40738, #20283 ),
 .UNSPECIFIED., .F., .F.,
 ( 4, 2, 2, 2, 2, 2, 2, 4 ),
 ( 6.613222000000000237E-15, 0.07216186899281500089, 0.1546325764131659952, 0.2061767685508859860, 0.2319488646197460091, 0.2731842183299219573, 0.3391607842662039962, 0.4123535371017659767 ),
 .UNSPECIFIED. ) ;
#45187 = EDGE_CURVE ( 'NONE', #44049, #11677, #50745, .T. ) ;
#45188 = DIRECTION ( 'NONE',  ( 1.000000000000000000, 0.000000000000000000, 0.000000000000000000 ) ) ;
#45189 = DIRECTION ( 'NONE',  ( 0.000000000000000000, 0.000000000000000000, -1.000000000000000000 ) ) ;
#45190 = ADVANCED_FACE ( 'NONE', ( #4119 ), #47137, .T. ) ;
#45191 = ORIENTED_EDGE ( 'NONE', *, *, #14713, .F. ) ;
#45192 = B_SPLINE_CURVE_WITH_KNOTS ( 'NONE', 3,
 ( #7797, #32379, #20338, #35572, #39250, #15401, #36325, #51558, #436 ),
 .UNSPECIFIED., .F., .F.,
 ( 4, 1, 1, 1, 1, 1, 4 ),
 ( 0.000000000000000000, 0.07759967679297839760, 0.1709532882598540637, 0.2643068997267294384, 0.3576605111936237424, 0.4510141226604987841, 0.4999989276629364099 ),
 .UNSPECIFIED. ) ;
#45193 = CARTESIAN_POINT ( 'NONE',  ( 11.13393739769619906, 24.07008072128950005, -43.74348518090240390 ) ) ;
#45194 = CARTESIAN_POINT ( 'NONE',  ( 47.14844574785740150, -54.72867718618289956, -74.72768729699521373 ) ) ;
#45195 = CARTESIAN_POINT ( 'NONE',  ( 60.34379256561150129, 14.63564648314799932, -47.72732608210870353 ) ) ;
#45196 = CARTESIAN_POINT ( 'NONE',  ( 51.90140114478749922, 14.76431734774619819, -13.70501522390690141 ) ) ;
#45197 = DIRECTION ( 'NONE',  ( 0.000000000000000000, -0.7071067811865466846, -0.7071067811865483499 ) ) ;
#45198 = FACE_OUTER_BOUND ( 'NONE', #34790, .T. ) ;
#45199 = AXIS2_PLACEMENT_3D ( 'NONE', #40282, #33174, #4372 ) ;
#45200 = VECTOR ( 'NONE', #7557, 1000.000000000000000 ) ;
#45201 = AXIS2_PLACEMENT_3D ( 'NONE', #27306, #51175, #7152 ) ;
#45202 = CARTESIAN_POINT ( 'NONE',  ( 14.67229395948385218, -22.51591050674139893, -55.41362847326020358 ) ) ;
#45203 = CARTESIAN_POINT ( 'NONE',  ( 60.84489046480559438, 13.88818919943340013, -26.73359653442770067 ) ) ;
#45204 = AXIS2_PLACEMENT_3D ( 'NONE', #14031, #10364, #14289 ) ;
#45205 = CARTESIAN_POINT ( 'NONE',  ( 8.551749739990640364, -13.59204010960809939, -68.37054538661399761 ) ) ;
#45206 = EDGE_CURVE ( 'NONE', #24197, #16397, #46766, .T. ) ;
#45207 = B_SPLINE_SURFACE_WITH_KNOTS ( 'NONE', 3, 3, ( 
 ( #27067, #38357, #23123, #19464, #3231, #18948, #19204, #11614, #22610, #27322, #38626, #18690, #34927, #7422, #23370, #43072, #39392, #31494, #35449, #46497, #34665, #50926, #50670, #10587, #3495, #51447, #18431, #43582, #27579, #15542, #14766, #15023, #7683, #46760, #30734, #2450, #50420, #10845, #30991, #26806, #42818, #6914, #47016, #11104, #8450, #32775, #27835, #32257, #4002, #3752, #8190, #12909, #28599, #16049, #19721, #47772, #40668, #32005, #24658, #36463, #28866, #39646, #7934, #32509, #23629, #23882, #28338, #20222, #44088, #4504, #24396, #31751, #48026, #39907, #36211, #48281, #35712, #77, #20474, #44868, #832, #36726, #12376, #4251, #11878, #44601, #51696, #15790, #12126, #44342, #35960, #28083, #16302, #43833, #8707, #20738, #4770, #24133, #16828, #571, #40156, #319, #48802, #40411, #16557, #48538, #12642, #17607, #9739, #41972, #40927, #33574, #17855, #25960, #13932, #21001, #29888, #36998, #45906, #37515, #45389, #9494, #18113, #25440, #41701, #29126, #5042, #45124, #9993, #5302, #49589, #22028, #6069, #1096, #30156, #1359, #37781, #38038, #49838, #49328, #5809, #2135, #34081, #50088, #5559, #1614, #9236, #17093, #14183, #13429, #8972, #25186, #21774, #24916, #29385, #33046, #41443, #49071, #13178, #41191, #21518, #1874, #21252, #33826, #37262, #17350, #13679, #33315, #29636, #45642, #25698, #19141, #3171, #46954, #50355, #14957, #7109, #43012, #10522, #26220, #47206, #39080, #2913, #14442, #30411, #39327, #23060, #51382, #11293, #46174, #18882, #14699, #34605, #6851, #15479, #26478, #42228, #30922, #34864, #10261, #11036, #27255, #27004, #30669, #35119, #3431, #46433, #51127, #42496, #6584, #46693, #15223, #31176, #50866, #43269, #19403, #7358, #22289, #22545, #22801, #38561, #18360, #23305, #2656, #6328, #35382, #38296, #18626, #2385, #34343, #50607, #10780, #26736, #42756, #38823, #27775, #8383, #31944, #16496, #40094, #43769, #23820, #31687, #4444, #36154, #7875, #32447, #44277, #4187, #12316, #506, #20411, #39583, #47967, #256, #24334, #44027, #39839, #44538, #16242, #24075, #20165, #19657, #48474, #36400, #3947, #15, #19906, #12575, #28539, #40602, #8639, #3688, #32196, #51636, #36659, #47709, #35900, #48217, #28277, #24590, #4702, #20671, #28022, #40350, #15731, #35650, #762, #15993, #31430, #11814, #47460, #11554, #27514, #43516, #7622, #23566, #12070, #8130, #17786, #25116, #13112, #25889, #37970, #4967, #33246, #45059, #28800, #49771, #33507, #37450, #1549, #41902, #20934, #25377, #49006, #48737 ),
 ( #29572, #6002, #32712, #1035, #25630, #16758, #17028, #21450, #13358, #37196, #49520, #17537, #24855, #41127, #32980, #29316, #41378, #44800, #9160, #13612, #21961, #45837, #29820, #5493, #49263, #40862, #21700, #12842, #8904, #5238, #45578, #29063, #21189, #9427, #36933, #1807, #13864, #33760, #1294, #9927, #9672, #17286, #45323, #37708, #41634, #5743, #23245, #19077, #10712, #2852, #35051, #34014, #26667, #10972, #51058, #7041, #14116, #22993, #30083, #39014, #30604, #38487, #2587, #11229, #18563, #34797, #22221, #50024, #38229, #3109, #50291, #42687, #15155, #31116, #46108, #2070, #46367, #30857, #47141, #42943, #42428, #50803, #18047, #42163, #34539, #30344, #10194, #27192, #18816, #22737, #38757, #43203, #6262, #6783, #34267, #26152, #50543, #7294, #2323, #10455, #18297, #14379, #26407, #6518, #22480, #14890, #14635, #46623, #46885, #26939, #39263, #23498, #43959, #35837, #7809, #20100, #24011, #47397, #47644, #3622, #51826, #12001, #51319, #15670, #36089, #28476, #16436, #445, #27956, #19846, #11493, #44215, #3364, #19338, #11750, #8064, #19594, #35585, #31882, #27449, #24269, #36335, #40290, #27707, #4381, #16174, #31625, #15926, #8315, #40031, #51570, #8584, #20349, #47901, #4125, #32388, #35320, #197, #48151, #48409, #12510, #15416, #44476, #31368, #43452, #32132, #23760, #39775, #7555, #3879, #12253, #39523, #43706, #28214, #45517, #20872, #13294, #37643, #41573, #701, #45776, #16969, #1491, #1743, #13550, #13046, #5429, #29512, #5686, #9614, #21131, #17222, #44735, #32649, #17726, #28998, #33696, #40798, #29254, #25567, #4633, #29757, #49711, #21635, #4901, #9097, #13801, #32915, #36870, #24526, #40543, #969, #17475, #25048, #20605, #33181, #48944, #44997, #24791, #49458, #45260, #41064, #36599, #37389, #49202, #21385, #16694, #48675, #12778, #5176, #9365, #33442, #37133, #1231, #28734, #25314, #41316, #8839, #49966, #27585, #35459, #38164, #30282, #18236, #15549, #31506, #19726, #23637, #17981, #51199, #30016, #15795, #10130, #6199, #2521, #7428, #43336, #31760, #50224, #11622, #14313, #14056, #43589, #37908, #46301, #23377, #5939, #39401, #2001, #46041, #10388, #26088, #42096, #3503, #47525, #51454, #19472, #11367, #22154, #31247, #7693, #39653, #2262, #41833, #3759, #35718, #18501, #34202, #26344, #51704, #9866, #25821, #21897, #33948, #34473, #42357, #6458, #22417, #38420, #15293, #47277, #27330, #36471, #47778, #32515, #28872, #16563, #32264, #48546, #5048, #32010, #4777, #16055, #48036, #48288, #12647, #28607 ),
 ( #32781, #8196, #1101, #24924, #11884, #28090, #43842, #27842, #7941, #44873, #28343, #44606, #36217, #48809, #326, #35966, #8977, #23888, #12383, #8714, #39912, #24664, #4008, #83, #44349, #12135, #44096, #40675, #839, #20744, #36731, #16833, #24139, #12916, #40933, #21007, #40164, #19969, #37004, #17100, #4510, #4257, #20229, #16311, #8456, #24403, #40417, #20480, #577, #1620, #21523, #45649, #38302, #13436, #13184, #1882, #21780, #33052, #17861, #14191, #33832, #17612, #49845, #42236, #17356, #41977, #1364, #33320, #33581, #13938, #29893, #37786, #45912, #26226, #30163, #9242, #37268, #9747, #29392, #5307, #18120, #45395, #2390, #10266, #49078, #9500, #29132, #45130, #25191, #46181, #13684, #9999, #6334, #25447, #25967, #49596, #34086, #41708, #41448, #5567, #49333, #6076, #22035, #37521, #50093, #38046, #5816, #2140, #22294, #41197, #21259, #29643, #25704, #47213, #30929, #30676, #31438, #3178, #11042, #27011, #6590, #35390, #43276, #46700, #38829, #26745, #23311, #39337, #27520, #47466, #26484, #7115, #38566, #23572, #18632, #14705, #43019, #15231, #51134, #39590, #2920, #42762, #3439, #19411, #43525, #11561, #42501, #23066, #2662, #18367, #34610, #10786, #39086, #31182, #11302, #34349, #6857, #51389, #22809, #22552, #15487, #46438, #18889, #27262, #14448, #7366, #10528, #50613, #34871, #50874, #14963, #7628, #50360, #30416, #46961, #19150, #35127, #24340, #16501, #514, #19913, #35656, #4709, #48480, #12322, #23827, #39845, #48745, #32453, #8911, #20678, #3695, #28283, #24080, #44032, #16247, #24861, #35904, #51643, #40355, #44282, #19664, #4451, #36666, #20417, #40100, #36408, #12849, #3951, #12582, #22, #15997, #4193, #28546, #44544, #8391, #8646, #28806, #769, #31692, #7880, #32202, #31948, #27781, #40610, #47972, #15738, #32718, #47715, #12074, #11819, #43775, #28028, #16765, #36158, #24597, #44807, #8134, #20170, #262, #48222, #51668, #3464, #35415, #43300, #16021, #47740, #19435, #44054, #3972, #15762, #23849, #12096, #31976, #51161, #7654, #11848, #19937, #3718, #51416, #4217, #27805, #35683, #31715, #31207, #8159, #47996, #15511, #31465, #11585, #47489, #28051, #24103, #288, #20191, #15254, #43802, #11327, #48249, #7391, #39362, #7902, #39872, #35927, #12343, #27546, #40124, #43552, #47236, #36181, #19174, #23597, #44, #39109, #16273, #35153, #27291, #39615, #23339, #19690, #32226, #43042, #7138, #23090, #3202, #32474, #49034, #41154, #25149, #44568, #8417, #29350, #37230, #36965, #48504, #12606, #21483 ),
 ( #8669, #24365, #13142, #17058, #28308, #29091, #9458, #45090, #12873, #9197, #37482, #28569, #1327, #24624, #40635, #28829, #5267, #17315, #33011, #33279, #1582, #25407, #4474, #4734, #40893, #20701, #539, #13392, #36691, #33540, #5528, #44308, #792, #40377, #20443, #36431, #41410, #8939, #49294, #17571, #16793, #45356, #44834, #49558, #1062, #32742, #48769, #24882, #16525, #5004, #20964, #14667, #26446, #38262, #46402, #34572, #38525, #21737, #30120, #34310, #42462, #26188, #25922, #26700, #50323, #6297, #22255, #1842, #30637, #2624, #41669, #34833, #6037, #6549, #42722, #18596, #2102, #10490, #50577, #46661, #10744, #10230, #2355, #33794, #37744, #6817, #18078, #22771, #29854, #18330, #38790, #45608, #18850, #2882, #13645, #45875, #50056, #29605, #21994, #9961, #9707, #25667, #17820, #46139, #41937, #5774, #49803, #30377, #14409, #22515, #13896, #38004, #34046, #14151, #42199, #35352, #40065, #3915, #43238, #46918, #23026, #15962, #7329, #51862, #11784, #4158, #14926, #35088, #7843, #50834, #51090, #3657, #47431, #19370, #31657, #35619, #7076, #23276, #15188, #11524, #23536, #11004, #27224, #47681, #20133, #27992, #12038, #39554, #31403, #39048, #19878, #30890, #26972, #39297, #19628, #31149, #47174, #43487, #3142, #35869, #47937, #31915, #3403, #43995, #27744, #51352, #27484, #8101, #51607, #11262, #42981, #24044, #7590, #15701, #19110, #15450, #43742, #23791, #39807, #41099, #48184, #5210, #12288, #21163, #12815, #20645, #36631, #45291, #733, #17004, #4417, #16211, #20383, #37169, #32422, #24828, #49235, #1266, #17255, #44510, #33218, #13083, #12547, #28770, #13330, #40836, #48445, #5466, #29290, #44771, #36904, #9400, #32168, #8875, #45032, #25349, #41349, #28249, #36124, #44247, #228, #4935, #16730, #32684, #8354, #48711, #32951, #36372, #24305, #479, #40322, #28513, #20908, #16467, #8614, #24562, #40575, #4672, #29036, #1004, #25086, #48978, #9132, #26377, #2559, #6491, #18016, #14088, #41607, #29546, #14605, #25855, #30573, #37677, #10162, #42394, #1522, #26637, #46595, #22448, #1778, #5973, #38455, #29790, #17759, #10684, #42655, #9644, #37942, #49743, #33477, #18533, #38199, #42134, #6233, #21420, #25600, #30049, #33730, #17507, #21930, #37422, #34509, #13833, #49494, #45549, #50515, #45811, #13581, #34236, #5713, #21669, #9898, #30316, #41870, #2036, #26122, #33982, #49997, #2295, #22189, #46077, #18268, #50260, #14347, #46338, #10425, #11918, #4541, #48583, #36507, #609, #28123, #24175, #14863, #38726, #40198 ) ),
 .UNSPECIFIED., .F., .F., .F.,
 ( 4, 4 ),
 ( 4, 1, 1, 1, 1, 1, 1, 1, 1, 1, 1, 1, 1, 1, 1, 1, 1, 1, 1, 1, 1, 1, 1, 1, 1, 1, 1, 1, 1, 1, 1, 1, 1, 1, 1, 1, 1, 1, 1, 1, 1, 1, 1, 1, 1, 1, 1, 1, 1, 1, 1, 1, 1, 1, 1, 1, 1, 1, 1, 1, 1, 1, 1, 1, 1, 1, 1, 1, 1, 1, 1, 1, 1, 1, 1, 1, 1, 1, 1, 1, 1, 1, 1, 1, 1, 1, 1, 1, 1, 1, 1, 1, 1, 1, 1, 1, 1, 1, 1, 1, 1, 1, 1, 1, 1, 1, 1, 1, 1, 1, 1, 1, 1, 1, 1, 1, 1, 1, 1, 1, 1, 1, 1, 1, 1, 1, 1, 1, 1, 1, 1, 1, 1, 1, 1, 1, 1, 1, 1, 1, 1, 1, 1, 1, 1, 1, 1, 1, 1, 1, 1, 1, 1, 1, 1, 1, 1, 1, 1, 1, 1, 1, 1, 1, 1, 1, 1, 1, 1, 1, 1, 1, 1, 1, 1, 1, 1, 1, 1, 1, 1, 1, 1, 1, 1, 1, 1, 1, 1, 1, 1, 1, 1, 1, 1, 1, 1, 1, 1, 1, 1, 1, 1, 1, 1, 1, 1, 1, 1, 1, 1, 1, 1, 1, 1, 1, 1, 1, 1, 1, 1, 1, 1, 1, 1, 1, 1, 1, 1, 1, 1, 1, 1, 1, 1, 1, 1, 1, 1, 1, 1, 1, 1, 1, 1, 1, 1, 1, 1, 1, 1, 1, 1, 1, 1, 1, 1, 1, 1, 1, 1, 1, 1, 1, 1, 1, 1, 1, 1, 1, 1, 1, 1, 1, 1, 1, 1, 1, 1, 1, 1, 1, 1, 1, 1, 1, 1, 1, 1, 1, 1, 1, 1, 1, 1, 1, 1, 1, 1, 1, 1, 1, 1, 1, 1, 1, 1, 1, 1, 1, 1, 1, 1, 1, 4 ),
 ( 0.000000000000000000, 0.1320977415905860153 ),
 ( 11.61503284781839973, 12.11278007152779956, 12.61052729523719940, 13.10827451894659923, 13.60602174265599906, 14.10376896636540067, 14.60151619007480051, 15.09926341378420034, 15.59701063749360017, 16.09475786120300000, 16.59250508491239984, 17.09025230862179967, 17.58799953233119950, 18.08574675604059934, 18.58349397974999917, 19.08124120345940256, 19.57898842716880239, 20.07673565087829815, 20.57448287458770153, 21.07223009829710136, 21.56997732200650120, 22.06772454571590103, 22.56547176942530086, 23.06321899313470070, 23.56096621684410053, 24.05871344055349681, 24.55646066426290020, 25.05420788797230003, 25.55195511168169986, 26.04970233539109969, 26.54744955910049953, 27.04519678280990291, 27.54294400651929919, 28.04069123022870258, 28.53843845393820189, 29.03618567764759817, 29.53393290135700155, 30.03168012506639784, 30.52942734877579767, 31.02717457248520105, 31.52492179619460089, 32.02266901990400072, 32.52041624361339700, 33.01816346732280039, 33.51591069103219667, 34.01365791474160005, 34.51140513845099633, 35.00915236216039972, 35.50689958586980310, 36.00464680957920649, 36.50239403328870225, 37.00014125699809853, 37.49788848070750191, 37.99563570441689819, 38.49338292812630158, 38.99113015183569786, 39.48887737554510124, 39.98662459925449753, 40.48437182296390091, 40.98211904667329719, 41.47986627038269347, 41.97761349409210396, 42.47536071780150024, 42.97310794151090363, 43.47085516522029991, 43.96860238892970330, 44.46634961263909958, 44.96409683634850296, 45.46184406005799872, 45.95959128376739500, 46.45733850747679838, 46.95508573118619466, 47.45283295489559805, 47.95058017860500144, 48.44832740231439772, 48.94607462602380110, 49.44382184973320449, 49.94156907344260077, 50.43931629715199705, 50.93706352086140043, 51.43481074457079671, 51.93255796828020010, 52.43030519198959638, 52.92805241569899977, 53.42579963940849552, 53.92354686311789891, 54.42129408682730229, 54.91904131053670568, 55.41678853424610196, 55.91453575795550535, 56.41228298166490163, 56.91003020537429791, 57.40777742908370129, 57.90552465279309757, 58.40327187650250096, 58.90101910021189724, 59.39876632392130062, 59.89651354763069691, 60.39426077134009319, 60.89200799504950368, 61.38975521875889996, 61.88750244246830334, 62.38524966617779910, 62.88299688988720249, 63.38074411359659877, 63.87849133730600215, 64.37623856101539843, 64.87398578472480892, 65.37173300843420520, 65.86948023214360148, 66.36722745585299776, 66.86497467956239404, 67.36272190327179032, 67.86046912698120082, 68.35821635069059710, 68.85596357440000759, 69.35371079810938966, 69.85145802181880015, 70.34920524552829590, 70.84695246923770640, 71.34469969294710268, 71.84244691665649896, 72.34019414036590945, 72.83794136407529152, 73.33568858778470201, 73.83343581149409829, 74.33118303520349457, 74.82893025891290506, 75.32667748262228713, 75.82442470633169762, 76.32217193004109390, 76.81991915375050439, 77.31766637745990067, 77.81541360116929695, 78.31316082487880692, 78.81090804858810372, 79.30865527229759948, 79.80640249600699576, 80.30414971971639204, 80.80189694342580253, 81.29964416713519881, 81.79739139084459509, 82.29513861455400558, 82.79288583826338765, 83.29063306197279815, 83.78838028568220864, 84.28612750939160492, 84.78387473310100120, 85.28162195681041169, 85.77936918051979376, 86.27711640422919004, 86.77486362793860053, 87.27261085164809629, 87.77035807535740730, 88.26810529906688885, 88.76585252277629934, 89.26359974648569562, 89.76134697019510611, 90.25909419390450239, 90.75684141761389867, 91.25458864132330916, 91.75233586503269123, 92.25008308874210172, 92.74783031245149800, 93.24557753616089428, 93.74332475987030477, 94.24107198357970105, 94.73881920728909733, 95.23656643099860730, 95.73431365470798937, 96.23206087841739986, 96.72980810212679614, 97.22755532583620663, 97.72530254954560291, 98.22304977325499920, 98.72079699696439548, 99.21854422067379176, 99.71629144438320225, 100.2140386680929964, 100.7117858918019948, 101.2095331155110074, 101.7072803392210005, 102.2050275629299989, 102.7027747866400063, 103.2005220103490046, 103.6982692340580030, 104.1960164577680104, 104.6937636814769945, 105.1915109051870019, 105.6892581288960002, 106.1870053526049986, 106.6847525763150060, 107.1824998000240043, 107.6802470237339975, 108.1779942474429959, 108.6757414711520084, 109.1734886948620016, 109.6712359185710000, 110.1689831422810073, 110.6667303659899915, 111.1644775896999988, 111.6622248134089972, 112.1599720371179956, 112.6577192608280029, 113.1554664845370013, 113.6532137082469944, 114.1509609319560070, 114.6487081556649912, 115.1464553793749985, 115.6442026030839969, 116.1419498267940043, 116.6396970505030026, 117.1374442742120010, 117.6351914979219941, 118.1329387216309925, 118.6306859453409999, 119.1284331690499982, 119.6261803927589966, 120.1239276164690040, 120.6216748401779881, 121.1194220638879955, 121.6171692875970081, 122.1149165113060064, 122.6126637350159996, 123.1104109587250122, 123.6081581824349911, 124.1059054061440037, 124.6036526298530021, 125.1013998535629952, 125.5991470772720078, 126.0968943009820009, 126.5946415246909993, 127.0923887484010066, 127.5901359721100050, 128.0878831958189892, 128.5856304195290249, 129.0833776432380091, 129.5811248669479880, 130.0788720906570006, 130.5766193143660132, 131.0743665380759921, 131.5721137617849763, 132.0698609854950121, 132.5676082092039962, 133.0653554329129804, 133.5631026566230162, 134.0608498803320003, 134.5585971040419793, 135.0563443277510203, 135.5540915514600044, 136.0518387751699834, 136.5495859988790244, 137.0473332225890033, 137.5450804462979875, 138.0428276700070001, 138.5405748937170074, 139.0383221174259916, 139.5360693411359989, 140.0338165648450115, 140.5315637885539957, 141.0293110122640030, 141.5270582359729872, 142.0248054596829945, 142.5225526833920071, 143.0202999071019860, 143.5180471308109986, 144.0157943545200112, 144.5135415782299901, 145.0112888019389743, 145.5090360256490101, 146.0067832493579942, 146.5045304730670068, 147.0022776967770142, 147.5000249204859983, 147.9977721441960057, 148.4955193679050183, 148.9932665916140024, 149.4910138153239814, 149.9887610390330224, 150.4865082627430013, 150.9842554864519855, 151.4820027101609980, 151.9797499338710054, 152.4774971575799896, 152.9752443812900253, 153.4729916049990095, 153.9707388287079937, 154.4684860524180010, 154.9662332761270136, 155.4639804998369925, 155.9617277235460051, 156.4594749472550177, 156.9572221709649966, 157.4549693946739808, 157.9527166183839881, 158.4504638420930007, 158.9482110658019849, 159.4459582895120207, 159.9437055132210048, 160.4414527369310122, 160.9391999606399963, 161.4369471843500037, 161.9346944080590163, 162.4324416317680004, 162.9301888554780078, 163.4279360791869919, 163.9256833028969993, 164.4234305266059835, 164.9211777503149960, 165.4189249740250034, 165.9166721977339876, 166.4144194214440233, 166.9121666451530075, 167.4099138688619917, 167.9076610925719990 ),
 .UNSPECIFIED. ) ;
#45208 = VERTEX_POINT ( 'NONE', #43197 ) ;
#45209 = DIRECTION ( 'NONE',  ( 0.000000000000000000, 0.000000000000000000, -1.000000000000000000 ) ) ;
#45210 = CARTESIAN_POINT ( 'NONE',  ( 73.11690592692650625, 0.8925687589132609290, -62.30780775221820278 ) ) ;
#45211 = CARTESIAN_POINT ( 'NONE',  ( 76.14068888614369257, -43.36749149024220173, -13.68366341276339959 ) ) ;
#45212 = ADVANCED_FACE ( 'NONE', ( #28210 ), #31445, .F. ) ;
#45213 = DIRECTION ( 'NONE',  ( 0.5516667872527449834, -0.8340645993220396903, -3.885780586188043947E-16 ) ) ;
#45214 = CARTESIAN_POINT ( 'NONE',  ( 50.03007040746459921, -36.85417771443089663, -76.14999999999999147 ) ) ;
#45215 = FACE_OUTER_BOUND ( 'NONE', #31139, .T. ) ;
#45216 = CARTESIAN_POINT ( 'NONE',  ( 17.90516167065736042, -22.20706873477158894, -78.86948505268290432 ) ) ;
#45217 = CARTESIAN_POINT ( 'NONE',  ( 49.59615837245039671, -53.70224911814690216, -55.11137432941160341 ) ) ;
#45218 = CARTESIAN_POINT ( 'NONE',  ( 12.14969623865099457, -22.52865004270027782, -56.45901417435899106 ) ) ;
#45219 = CARTESIAN_POINT ( 'NONE',  ( 19.33599456300022723, -22.89773004841487847, -33.87591038700520585 ) ) ;
#45220 = CARTESIAN_POINT ( 'NONE',  ( 17.92366719485290005, -51.11618258419110106, -74.34711752987139732 ) ) ;
#45221 = DIRECTION ( 'NONE',  ( -0.7071067811865476838, -0.7071067811865473507, 0.000000000000000000 ) ) ;
#45222 = AXIS2_PLACEMENT_3D ( 'NONE', #13302, #32656, #28745 ) ;
#45223 = VERTEX_POINT ( 'NONE', #35833 ) ;
#45224 = CARTESIAN_POINT ( 'NONE',  ( 19.18353301396849986, -8.818640789972748806, -44.70157888913149691 ) ) ;
#45225 = CARTESIAN_POINT ( 'NONE',  ( 64.56814038767528530, 1.034647430440490234, -60.83434081278629435 ) ) ;
#45226 = EDGE_LOOP ( 'NONE', ( #30724, #9665, #22232, #34240 ) ) ;
#45227 = CARTESIAN_POINT ( 'NONE',  ( 71.33393739769628894, 1.383811055320669947, -62.44999999999999574 ) ) ;
#45228 = CARTESIAN_POINT ( 'NONE',  ( 61.29825847224749680, -45.52681296980589565, -47.59225652243559779 ) ) ;
#45229 = LINE ( 'NONE', #28965, #48003 ) ;
#45230 = CARTESIAN_POINT ( 'NONE',  ( 50.39461195648269864, 18.90258328430419965, -76.14999999999999147 ) ) ;
#45232 = DIRECTION ( 'NONE',  ( 0.000000000000000000, 0.000000000000000000, 1.000000000000000000 ) ) ;
#45231 = CARTESIAN_POINT ( 'NONE',  ( 45.05789191074332223, 8.802198375054555157, -61.53174790021666496 ) ) ;
#45233 = CARTESIAN_POINT ( 'NONE',  ( -31.36606260230380272, -53.11618894467930119, 16.35000000000000142 ) ) ;
#45234 = CARTESIAN_POINT ( 'NONE',  ( 60.70500520956167634, 28.95487886718607839, 17.35000000000000142 ) ) ;
#45235 = EDGE_LOOP ( 'NONE', ( #9283, #19260, #47579, #37557 ) ) ;
#45236 = ORIENTED_EDGE ( 'NONE', *, *, #46212, .F. ) ;
#45237 = ORIENTED_EDGE ( 'NONE', *, *, #12008, .F. ) ;
#45238 = ORIENTED_EDGE ( 'NONE', *, *, #33909, .T. ) ;
#45239 = CARTESIAN_POINT ( 'NONE',  ( 61.48302575854449969, -45.30855424813389476, -47.22534401859969933 ) ) ;
#45240 = VECTOR ( 'NONE', #26600, 1000.000000000000000 ) ;
#45241 = CYLINDRICAL_SURFACE ( 'NONE', #6486, 0.9999999999999976685 ) ;
#45242 = CIRCLE ( 'NONE', #37666, 1.999999999999998224 ) ;
#45243 = CYLINDRICAL_SURFACE ( 'NONE', #24288, 0.4999999999999992784 ) ;
#45244 = ORIENTED_EDGE ( 'NONE', *, *, #41352, .F. ) ;
#45245 = VERTEX_POINT ( 'NONE', #31363 ) ;
#45246 = AXIS2_PLACEMENT_3D ( 'NONE', #25033, #38880, #1217 ) ;
#45247 = CARTESIAN_POINT ( 'NONE',  ( 62.09157612670949788, -33.11618894467940066, -65.34607522167520699 ) ) ;
#45248 = ORIENTED_EDGE ( 'NONE', *, *, #9121, .T. ) ;
#45249 = CARTESIAN_POINT ( 'NONE',  ( 22.87920509261272883, -16.16928286307435769, -72.47886173722646674 ) ) ;
#45250 = CARTESIAN_POINT ( 'NONE',  ( 19.34932770686961589, -27.61618894467928698, -22.14999999999998792 ) ) ;
#45251 = DIRECTION ( 'NONE',  ( -1.000000000000000000, -1.007258792502662152E-15, 0.000000000000000000 ) ) ;
#45252 = ADVANCED_FACE ( 'NONE', ( #47392 ), #23252, .T. ) ;
#45253 = DIRECTION ( 'NONE',  ( 0.5720614028176843613, 0.4156269377774527984, 0.7071067811865479058 ) ) ;
#45254 = DIRECTION ( 'NONE',  ( 0.000000000000000000, 0.000000000000000000, -1.000000000000000000 ) ) ;
#45255 = ORIENTED_EDGE ( 'NONE', *, *, #21105, .F. ) ;
#45256 = CARTESIAN_POINT ( 'NONE',  ( 2.558369240368420172, -25.18609768228349921, -34.64999999999999858 ) ) ;
#45257 = CARTESIAN_POINT ( 'NONE',  ( 52.95141962741540453, -51.03458903264449731, -76.06582098811649928 ) ) ;
#45258 = CARTESIAN_POINT ( 'NONE',  ( 10.72254675965764115, -19.77476841094461690, -47.24445590664701911 ) ) ;
#45259 = CARTESIAN_POINT ( 'NONE',  ( 60.55537580064579828, 14.38087405962720133, -47.18092733277320150 ) ) ;
#45260 = CARTESIAN_POINT ( 'NONE',  ( 18.67428148936129872, -23.04137577650549673, -66.40756600056339209 ) ) ;
#45261 = CARTESIAN_POINT ( 'NONE',  ( 8.731180243531472485, 17.69319178430564321, -34.79644561402098191 ) ) ;
#45262 = CARTESIAN_POINT ( 'NONE',  ( 42.39659219033849524, 13.74223253253360078, -5.990488029809371007 ) ) ;
#45263 = CARTESIAN_POINT ( 'NONE',  ( 41.66707677620669870, -44.64833008590599661, -5.278831885195840457 ) ) ;
#45264 = CARTESIAN_POINT ( 'NONE',  ( 64.04379473442959636, 1.409763143870969904, -69.80805258500740251 ) ) ;
#45265 = CARTESIAN_POINT ( 'NONE',  ( 46.66402864381289817, 8.651351690988509091, -54.57073507588959416 ) ) ;
#45266 = CARTESIAN_POINT ( 'NONE',  ( 67.73241107036501774, 0.07875534547170300048, -17.99564714788500197 ) ) ;
#45267 = VERTEX_POINT ( 'NONE', #16170 ) ;
#45268 = CARTESIAN_POINT ( 'NONE',  ( 14.09076352594090054, -51.44957460137000282, -75.17186369577468952 ) ) ;
#45269 = CARTESIAN_POINT ( 'NONE',  ( 47.18324198357289845, -54.80726809202429450, -54.61058319554170026 ) ) ;
#45270 = ADVANCED_FACE ( 'NONE', ( #12773 ), #16431, .T. ) ;
#45271 = FACE_BOUND ( 'NONE', #36274, .T. ) ;
#45272 = DIRECTION ( 'NONE',  ( 1.000000000000000000, 0.000000000000000000, 0.000000000000000000 ) ) ;
#45273 = VECTOR ( 'NONE', #12604, 1000.000000000000000 ) ;
#45274 = AXIS2_PLACEMENT_3D ( 'NONE', #15056, #23666, #43869 ) ;
#45275 = CARTESIAN_POINT ( 'NONE',  ( 22.63728796599880155, -19.53131553281569666, -32.14999999999999858 ) ) ;
#45276 = CARTESIAN_POINT ( 'NONE',  ( 57.38152646595799666, 14.21216655855363875, -26.07295477665448757 ) ) ;
#45277 = CARTESIAN_POINT ( 'NONE',  ( 11.14146392938010166, 33.97654110380459969, -17.73105615077219710 ) ) ;
#45279 = CARTESIAN_POINT ( 'NONE',  ( 72.13393739769620083, -1.116188944679340045, -20.65000000000000213 ) ) ;
#45278 = DIRECTION ( 'NONE',  ( 1.000000000000000000, 0.000000000000000000, 0.000000000000000000 ) ) ;
#45280 = ADVANCED_FACE ( 'NONE', ( #17471 ), #33437, .F. ) ;
#45281 = DIRECTION ( 'NONE',  ( 0.000000000000000000, -1.000000000000000000, 0.000000000000000000 ) ) ;
#45282 = CARTESIAN_POINT ( 'NONE',  ( 48.60495210931490107, 22.85368323561639770, -54.93239174769010447 ) ) ;
#45283 = VERTEX_POINT ( 'NONE', #45256 ) ;
#45284 = CARTESIAN_POINT ( 'NONE',  ( 14.78993376734899989, -8.692590644946379896, -64.28614875238550042 ) ) ;
#45285 = ORIENTED_EDGE ( 'NONE', *, *, #20913, .F. ) ;
#45286 = CARTESIAN_POINT ( 'NONE',  ( 70.99050876911339003, 0.8838110553206759423, -60.94999999999999574 ) ) ;
#45287 = CARTESIAN_POINT ( 'NONE',  ( 68.13393739769618662, -29.66618894467940137, -40.64999999999999858 ) ) ;
#45288 = CARTESIAN_POINT ( 'NONE',  ( 22.90121965235462653, -15.61618904849089340, -42.45282069170939110 ) ) ;
#45290 = CARTESIAN_POINT ( 'NONE',  ( 52.56521762488900151, 18.62942129817990278, -28.06242660726239890 ) ) ;
#45289 = CARTESIAN_POINT ( 'NONE',  ( 83.70743316420070812, 13.68261143785749923, -47.36488538498209522 ) ) ;
#45291 = CARTESIAN_POINT ( 'NONE',  ( 10.02550514365970002, -12.09062316108200008, -61.61944235566640060 ) ) ;
#45292 = DIRECTION ( 'NONE',  ( 0.07088902009066748444, 0.000000000000000000, 0.9974842088126432138 ) ) ;
#45293 = CARTESIAN_POINT ( 'NONE',  ( 72.72056432233058842, 1.396834109478129804, -68.84999999999999432 ) ) ;
#45294 = CARTESIAN_POINT ( 'NONE',  ( 24.04513741079867017, -15.61618875311435417, -79.79232954107749265 ) ) ;
#45295 = ORIENTED_EDGE ( 'NONE', *, *, #10112, .F. ) ;
#45296 = PRODUCT_DEFINITION ( 'UNKNOWN', '', #30180, #34741 ) ;
#45297 = ORIENTED_EDGE ( 'NONE', *, *, #14353, .T. ) ;
#45298 = CARTESIAN_POINT ( 'NONE',  ( 12.05606148284189949, -65.16757949402220618, -16.66333073004830112 ) ) ;
#45299 = CARTESIAN_POINT ( 'NONE',  ( 12.30109459971790109, 34.11576030229039702, -46.67181612106659827 ) ) ;
#45300 = CARTESIAN_POINT ( 'NONE',  ( 8.824272223518924818, -12.52937285024285430, -38.63483393334039562 ) ) ;
#45301 = DIRECTION ( 'NONE',  ( 0.000000000000000000, -0.7071067811865492381, 0.7071067811865457964 ) ) ;
#45302 = CARTESIAN_POINT ( 'NONE',  ( 10.52748814419759960, -64.93771388453561144, -47.11278010051370302 ) ) ;
#45303 = ORIENTED_EDGE ( 'NONE', *, *, #40536, .T. ) ;
#45304 = CARTESIAN_POINT ( 'NONE',  ( -1.553653935055010038, -50.14529331550839686, -36.11652824808269457 ) ) ;
#45305 = DIRECTION ( 'NONE',  ( 1.000000000000000000, 0.000000000000000000, 0.000000000000000000 ) ) ;
#45306 = CARTESIAN_POINT ( 'NONE',  ( 52.82975622904280755, 18.42854261028849905, -28.15000000000000213 ) ) ;
#45307 = EDGE_CURVE ( 'NONE', #50075, #21125, #26623, .T. ) ;
#45308 = CARTESIAN_POINT ( 'NONE',  ( 52.92565939194879832, 18.90186872980919830, -50.10275203585430148 ) ) ;
#45309 = DIRECTION ( 'NONE',  ( -1.000000000000000000, 0.000000000000000000, 0.000000000000000000 ) ) ;
#45310 = CARTESIAN_POINT ( 'NONE',  ( 50.31596467094429670, -49.96707859667039742, -76.14999999999999147 ) ) ;
#45311 = EDGE_CURVE ( 'NONE', #13640, #4297, #9744, .T. ) ;
#45312 = CARTESIAN_POINT ( 'NONE',  ( 8.222936843878629887, -16.65173236265913204, -44.46600688272611279 ) ) ;
#45313 = VECTOR ( 'NONE', #5265, 1000.000000000000000 ) ;
#45314 = ORIENTED_EDGE ( 'NONE', *, *, #31431, .F. ) ;
#45315 = EDGE_CURVE ( 'NONE', #24832, #6439, #49455, .T. ) ;
#45316 = CARTESIAN_POINT ( 'NONE',  ( 53.67452698258109933, -48.64253627208800168, -26.37822025900069889 ) ) ;
#45317 = CARTESIAN_POINT ( 'NONE',  ( 68.13393739769769297, 18.72622661238300168, -73.39853292320978539 ) ) ;
#45318 = ORIENTED_EDGE ( 'NONE', *, *, #18444, .F. ) ;
#45319 = CARTESIAN_POINT ( 'NONE',  ( 12.14992535548874919, -8.703598238564360656, -56.84100149383260003 ) ) ;
#45320 = CARTESIAN_POINT ( 'NONE',  ( 45.07858682377059978, -46.11248607424209922, -9.026855431852869316 ) ) ;
#45321 = CIRCLE ( 'NONE', #3505, 5.500000000000005329 ) ;
#45322 = EDGE_CURVE ( 'NONE', #16107, #47514, #34825, .T. ) ;
#45323 = CARTESIAN_POINT ( 'NONE',  ( 22.58091822151520134, -20.09091640553009839, -38.20562654191479623 ) ) ;
#45324 = CARTESIAN_POINT ( 'NONE',  ( 14.05644112269600043, -51.15811488272049701, -22.83288693232809763 ) ) ;
#45325 = CARTESIAN_POINT ( 'NONE',  ( 53.68554366443980541, 19.91410632359709965, -75.73797465767289339 ) ) ;
#45326 = CARTESIAN_POINT ( 'NONE',  ( 47.24348367421029593, -54.32908577617870094, -75.29143818916560349 ) ) ;
#45327 = EDGE_LOOP ( 'NONE', ( #22967, #29891, #50328, #28587, #25624, #30426 ) ) ;
#45328 = CARTESIAN_POINT ( 'NONE',  ( 56.08436867299899831, 14.47011214112430011, -17.76910799214320136 ) ) ;
#45329 = CARTESIAN_POINT ( 'NONE',  ( 22.90082190116586602, -14.57027037197810060, -46.79796611410813512 ) ) ;
#45330 = EDGE_CURVE ( 'NONE', #36574, #40950, #24099, .T. ) ;
#45331 = CARTESIAN_POINT ( 'NONE',  ( 9.095229150429339882, -16.06244602788209974, -37.82702577713659764 ) ) ;
#45332 = CARTESIAN_POINT ( 'NONE',  ( 12.40732551566485320, 34.15351444851818030, -23.57257803396428386 ) ) ;
#45333 = ORIENTED_EDGE ( 'NONE', *, *, #43822, .T. ) ;
#45334 = CARTESIAN_POINT ( 'NONE',  ( 46.85154411375850714, 22.40880507094490071, -75.96071349691810326 ) ) ;
#45335 = CARTESIAN_POINT ( 'NONE',  ( 64.99525386628140211, 0.8838110553206759423, -60.53635606803790381 ) ) ;
#45336 = EDGE_CURVE ( 'NONE', #32200, #38150, #5740, .T. ) ;
#45337 = CARTESIAN_POINT ( 'NONE',  ( 75.16192729188773569, -29.52942022316926440, -11.85564034879345741 ) ) ;
#45338 = CARTESIAN_POINT ( 'NONE',  ( 66.53393739769619231, 10.88381105532070059, -69.34999999999999432 ) ) ;
#45339 = CARTESIAN_POINT ( 'NONE',  ( 8.509650980192089875, -12.47724301513739853, -80.63198581093510597 ) ) ;
#45340 = CARTESIAN_POINT ( 'NONE',  ( 9.366937397696199596, -15.61618894467949836, -28.45282021618999835 ) ) ;
#45341 = DIRECTION ( 'NONE',  ( 0.7071067811865475727, -0.7071067811865475727, 0.000000000000000000 ) ) ;
#45343 = CARTESIAN_POINT ( 'NONE',  ( 46.56087410975415253, -40.27520908467922567, -53.62939914585523127 ) ) ;
#45342 = CARTESIAN_POINT ( 'NONE',  ( 64.79174514991440503, 0.8925687589132609290, -60.66703147076970737 ) ) ;
#45344 = CARTESIAN_POINT ( 'NONE',  ( 61.23052733764490085, 14.02714310753309945, -46.65867039562650120 ) ) ;
#45345 = CARTESIAN_POINT ( 'NONE',  ( 9.807758692938932654, -10.75452821090589239, -68.71600247355699764 ) ) ;
#45346 = CARTESIAN_POINT ( 'NONE',  ( -31.82194261889170050, -25.03117784670399715, -55.69495912570319973 ) ) ;
#45347 = ORIENTED_EDGE ( 'NONE', *, *, #33917, .F. ) ;
#45348 = TOROIDAL_SURFACE ( 'NONE', #32735, 47.00000000000000000, 3.000000000000000000 ) ;
#45349 = CARTESIAN_POINT ( 'NONE',  ( 52.93112654626390423, -49.60820240547079862, -48.77840571416800231 ) ) ;
#45350 = AXIS2_PLACEMENT_3D ( 'NONE', #29928, #10300, #26001 ) ;
#45351 = EDGE_CURVE ( 'NONE', #45801, #32578, #41716, .T. ) ;
#45352 = CARTESIAN_POINT ( 'NONE',  ( 57.40499924366620377, -45.30275284725809826, -25.91811620706180008 ) ) ;
#45353 = CARTESIAN_POINT ( 'NONE',  ( 75.04939620295748171, -15.61618894467929941, -11.30491871076499955 ) ) ;
#45354 = CARTESIAN_POINT ( 'NONE',  ( 57.48164938133449908, 13.89721140088779983, -25.54051126100410229 ) ) ;
#45355 = VECTOR ( 'NONE', #45253, 1000.000000000000000 ) ;
#45356 = CARTESIAN_POINT ( 'NONE',  ( 23.14492557087420010, -16.38339395781729735, -38.48751448508959783 ) ) ;
#45357 = CARTESIAN_POINT ( 'NONE',  ( 50.23538082579219832, 18.53774256725959901, -76.14999999999999147 ) ) ;
#45358 = CARTESIAN_POINT ( 'NONE',  ( 53.21058286982849950, 18.26096715473390120, -49.03901014878070441 ) ) ;
#45359 = CARTESIAN_POINT ( 'NONE',  ( 71.21710443884710173, 1.384378348444520013, -70.31241234944640439 ) ) ;
#45360 = CARTESIAN_POINT ( 'NONE',  ( 60.71739103784720015, -45.52836762685870298, -47.07893917820750573 ) ) ;
#45361 = CARTESIAN_POINT ( 'NONE',  ( 68.66192157695549270, -45.11618894467940066, -13.19177143207549996 ) ) ;
#45362 = ORIENTED_EDGE ( 'NONE', *, *, #31656, .F. ) ;
#45363 = CARTESIAN_POINT ( 'NONE',  ( 22.73945831596759959, -19.06202523455430153, -73.22039407203459405 ) ) ;
#45364 = CARTESIAN_POINT ( 'NONE',  ( 73.00772670898579975, 1.265401080857980087, -68.86031185997930493 ) ) ;
#45365 = CARTESIAN_POINT ( 'NONE',  ( 47.39313543291059716, -54.66174527355829582, -54.87093675547399840 ) ) ;
#45366 = DIRECTION ( 'NONE',  ( 0.000000000000000000, 0.000000000000000000, -1.000000000000000000 ) ) ;
#45367 = CARTESIAN_POINT ( 'NONE',  ( 73.20987945474540481, 1.101170701158060039, -62.53612607382319766 ) ) ;
#45368 = CARTESIAN_POINT ( 'NONE',  ( 58.69128839982990087, 16.72420414854200033, -50.02955822931539132 ) ) ;
#45369 = CARTESIAN_POINT ( 'NONE',  ( 52.96846354095290366, 18.35586996326500042, -48.76456332840290031 ) ) ;
#45370 = CARTESIAN_POINT ( 'NONE',  ( 11.48393739769620048, -15.61618894467929941, -14.03562394879499919 ) ) ;
#45371 = CARTESIAN_POINT ( 'NONE',  ( 71.71899590570779992, 1.318402576460610209, -61.03419568858579680 ) ) ;
#45372 = CARTESIAN_POINT ( 'NONE',  ( 73.01385068780759013, 0.9098571636355720083, -69.14090909090960224 ) ) ;
#45373 = CARTESIAN_POINT ( 'NONE',  ( 65.03752560835739871, 1.369664981662529923, -70.37861443921559612 ) ) ;
#45374 = ORIENTED_EDGE ( 'NONE', *, *, #35536, .F. ) ;
#45375 = CARTESIAN_POINT ( 'NONE',  ( 9.275121881254090539, -63.12602292003808913, -46.53341764687979776 ) ) ;
#45376 = CARTESIAN_POINT ( 'NONE',  ( 16.13393739769620083, -15.61618894467929941, -32.14999999999999858 ) ) ;
#45377 = EDGE_LOOP ( 'NONE', ( #48267, #44201, #28545, #20530, #40919, #51041, #43062, #21531 ) ) ;
#45378 = DIRECTION ( 'NONE',  ( -1.000000000000000000, 0.000000000000000000, 0.000000000000000000 ) ) ;
#45379 = CARTESIAN_POINT ( 'NONE',  ( 84.25370905163079271, 12.95080358240966589, -47.43624044227698278 ) ) ;
#45380 = CARTESIAN_POINT ( 'NONE',  ( 19.36900924991789807, -21.88331502330690270, -53.19549840347880121 ) ) ;
#45381 = EDGE_CURVE ( 'NONE', #5682, #19762, #29472, .T. ) ;
#45382 = CARTESIAN_POINT ( 'NONE',  ( 51.52597262436339776, 19.39045939329939827, -76.24693439086530589 ) ) ;
#45383 = EDGE_LOOP ( 'NONE', ( #42403, #2778, #4566, #34138, #9123 ) ) ;
#45384 = PRODUCT_DEFINITION_SHAPE ( 'NONE', 'NONE',  #51874 ) ;
#45385 = CARTESIAN_POINT ( 'NONE',  ( 61.28610861176739633, 13.99802266614350010, -46.54508491471729315 ) ) ;
#45386 = LINE ( 'NONE', #9492, #5071 ) ;
#45387 = CARTESIAN_POINT ( 'NONE',  ( 10.76140486198004353, -21.45664709977270235, -66.24430264515250144 ) ) ;
#45388 = EDGE_CURVE ( 'NONE', #3175, #17463, #3240, .T. ) ;
#45389 = CARTESIAN_POINT ( 'NONE',  ( 14.81123514133290087, -23.75456585884019844, -50.34361688518850286 ) ) ;
#45390 = LINE ( 'NONE', #9495, #16250 ) ;
#45391 = CARTESIAN_POINT ( 'NONE',  ( 42.90933435587908207, -37.76413940282665749, -75.77300232340927266 ) ) ;
#45392 = ORIENTED_EDGE ( 'NONE', *, *, #29794, .T. ) ;
#45393 = AXIS2_PLACEMENT_3D ( 'NONE', #41396, #40881, #33266 ) ;
#45394 = CARTESIAN_POINT ( 'NONE',  ( 56.86403139865790024, -45.97907083540439999, -26.24559160732940200 ) ) ;
#45395 = CARTESIAN_POINT ( 'NONE',  ( 19.04528445129210112, -22.47408600855129990, -44.60486606752809990 ) ) ;
#45396 = CIRCLE ( 'NONE', #4334, 36.00000000000000000 ) ;
#45397 = CARTESIAN_POINT ( 'NONE',  ( 52.10267379959660161, 1.883811054221469883, -20.65000000000000213 ) ) ;
#45398 = CARTESIAN_POINT ( 'NONE',  ( 14.33270604179080010, 20.31584378320569684, -75.38352342698830455 ) ) ;
#45399 = ADVANCED_FACE ( 'NONE', ( #4629 ), #16613, .F. ) ;
#45400 = DIRECTION ( 'NONE',  ( 0.000000000000000000, 0.000000000000000000, -1.000000000000000000 ) ) ;
#45401 = DIRECTION ( 'NONE',  ( 0.000000000000000000, 0.000000000000000000, -1.000000000000000000 ) ) ;
#45402 = CARTESIAN_POINT ( 'NONE',  ( 14.95141725257159848, -23.77611338154449783, -50.05347842037799211 ) ) ;
#45403 = EDGE_LOOP ( 'NONE', ( #15655, #38827, #27941, #15445, #50021 ) ) ;
#45404 = CARTESIAN_POINT ( 'NONE',  ( 54.23558483962950305, -48.00900124132819258, -26.19310004703979899 ) ) ;
#45405 = CARTESIAN_POINT ( 'NONE',  ( 16.44553025965039694, -51.11619093951029669, -20.85618808646060174 ) ) ;
#45406 = CARTESIAN_POINT ( 'NONE',  ( 6.676100005714199703, 28.78052395729680057, -12.44386222061440073 ) ) ;
#45407 = CARTESIAN_POINT ( 'NONE',  ( 14.36259785100323505, -22.20703835893396061, -57.03609844898498693 ) ) ;
#45408 = CARTESIAN_POINT ( 'NONE',  ( 22.90108808520262329, -15.61618901356150069, -52.45282226904397049 ) ) ;
#45409 = ORIENTED_EDGE ( 'NONE', *, *, #7052, .T. ) ;
#45410 =( BOUNDED_SURFACE ( )  B_SPLINE_SURFACE ( 2, 2, ( 
 ( #6258, #5737, #5997, #34263, #34010, #50287, #14374, #26148, #10189 ),
 ( #10450, #9423, #2065, #38225, #46363, #30340, #41374, #13607, #22216 ),
 ( #26403, #13859, #29816, #38483, #45833, #2319, #21696, #9667, #45317 ),
 ( #18041, #49767, #18291, #42424, #5488, #50539, #37704, #6514, #22474 ),
 ( #17782, #2583, #18558, #34534, #29312, #25884, #21956, #25373, #21446 ) ),
 .UNSPECIFIED., .F., .T., .T. ) 
 B_SPLINE_SURFACE_WITH_KNOTS ( ( 3, 2, 3 ),
 ( 3, 2, 2, 2, 3 ),
 ( -0.003205554297748039981, 0.8238407534185530068, 1.650887061134849843 ),
 ( -3.141592653589790007, -1.570796326794899889, 0.000000000000000000, 1.570796326794899889, 3.141592653589790007 ),
 .UNSPECIFIED. ) 
 GEOMETRIC_REPRESENTATION_ITEM ( )  RATIONAL_B_SPLINE_SURFACE ( (
 ( 1.000000000000000000, 0.7071067811865480168, 1.000000000000000000, 0.7071067811865480168, 1.000000000000000000, 0.7071067811865480168, 1.000000000000000000, 0.7071067811865480168, 1.000000000000000000),
 ( 0.9157107718030679244, 0.6475052963475169676, 0.9157107718030679244, 0.6475052963475169676, 0.9157107718030679244, 0.6475052963475169676, 0.9157107718030679244, 0.6475052963475169676, 0.9157107718030679244),
 ( 1.000000000000000000, 0.7071067811865480168, 1.000000000000000000, 0.7071067811865480168, 1.000000000000000000, 0.7071067811865480168, 1.000000000000000000, 0.7071067811865480168, 1.000000000000000000),
 ( 0.9157107718030469412, 0.6475052963475019796, 0.9157107718030469412, 0.6475052963475019796, 0.9157107718030469412, 0.6475052963475019796, 0.9157107718030469412, 0.6475052963475019796, 0.9157107718030469412),
 ( 1.000000000000000000, 0.7071067811865480168, 1.000000000000000000, 0.7071067811865480168, 1.000000000000000000, 0.7071067811865480168, 1.000000000000000000, 0.7071067811865480168, 1.000000000000000000) ) ) 
 REPRESENTATION_ITEM ( '' )  SURFACE ( )  );
#45411 = CARTESIAN_POINT ( 'NONE',  ( -6.536610114769960234, -46.12166273162970498, -4.851352225809789864 ) ) ;
#45412 = B_SPLINE_CURVE_WITH_KNOTS ( 'NONE', 3,
 ( #32061, #36267, #377, #16359, #40466, #4561, #20531, #44659, #8764, #24713, #40730, #17404, #41505, #49389, #1418, #33372, #33631, #13485, #29444 ),
 .UNSPECIFIED., .F., .F.,
 ( 4, 2, 2, 1, 1, 2, 2, 1, 1, 1, 2, 4 ),
 ( 0.000000000000000000, 0.2499999999999918954, 0.3124999999999898970, 0.3281249999999893419, 0.3320312499999892308, 0.3330078124999892308, 0.3339843749999891753, 0.3359374999999891753, 0.3437499999999892863, 0.3749999999999897859, 0.4999999999999917843, 1.000000000000000000 ),
 .UNSPECIFIED. ) ;
#45413 = CARTESIAN_POINT ( 'NONE',  ( 47.54190215014880039, 23.33258332477480224, -54.75916635913850428 ) ) ;
#45414 = EDGE_CURVE ( 'NONE', #24458, #33328, #19158, .T. ) ;
#45415 = CARTESIAN_POINT ( 'NONE',  ( 56.50435945713609698, -45.38311456361396523, -25.29338994599695667 ) ) ;
#45416 = CARTESIAN_POINT ( 'NONE',  ( 63.38363568028500339, 1.325841671674429900, -62.37472934403619718 ) ) ;
#45417 = CARTESIAN_POINT ( 'NONE',  ( 57.24929572629130092, -50.61618894467930119, -53.91492775910359114 ) ) ;
#45418 = CARTESIAN_POINT ( 'NONE',  ( 11.06646955189519943, 33.78253783233920160, -17.18453609578200059 ) ) ;
#45419 = DIRECTION ( 'NONE',  ( 0.000000000000000000, 0.000000000000000000, 1.000000000000000000 ) ) ;
#45420 = CARTESIAN_POINT ( 'NONE',  ( 52.98014233026830055, 18.34975111832529748, -48.77045026161920305 ) ) ;
#45421 = CARTESIAN_POINT ( 'NONE',  ( 15.05440318628160057, -53.11618894467930119, -76.14999999999999147 ) ) ;
#45422 = CARTESIAN_POINT ( 'NONE',  ( 55.20159258013029557, -48.56083622538359634, -48.75785604020860120 ) ) ;
#45423 = DIRECTION ( 'NONE',  ( 0.000000000000000000, 0.000000000000000000, -1.000000000000000000 ) ) ;
#45424 = ADVANCED_FACE ( 'NONE', ( #36866 ), #28993, .T. ) ;
#45425 = CARTESIAN_POINT ( 'NONE',  ( 56.30248980166020090, 19.39266325063019991, -52.97169149132179911 ) ) ;
#45426 = CARTESIAN_POINT ( 'NONE',  ( 63.55717560081600226, 1.377109494087380037, -69.13845142168129598 ) ) ;
#45427 = DIRECTION ( 'NONE',  ( 0.000000000000000000, 0.000000000000000000, 1.000000000000000000 ) ) ;
#45428 = CARTESIAN_POINT ( 'NONE',  ( 52.06789743686220362, 13.88381105532070059, -11.75767006323859931 ) ) ;
#45429 = EDGE_LOOP ( 'NONE', ( #6780, #901, #1091, #46755 ) ) ;
#45430 = CARTESIAN_POINT ( 'NONE',  ( 71.24581987525910165, 0.9960089569207349891, -60.52992920782880049 ) ) ;
#45431 = CARTESIAN_POINT ( 'NONE',  ( 9.739676515705429694, 32.00768368828209987, -46.29753770347090125 ) ) ;
#45432 = AXIS2_PLACEMENT_3D ( 'NONE', #2133, #13931, #9738 ) ;
#45433 = CARTESIAN_POINT ( 'NONE',  ( 45.24668088971260005, 13.87996455531310147, -7.238505014500240087 ) ) ;
#45434 = B_SPLINE_CURVE_WITH_KNOTS ( 'NONE', 3,
 ( #28183, #37102, #8807, #36568, #16660, #9337, #40769, #1199, #4600, #32879, #44184, #17191 ),
 .UNSPECIFIED., .F., .F.,
 ( 4, 2, 2, 2, 2, 4 ),
 ( 0.2986826963453840245, 0.3113669956202789746, 0.6672149786996869336, 0.8896199681243159851, 1.000822462836630011, 1.104809710335580064 ),
 .UNSPECIFIED. ) ;
#45435 = CARTESIAN_POINT ( 'NONE',  ( 12.62325813502959981, -8.714595329762380160, -81.23899999999999011 ) ) ;
#45436 = CARTESIAN_POINT ( 'NONE',  ( 17.85627069094109842, 20.07361457936550053, -75.01675372117850316 ) ) ;
#45437 = VERTEX_POINT ( 'NONE', #42618 ) ;
#45438 = ORIENTED_EDGE ( 'NONE', *, *, #21884, .F. ) ;
#45439 = CARTESIAN_POINT ( 'NONE',  ( 52.82975622904280755, -49.66092049964720445, -48.47378032971909789 ) ) ;
#45440 = ORIENTED_EDGE ( 'NONE', *, *, #39899, .T. ) ;
#45441 = CARTESIAN_POINT ( 'NONE',  ( 10.96794134783359986, -64.35858938242169813, -45.78400131938840190 ) ) ;
#45442 = CARTESIAN_POINT ( 'NONE',  ( 56.56917054403719902, -45.93657512408730526, -26.17243226664860245 ) ) ;
#45443 = CARTESIAN_POINT ( 'NONE',  ( 9.543053535305935142, -17.38739775376582841, -45.36949389193291182 ) ) ;
#45444 = EDGE_CURVE ( 'NONE', #4837, #33893, #22151, .T. ) ;
#45445 = CARTESIAN_POINT ( 'NONE',  ( 61.58832133341670101, 13.92430514912590134, -46.73588551253889989 ) ) ;
#45446 = CARTESIAN_POINT ( 'NONE',  ( 2.404741263826560171, -25.85214510508460251, -35.14999999999999858 ) ) ;
#45447 = ORIENTED_EDGE ( 'NONE', *, *, #44756, .T. ) ;
#45448 = CARTESIAN_POINT ( 'NONE',  ( 46.64226618924153911, 6.984935876691593215, -57.10832150000753415 ) ) ;
#45449 = EDGE_CURVE ( 'NONE', #37059, #18021, #30534, .T. ) ;
#45450 = VERTEX_POINT ( 'NONE', #46557 ) ;
#45451 = CARTESIAN_POINT ( 'NONE',  ( 53.63777509634339680, -45.61032762683289832, -14.62067372278509936 ) ) ;
#45452 = LINE ( 'NONE', #29185, #45553 ) ;
#45453 = DIRECTION ( 'NONE',  ( 0.000000000000000000, 0.000000000000000000, -1.000000000000000000 ) ) ;
#45454 = VERTEX_POINT ( 'NONE', #21631 ) ;
#45455 = CARTESIAN_POINT ( 'NONE',  ( 28.13393739769619728, -8.687985714403851034, -35.14999999999999858 ) ) ;
#45456 = CARTESIAN_POINT ( 'NONE',  ( 47.08252998902620590, -54.52665379529010181, -75.17661032366730467 ) ) ;
#45457 = DIRECTION ( 'NONE',  ( 0.000000000000000000, 0.000000000000000000, -1.000000000000000000 ) ) ;
#45458 = CARTESIAN_POINT ( 'NONE',  ( 50.03007040746459921, -48.61618894467930119, -76.14999999999999147 ) ) ;
#45459 = DIRECTION ( 'NONE',  ( 0.000000000000000000, 1.000000000000000000, 0.000000000000000000 ) ) ;
#45460 = CARTESIAN_POINT ( 'NONE',  ( 16.13393739769620083, -15.61618894467929941, -10.44999999999999929 ) ) ;
#45461 = AXIS2_PLACEMENT_3D ( 'NONE', #5436, #14062, #9870 ) ;
#45462 = AXIS2_PLACEMENT_3D ( 'NONE', #48042, #28096, #19734 ) ;
#45463 = CARTESIAN_POINT ( 'NONE',  ( 6.488481933958597736, -58.66853282520657586, -10.99658928318876328 ) ) ;
#45464 = CARTESIAN_POINT ( 'NONE',  ( 61.58992610407029389, 13.89565648923180063, -28.08969723792819906 ) ) ;
#45465 = CARTESIAN_POINT ( 'NONE',  ( 21.45970996866769909, -9.852258453645399428, -75.02493559595789918 ) ) ;
#45466 = VERTEX_POINT ( 'NONE', #22414 ) ;
#45467 = DIRECTION ( 'NONE',  ( 1.000000000000000000, 0.000000000000000000, 0.000000000000000000 ) ) ;
#45468 = CARTESIAN_POINT ( 'NONE',  ( -9.951751048134941158, -43.31993781838389879, -6.292775219062558989 ) ) ;
#45469 = CARTESIAN_POINT ( 'NONE',  ( 75.44426646237340606, -42.28045139918640416, -13.24736862165440066 ) ) ;
#45470 = CARTESIAN_POINT ( 'NONE',  ( 72.71656993463111007, 0.9860880133275220505, -69.52393415259200538 ) ) ;
#45471 = CARTESIAN_POINT ( 'NONE',  ( 11.06646970394739959, -65.01491572843740130, -17.18453585839250053 ) ) ;
#45472 = CARTESIAN_POINT ( 'NONE',  ( 71.83393739769628894, 11.38381105532070059, -68.85000000000408704 ) ) ;
#45473 = CARTESIAN_POINT ( 'NONE',  ( 47.53479508864854353, -54.39911497212986546, -74.95188530368821489 ) ) ;
#45474 = CARTESIAN_POINT ( 'NONE',  ( 48.88899477876550037, -53.95617853557810406, -54.86330888163660546 ) ) ;
#45475 = CARTESIAN_POINT ( 'NONE',  ( 78.22251691734010137, -33.11618894467940066, -20.65000000000000213 ) ) ;
#45476 = EDGE_CURVE ( 'NONE', #32837, #49018, #31962, .T. ) ;
#45477 = AXIS2_PLACEMENT_3D ( 'NONE', #42268, #9273, #17892 ) ;
#45478 = B_SPLINE_CURVE_WITH_KNOTS ( 'NONE', 3,
 ( #15178, #51595, #7580, #34561, #31646, #23524, #43730, #47667, #42711, #23265, #2872, #39795, #34820, #30878, #15691, #3130, #10993, #38780 ),
 .UNSPECIFIED., .F., .F.,
 ( 4, 2, 2, 2, 2, 2, 2, 2, 4 ),
 ( 0.000000000000000000, 0.06250001769099303162, 0.1250000353819860632, 0.1875000530729790948, 0.2500000707639721265, 0.3125000884549652413, 0.3750001061459584117, 0.4375001238369515266, 0.5000001415279446970 ),
 .UNSPECIFIED. ) ;
#45479 = PLANE ( 'NONE',  #41081 ) ;
#45480 = CARTESIAN_POINT ( 'NONE',  ( 18.86791100745899996, -51.78681560013630047, -74.34711752987139732 ) ) ;
#45481 = CARTESIAN_POINT ( 'NONE',  ( 18.13393739769619728, -45.61618894467940066, -49.33749999999999858 ) ) ;
#45482 = EDGE_CURVE ( 'NONE', #46160, #9287, #30013, .T. ) ;
#45483 = VERTEX_POINT ( 'NONE', #42092 ) ;
#45484 = CARTESIAN_POINT ( 'NONE',  ( 9.042753068858660370, -13.33106331294909985, -42.16657309509579932 ) ) ;
#45485 = CARTESIAN_POINT ( 'NONE',  ( 64.23238216415199986, 1.087300712305290018, -61.09829428330199619 ) ) ;
#45486 = VERTEX_POINT ( 'NONE', #22671 ) ;
#45487 = CARTESIAN_POINT ( 'NONE',  ( 9.366560669795820360, -15.61606439180730099, -33.84717978380999881 ) ) ;
#45488 = CARTESIAN_POINT ( 'NONE',  ( 60.30540951500689317, -45.82523471321780306, -47.61343627861160144 ) ) ;
#45489 = CARTESIAN_POINT ( 'NONE',  ( 28.13393739769619728, -8.687985714403851034, -47.64999999999999858 ) ) ;
#45490 = CARTESIAN_POINT ( 'NONE',  ( 42.93197233849409855, 11.32569894967160096, -3.187564294433600232 ) ) ;
#45492 = CARTESIAN_POINT ( 'NONE',  ( 1.014378609951400056, -15.61618894467929941, -6.721843382729280059 ) ) ;
#45491 = CARTESIAN_POINT ( 'NONE',  ( 43.25365395683799363, 8.657428456887169332, -70.27234317976126476 ) ) ;
#45493 = CARTESIAN_POINT ( 'NONE',  ( 51.98443728612009096, -51.36758245232200437, -75.98853294935470615 ) ) ;
#45494 = DIRECTION ( 'NONE',  ( 0.6676418852213039656, 0.2329255526947077437, 0.7071067811865533459 ) ) ;
#45495 = ORIENTED_EDGE ( 'NONE', *, *, #40875, .T. ) ;
#45496 = VERTEX_POINT ( 'NONE', #38691 ) ;
#45497 = VERTEX_POINT ( 'NONE', #2779 ) ;
#45498 = AXIS2_PLACEMENT_3D ( 'NONE', #16871, #28382, #28640 ) ;
#45499 = EDGE_LOOP ( 'NONE', ( #50925, #24318, #9922, #28922 ) ) ;
#45500 = CARTESIAN_POINT ( 'NONE',  ( 61.35985704537380059, -45.28492337451550043, -47.11846253721390099 ) ) ;
#45501 = CARTESIAN_POINT ( 'NONE',  ( 52.84261786122310411, -49.69241002008439523, -48.97154812789309375 ) ) ;
#45502 = LINE ( 'NONE', #33424, #39969 ) ;
#45503 = CONICAL_SURFACE ( 'NONE', #22878, 0.2705324999999987323, 1.029744258676660307 ) ;
#45504 = DIRECTION ( 'NONE',  ( 0.000000000000000000, 0.000000000000000000, 1.000000000000000000 ) ) ;
#45505 = VECTOR ( 'NONE', #3483, 1000.000000000000000 ) ;
#45506 = EDGE_LOOP ( 'NONE', ( #35702, #9205, #49843, #5486 ) ) ;
#45507 = VERTEX_POINT ( 'NONE', #13798 ) ;
#45508 = EDGE_CURVE ( 'NONE', #37534, #31864, #35882, .T. ) ;
#45509 = EDGE_LOOP ( 'NONE', ( #22713, #533, #35114, #23467 ) ) ;
#45510 = CARTESIAN_POINT ( 'NONE',  ( 24.04493738792232804, -15.61196413652903736, -77.50751794856931554 ) ) ;
#45511 = CARTESIAN_POINT ( 'NONE',  ( 52.56495426071009547, -52.43765526798460286, -54.45623365677440120 ) ) ;
#45512 = CARTESIAN_POINT ( 'NONE',  ( 58.92073396209919878, -3.116188944679349593, -18.64999999999999858 ) ) ;
#45513 = VERTEX_POINT ( 'NONE', #9863 ) ;
#45514 = DIRECTION ( 'NONE',  ( 0.6339889056055382222, 0.000000000000000000, -0.7733421413379021336 ) ) ;
#45515 = CARTESIAN_POINT ( 'NONE',  ( 52.36900553906810529, -50.72407173529079927, -76.35261119407400088 ) ) ;
#45516 = CARTESIAN_POINT ( 'NONE',  ( 60.56101234812630452, 14.37792091447689913, -47.14853648965690525 ) ) ;
#45517 = CARTESIAN_POINT ( 'NONE',  ( 8.724870845853098800, -13.02920606457709951, -59.11942434271038849 ) ) ;
#45518 = CARTESIAN_POINT ( 'NONE',  ( 68.13393739769618662, -30.31618894467939995, -49.64999999999999858 ) ) ;
#45519 = AXIS2_PLACEMENT_3D ( 'NONE', #9420, #20405, #49511 ) ;
#45520 = CARTESIAN_POINT ( 'NONE',  ( 41.46797725167870396, 13.65730434570830099, -5.587150232416230544 ) ) ;
#45521 = CARTESIAN_POINT ( 'NONE',  ( 43.83393256038859676, -43.46487882048660367, -5.056952191481060233 ) ) ;
#45522 = CARTESIAN_POINT ( 'NONE',  ( 68.13393739769840352, -50.61618894467879670, -73.25000000000220268 ) ) ;
#45523 = CARTESIAN_POINT ( 'NONE',  ( -7.973795448866470181, 13.91176078833520080, -5.720958296299230028 ) ) ;
#45524 = CARTESIAN_POINT ( 'NONE',  ( 63.77351956156250878, 1.056849143885769893, -69.77234944045780196 ) ) ;
#45525 = LINE ( 'NONE', #26098, #22614 ) ;
#45526 = B_SPLINE_CURVE_WITH_KNOTS ( 'NONE', 3,
 ( #29609, #32747, #13397, #36970, #33544, #45095, #48774, #1066, #17063, #25411, #1332, #49039, #9712, #29355 ),
 .UNSPECIFIED., .F., .F.,
 ( 4, 2, 2, 2, 2, 2, 4 ),
 ( 0.000000000000000000, 0.004139501987503274756, 0.1286220642390652202, 0.3277941638415642900, 0.6464695232055646112, 0.9209749313270280124, 1.000000000000000000 ),
 .UNSPECIFIED. ) ;
#45527 = CARTESIAN_POINT ( 'NONE',  ( 66.28213684734230071, 1.842697259673649945, -19.91087727140369878 ) ) ;
#45528 = ORIENTED_EDGE ( 'NONE', *, *, #39261, .T. ) ;
#45529 = CARTESIAN_POINT ( 'NONE',  ( 14.98839781681999916, -52.93030938277399855, -76.14999999999999147 ) ) ;
#45530 = CARTESIAN_POINT ( 'NONE',  ( 47.18324198357289845, -54.80726809202429450, -54.61058319554170026 ) ) ;
#45531 = CARTESIAN_POINT ( 'NONE',  ( 68.13393739844677555, -29.16618894467940137, -89.15000000000000568 ) ) ;
#45532 = AXIS2_PLACEMENT_3D ( 'NONE', #39798, #47669, #3904 ) ;
#45533 = CARTESIAN_POINT ( 'NONE',  ( 56.55522355860080097, -46.21195502513410247, -26.26695352263039851 ) ) ;
#45534 = CARTESIAN_POINT ( 'NONE',  ( 23.43719904012089827, -15.74375136141919995, -32.14999999999999858 ) ) ;
#45535 = CARTESIAN_POINT ( 'NONE',  ( 61.98540824044663111, -31.81618894467930403, -70.11716791742267674 ) ) ;
#45536 = CARTESIAN_POINT ( 'NONE',  ( 10.95445192191350081, 33.82498797628089449, -17.59525104008959673 ) ) ;
#45537 = CARTESIAN_POINT ( 'NONE',  ( 20.11808254608159174, -22.52870385452940383, -52.12566311908927474 ) ) ;
#45538 = EDGE_CURVE ( 'NONE', #31815, #3546, #17722, .T. ) ;
#45539 = CARTESIAN_POINT ( 'NONE',  ( 47.13393739769619373, -15.61618894467929941, -54.64999999999999858 ) ) ;
#45540 = CARTESIAN_POINT ( 'NONE',  ( 48.26248612645670022, 22.97322273838690165, -54.82342444101630008 ) ) ;
#45541 = ORIENTED_EDGE ( 'NONE', *, *, #46320, .F. ) ;
#45542 = CARTESIAN_POINT ( 'NONE',  ( 20.79454452025889921, -20.90970388501609989, -61.11739150984060132 ) ) ;
#45543 = ORIENTED_EDGE ( 'NONE', *, *, #40885, .T. ) ;
#45544 = CARTESIAN_POINT ( 'NONE',  ( 82.45630311851421368, 13.86034003618500066, -46.38988467804559690 ) ) ;
#45545 = CARTESIAN_POINT ( 'NONE',  ( 22.90122612410699077, -15.61618894223031440, -74.45282020639018583 ) ) ;
#45546 = CARTESIAN_POINT ( 'NONE',  ( 17.90524304069786510, -22.20704573693384987, -42.86948654708372430 ) ) ;
#45548 = CARTESIAN_POINT ( 'NONE',  ( 55.44576274181309827, 15.28165783319309945, -25.46131564888750276 ) ) ;
#45547 = CARTESIAN_POINT ( 'NONE',  ( 83.16755290732228900, 13.77093069207690057, -46.93255211562899376 ) ) ;
#45549 = CARTESIAN_POINT ( 'NONE',  ( 12.10516040838770024, -21.40510202634260040, -77.14635284413569138 ) ) ;
#45550 = CARTESIAN_POINT ( 'NONE',  ( 11.28671401888813719, 33.77463329229922806, -16.86100853830620849 ) ) ;
#45551 = CARTESIAN_POINT ( 'NONE',  ( 55.74013705948259911, -45.13221362293969463, -14.86594848831030014 ) ) ;
#45552 = DIRECTION ( 'NONE',  ( 0.000000000000000000, 0.7071067811865492381, -0.7071067811865457964 ) ) ;
#45553 = VECTOR ( 'NONE', #17155, 1000.000000000000000 ) ;
#45554 = VERTEX_POINT ( 'NONE', #50729 ) ;
#45555 = VERTEX_POINT ( 'NONE', #25817 ) ;
#45556 = CARTESIAN_POINT ( 'NONE',  ( 12.15898433498739983, -65.06882048843399957, -16.45263499446509670 ) ) ;
#45557 = CARTESIAN_POINT ( 'NONE',  ( 10.93504234667139841, 32.38329808718709302, -44.92331353542380157 ) ) ;
#45558 = CARTESIAN_POINT ( 'NONE',  ( 23.98529412776635183, -14.62549353487179182, -39.46773035656453743 ) ) ;
#45559 =( BOUNDED_CURVE ( )  B_SPLINE_CURVE ( 3, ( #22412, #29243, #37902, #29752 ),
 .UNSPECIFIED., .F., .T. ) 
 B_SPLINE_CURVE_WITH_KNOTS ( ( 4, 4 ),
 ( 0.000000000000000000, 0.7853981633974557175 ),
 .UNSPECIFIED. ) 
 CURVE ( )  GEOMETRIC_REPRESENTATION_ITEM ( )  RATIONAL_B_SPLINE_CURVE ( ( 1.000000000000000000, 0.9492530216741901228, 0.9492530216741901228, 1.000000000000000000 ) ) 
 REPRESENTATION_ITEM ( '' )  );
#45560 = CARTESIAN_POINT ( 'NONE',  ( 21.54529383757935435, -19.77481161222722861, -54.66115604025567620 ) ) ;
#45561 = CARTESIAN_POINT ( 'NONE',  ( 51.23436977250750601, 3.565853774335477233, -76.55134428789229162 ) ) ;
#45562 = ORIENTED_EDGE ( 'NONE', *, *, #34132, .F. ) ;
#45563 = EDGE_CURVE ( 'NONE', #36574, #2651, #35048, .T. ) ;
#45564 = CARTESIAN_POINT ( 'NONE',  ( -13.69310020793190041, -40.86924150905350217, -46.67353371693619835 ) ) ;
#45565 = CARTESIAN_POINT ( 'NONE',  ( 16.13393739667419879, -15.61618894434099936, -11.12000000014429979 ) ) ;
#45566 = CIRCLE ( 'NONE', #7892, 5.499999999999998224 ) ;
#45567 = CARTESIAN_POINT ( 'NONE',  ( 51.42675427039450398, 19.81429176188510155, -50.04217728894000317 ) ) ;
#45568 = EDGE_CURVE ( 'NONE', #50146, #37013, #38885, .T. ) ;
#45569 = CARTESIAN_POINT ( 'NONE',  ( 64.91976642084398463, -1.113755444385029936, -16.49433693280849766 ) ) ;
#45570 = CARTESIAN_POINT ( 'NONE',  ( 51.30983199192319688, -49.53152618182630107, -76.46178133275020627 ) ) ;
#45571 = CARTESIAN_POINT ( 'NONE',  ( 22.37218167695519710, -53.60956520270859471, -34.65000333313919612 ) ) ;
#45572 = ORIENTED_EDGE ( 'NONE', *, *, #8046, .T. ) ;
#45573 = CARTESIAN_POINT ( 'NONE',  ( 21.54530314169335625, -11.45757904198565491, -68.24448498028382915 ) ) ;
#45574 = CARTESIAN_POINT ( 'NONE',  ( 14.56242188612286448, -16.75796179725742974, -7.393828452885189861 ) ) ;
#45575 = ORIENTED_EDGE ( 'NONE', *, *, #26347, .T. ) ;
#45576 = CARTESIAN_POINT ( 'NONE',  ( 17.16946032303731329, -7.705185438491676919, -53.33399987908899220 ) ) ;
#45577 = CARTESIAN_POINT ( 'NONE',  ( 8.223251455316621161, -15.61600507739779786, -72.79233150823699816 ) ) ;
#45578 = CARTESIAN_POINT ( 'NONE',  ( 20.90719767621910208, -21.84537299277410227, -36.30437219638799462 ) ) ;
#45579 = CARTESIAN_POINT ( 'NONE',  ( 14.08262962865900114, -51.14923377493139611, -22.65114920387059883 ) ) ;
#45580 = CARTESIAN_POINT ( 'NONE',  ( 56.44450715656099504, 19.45673396471810079, -74.92602466682960483 ) ) ;
#45581 = VECTOR ( 'NONE', #40352, 1000.000000000000000 ) ;
#45582 = CARTESIAN_POINT ( 'NONE',  ( 47.53479509476479592, -54.39911496936699820, -74.95188530402140259 ) ) ;
#45583 = EDGE_LOOP ( 'NONE', ( #51376, #39922, #16743, #31459 ) ) ;
#45584 = CARTESIAN_POINT ( 'NONE',  ( 56.35090670788920164, 14.15977167711390017, -17.04118023804650051 ) ) ;
#45585 = CARTESIAN_POINT ( 'NONE',  ( 16.13393739769620083, -15.61618894467929941, -32.14999999999999858 ) ) ;
#45586 = CARTESIAN_POINT ( 'NONE',  ( 57.25486276105269923, -50.42116208795279420, -53.00955584233389573 ) ) ;
#45587 = DIRECTION ( 'NONE',  ( -1.000000000000000000, -3.191443934968489902E-12, -8.980656580310985401E-23 ) ) ;
#45588 = DIRECTION ( 'NONE',  ( 0.000000000000000000, -1.000000000000000000, 0.000000000000000000 ) ) ;
#45589 = AXIS2_PLACEMENT_3D ( 'NONE', #5177, #41066, #703 ) ;
#45590 = CARTESIAN_POINT ( 'NONE',  ( 47.43576539955360261, 23.40338254006309882, -74.19735651161070678 ) ) ;
#45591 = CARTESIAN_POINT ( 'NONE',  ( 65.01767771978660448, 0.9212109678634080590, -60.52272727272730179 ) ) ;
#45592 = CARTESIAN_POINT ( 'NONE',  ( 75.16209103024675642, -29.53953162302573787, -11.85643004527870481 ) ) ;
#45593 = CARTESIAN_POINT ( 'NONE',  ( 68.13393739769598767, -2.032350560840590070, -29.09832030244560741 ) ) ;
#45594 = CARTESIAN_POINT ( 'NONE',  ( -18.86606260230360022, -50.61618894467959962, 11.97999999999999865 ) ) ;
#45595 = CARTESIAN_POINT ( 'NONE',  ( 17.16575499510360103, -7.435842179093509863, -79.04760718966269906 ) ) ;
#45596 = FACE_OUTER_BOUND ( 'NONE', #40813, .T. ) ;
#45598 = CARTESIAN_POINT ( 'NONE',  ( 46.01742420967821801, -39.26550661771518236, -60.45755080081597299 ) ) ;
#45597 = CARTESIAN_POINT ( 'NONE',  ( 64.72741779930979078, 0.8986939045430368811, -60.71074964625670134 ) ) ;
#45599 = EDGE_CURVE ( 'NONE', #26915, #48851, #49563, .T. ) ;
#45600 = CARTESIAN_POINT ( 'NONE',  ( 61.06807839133419691, 14.11225480744460015, -46.83711763858070043 ) ) ;
#45601 = CARTESIAN_POINT ( 'NONE',  ( -12.15512026600820050, 24.36382048915779919, -51.32444474606599982 ) ) ;
#45602 = ORIENTED_EDGE ( 'NONE', *, *, #17509, .T. ) ;
#45603 = CARTESIAN_POINT ( 'NONE',  ( 52.87179757757409959, -49.64089313818260507, -48.76566979334150176 ) ) ;
#45604 = ORIENTED_EDGE ( 'NONE', *, *, #22249, .T. ) ;
#45605 = CARTESIAN_POINT ( 'NONE',  ( 60.62404192237740119, -45.11617399124450145, -26.47736735333209879 ) ) ;
#45606 = CARTESIAN_POINT ( 'NONE',  ( 24.00165179737271259, -16.46122918689899350, -65.82638113334461138 ) ) ;
#45607 = CARTESIAN_POINT ( 'NONE',  ( 57.55135366195850111, 13.89752427999699869, -25.54668255911809993 ) ) ;
#45608 = CARTESIAN_POINT ( 'NONE',  ( 23.12128521099250023, -14.65726807586429992, -46.40940759145149741 ) ) ;
#45609 = CARTESIAN_POINT ( 'NONE',  ( 50.36549662992300114, 18.84323467693539911, -76.14999999999999147 ) ) ;
#45610 = CARTESIAN_POINT ( 'NONE',  ( 53.05460983997079438, 18.33279354663559957, -48.99361253809119887 ) ) ;
#45611 = CARTESIAN_POINT ( 'NONE',  ( 47.13393739769620794, 4.077527749126597989, -54.64999999999996305 ) ) ;
#45612 = FACE_OUTER_BOUND ( 'NONE', #21455, .T. ) ;
#45613 = CARTESIAN_POINT ( 'NONE',  ( 63.87213755537349158, -43.73219550796380162, -10.18606854234780101 ) ) ;
#45614 = ORIENTED_EDGE ( 'NONE', *, *, #42779, .T. ) ;
#45615 = CARTESIAN_POINT ( 'NONE',  ( 9.420195413154878850, -12.38627208764589938, -70.21007469161709480 ) ) ;
#45616 = CARTESIAN_POINT ( 'NONE',  ( 72.94195630468689728, 1.327322800621349996, -68.80227784490020326 ) ) ;
#45617 = CARTESIAN_POINT ( 'NONE',  ( 47.44110378858790256, -54.62521372874980585, -54.71913897434770035 ) ) ;
#45618 = CARTESIAN_POINT ( 'NONE',  ( 8.363305339577767228, -13.92330431280884007, -48.86050672628254432 ) ) ;
#45619 = CARTESIAN_POINT ( 'NONE',  ( 73.03020225798630349, 1.267233196669050210, -62.48314610740069242 ) ) ;
#45620 = CARTESIAN_POINT ( 'NONE',  ( 11.77545672746500216, -65.42605939611310362, -17.95294975585129649 ) ) ;
#45621 = CARTESIAN_POINT ( 'NONE',  ( 71.40920805366010882, 1.325841671674429900, -60.89969828258869455 ) ) ;
#45622 = CARTESIAN_POINT ( 'NONE',  ( 24.03373631122487808, -16.07077874150862584, -75.81061925190356021 ) ) ;
#45623 = CARTESIAN_POINT ( 'NONE',  ( 12.14983763036492448, -8.703647864385146704, -45.12563104342815734 ) ) ;
#45624 = CYLINDRICAL_SURFACE ( 'NONE', #9260, 1.999999999999970246 ) ;
#45625 = CARTESIAN_POINT ( 'NONE',  ( 65.02936113742829605, 1.390208944942409985, -70.27002685503249779 ) ) ;
#45626 = ORIENTED_EDGE ( 'NONE', *, *, #22288, .F. ) ;
#45627 = VECTOR ( 'NONE', #26089, 1000.000000000000000 ) ;
#45628 = CARTESIAN_POINT ( 'NONE',  ( 8.812257860101720297, -63.26324333009419831, -46.67111697731629505 ) ) ;
#45629 = CARTESIAN_POINT ( 'NONE',  ( 82.13853704237929776, 14.40950277491920062, -47.72348187592560009 ) ) ;
#45630 = ORIENTED_EDGE ( 'NONE', *, *, #47568, .F. ) ;
#45631 = EDGE_CURVE ( 'NONE', #49388, #47619, #45869, .T. ) ;
#45632 = FACE_OUTER_BOUND ( 'NONE', #9345, .T. ) ;
#45633 = CARTESIAN_POINT ( 'NONE',  ( 23.83903273756216024, -13.54548894720846519, -59.42431809898250350 ) ) ;
#45634 = CARTESIAN_POINT ( 'NONE',  ( 17.16954247147122814, -23.52718072034940278, -69.96600351109410099 ) ) ;
#45635 = CARTESIAN_POINT ( 'NONE',  ( 51.20054136575519976, 19.52715359417319974, -76.16661699907028549 ) ) ;
#45636 = CIRCLE ( 'NONE', #15520, 10.00000000000000355 ) ;
#45637 = ORIENTED_EDGE ( 'NONE', *, *, #19580, .F. ) ;
#45638 = CARTESIAN_POINT ( 'NONE',  ( 8.133937397696209715, 31.88305279702909800, -43.74348518090240390 ) ) ;
#45639 = CYLINDRICAL_SURFACE ( 'NONE', #15947, 0.4999999999999967248 ) ;
#45640 = CARTESIAN_POINT ( 'NONE',  ( 24.03381980306747678, -15.16329903094799292, -43.77409963459896858 ) ) ;
#45641 = B_SPLINE_SURFACE_WITH_KNOTS ( 'NONE', 3, 3, ( 
 ( #4688, #36643, #40849, #29303, #38214, #34254 ),
 ( #30331, #45304, #22205, #30067, #33492, #25874 ),
 ( #21687, #46353, #5728, #5986, #5479, #33743 ),
 ( #46094, #21434, #37693, #50012, #21177, #49249 ),
 ( #45564, #29559, #25616, #37956, #2310, #33232 ),
 ( #18033, #1279, #33999, #13345, #9415, #1791 ),
 ( #37436, #2052, #14101, #41619, #10440, #17774 ),
 ( #41888, #10178, #26139, #1536, #37182, #6247 ),
 ( #9660, #13850, #49758, #50277, #42149, #26393 ),
 ( #5225, #18283, #29807, #21945, #45824, #41364 ),
 ( #17523, #9911, #14364, #17271, #25363, #49506 ),
 ( #13596, #42185, #34559, #6804, #34818, #38778 ),
 ( #46389, #21982, #9946, #46127, #30624, #30876 ),
 ( #6284, #50564, #22757, #50822, #2869, #50311 ),
 ( #37992, #25910, #46906, #38249, #10992, #18066 ),
 ( #14396, #34034, #41924, #6536, #26174, #10476 ),
 ( #1829, #50044, #49790, #17807, #13882, #14912 ),
 ( #2610, #26957, #14137, #46648, #2342, #18835 ),
 ( #30107, #10214, #14654, #34295, #42967, #7063 ),
 ( #23013, #18316, #33781, #30364, #26431, #42449 ) ),
 .UNSPECIFIED., .F., .F., .F.,
 ( 4, 2, 2, 2, 2, 2, 2, 2, 2, 4 ),
 ( 4, 1, 1, 4 ),
 ( -1.170155825275029926, -0.9733514710058079888, -0.5765163061072460238, -0.2263816566490509941, 0.000000000000000000, 0.1472167173675059948, 0.3827634651555170131, 0.7338073664531429285, 1.133511627823170054, 1.155436281008310084 ),
 ( -0.007901665929633120908, 0.3333333333333329818, 0.6666666666666670737, 1.002701522820989899 ),
 .UNSPECIFIED. ) ;
#45642 = CARTESIAN_POINT ( 'NONE',  ( 20.66633427577639992, -22.50386624515620326, -58.10707212942319444 ) ) ;
#45643 = CARTESIAN_POINT ( 'NONE',  ( 22.90071998467804804, -15.61618839864605057, -72.45282571548244732 ) ) ;
#45644 = AXIS2_PLACEMENT_3D ( 'NONE', #26826, #35730, #51713 ) ;
#45645 = CARTESIAN_POINT ( 'NONE',  ( 45.37135124562947652, -38.08537628155816890, -63.46287384018188504 ) ) ;
#45646 = B_SPLINE_CURVE_WITH_KNOTS ( 'NONE', 3,
 ( #1649, #50640, #25730, #42263, #6362, #18399, #10556, #34378, #1909, #17888, #33859, #38072 ),
 .UNSPECIFIED., .F., .F.,
 ( 4, 2, 2, 2, 2, 4 ),
 ( 0.000000000000000000, 0.2528991456834384088, 0.3793487185251589455, 0.4425735049460208237, 0.4741858981564516240, 0.5057982913668825908 ),
 .UNSPECIFIED. ) ;
#45647 = ORIENTED_EDGE ( 'NONE', *, *, #23985, .T. ) ;
#45648 = CARTESIAN_POINT ( 'NONE',  ( 62.09157612670949788, -43.11618894467930119, -65.34607522167520699 ) ) ;
#45649 = CARTESIAN_POINT ( 'NONE',  ( 18.85638145099070329, -8.681133632583570403, -39.85173020371099284 ) ) ;
#45650 = CARTESIAN_POINT ( 'NONE',  ( 52.57435367313230046, -49.85246693219060177, -48.51308846454130475 ) ) ;
#45651 = CARTESIAN_POINT ( 'NONE',  ( 9.062362672667880759, -14.30322387553499830, -32.14999999999999858 ) ) ;
#45652 = CARTESIAN_POINT ( 'NONE',  ( 14.35346408579549937, 19.90988454773659910, -74.52171359303420672 ) ) ;
#45653 = CARTESIAN_POINT ( 'NONE',  ( 15.09848876230330639, -7.705177000359721085, -51.25066365736460483 ) ) ;
#45654 = CARTESIAN_POINT ( 'NONE',  ( 45.28516362987719646, -45.38267274594659995, -8.309856332598471340 ) ) ;
#45655 = DIRECTION ( 'NONE',  ( 0.000000000000000000, 0.000000000000000000, -1.000000000000000000 ) ) ;
#45656 = CARTESIAN_POINT ( 'NONE',  ( 16.96908921244479984, -23.81894714880170127, -57.97537152673989880 ) ) ;
#45657 = ORIENTED_EDGE ( 'NONE', *, *, #21791, .F. ) ;
#45658 = CARTESIAN_POINT ( 'NONE',  ( 53.66151296940279991, -48.70894861344299898, -26.71281138883589890 ) ) ;
#45659 = CONICAL_SURFACE ( 'NONE', #36437, 0.7350000000000003197, 0.06981317007977388966 ) ;
#45660 = CARTESIAN_POINT ( 'NONE',  ( 14.50346589895649885, -50.97187126869069829, -21.59847332898880268 ) ) ;
#45662 = DIRECTION ( 'NONE',  ( 0.000000000000000000, 0.000000000000000000, 1.000000000000000000 ) ) ;
#45661 = CARTESIAN_POINT ( 'NONE',  ( 7.782855510348779760, 30.62954478035329942, -15.35487569384610040 ) ) ;
#45663 = EDGE_CURVE ( 'NONE', #34738, #48296, #23946, .T. ) ;
#45664 = CARTESIAN_POINT ( 'NONE',  ( 17.90512143763164588, -22.20708015056001372, -56.86943258823897196 ) ) ;
#45665 = CARTESIAN_POINT ( 'NONE',  ( 50.20812736443180313, 14.95961625580089915, -12.60693812980999873 ) ) ;
#45666 = VERTEX_POINT ( 'NONE', #42877 ) ;
#45667 = CARTESIAN_POINT ( 'NONE',  ( -8.360280049586719997, -44.70025899903389899, -5.480459871618819534 ) ) ;
#45668 = EDGE_CURVE ( 'NONE', #12820, #33893, #30125, .T. ) ;
#45669 = CARTESIAN_POINT ( 'NONE',  ( 47.57151154772099488, 23.30286101566669998, -54.67895741658460196 ) ) ;
#45670 = DIRECTION ( 'NONE',  ( -6.008901426489750921E-29, 1.000000000000000000, 1.065814103640290065E-14 ) ) ;
#45671 = CARTESIAN_POINT ( 'NONE',  ( 63.32918872797849019, 1.327097482837290121, -62.49054404195729973 ) ) ;
#45672 = CARTESIAN_POINT ( 'NONE',  ( 61.01745591375750877, 14.14199598592190021, -47.00094549329430293 ) ) ;
#45673 = CARTESIAN_POINT ( 'NONE',  ( 42.70036220023900597, 12.92082705698970102, -5.071714814876659538 ) ) ;
#45674 = EDGE_CURVE ( 'NONE', #26643, #38464, #35518, .T. ) ;
#45675 = FACE_OUTER_BOUND ( 'NONE', #15136, .T. ) ;
#45676 = CARTESIAN_POINT ( 'NONE',  ( 52.84340576260750311, 18.42139123722009941, -48.59551021507399327 ) ) ;
#45677 = CARTESIAN_POINT ( 'NONE',  ( -30.36606260230379917, -15.61618894467929941, 11.84999999999999964 ) ) ;
#45678 = VECTOR ( 'NONE', #26819, 1000.000000000000000 ) ;
#45679 = DIRECTION ( 'NONE',  ( -0.4640893551880601597, 0.8857883891771953788, 0.000000000000000000 ) ) ;
#45680 = CARTESIAN_POINT ( 'NONE',  ( 22.49007974669167709, -18.02578827406430406, -66.56823315451654821 ) ) ;
#45681 = CARTESIAN_POINT ( 'NONE',  ( 55.72751318460259995, 19.85814786334140081, -53.82427627174779872 ) ) ;
#45682 = CARTESIAN_POINT ( 'NONE',  ( 63.58805182154581104, 0.9952259095800459754, -69.56719234871339097 ) ) ;
#45683 = CARTESIAN_POINT ( 'NONE',  ( 11.93810467663310071, -65.43945453151620484, -17.87564855520800222 ) ) ;
#45684 = CARTESIAN_POINT ( 'NONE',  ( 22.90093739769620029, -15.61618894467913243, -28.45282021618999835 ) ) ;
#45685 = ORIENTED_EDGE ( 'NONE', *, *, #44781, .F. ) ;
#45686 = CARTESIAN_POINT ( 'NONE',  ( 19.82948959376360776, 23.31066016154319698, -17.79040102455563854 ) ) ;
#45687 = CARTESIAN_POINT ( 'NONE',  ( 10.97995777053410116, 32.18935651174339796, -44.74773172946899535 ) ) ;
#45688 = CARTESIAN_POINT ( 'NONE',  ( 72.96189588675559889, 1.134960180547819997, -62.16566220516190100 ) ) ;
#45689 = EDGE_CURVE ( 'NONE', #11008, #367, #19270, .T. ) ;
#45690 = CARTESIAN_POINT ( 'NONE',  ( 66.23673192723569514, -31.73979966234530181, -17.49602702209859828 ) ) ;
#45691 = CIRCLE ( 'NONE', #23070, 12.00000000000000000 ) ;
#45692 = CARTESIAN_POINT ( 'NONE',  ( 17.99229889273830096, 19.88380863237500051, -74.14994161014911356 ) ) ;
#45693 = ORIENTED_EDGE ( 'NONE', *, *, #48099, .F. ) ;
#45694 = ORIENTED_EDGE ( 'NONE', *, *, #49415, .T. ) ;
#45695 = CARTESIAN_POINT ( 'NONE',  ( 9.205734167420720482, -3.616188944679329609, -24.15000000000000213 ) ) ;
#45696 = ORIENTED_EDGE ( 'NONE', *, *, #11613, .F. ) ;
#45697 = EDGE_CURVE ( 'NONE', #46482, #19317, #47836, .T. ) ;
#45698 = CARTESIAN_POINT ( 'NONE',  ( 11.67609344190909937, -65.14710708552239282, -46.80893820645799508 ) ) ;
#45699 = CARTESIAN_POINT ( 'NONE',  ( 56.61876495832499501, -45.69764771475809795, -26.04439677746109894 ) ) ;
#45700 = CARTESIAN_POINT ( 'NONE',  ( 12.72592204613637179, -21.52908688870203235, -45.11950636888933985 ) ) ;
#45701 = CARTESIAN_POINT ( 'NONE',  ( 41.13393739769620794, -15.61618894467929941, 4.450000000000000178 ) ) ;
#45702 = ORIENTED_EDGE ( 'NONE', *, *, #50717, .T. ) ;
#45703 = CARTESIAN_POINT ( 'NONE',  ( 46.24009931898407189, 6.945389266097389935, -59.11915260907306191 ) ) ;
#45704 = AXIS2_PLACEMENT_3D ( 'NONE', #14021, #2228, #29980 ) ;
#45705 = EDGE_LOOP ( 'NONE', ( #39699, #2508, #949, #24954 ) ) ;
#45706 = CARTESIAN_POINT ( 'NONE',  ( 52.22793003137540069, -45.20715030507830079, -12.77863615568089983 ) ) ;
#45707 = CIRCLE ( 'NONE', #33107, 6.000000000000000000 ) ;
#45708 = DIRECTION ( 'NONE',  ( 0.000000000000000000, 0.000000000000000000, 1.000000000000000000 ) ) ;
#45709 = CARTESIAN_POINT ( 'NONE',  ( 16.58032161481230204, 19.88381278803589680, -20.45514663783420062 ) ) ;
#45710 = LINE ( 'NONE', #5624, #41042 ) ;
#45711 = ORIENTED_EDGE ( 'NONE', *, *, #23928, .F. ) ;
#45712 = CARTESIAN_POINT ( 'NONE',  ( 73.10855093309899644, 0.8936201581567910779, -69.00461532610479765 ) ) ;
#45713 = CARTESIAN_POINT ( 'NONE',  ( 46.97135903472899798, -54.28212950231179690, -75.52157719890121257 ) ) ;
#45714 = CARTESIAN_POINT ( 'NONE',  ( 66.89072473720391088, 12.48801267837889917, -11.01669209824130036 ) ) ;
#45715 = EDGE_CURVE ( 'NONE', #9983, #7868, #7749, .T. ) ;
#45716 = CIRCLE ( 'NONE', #49087, 5.251829701412240148 ) ;
#45717 = CARTESIAN_POINT ( 'NONE',  ( 54.44698107792579833, 13.88381105532070059, -13.49511294515519921 ) ) ;
#45718 = CARTESIAN_POINT ( 'NONE',  ( -0.007164427059776000244, -45.70803162167019451, -34.77269723891829756 ) ) ;
#45720 = AXIS2_PLACEMENT_3D ( 'NONE', #14127, #33771, #46635 ) ;
#45719 = CARTESIAN_POINT ( 'NONE',  ( 51.26685560572850164, 19.79157626071939902, -76.14349090804589082 ) ) ;
#45721 = CARTESIAN_POINT ( 'NONE',  ( 60.27114510410760317, 14.00925828241220117, -26.79014729864100275 ) ) ;
#45722 = CARTESIAN_POINT ( 'NONE',  ( 9.297346275370859559, -11.76290852284069999, -76.45087635510310520 ) ) ;
#45723 = ORIENTED_EDGE ( 'NONE', *, *, #27539, .T. ) ;
#45724 = VECTOR ( 'NONE', #1450, 1000.000000000000000 ) ;
#45725 = CARTESIAN_POINT ( 'NONE',  ( 57.55751162087899786, 18.85811933572220056, -52.57651812407429759 ) ) ;
#45726 = FACE_OUTER_BOUND ( 'NONE', #7324, .T. ) ;
#45727 = CARTESIAN_POINT ( 'NONE',  ( 28.18536260820836858, -22.57408253408722132, -34.89146800830129536 ) ) ;
#45728 = DIRECTION ( 'NONE',  ( -0.5897727341282554825, -0.3900873262218120252, 0.7071067811865473507 ) ) ;
#45729 = EDGE_CURVE ( 'NONE', #2348, #44367, #26870, .T. ) ;
#45730 = FACE_OUTER_BOUND ( 'NONE', #45705, .T. ) ;
#45731 = VECTOR ( 'NONE', #1125, 1000.000000000000000 ) ;
#45732 = CARTESIAN_POINT ( 'NONE',  ( 72.33393739769486785, 11.38381105531920845, -68.85000000000410125 ) ) ;
#45733 = CARTESIAN_POINT ( 'NONE',  ( 12.57902832706879970, 19.10565774180280130, -21.19240428151960032 ) ) ;
#45734 = EDGE_CURVE ( 'NONE', #44367, #43625, #51508, .T. ) ;
#45735 = CARTESIAN_POINT ( 'NONE',  ( 64.93393739769619799, 1.396834109478129804, -70.23662692463440749 ) ) ;
#45736 = CARTESIAN_POINT ( 'NONE',  ( 56.39270785951039500, 19.29512406318060158, -52.86271188469099513 ) ) ;
#45737 = AXIS2_PLACEMENT_3D ( 'NONE', #29439, #9546, #5614 ) ;
#45738 = CARTESIAN_POINT ( 'NONE',  ( 20.11801211374420006, -22.52874597533168100, -56.12568250423961302 ) ) ;
#45739 = CARTESIAN_POINT ( 'NONE',  ( 75.76193235035715645, -43.34893572151489849, -13.50695346075995573 ) ) ;
#45740 = CARTESIAN_POINT ( 'NONE',  ( 17.91323993525340086, -51.14554741935710069, -74.54427505469620030 ) ) ;
#45741 = DIRECTION ( 'NONE',  ( -1.000000000000000000, 0.000000000000000000, 0.000000000000000000 ) ) ;
#45742 = B_SPLINE_CURVE_WITH_KNOTS ( 'NONE', 3,
 ( #33334, #5832, #1116, #1637, #25717, #13699, #13195, #17112, #45928, #49349 ),
 .UNSPECIFIED., .F., .F.,
 ( 4, 1, 1, 1, 1, 1, 1, 4 ),
 ( 0.000000000000000000, 0.07136600257796542335, 0.1505849336415300554, 0.2298038647052530192, 0.3090227957688131410, 0.3882417268325360493, 0.4674606578961007508, 0.5000020751347326042 ),
 .UNSPECIFIED. ) ;
#45743 = EDGE_LOOP ( 'NONE', ( #32927, #15936, #27821, #24124, #15958, #26404, #21988, #15192, #38621, #34456, #12751, #20885, #22791, #2619 ) ) ;
#45744 = CARTESIAN_POINT ( 'NONE',  ( 23.54789985460810087, -16.35093721847229986, -53.09878558187529052 ) ) ;
#45745 = CARTESIAN_POINT ( 'NONE',  ( 64.43604309779919959, 0.9828917932950889114, -60.92414392080449659 ) ) ;
#45746 = EDGE_LOOP ( 'NONE', ( #5826, #46744, #7071, #44514 ) ) ;
#45747 = FACE_OUTER_BOUND ( 'NONE', #32426, .T. ) ;
#45748 = CARTESIAN_POINT ( 'NONE',  ( 60.40987110273919569, -45.83497225692880050, -47.72180312432629989 ) ) ;
#45749 = CARTESIAN_POINT ( 'NONE',  ( 11.34022645397350004, -10.44290231406579927, -74.10929620427420161 ) ) ;
#45750 = CARTESIAN_POINT ( 'NONE',  ( 12.14971913517640090, -22.52866241416458948, -62.17430703707206874 ) ) ;
#45752 = CYLINDRICAL_SURFACE ( 'NONE', #27323, 6.766999999999998572 ) ;
#45751 = CARTESIAN_POINT ( 'NONE',  ( 43.58840487354246562, 8.687362816293918044, -68.65277826447533016 ) ) ;
#45753 = CARTESIAN_POINT ( 'NONE',  ( 52.20740540343859237, -51.40483972235690402, -75.93239679552310406 ) ) ;
#45754 = CARTESIAN_POINT ( 'NONE',  ( 40.71243489632720269, -45.33518156949239852, -5.692226379959530291 ) ) ;
#45755 = ORIENTED_EDGE ( 'NONE', *, *, #47406, .F. ) ;
#45756 = ORIENTED_EDGE ( 'NONE', *, *, #19681, .F. ) ;
#45757 = ORIENTED_EDGE ( 'NONE', *, *, #23122, .T. ) ;
#45758 = CIRCLE ( 'NONE', #34853, 2.576499999999998902 ) ;
#45759 = ORIENTED_EDGE ( 'NONE', *, *, #33093, .F. ) ;
#45760 = CARTESIAN_POINT ( 'NONE',  ( 61.19893174391710033, -45.31225206941749661, -47.06093154577280302 ) ) ;
#45761 = CARTESIAN_POINT ( 'NONE',  ( 53.23936142806359584, -49.53019510929430425, -49.17934721267350540 ) ) ;
#45762 = CARTESIAN_POINT ( 'NONE',  ( 47.13393739769619373, 4.883811055320659733, -54.64999999999999858 ) ) ;
#45763 = DIRECTION ( 'NONE',  ( -0.3535533905932738974, 0.6123724356957941373, 0.7071067811865477948 ) ) ;
#45764 = CIRCLE ( 'NONE', #18141, 0.4999999999999987232 ) ;
#45765 = VERTEX_POINT ( 'NONE', #27132 ) ;
#45766 = VERTEX_POINT ( 'NONE', #39197 ) ;
#45767 = CARTESIAN_POINT ( 'NONE',  ( 24.04341712964290423, -15.44869698543556780, -77.50093736165744929 ) ) ;
#45768 = CARTESIAN_POINT ( 'NONE',  ( 53.42313316096070253, -52.07210377827539816, -54.29429654136570349 ) ) ;
#45769 = DIRECTION ( 'NONE',  ( 0.000000000000000000, 0.000000000000000000, -1.000000000000000000 ) ) ;
#45770 = VERTEX_POINT ( 'NONE', #35256 ) ;
#45771 = CARTESIAN_POINT ( 'NONE',  ( 38.67452568954060155, 6.328436186825659782, -81.65000000000000568 ) ) ;
#45772 = CARTESIAN_POINT ( 'NONE',  ( 52.02214954632180621, -50.31644395759909827, -76.54113481940019881 ) ) ;
#45773 = CARTESIAN_POINT ( 'NONE',  ( 60.54707010150900715, 14.38522564811469984, -47.15409972330730426 ) ) ;
#45774 = TOROIDAL_SURFACE ( 'NONE', #8970, 10.49999999968949815, 0.4999999999856510335 ) ;
#45775 = EDGE_CURVE ( 'NONE', #14121, #4949, #45186, .T. ) ;
#45776 = CARTESIAN_POINT ( 'NONE',  ( 23.85371357567289863, -17.02750157961389732, -60.07005151547379995 ) ) ;
#45777 = EDGE_CURVE ( 'NONE', #22647, #14356, #709, .T. ) ;
#45778 = DIRECTION ( 'NONE',  ( 0.8660254037844387076, 0.4999999999999998890, 0.000000000000000000 ) ) ;
#45779 = CARTESIAN_POINT ( 'NONE',  ( 41.47580373046699975, 13.55635338172790050, -5.433826806151940580 ) ) ;
#45780 = CARTESIAN_POINT ( 'NONE',  ( 41.94994391203700701, -43.92468623023520280, -4.524181474801060254 ) ) ;
#45781 = EDGE_CURVE ( 'NONE', #31736, #40328, #34486, .T. ) ;
#45782 = LINE ( 'NONE', #25825, #32030 ) ;
#45783 = CARTESIAN_POINT ( 'NONE',  ( -6.178851728588689696, 15.46435443030710033, -5.588668033364348808 ) ) ;
#45784 = CARTESIAN_POINT ( 'NONE',  ( 64.00162532095220058, 1.348264980582170036, -69.84906706027560119 ) ) ;
#45785 = DIRECTION ( 'NONE',  ( -0.2260571801428189198, 0.000000000000000000, 0.9741140340359936145 ) ) ;
#45786 = CARTESIAN_POINT ( 'NONE',  ( 66.32948755469080027, 1.142895182770250040, -18.17795024893420219 ) ) ;
#45787 = ORIENTED_EDGE ( 'NONE', *, *, #2799, .F. ) ;
#45788 = CARTESIAN_POINT ( 'NONE',  ( 14.75663690171680109, -52.86216653946310373, -76.12493046668770091 ) ) ;
#45789 = AXIS2_PLACEMENT_3D ( 'NONE', #9103, #708, #45003 ) ;
#45790 = CARTESIAN_POINT ( 'NONE',  ( 47.18324198357289845, -54.80726809202429450, -54.61058319554170026 ) ) ;
#45791 = CARTESIAN_POINT ( 'NONE',  ( 46.26898798325825624, -40.10830698849575526, -55.65325670449188777 ) ) ;
#45792 = DIRECTION ( 'NONE',  ( 1.000000000000000000, 0.000000000000000000, 0.000000000000000000 ) ) ;
#45793 = B_SPLINE_CURVE_WITH_KNOTS ( 'NONE', 3,
 ( #19155, #51650, #31444, #47723, #43535, #7123, #35397, #7633, #35665, #39597 ),
 .UNSPECIFIED., .F., .F.,
 ( 4, 2, 2, 2, 4 ),
 ( -0.0003767167460152949792, 0.000000000000000000, 0.01529901560004469883, 0.03030530679046750109, 0.04513248637254871354 ),
 .UNSPECIFIED. ) ;
#45794 = CARTESIAN_POINT ( 'NONE',  ( 16.13393739769620083, -15.61618894467929941, -84.65000000000000568 ) ) ;
#45795 = EDGE_CURVE ( 'NONE', #44136, #18843, #22477, .T. ) ;
#45796 = CARTESIAN_POINT ( 'NONE',  ( 63.21464875163319874, 1.097545367735389910, -69.01875481685129898 ) ) ;
#45797 = CARTESIAN_POINT ( 'NONE',  ( 47.80730873599560482, -54.40538902786819619, -54.73352113645039907 ) ) ;
#45798 = CARTESIAN_POINT ( 'NONE',  ( 12.69742525567431635, -9.457216345889188247, -50.18517902307924317 ) ) ;
#45799 = FACE_OUTER_BOUND ( 'NONE', #7216, .T. ) ;
#45800 = CARTESIAN_POINT ( 'NONE',  ( 48.01952589465019372, 23.10709900649499815, -54.91785799752790354 ) ) ;
#45801 = VERTEX_POINT ( 'NONE', #8773 ) ;
#45802 = CARTESIAN_POINT ( 'NONE',  ( 13.36620148929459972, -22.10326818851440223, -73.47554475576528432 ) ) ;
#45803 = ORIENTED_EDGE ( 'NONE', *, *, #47030, .F. ) ;
#45804 = PRODUCT_DEFINITION_SHAPE ( 'NONE', 'NONE',  #15826 ) ;
#45805 = LINE ( 'NONE', #34504, #44667 ) ;
#45806 = VECTOR ( 'NONE', #32, 1000.000000000000000 ) ;
#45807 = LINE ( 'NONE', #37938, #11841 ) ;
#45808 = CARTESIAN_POINT ( 'NONE',  ( 11.97538130472928408, -21.02759617003068726, -43.16115338163687198 ) ) ;
#45810 = CARTESIAN_POINT ( 'NONE',  ( 42.93197233849399908, -42.55807683903039162, -3.187564294433600232 ) ) ;
#45809 = CARTESIAN_POINT ( 'NONE',  ( 84.44066163939218939, 12.08519577684469937, -47.44491107334449964 ) ) ;
#45811 = CARTESIAN_POINT ( 'NONE',  ( 9.084867081448990689, -15.38561059954679955, -77.46322856839019266 ) ) ;
#45812 = FACE_OUTER_BOUND ( 'NONE', #44453, .T. ) ;
#45813 = CARTESIAN_POINT ( 'NONE',  ( 56.21747353221379484, -45.13074185381659476, -15.33522795547970041 ) ) ;
#45814 = LINE ( 'NONE', #18536, #28608 ) ;
#45815 = CARTESIAN_POINT ( 'NONE',  ( 56.61928439928508539, 14.09173447728649720, -17.93019253464870033 ) ) ;
#45816 = EDGE_LOOP ( 'NONE', ( #10906, #51303 ) ) ;
#45817 = ORIENTED_EDGE ( 'NONE', *, *, #51125, .T. ) ;
#45818 = CARTESIAN_POINT ( 'NONE',  ( 12.36320305068320025, -64.54682834576858852, -15.76422791927960176 ) ) ;
#45819 = CARTESIAN_POINT ( 'NONE',  ( 12.21269279732720037, 34.11710210141869482, -47.01935258852740418 ) ) ;
#45820 = CARTESIAN_POINT ( 'NONE',  ( 16.13393739769620083, -15.61618894467929941, -9.392532499999980189 ) ) ;
#45821 = FACE_OUTER_BOUND ( 'NONE', #21778, .T. ) ;
#45822 = CARTESIAN_POINT ( 'NONE',  ( 51.13862808468330456, 3.739953746215777475, -76.48488464726803215 ) ) ;
#45823 = ORIENTED_EDGE ( 'NONE', *, *, #47575, .T. ) ;
#45824 = CARTESIAN_POINT ( 'NONE',  ( -22.86617264519300008, -13.70436038122300104, -54.83108237264280405 ) ) ;
#45825 = DIRECTION ( 'NONE',  ( 0.000000000000000000, 0.000000000000000000, 1.000000000000000000 ) ) ;
#45826 = CARTESIAN_POINT ( 'NONE',  ( 52.59914051912740263, -49.82906292203490040, -48.56924359530199808 ) ) ;
#45827 = CARTESIAN_POINT ( 'NONE',  ( 49.83651295974559758, 21.41060930851670108, -52.45077174872059800 ) ) ;
#45828 = CARTESIAN_POINT ( 'NONE',  ( 59.39915200420649910, -2.757920925504779852, -15.68862214463160143 ) ) ;
#45829 = CARTESIAN_POINT ( 'NONE',  ( 50.81500904190379941, -49.69956259698449941, -76.22412500851820027 ) ) ;
#45830 = CARTESIAN_POINT ( 'NONE',  ( 60.41046171663749931, -46.68362944077280474, -48.85993508664739693 ) ) ;
#45831 = ORIENTED_EDGE ( 'NONE', *, *, #14445, .F. ) ;
#45832 = CARTESIAN_POINT ( 'NONE',  ( 23.53669455186071602, -48.92556967366427756, -34.79644561402096770 ) ) ;
#45833 = CARTESIAN_POINT ( 'NONE',  ( 68.13393739769769297, 18.72622661238600017, -69.60146707679309941 ) ) ;
#45834 = ORIENTED_EDGE ( 'NONE', *, *, #33711, .T. ) ;
#45835 = DIRECTION ( 'NONE',  ( 0.000000000000000000, 0.000000000000000000, -1.000000000000000000 ) ) ;
#45836 = DIRECTION ( 'NONE',  ( 1.000000000000000000, 0.000000000000000000, 0.000000000000000000 ) ) ;
#45837 = CARTESIAN_POINT ( 'NONE',  ( 8.972021738993211315, -18.82457042039120054, -34.87843143724279571 ) ) ;
#45838 = ADVANCED_FACE ( 'NONE', ( #36535 ), #904, .F. ) ;
#45839 = CARTESIAN_POINT ( 'NONE',  ( 13.29213509620739941, -50.86275351173860315, -21.61097465929019990 ) ) ;
#45840 = CARTESIAN_POINT ( 'NONE',  ( 53.92402291300970063, 19.73846352820710237, -75.87933617372019057 ) ) ;
#45841 = B_SPLINE_CURVE_WITH_KNOTS ( 'NONE', 3,
 ( #3367, #23501, #35324, #47904, #12005, #14893, #34801, #51323, #15674, #27960 ),
 .UNSPECIFIED., .F., .F.,
 ( 4, 1, 1, 1, 1, 1, 1, 4 ),
 ( 0.000000000000000000, 0.06104662216038692080, 0.1402655532241073311, 0.2194844842876716440, 0.2987034153513898338, 0.3779223464149541467, 0.4571412774786768329, 0.4999989579104466841 ),
 .UNSPECIFIED. ) ;
#45842 = CARTESIAN_POINT ( 'NONE',  ( 47.29285256804840287, -54.09193043622850183, -75.52284329973289800 ) ) ;
#45843 = ORIENTED_EDGE ( 'NONE', *, *, #13844, .T. ) ;
#45844 = EDGE_CURVE ( 'NONE', #47621, #46679, #25252, .T. ) ;
#45845 = CARTESIAN_POINT ( 'NONE',  ( 55.87349882819940206, 14.34368325183129933, -16.58361811465810121 ) ) ;
#45846 = CYLINDRICAL_SURFACE ( 'NONE', #26497, 7.910999999999997812 ) ;
#45847 = B_SPLINE_CURVE_WITH_KNOTS ( 'NONE', 3,
 ( #47256, #6378, #22339, #15274, #31229, #18418, #34393, #20212, #51687, #12631, #24647, #28589, #35945, #44589, #4495, #3993 ),
 .UNSPECIFIED., .F., .F.,
 ( 4, 2, 2, 2, 2, 2, 2, 4 ),
 ( 0.2986826963453430017, 0.6144977923521359742, 0.8991761887526290575, 1.077100186502939927, 1.188302685096880085, 1.410707682284769948, 1.766555677785379919, 1.779239977503060066 ),
 .UNSPECIFIED. ) ;
#45848 = CARTESIAN_POINT ( 'NONE',  ( 57.32592487833510120, -50.41428338388260499, -53.00067887287889334 ) ) ;
#45849 = CARTESIAN_POINT ( 'NONE',  ( 52.88344664573250498, -49.67337909505339866, -49.00461641361030019 ) ) ;
#45850 = PRESENTATION_LAYER_ASSIGNMENT (  '', '', ( #13240 ) ) ;
#45851 = DIRECTION ( 'NONE',  ( 3.191891195582396227E-12, -1.000000000000000000, 0.000000000000000000 ) ) ;
#45852 = CARTESIAN_POINT ( 'NONE',  ( 9.366359996283680545, -15.61618532483699973, -43.84717978381009118 ) ) ;
#45853 = CARTESIAN_POINT ( 'NONE',  ( 46.40528337222430366, 21.74482207379540100, -76.14872548090239945 ) ) ;
#45854 = VECTOR ( 'NONE', #38863, 1000.000000000000000 ) ;
#45855 = CARTESIAN_POINT ( 'NONE',  ( 19.98170351883816309, -54.97933364285017888, -18.57148459735737234 ) ) ;
#45856 = CARTESIAN_POINT ( 'NONE',  ( 75.15070962298389645, -28.81814377174942621, -11.80138244787392665 ) ) ;
#45857 = CARTESIAN_POINT ( 'NONE',  ( 105.5832649133809724, -15.41618894467840484, -65.65000000000004832 ) ) ;
#45858 = DIRECTION ( 'NONE',  ( 0.8660254037843907460, 0.5000000000000829337, 0.000000000000000000 ) ) ;
#45859 = CARTESIAN_POINT ( 'NONE',  ( 14.16187783161290170, -50.35113599914600258, -20.85710678118659800 ) ) ;
#45860 = EDGE_CURVE ( 'NONE', #38938, #15849, #33112, .T. ) ;
#45861 = DIRECTION ( 'NONE',  ( 0.000000000000000000, 8.635067969306036542E-13, 1.000000000000000000 ) ) ;
#45862 = LINE ( 'NONE', #2088, #14262 ) ;
#45864 = CARTESIAN_POINT ( 'NONE',  ( 41.44407966280440547, -37.52288105733000378, -83.09921727618568355 ) ) ;
#45863 = DIRECTION ( 'NONE',  ( 0.000000000000000000, 1.000000000000000000, 0.000000000000000000 ) ) ;
#45865 = EDGE_CURVE ( 'NONE', #14168, #46682, #41255, .T. ) ;
#45866 = CARTESIAN_POINT ( 'NONE',  ( 61.23360558058650582, 14.02553047523030116, -46.60520175737810433 ) ) ;
#45867 = CARTESIAN_POINT ( 'NONE',  ( -25.59424942068570275, 9.591493339629250769, -54.31183179444199993 ) ) ;
#45868 = ORIENTED_EDGE ( 'NONE', *, *, #16974, .F. ) ;
#45869 =( BOUNDED_CURVE ( )  B_SPLINE_CURVE ( 3, ( #31562, #39460, #30792, #47076 ),
 .UNSPECIFIED., .F., .T. ) 
 B_SPLINE_CURVE_WITH_KNOTS ( ( 4, 4 ),
 ( 0.000000000000000000, 0.9725514443758180860 ),
 .UNSPECIFIED. ) 
 CURVE ( )  GEOMETRIC_REPRESENTATION_ITEM ( )  RATIONAL_B_SPLINE_CURVE ( ( 1.000000000000000000, 0.9227196513546164214, 0.9227196513546164214, 1.000000000000000000 ) ) 
 REPRESENTATION_ITEM ( '' )  );
#45870 = CARTESIAN_POINT ( 'NONE',  ( 52.87376179874240734, -49.63822605030750168, -48.72414007904549749 ) ) ;
#45871 = ORIENTED_EDGE ( 'NONE', *, *, #35076, .T. ) ;
#45872 = CARTESIAN_POINT ( 'NONE',  ( -11.32734370190460105, -41.88171845330919751, -19.14999999999999858 ) ) ;
#45873 = CARTESIAN_POINT ( 'NONE',  ( -0.03447620312153643757, -27.09132598751343579, -34.79644660940672907 ) ) ;
#45874 = CARTESIAN_POINT ( 'NONE',  ( 20.38275687770182643, -41.70313699072102054, -59.64999999999999147 ) ) ;
#45875 = CARTESIAN_POINT ( 'NONE',  ( 14.15904947058580099, -22.38688878826850015, -47.04315903996049286 ) ) ;
#45876 = CARTESIAN_POINT ( 'NONE',  ( -1.566062602303800677, -15.61618894467939889, -6.649999999999999467 ) ) ;
#45877 = CARTESIAN_POINT ( 'NONE',  ( 52.68398807097789671, 18.52347269652620199, -48.59016489651170190 ) ) ;
#45878 = CARTESIAN_POINT ( 'NONE',  ( 46.63833728752520358, -15.61618894467929586, 7.349999999999999645 ) ) ;
#45879 = CARTESIAN_POINT ( 'NONE',  ( 60.51913464264409726, -45.63223970707090160, -47.16508087703120111 ) ) ;
#45880 = CARTESIAN_POINT ( 'NONE',  ( 38.67452568954060155, 4.883811055320659733, -81.65000000000000568 ) ) ;
#45881 = EDGE_LOOP ( 'NONE', ( #51685, #2642, #49683, #41539 ) ) ;
#45882 = CARTESIAN_POINT ( 'NONE',  ( 9.771079295578939394, -19.49184774166629808, -69.89319896736259352 ) ) ;
#45883 = DIRECTION ( 'NONE',  ( 0.000000000000000000, 0.000000000000000000, 1.000000000000000000 ) ) ;
#45884 = DIRECTION ( 'NONE',  ( -1.000000000000000000, 0.000000000000000000, 0.000000000000000000 ) ) ;
#45885 = CARTESIAN_POINT ( 'NONE',  ( 72.97487308438059017, 1.330484379554840002, -62.57139521546629624 ) ) ;
#45886 = CARTESIAN_POINT ( 'NONE',  ( 11.89339496835929921, -65.43604241733970639, -18.15362147994479614 ) ) ;
#45887 = CARTESIAN_POINT ( 'NONE',  ( 52.84340576260759548, 18.42139123722009941, -48.59551021507390089 ) ) ;
#45888 = CARTESIAN_POINT ( 'NONE',  ( 65.03603135424580728, -15.61618894467929941, -19.52361391316370032 ) ) ;
#45889 = CARTESIAN_POINT ( 'NONE',  ( 71.29497000743199919, 0.8840451408750739093, -60.55014093144440324 ) ) ;
#45890 = VECTOR ( 'NONE', #25042, 1000.000000000000000 ) ;
#45891 = CARTESIAN_POINT ( 'NONE',  ( 17.01981038939924318, -8.849199620768295915, -57.99448672953406003 ) ) ;
#45892 = CARTESIAN_POINT ( 'NONE',  ( 65.03036676789579928, 1.369613126987639928, -70.37582656035600337 ) ) ;
#45893 = ORIENTED_EDGE ( 'NONE', *, *, #50562, .F. ) ;
#45894 = CARTESIAN_POINT ( 'NONE',  ( 8.808591387964359143, -63.24239172143919774, -46.67055361988870033 ) ) ;
#45895 = CARTESIAN_POINT ( 'NONE',  ( 22.52085816870240009, -13.23982764291192815, -32.33926356356143827 ) ) ;
#45896 = VERTEX_POINT ( 'NONE', #20540 ) ;
#45897 = DIRECTION ( 'NONE',  ( 0.000000000000000000, 0.000000000000000000, 1.000000000000000000 ) ) ;
#45898 = CARTESIAN_POINT ( 'NONE',  ( 22.46008303819101215, -10.75448409851621001, -59.29930691482108074 ) ) ;
#45899 = CARTESIAN_POINT ( 'NONE',  ( 71.83393739769618946, 10.88381105532070059, -67.25000000000000000 ) ) ;
#45900 = CARTESIAN_POINT ( 'NONE',  ( 52.80343914517980153, 19.25517939188599570, -76.73469608800270692 ) ) ;
#45901 = VERTEX_POINT ( 'NONE', #12188 ) ;
#45902 = DIRECTION ( 'NONE',  ( 1.000000000000000000, 0.000000000000000000, 0.000000000000000000 ) ) ;
#45903 = DIRECTION ( 'NONE',  ( 0.000000000000000000, 0.000000000000000000, 1.000000000000000000 ) ) ;
#45904 = CARTESIAN_POINT ( 'NONE',  ( 22.90078658882962159, -15.56738391629757778, -72.45053053649107255 ) ) ;
#45905 = CARTESIAN_POINT ( 'NONE',  ( 11.27216508573649278, -9.290094983139432827, -43.08403395730018559 ) ) ;
#45906 = CARTESIAN_POINT ( 'NONE',  ( 22.24259769081709948, -21.15396733309309596, -50.02674116093399448 ) ) ;
#45907 = EDGE_CURVE ( 'NONE', #5766, #39844, #21642, .T. ) ;
#45908 = CARTESIAN_POINT ( 'NONE',  ( 0.03129314105546310287, -20.74349987192420031, -34.73925587533990011 ) ) ;
#45909 = CARTESIAN_POINT ( 'NONE',  ( 44.25911907560086433, -37.95088198482868336, -69.02407459214848018 ) ) ;
#45910 = EDGE_LOOP ( 'NONE', ( #46849, #1207, #16552, #51789 ) ) ;
#45911 = CARTESIAN_POINT ( 'NONE',  ( 18.71088192717838439, 20.68057025370971758, -75.01676221305848458 ) ) ;
#45912 = CARTESIAN_POINT ( 'NONE',  ( 8.789551320866550554, -16.86786260806620064, -43.17892530838289389 ) ) ;
#45913 = CARTESIAN_POINT ( 'NONE',  ( 53.54323433243279595, -49.41229159844919394, -49.20622374552320366 ) ) ;
#45914 = CARTESIAN_POINT ( 'NONE',  ( 10.07444332260010000, -12.10786745998580116, -32.14999999999999858 ) ) ;
#45915 = B_SPLINE_CURVE_WITH_KNOTS ( 'NONE', 3,
 ( #20272, #44921, #36265, #628, #374, #16355, #32568, #891, #23686, #49645, #22084, #2190, #38095, #41500, #45179, #33882, #9292, #29947 ),
 .UNSPECIFIED., .F., .F.,
 ( 4, 2, 2, 2, 2, 2, 2, 2, 4 ),
 ( 0.000000000000000000, 0.06250010287737421677, 0.1250002057547484335, 0.1875003086321226364, 0.2500004115094968671, 0.3125005143868710977, 0.3750006172642452729, 0.4375007201416195035, 0.5000008230189937342 ),
 .UNSPECIFIED. ) ;
#45916 = CARTESIAN_POINT ( 'NONE',  ( 14.27557369763509953, 19.88380302201240113, -74.34036667011370980 ) ) ;
#45917 = CARTESIAN_POINT ( 'NONE',  ( 68.13393739769618662, -28.80002732851770020, -65.65000000000000568 ) ) ;
#45918 = CARTESIAN_POINT ( 'NONE',  ( 40.90034483661249709, -45.10436747181810091, -5.606159996611790319 ) ) ;
#45919 = CARTESIAN_POINT ( 'NONE',  ( 72.13393739769620083, -15.61618894467929941, -20.65000000000000213 ) ) ;
#45920 = VECTOR ( 'NONE', #2258, 1000.000000000000000 ) ;
#45922 = AXIS2_PLACEMENT_3D ( 'NONE', #35367, #7856, #51365 ) ;
#45921 = CARTESIAN_POINT ( 'NONE',  ( 24.17771624763599903, -17.42736053297119980, -49.57816483399629703 ) ) ;
#45923 = VERTEX_POINT ( 'NONE', #44669 ) ;
#45924 = CARTESIAN_POINT ( 'NONE',  ( 55.02169238797419837, -47.04713376395680058, -25.69011823353289969 ) ) ;
#45925 = CARTESIAN_POINT ( 'NONE',  ( 56.50576444368559237, -50.74247142358070306, -74.45835159213530119 ) ) ;
#45927 = CARTESIAN_POINT ( 'NONE',  ( 42.01335208650808539, -39.76583440177442696, -76.26778565571557067 ) ) ;
#45926 = CARTESIAN_POINT ( 'NONE',  ( 10.69487833177709923, 33.67413918231929415, -18.00053523990690252 ) ) ;
#45929 = EDGE_CURVE ( 'NONE', #21614, #34841, #15097, .T. ) ;
#45928 = CARTESIAN_POINT ( 'NONE',  ( 22.90065710272254762, -15.15489767342495320, -70.82548965592042123 ) ) ;
#45930 = DIRECTION ( 'NONE',  ( -0.8732394366197182567, 0.4872913772396111343, -1.665334536937735304E-16 ) ) ;
#45931 = ORIENTED_EDGE ( 'NONE', *, *, #22908, .T. ) ;
#45932 = CARTESIAN_POINT ( 'NONE',  ( -2.656266621570580355, -48.72136079459129832, -4.829465372056970018 ) ) ;
#45933 = CARTESIAN_POINT ( 'NONE',  ( 47.45846583226310145, 23.39139597829760220, -54.90779131713600236 ) ) ;
#45934 = CARTESIAN_POINT ( 'NONE',  ( 23.98389812145492428, -14.41982823175175810, -65.74426863541066268 ) ) ;
#45935 = CARTESIAN_POINT ( 'NONE',  ( 63.15096886846599489, 0.8925687589132640376, -62.30780775221820278 ) ) ;
#45936 = DIRECTION ( 'NONE',  ( -1.224646799147336690E-16, 1.000000000000000000, 1.919972818367720325E-16 ) ) ;
#45937 = CARTESIAN_POINT ( 'NONE',  ( 11.70209409420199975, 33.86888164218810005, -16.68277806565760102 ) ) ;
#45938 = CARTESIAN_POINT ( 'NONE',  ( 16.84831893358406418, -22.63275635301463140, -57.31488281879011737 ) ) ;
#45939 = CARTESIAN_POINT ( 'NONE',  ( 35.44295439207109411, -15.61618894467929763, 16.85000000000000142 ) ) ;
#45940 = CARTESIAN_POINT ( 'NONE',  ( 22.63393739769619728, -15.61618894467929941, -5.690000000000000391 ) ) ;
#45941 = CARTESIAN_POINT ( 'NONE',  ( 38.67452568954060155, 6.328436186825659782, -81.65000000000000568 ) ) ;
#45942 = CARTESIAN_POINT ( 'NONE',  ( 9.367002091613079173, -15.61601527432330094, -39.84717978380999881 ) ) ;
#45943 = CARTESIAN_POINT ( 'NONE',  ( 55.73977427824559783, 19.85292510495689910, -53.93776639183540311 ) ) ;
#45944 = CARTESIAN_POINT ( 'NONE',  ( 63.42971025143901187, 1.310552486429319874, -69.07674887557429599 ) ) ;
#45945 = CARTESIAN_POINT ( 'NONE',  ( 0.1542402430813090142, -50.99248106341759978, -19.14999999999999858 ) ) ;
#45946 = DIRECTION ( 'NONE',  ( 0.000000000000000000, 0.000000000000000000, 1.000000000000000000 ) ) ;
#45947 = ORIENTED_EDGE ( 'NONE', *, *, #32662, .T. ) ;
#45948 = CARTESIAN_POINT ( 'NONE',  ( 20.05501060430114180, 23.95707817317984833, -19.14226881137857106 ) ) ;
#45949 = CARTESIAN_POINT ( 'NONE',  ( 11.10572504400830063, 32.22711006948190260, -44.26001407538520027 ) ) ;
#45950 = CARTESIAN_POINT ( 'NONE',  ( 72.94808712738880274, 1.229084191802120030, -62.25930094257930136 ) ) ;
#45951 = CARTESIAN_POINT ( 'NONE',  ( 65.36111452216670159, -32.61132144897129592, -18.37584006277759840 ) ) ;
#45952 = CARTESIAN_POINT ( 'NONE',  ( 12.69291600278502763, 24.23553010417859710, -75.52237511313917651 ) ) ;
#45953 = ORIENTED_EDGE ( 'NONE', *, *, #38939, .F. ) ;
#45954 = ORIENTED_EDGE ( 'NONE', *, *, #5906, .F. ) ;
#45955 = CARTESIAN_POINT ( 'NONE',  ( 48.40744063480869386, 22.97621965999729809, -55.31593188200960043 ) ) ;
#45956 = CARTESIAN_POINT ( 'NONE',  ( 49.89456891052482490, -1.537756983171397973, -15.90506407067071848 ) ) ;
#45957 = VERTEX_POINT ( 'NONE', #40997 ) ;
#45958 = CARTESIAN_POINT ( 'NONE',  ( 12.21878994645900107, -65.31006707541760647, -46.54195938077629791 ) ) ;
#45959 = CARTESIAN_POINT ( 'NONE',  ( 56.98013733811719561, -45.52736395732640062, -26.04777137428060030 ) ) ;
#45960 = CARTESIAN_POINT ( 'NONE',  ( 24.04483843941790866, -15.61617050235280679, -77.50767555791956909 ) ) ;
#45961 = CARTESIAN_POINT ( 'NONE',  ( 2.414204846871014887, -25.84668130286647170, -35.10658870009421406 ) ) ;
#45962 = ORIENTED_EDGE ( 'NONE', *, *, #9279, .T. ) ;
#45963 = AXIS2_PLACEMENT_3D ( 'NONE', #11041, #20352, #36339 ) ;
#45964 = CARTESIAN_POINT ( 'NONE',  ( 46.83508469244584660, 7.002556948733312581, -56.14421558670044732 ) ) ;
#45965 = CIRCLE ( 'NONE', #44292, 2.700000000000230216 ) ;
#45966 = VECTOR ( 'NONE', #4371, 1000.000000000000000 ) ;
#45967 = ORIENTED_EDGE ( 'NONE', *, *, #26317, .F. ) ;
#45968 = CARTESIAN_POINT ( 'NONE',  ( 51.09762045080680792, -45.11618894460819718, -11.35987698341929963 ) ) ;
#45969 = EDGE_CURVE ( 'NONE', #6259, #40855, #47557, .T. ) ;
#45970 = CARTESIAN_POINT ( 'NONE',  ( 8.317661897737014698, -17.01424986305827858, -34.73604595880143364 ) ) ;
#45971 = CARTESIAN_POINT ( 'NONE',  ( 14.48916582607680148, 19.87152568006800024, -22.14433180932219969 ) ) ;
#45972 = CARTESIAN_POINT ( 'NONE',  ( 22.72320028845815898, -17.73845357403389045, -48.94698896582607972 ) ) ;
#45973 = ADVANCED_FACE ( 'NONE', ( #8516 ), #32579, .F. ) ;
#45974 = EDGE_CURVE ( 'NONE', #43315, #9983, #45084, .T. ) ;
#45975 = DIRECTION ( 'NONE',  ( 1.000000000000000000, 0.000000000000000000, 0.000000000000000000 ) ) ;
#45976 = CARTESIAN_POINT ( 'NONE',  ( 46.77981249583429957, -53.79990661969940646, -75.90649761523269490 ) ) ;
#45977 = CARTESIAN_POINT ( 'NONE',  ( 60.42958242686469816, 13.88381321558630077, -10.92174602670019823 ) ) ;
#45978 = EDGE_CURVE ( 'NONE', #5441, #49041, #10795, .T. ) ;
#45979 = CARTESIAN_POINT ( 'NONE',  ( 51.61031096252850148, 13.88381105524890025, -11.72816892371229969 ) ) ;
#45980 = CARTESIAN_POINT ( 'NONE',  ( 53.46638755025719547, 20.54076140048909949, -53.27253650584940203 ) ) ;
#45981 = B_SPLINE_CURVE_WITH_KNOTS ( 'NONE', 3,
 ( #18568, #1813, #22743, #38761, #2856, #2076, #18055, #18820, #34803, #13871, #46114, #34020, #25638, #13618, #46373, #50296, #10461, #29579 ),
 .UNSPECIFIED., .F., .F.,
 ( 4, 2, 2, 2, 2, 2, 2, 2, 4 ),
 ( 0.000000000000000000, 0.06249980390995341084, 0.1249996078199068217, 0.1874994117298602325, 0.2499992156398136434, 0.3124990195497670542, 0.3749988234597204650, 0.4374986273696738759, 0.4999984312796272867 ),
 .UNSPECIFIED. ) ;
#45982 = VECTOR ( 'NONE', #16244, 1000.000000000000000 ) ;
#45983 = CARTESIAN_POINT ( 'NONE',  ( 52.35627133321460036, 19.94929664549539794, -76.02218070044929732 ) ) ;
#45984 = EDGE_CURVE ( 'NONE', #28507, #4867, #37568, .T. ) ;
#45985 = CARTESIAN_POINT ( 'NONE',  ( 57.93647699516559868, 13.95499690129120118, -25.80740772885510026 ) ) ;
#45986 = CARTESIAN_POINT ( 'NONE',  ( 23.48373881468570090, -18.36703741633409948, -77.40150352786659482 ) ) ;
#45987 = ORIENTED_EDGE ( 'NONE', *, *, #457, .T. ) ;
#45988 = CARTESIAN_POINT ( 'NONE',  ( 15.21636614235080032, -50.60415920577569437, -15.64999998222989852 ) ) ;
#45989 = CARTESIAN_POINT ( 'NONE',  ( -11.09439285730369917, -42.12527450341799806, -6.431386034134429330 ) ) ;
#45990 = CARTESIAN_POINT ( 'NONE',  ( 76.62358681188410969, -34.82467708757799585, -13.75998128426440026 ) ) ;
#45992 = EDGE_CURVE ( 'NONE', #47951, #51345, #14972, .T. ) ;
#45991 = CARTESIAN_POINT ( 'NONE',  ( 72.86935405752659278, 1.308983041454300000, -69.01646217275099104 ) ) ;
#45993 = CARTESIAN_POINT ( 'NONE',  ( 75.01912134484176420, -45.11618894467940066, -15.00305751307385371 ) ) ;
#45994 = CONICAL_SURFACE ( 'NONE', #19196, 0.6299999999999977840, 0.7853981633974476129 ) ;
#45995 = CIRCLE ( 'NONE', #16641, 1.999999999999999778 ) ;
#45996 = DIRECTION ( 'NONE',  ( 0.000000000000000000, 0.000000000000000000, -1.000000000000000000 ) ) ;
#45997 = AXIS2_PLACEMENT_3D ( 'NONE', #41158, #40128, #16798 ) ;
#45998 = CARTESIAN_POINT ( 'NONE',  ( 20.99558456173523524, -9.289999057355428747, -43.21596523485415275 ) ) ;
#45999 = AXIS2_PLACEMENT_3D ( 'NONE', #37814, #42006, #17887 ) ;
#46000 = CARTESIAN_POINT ( 'NONE',  ( 42.94731284509209246, 11.34112180473979947, -3.548345704167709780 ) ) ;
#46001 = CARTESIAN_POINT ( 'NONE',  ( 65.13185782384009315, 1.385888765344500007, -70.30422512560809878 ) ) ;
#46002 = CARTESIAN_POINT ( 'NONE',  ( 16.13393739769620083, -15.61618894467929941, 9.349999999999999645 ) ) ;
#46003 = LINE ( 'NONE', #10091, #9703 ) ;
#46004 = CARTESIAN_POINT ( 'NONE',  ( 76.40330808254813633, -43.26114854291000000, -13.96576318196657596 ) ) ;
#46005 = CARTESIAN_POINT ( 'NONE',  ( 18.32671526132769912, -51.19325459173029458, -74.14992922886710858 ) ) ;
#46006 = DIRECTION ( 'NONE',  ( -0.5685928097855378338, 0.5944782866685498490, 0.5685928097855378338 ) ) ;
#46007 = ORIENTED_EDGE ( 'NONE', *, *, #4116, .F. ) ;
#46008 = CARTESIAN_POINT ( 'NONE',  ( 8.802719410737489980, -16.94281517916839874, -58.01035930781959138 ) ) ;
#46009 = CARTESIAN_POINT ( 'NONE',  ( 63.76999183493178691, 1.442158793902849956, -61.94395472936509606 ) ) ;
#46010 = ORIENTED_EDGE ( 'NONE', *, *, #1633, .T. ) ;
#46011 = CARTESIAN_POINT ( 'NONE',  ( 68.13393739769618662, -30.31618894467939995, -65.65000000000000568 ) ) ;
#46012 = FACE_OUTER_BOUND ( 'NONE', #26589, .T. ) ;
#46013 = DIRECTION ( 'NONE',  ( 0.000000000000000000, 0.000000000000000000, -1.000000000000000000 ) ) ;
#46014 = CARTESIAN_POINT ( 'NONE',  ( 19.75585232009591863, -22.67399444841611000, -61.85680124542592750 ) ) ;
#46016 = DIRECTION ( 'NONE',  ( 0.000000000000000000, -1.205285871143275290E-11, -1.000000000000000000 ) ) ;
#46015 = CARTESIAN_POINT ( 'NONE',  ( 44.23496081612994857, 8.741156191882240023, -65.52195280072128014 ) ) ;
#46017 = EDGE_CURVE ( 'NONE', #35078, #7528, #20427, .T. ) ;
#46018 = CARTESIAN_POINT ( 'NONE',  ( 19.13393739769600188, 18.38381105532069881, -35.14999999999999858 ) ) ;
#46019 = CARTESIAN_POINT ( 'NONE',  ( 10.11211546542419804, -54.10246922935670000, -34.93361312117490058 ) ) ;
#46020 = EDGE_LOOP ( 'NONE', ( #41612, #9380, #25339, #10695 ) ) ;
#46021 = VERTEX_POINT ( 'NONE', #10067 ) ;
#46022 = B_SPLINE_CURVE_WITH_KNOTS ( 'NONE', 3,
 ( #33698, #6460, #1744, #29759, #34474, #46822, #49967, #22418 ),
 .UNSPECIFIED., .F., .F.,
 ( 4, 2, 2, 4 ),
 ( 0.05028014561732388477, 0.06097673919802479997, 0.07774712209307470256, 0.08013618654850850065 ),
 .UNSPECIFIED. ) ;
#46023 = ORIENTED_EDGE ( 'NONE', *, *, #49288, .F. ) ;
#46024 = CARTESIAN_POINT ( 'NONE',  ( 61.38174641265649711, -45.18824807282129541, -46.54645048572430710 ) ) ;
#46025 = CARTESIAN_POINT ( 'NONE',  ( 17.98749078828957337, 10.53025766472752522, -34.79644660940672907 ) ) ;
#46026 = CARTESIAN_POINT ( 'NONE',  ( 68.13393739769620083, 4.883811055320659733, -65.65000000000000568 ) ) ;
#46027 = EDGE_LOOP ( 'NONE', ( #45238, #28719, #36251, #17923 ) ) ;
#46028 = VERTEX_POINT ( 'NONE', #45455 ) ;
#46029 = CARTESIAN_POINT ( 'NONE',  ( 23.99007353491660055, -14.66733099292005704, -77.46942086223019430 ) ) ;
#46030 = CARTESIAN_POINT ( 'NONE',  ( 52.85072064880949938, -52.31592968273889710, -54.40017261481339972 ) ) ;
#46031 = FACE_OUTER_BOUND ( 'NONE', #51032, .T. ) ;
#46032 = VECTOR ( 'NONE', #30276, 1000.000000000000000 ) ;
#46033 = CIRCLE ( 'NONE', #25076, 1.000000000000000888 ) ;
#46034 = VERTEX_POINT ( 'NONE', #38107 ) ;
#46035 = CARTESIAN_POINT ( 'NONE',  ( 24.04493184060211419, -15.62634507059355116, -49.50807437602926342 ) ) ;
#46036 = CARTESIAN_POINT ( 'NONE',  ( 52.80343917019639832, -50.48755729126909841, -76.73469608504859707 ) ) ;
#46037 = AXIS2_PLACEMENT_3D ( 'NONE', #43281, #38835, #23831 ) ;
#46038 = CARTESIAN_POINT ( 'NONE',  ( 60.44851881380330383, 14.43911564095640010, -47.27117109066509926 ) ) ;
#46039 = AXIS2_PLACEMENT_3D ( 'NONE', #29678, #1659, #9535 ) ;
#46040 = EDGE_CURVE ( 'NONE', #33885, #48970, #32606, .T. ) ;
#46041 = CARTESIAN_POINT ( 'NONE',  ( 23.02837255652150006, -19.36499027741710321, -74.17102124479808367 ) ) ;
#46042 = DIRECTION ( 'NONE',  ( 0.000000000000000000, -1.000000000000000000, 0.000000000000000000 ) ) ;
#46044 = CARTESIAN_POINT ( 'NONE',  ( 41.11636130713259973, 13.67919800510379957, -5.497150100476379642 ) ) ;
#46043 = B_SPLINE_CURVE_WITH_KNOTS ( 'NONE', 3,
 ( #35682, #19434, #15510, #31464, #7652, #39614 ),
 .UNSPECIFIED., .F., .F.,
 ( 4, 2, 4 ),
 ( 0.000000000000000000, 0.1329384993766630774, 0.2774707949478909530 ),
 .UNSPECIFIED. ) ;
#46045 = CIRCLE ( 'NONE', #834, 40.00000000000000711 ) ;
#46046 = CARTESIAN_POINT ( 'NONE',  ( 42.10819013297950164, -43.62195994593520254, -4.221348723911680700 ) ) ;
#46047 = DIRECTION ( 'NONE',  ( 0.000000000000000000, 1.000000000000000000, 0.000000000000000000 ) ) ;
#46048 = CARTESIAN_POINT ( 'NONE',  ( -3.454818612163319536, 17.59177618004110144, -5.676727923997320069 ) ) ;
#46049 = CARTESIAN_POINT ( 'NONE',  ( 64.67348939754930370, 1.419996320997050088, -70.13930819973541020 ) ) ;
#46050 = CARTESIAN_POINT ( 'NONE',  ( 18.62387150434391003, -22.21488518936683221, -33.23232777544671279 ) ) ;
#46051 = LINE ( 'NONE', #14321, #15866 ) ;
#46052 = ORIENTED_EDGE ( 'NONE', *, *, #45058, .T. ) ;
#46053 = CARTESIAN_POINT ( 'NONE',  ( -3.610905026690430120, -50.40327272064629938, -4.296538310234230273 ) ) ;
#46054 = FACE_OUTER_BOUND ( 'NONE', #31993, .T. ) ;
#46055 = EDGE_CURVE ( 'NONE', #14553, #47534, #24400, .T. ) ;
#46056 = CARTESIAN_POINT ( 'NONE',  ( 44.13393739769620083, 4.883811055320659733, -44.64999999999999858 ) ) ;
#46057 = FACE_OUTER_BOUND ( 'NONE', #35240, .T. ) ;
#46058 = CARTESIAN_POINT ( 'NONE',  ( 46.53687296277449548, -53.33479509908829641, -76.10218428122850298 ) ) ;
#46059 = CARTESIAN_POINT ( 'NONE',  ( 63.41538649190439969, 1.369535599030039963, -68.77214795431979155 ) ) ;
#46060 = CARTESIAN_POINT ( 'NONE',  ( 48.21566362429800279, -54.17964390236579675, -54.67775470772419766 ) ) ;
#46061 = CARTESIAN_POINT ( 'NONE',  ( 16.32680532830336517, -7.629206002645773310, -45.01510652521700706 ) ) ;
#46062 = FACE_OUTER_BOUND ( 'NONE', #3633, .T. ) ;
#46063 = CARTESIAN_POINT ( 'NONE',  ( 42.26864913071712238, 13.12941410808000242, -5.126484831624812166 ) ) ;
#46064 = CARTESIAN_POINT ( 'NONE',  ( 47.88656099864510196, 23.18744658311759821, -55.03929334947260088 ) ) ;
#46065 = ORIENTED_EDGE ( 'NONE', *, *, #29261, .F. ) ;
#46066 = CIRCLE ( 'NONE', #33514, 0.9999999999999940048 ) ;
#46067 = CARTESIAN_POINT ( 'NONE',  ( 15.24135970174500088, -8.620056853935039953, -70.30678751322059838 ) ) ;
#46068 = EDGE_LOOP ( 'NONE', ( #5796, #22013, #26967, #27260 ) ) ;
#46069 = AXIS2_PLACEMENT_3D ( 'NONE', #15066, #34970, #22396 ) ;
#46070 = CARTESIAN_POINT ( 'NONE',  ( 16.13393739769620083, -15.61618894467929941, -14.03562394879499919 ) ) ;
#46071 = FACE_OUTER_BOUND ( 'NONE', #35035, .T. ) ;
#46072 = CARTESIAN_POINT ( 'NONE',  ( 9.807872590848809580, -10.75438206521125295, -40.71600156056624797 ) ) ;
#46074 = DIRECTION ( 'NONE',  ( 0.000000000000000000, 1.000000000000000000, 0.000000000000000000 ) ) ;
#46073 = CARTESIAN_POINT ( 'NONE',  ( 84.01174786492798319, 13.38463874174230028, -47.41946551740999638 ) ) ;
#46075 = EDGE_CURVE ( 'NONE', #35304, #38311, #44262, .T. ) ;
#46076 = CIRCLE ( 'NONE', #30154, 2.745157762967529447 ) ;
#46077 = CARTESIAN_POINT ( 'NONE',  ( 10.82216332218549937, -10.97640288017059973, -79.68135863817170161 ) ) ;
#46078 = CIRCLE ( 'NONE', #7575, 40.00000000000000711 ) ;
#46079 = DIRECTION ( 'NONE',  ( 0.000000000000000000, -1.000000000000000000, 0.000000000000000000 ) ) ;
#46080 = CARTESIAN_POINT ( 'NONE',  ( 14.13393739769640156, 10.38381105532060111, -54.64999999999999858 ) ) ;
#46081 = CARTESIAN_POINT ( 'NONE',  ( 12.72585196119663387, -21.52904731480777301, -41.11943263090543610 ) ) ;
#46082 = EDGE_LOOP ( 'NONE', ( #27685, #14363, #14100, #28648 ) ) ;
#46083 = FACE_OUTER_BOUND ( 'NONE', #43826, .T. ) ;
#46084 = EDGE_CURVE ( 'NONE', #34653, #19900, #26664, .T. ) ;
#46085 = ORIENTED_EDGE ( 'NONE', *, *, #16488, .F. ) ;
#46086 = VERTEX_POINT ( 'NONE', #25765 ) ;
#46087 = ADVANCED_FACE ( 'NONE', ( #10594 ), #37577, .T. ) ;
#46088 = CARTESIAN_POINT ( 'NONE',  ( 12.17975455547079910, -64.68546118318118943, -15.92303081430319978 ) ) ;
#46089 = CARTESIAN_POINT ( 'NONE',  ( 18.66382343656906073, -8.049420821458873831, -39.11066728049964070 ) ) ;
#46090 = CARTESIAN_POINT ( 'NONE',  ( 17.90522083139575571, -22.20705201471875512, -54.86948871813314099 ) ) ;
#46091 = CARTESIAN_POINT ( 'NONE',  ( 50.95940558857264335, 4.060833044306336070, -76.37898308257572921 ) ) ;
#46092 = ORIENTED_EDGE ( 'NONE', *, *, #36893, .T. ) ;
#46093 = ORIENTED_EDGE ( 'NONE', *, *, #24385, .F. ) ;
#46094 = CARTESIAN_POINT ( 'NONE',  ( -10.06026339569850059, -44.57856433944859731, -43.51454834703589825 ) ) ;
#46095 = DIRECTION ( 'NONE',  ( 0.000000000000000000, -1.000000000000000000, 0.000000000000000000 ) ) ;
#46096 = CARTESIAN_POINT ( 'NONE',  ( 52.99306741825720479, 18.23831009604760212, -48.55383660268419987 ) ) ;
#46097 = CARTESIAN_POINT ( 'NONE',  ( 61.61391020117169859, -1.934278441492739864, -16.00420058451779681 ) ) ;
#46098 = CARTESIAN_POINT ( 'NONE',  ( 51.47090657186449647, -50.21087343025810412, -76.34335276480290133 ) ) ;
#46099 = CARTESIAN_POINT ( 'NONE',  ( 60.02266206094759582, -46.59019202402480886, -48.66142267842249680 ) ) ;
#46100 = EDGE_CURVE ( 'NONE', #42078, #22439, #49656, .T. ) ;
#46101 = ORIENTED_EDGE ( 'NONE', *, *, #447, .T. ) ;
#46102 = CYLINDRICAL_SURFACE ( 'NONE', #22430, 39.00000000000000711 ) ;
#46103 = CARTESIAN_POINT ( 'NONE',  ( 11.27237203167939050, -21.94243938119325321, -48.50066542447320472 ) ) ;
#46104 = ORIENTED_EDGE ( 'NONE', *, *, #19963, .T. ) ;
#46105 = CARTESIAN_POINT ( 'NONE',  ( 54.17308945005400034, -50.61618894467930119, -77.01198594373980200 ) ) ;
#46106 = CARTESIAN_POINT ( 'NONE',  ( 53.59007319875249920, 18.17385789302069554, -49.22505640236219904 ) ) ;
#46107 = EDGE_CURVE ( 'NONE', #34997, #32498, #30225, .T. ) ;
#46108 = CARTESIAN_POINT ( 'NONE',  ( 10.81856248199949988, -9.842668606344618709, -43.27563812998649695 ) ) ;
#46109 = CARTESIAN_POINT ( 'NONE',  ( 13.97043394117600101, -50.94378507946090195, -21.74715833460999903 ) ) ;
#46110 = CARTESIAN_POINT ( 'NONE',  ( 55.28123845478469889, 19.42107725494309989, -76.05360625656349782 ) ) ;
#46111 = CARTESIAN_POINT ( 'NONE',  ( 47.64143405400680109, -54.53488714545009941, -74.14999999999999147 ) ) ;
#46112 = ORIENTED_EDGE ( 'NONE', *, *, #1045, .F. ) ;
#46113 = CARTESIAN_POINT ( 'NONE',  ( 55.90707799132489697, 14.33971025050679948, -16.63726872277679902 ) ) ;
#46114 = CARTESIAN_POINT ( 'NONE',  ( 17.90521547582839545, -9.025324361372922155, -78.03615171934956152 ) ) ;
#46115 = AXIS2_PLACEMENT_3D ( 'NONE', #34894, #6880, #2412 ) ;
#46116 = CARTESIAN_POINT ( 'NONE',  ( 57.28557293626779767, -50.57890658449659327, -53.44460714491770403 ) ) ;
#46117 = CARTESIAN_POINT ( 'NONE',  ( 17.77056402554710246, -8.755867344676808273, -42.42172377882659617 ) ) ;
#46118 = CARTESIAN_POINT ( 'NONE',  ( 9.367199122489369145, -14.48686353315465780, -43.90031557396017092 ) ) ;
#46119 = VECTOR ( 'NONE', #3928, 1000.000000000000000 ) ;
#46120 = ORIENTED_EDGE ( 'NONE', *, *, #2973, .F. ) ;
#46121 = CARTESIAN_POINT ( 'NONE',  ( 47.35407109286579441, 23.03649510332309802, -75.29485535639010152 ) ) ;
#46122 = CARTESIAN_POINT ( 'NONE',  ( 64.97290478796050195, 0.8840451408750739093, -60.55014093144429665 ) ) ;
#46123 = FACE_OUTER_BOUND ( 'NONE', #7836, .T. ) ;
#46124 = CARTESIAN_POINT ( 'NONE',  ( 12.70130225181580741, -65.47524089349515464, -23.44891406722884142 ) ) ;
#46125 = CARTESIAN_POINT ( 'NONE',  ( 46.25525774125583922, 2.762490711761015572, -35.14999999999999858 ) ) ;
#46126 = CARTESIAN_POINT ( 'NONE',  ( 82.75519962004040053, 14.36566124015802082, -47.67565474709540041 ) ) ;
#46127 = CARTESIAN_POINT ( 'NONE',  ( -21.18404982641129664, -3.931304892986000166, -53.29316999191859594 ) ) ;
#46129 = CARTESIAN_POINT ( 'NONE',  ( 45.67777725554724100, -40.20714941387052477, -57.99046403957294871 ) ) ;
#46128 = CARTESIAN_POINT ( 'NONE',  ( 64.74712693194929614, 0.8966068345641480253, -60.69721413447479819 ) ) ;
#46130 = FACE_OUTER_BOUND ( 'NONE', #35775, .T. ) ;
#46131 = CARTESIAN_POINT ( 'NONE',  ( 6.264007226343670354, 32.14677423655729882, -47.23119725298469973 ) ) ;
#46132 = ORIENTED_EDGE ( 'NONE', *, *, #31846, .F. ) ;
#46133 = CARTESIAN_POINT ( 'NONE',  ( 53.35042868538379679, -49.41591823479419787, -49.00406147840819671 ) ) ;
#46134 = ORIENTED_EDGE ( 'NONE', *, *, #33300, .F. ) ;
#46135 = CARTESIAN_POINT ( 'NONE',  ( 42.88601970632411309, 8.687503640012517181, -71.78374453940418221 ) ) ;
#46136 = CARTESIAN_POINT ( 'NONE',  ( 53.62552786343490396, -51.33071804962359153, -75.58099297212140755 ) ) ;
#46137 = CARTESIAN_POINT ( 'NONE',  ( 13.75275436563869924, 20.07553849835239745, -22.95880022689469868 ) ) ;
#46138 = CARTESIAN_POINT ( 'NONE',  ( 56.24035600606469387, 14.32860529291999896, -25.36904170088440225 ) ) ;
#46139 = CARTESIAN_POINT ( 'NONE',  ( 22.49503038576149905, -12.57003486226449951, -48.31066193697829902 ) ) ;
#46140 = CARTESIAN_POINT ( 'NONE',  ( 29.02733844998730106, -26.70053505390490400, -34.83948955561429983 ) ) ;
#46141 = CARTESIAN_POINT ( 'NONE',  ( 53.23494276941970327, 18.29173816151630305, -49.16096157153140211 ) ) ;
#46142 = CARTESIAN_POINT ( 'NONE',  ( 64.74712693194929614, 0.8966068345641440285, -60.69721413447479819 ) ) ;
#46143 = DIRECTION ( 'NONE',  ( 0.3918900565165093774, -0.9200120562272470215, -1.682577688288945566E-10 ) ) ;
#46144 = EDGE_CURVE ( 'NONE', #29490, #19827, #24140, .T. ) ;
#46145 = B_SPLINE_CURVE_WITH_KNOTS ( 'NONE', 3,
 ( #35799, #51784, #11964, #29212, #33139, #41279, #25005, #24750 ),
 .UNSPECIFIED., .F., .F.,
 ( 4, 2, 2, 4 ),
 ( 0.000000000000000000, 0.2018913194515775666, 0.4037826389031551333, 0.8075652778063105997 ),
 .UNSPECIFIED. ) ;
#46146 = EDGE_LOOP ( 'NONE', ( #13702, #34706, #16267, #46010 ) ) ;
#46147 = CARTESIAN_POINT ( 'NONE',  ( 22.63968590808610415, -11.22734120214469833, -35.09859433989379340 ) ) ;
#46148 = ADVANCED_FACE ( 'NONE', ( #26292 ), #34147, .T. ) ;
#46149 = FACE_OUTER_BOUND ( 'NONE', #36157, .T. ) ;
#46150 = CARTESIAN_POINT ( 'NONE',  ( 24.04493739830126131, -15.61513439321896080, -49.79228809144822776 ) ) ;
#46151 = CARTESIAN_POINT ( 'NONE',  ( 73.00772670898579975, 1.265401080857980087, -62.43968814002079881 ) ) ;
#46152 = CIRCLE ( 'NONE', #26890, 1.000000000000000888 ) ;
#46153 = CARTESIAN_POINT ( 'NONE',  ( 10.63085527530649976, -64.83908867352720051, -18.12439166849010164 ) ) ;
#46154 = FACE_OUTER_BOUND ( 'NONE', #22150, .T. ) ;
#46155 = CARTESIAN_POINT ( 'NONE',  ( 24.04213744851809409, -15.84352304058485394, -75.80147181961574177 ) ) ;
#46156 = AXIS2_PLACEMENT_3D ( 'NONE', #36456, #15534, #47511 ) ;
#46157 = AXIS2_PLACEMENT_3D ( 'NONE', #22275, #50598, #50345 ) ;
#46158 = CARTESIAN_POINT ( 'NONE',  ( 62.09157612670949788, -33.11618894467940066, -65.34607522167520699 ) ) ;
#46159 = CARTESIAN_POINT ( 'NONE',  ( 64.84562941585738827, 1.096044978595170027, -70.62064874955129312 ) ) ;
#46160 = VERTEX_POINT ( 'NONE', #10331 ) ;
#46161 = CARTESIAN_POINT ( 'NONE',  ( 10.49214094476729997, -63.29059696784919709, -45.62564302952420547 ) ) ;
#46162 = DIRECTION ( 'NONE',  ( 0.000000000000000000, 0.000000000000000000, 1.000000000000000000 ) ) ;
#46163 = VERTEX_POINT ( 'NONE', #26028 ) ;
#46164 = LINE ( 'NONE', #22277, #4948 ) ;
#46165 = CARTESIAN_POINT ( 'NONE',  ( 57.25859902321930406, 19.38378582711590070, -53.75766468042880319 ) ) ;
#46166 = DIRECTION ( 'NONE',  ( 0.000000000000000000, 0.000000000000000000, -1.000000000000000000 ) ) ;
#46167 = CARTESIAN_POINT ( 'NONE',  ( 52.43830859903380315, 18.75446654067290098, -77.15472074777260048 ) ) ;
#46168 = ORIENTED_EDGE ( 'NONE', *, *, #47758, .F. ) ;
#46169 = DIRECTION ( 'NONE',  ( 1.000000000000000000, 0.000000000000000000, 0.000000000000000000 ) ) ;
#46170 = DIRECTION ( 'NONE',  ( -0.000000000000000000, 1.000000000000000000, 0.000000000000000000 ) ) ;
#46171 = LINE ( 'NONE', #13676, #13458 ) ;
#46172 = CARTESIAN_POINT ( 'NONE',  ( 14.41409827330783244, -23.35832077669386919, -66.07723603011802993 ) ) ;
#46173 = EDGE_CURVE ( 'NONE', #23933, #16762, #42301, .T. ) ;
#46174 = CARTESIAN_POINT ( 'NONE',  ( 15.70667492358600015, -7.382103273874560223, -61.27582937196799406 ) ) ;
#46175 = CARTESIAN_POINT ( 'NONE',  ( 16.13393739769620083, -15.61618894467929941, -32.14999999999999858 ) ) ;
#46176 = CARTESIAN_POINT ( 'NONE',  ( 44.67240390351668111, -38.00310740330090908, -66.95760940388875326 ) ) ;
#46177 = EDGE_CURVE ( 'NONE', #16605, #34659, #11952, .T. ) ;
#46178 = CARTESIAN_POINT ( 'NONE',  ( 0.000000000000000000, 0.000000000000000000, 0.000000000000000000 ) ) ;
#46179 = ORIENTED_EDGE ( 'NONE', *, *, #19681, .T. ) ;
#46180 = CARTESIAN_POINT ( 'NONE',  ( 23.13393739769620083, -38.61618894467930119, -59.64999999999999147 ) ) ;
#46181 = CARTESIAN_POINT ( 'NONE',  ( 19.30000495840850050, -8.872101904452820875, -45.87236896454599844 ) ) ;
#46182 = CARTESIAN_POINT ( 'NONE',  ( 9.694235770851330258, -12.72427817909970038, -32.14999999999999858 ) ) ;
#46183 = CARTESIAN_POINT ( 'NONE',  ( 14.43211210535319999, 20.28384221772149942, -75.35480091913980516 ) ) ;
#46184 = CARTESIAN_POINT ( 'NONE',  ( 72.13393739769620083, -30.11618894467929763, -20.65000000000000213 ) ) ;
#46185 = AXIS2_PLACEMENT_3D ( 'NONE', #33000, #29339, #12594 ) ;
#46186 =( BOUNDED_CURVE ( )  B_SPLINE_CURVE ( 3, ( #8682, #28061, #36189, #36976 ),
 .UNSPECIFIED., .F., .T. ) 
 B_SPLINE_CURVE_WITH_KNOTS ( ( 4, 4 ),
 ( 2.742903481755264661, 2.960178077714945122 ),
 .UNSPECIFIED. ) 
 CURVE ( )  GEOMETRIC_REPRESENTATION_ITEM ( )  RATIONAL_B_SPLINE_CURVE ( ( 1.000000000000000000, 0.9960698467707308490, 0.9960698467707308490, 1.000000000000000000 ) ) 
 REPRESENTATION_ITEM ( '' )  );
#46187 = CARTESIAN_POINT ( 'NONE',  ( 43.31517999238410255, -45.11752382326270094, -6.625465738846780361 ) ) ;
#46188 = CIRCLE ( 'NONE', #36139, 0.5000000000000004441 ) ;
#46189 = DIRECTION ( 'NONE',  ( 0.000000000000000000, 0.000000000000000000, 1.000000000000000000 ) ) ;
#46190 = CIRCLE ( 'NONE', #22736, 20.00000000000000355 ) ;
#46191 = B_SPLINE_CURVE_WITH_KNOTS ( 'NONE', 3,
 ( #12468, #28692, #12737, #16652, #44694, #21092, #25007, #4084, #32095, #40502, #8276, #160, #13003, #40249, #33141, #5136, #27922, #24225 ),
 .UNSPECIFIED., .F., .F.,
 ( 4, 2, 2, 2, 2, 2, 2, 2, 4 ),
 ( 0.000000000000000000, 0.06249980336323174290, 0.1249996067264634858, 0.1874994100896952287, 0.2499992134529269716, 0.3124990168161584925, 0.3749988201793900133, 0.4374986235426215342, 0.4999984269058530550 ),
 .UNSPECIFIED. ) ;
#46192 = CARTESIAN_POINT ( 'NONE',  ( 8.487904048203290586, -12.53059423256670080, -64.62976173608389274 ) ) ;
#46193 = ORIENTED_EDGE ( 'NONE', *, *, #44756, .F. ) ;
#46194 = CARTESIAN_POINT ( 'NONE',  ( 52.61926156638589447, -49.80650514857250499, -27.99463703858910080 ) ) ;
#46195 = CARTESIAN_POINT ( 'NONE',  ( 56.01738229311430217, -50.84638869582439469, -74.81998313493859598 ) ) ;
#46197 = DIRECTION ( 'NONE',  ( -1.000000000000000000, 0.000000000000000000, 0.000000000000000000 ) ) ;
#46196 = CARTESIAN_POINT ( 'NONE',  ( 9.944906686717320810, 32.89002097141860048, -17.55162828126229613 ) ) ;
#46198 = DIRECTION ( 'NONE',  ( 0.9316796806447995571, 5.770384170489247332E-14, 0.3632808454537678755 ) ) ;
#46199 = CARTESIAN_POINT ( 'NONE',  ( -22.39277411605874235, 24.23791302157028227, 17.35000000000000142 ) ) ;
#46200 = ORIENTED_EDGE ( 'NONE', *, *, #45599, .F. ) ;
#46201 = CARTESIAN_POINT ( 'NONE',  ( -7.645228210567119653, -45.25745332872840265, -5.002875026096710087 ) ) ;
#46202 = CARTESIAN_POINT ( 'NONE',  ( 47.44137716603319888, 23.39923864022719968, -54.82496924537529992 ) ) ;
#46203 = CARTESIAN_POINT ( 'NONE',  ( 23.66141598489997477, -13.08829882855880911, -65.68915168220915746 ) ) ;
#46204 = CARTESIAN_POINT ( 'NONE',  ( 1.260912450620399916, -15.61618894467929763, -7.225658350974740074 ) ) ;
#46205 = CARTESIAN_POINT ( 'NONE',  ( 60.96910362672209516, 14.16411045968260041, -46.92511258430779719 ) ) ;
#46206 = CARTESIAN_POINT ( 'NONE',  ( 11.92291169285739905, 34.11167932846120010, -17.18421408354569735 ) ) ;
#46207 = CARTESIAN_POINT ( 'NONE',  ( 51.68229834221979502, 17.53315898051910082, -77.01558403217930504 ) ) ;
#46208 = CARTESIAN_POINT ( 'NONE',  ( 53.30280620372429468, 18.18069847459639732, -48.78464136231010428 ) ) ;
#46209 = CARTESIAN_POINT ( 'NONE',  ( -9.882013117715120032, 9.266944274022621997, -19.14999999999999858 ) ) ;
#46210 = CARTESIAN_POINT ( 'NONE',  ( 24.04493739769619864, -15.61618894467929941, -32.14999999999999858 ) ) ;
#46211 = CARTESIAN_POINT ( 'NONE',  ( 56.05988273593580118, 15.17408758016209980, -26.21244545727219943 ) ) ;
#46212 = EDGE_CURVE ( 'NONE', #16411, #28603, #35037, .T. ) ;
#46213 = CARTESIAN_POINT ( 'NONE',  ( 53.36385794813689643, 20.84367329114500222, -53.95571242954590474 ) ) ;
#46214 = CARTESIAN_POINT ( 'NONE',  ( 63.40602163964879878, 1.051323308921499944, -69.33345902934181026 ) ) ;
#46215 = CARTESIAN_POINT ( 'NONE',  ( 53.41952757764659765, 18.23162460577420063, -49.21226385651820578 ) ) ;
#46216 = CARTESIAN_POINT ( 'NONE',  ( 49.87147262927059899, -45.11618894467940066, -8.489676102032369442 ) ) ;
#46217 = DIRECTION ( 'NONE',  ( -0.9200120562340469155, 0.3918900565005459247, -8.326672684688669123E-17 ) ) ;
#46218 = CARTESIAN_POINT ( 'NONE',  ( 11.10555358749919996, 32.08123220696739253, -44.25270282110179920 ) ) ;
#46219 = CARTESIAN_POINT ( 'NONE',  ( 72.97999464611700660, 0.9170823515334800557, -62.11176382508629956 ) ) ;
#46220 = CARTESIAN_POINT ( 'NONE',  ( 67.77237640127140139, -32.48158740639239994, -19.08110272389540185 ) ) ;
#46221 = CARTESIAN_POINT ( 'NONE',  ( 18.12954728147380123, 19.89797661840560039, -74.34810712130391153 ) ) ;
#46222 = ORIENTED_EDGE ( 'NONE', *, *, #30670, .F. ) ;
#46223 = ORIENTED_EDGE ( 'NONE', *, *, #23634, .T. ) ;
#46224 = CARTESIAN_POINT ( 'NONE',  ( 48.17397874823690529, 23.07566552192859888, -55.30238548989590441 ) ) ;
#46225 = CARTESIAN_POINT ( 'NONE',  ( 76.55823188635187648, 0.1748944968071982631, -13.47834810069977962 ) ) ;
#46226 = ORIENTED_EDGE ( 'NONE', *, *, #20278, .T. ) ;
#46227 = CARTESIAN_POINT ( 'NONE',  ( 12.95205822670359908, -65.51487522867400060, -47.64438479393490411 ) ) ;
#46228 = CARTESIAN_POINT ( 'NONE',  ( 56.42422650276310492, -45.43209815878279301, -25.36438790313970060 ) ) ;
#46229 = CARTESIAN_POINT ( 'NONE',  ( 24.02198689557684474, -16.27232187956634490, -77.53406589020798378 ) ) ;
#46230 = CARTESIAN_POINT ( 'NONE',  ( 63.44018392888030178, 1.383811055320669947, -68.52712657046359368 ) ) ;
#46231 = ORIENTED_EDGE ( 'NONE', *, *, #12554, .T. ) ;
#46232 = AXIS2_PLACEMENT_3D ( 'NONE', #51029, #35025, #51547 ) ;
#46233 = DIRECTION ( 'NONE',  ( 0.8535492322835283030, 0.3460892239715681606, 0.3894559758418881801 ) ) ;
#46234 = CARTESIAN_POINT ( 'NONE',  ( 46.18989734099319122, 6.940418880791806799, -59.37015247182863220 ) ) ;
#46235 = CARTESIAN_POINT ( 'NONE',  ( -5.885796488028379514, 16.61635989263051627, -40.29953568053277024 ) ) ;
#46236 = ORIENTED_EDGE ( 'NONE', *, *, #10538, .F. ) ;
#46237 = EDGE_CURVE ( 'NONE', #29814, #20523, #4907, .T. ) ;
#46238 = CARTESIAN_POINT ( 'NONE',  ( 47.34305974329570432, -45.94041436994260152, -10.43357978122729968 ) ) ;
#46239 = CARTESIAN_POINT ( 'NONE',  ( 51.85727070035964203, 1.492828087247280999, -18.71161526954956500 ) ) ;
#46240 = CARTESIAN_POINT ( 'NONE',  ( 15.46269294852310061, 19.79576386060080040, -21.20027565686660154 ) ) ;
#46241 = EDGE_CURVE ( 'NONE', #679, #9344, #1578, .T. ) ;
#46242 = CARTESIAN_POINT ( 'NONE',  ( 16.13393739769599833, 14.38381105532070059, -35.14999999999999858 ) ) ;
#46243 = CARTESIAN_POINT ( 'NONE',  ( 16.30959015889229136, -22.38100858503597479, -46.94456242962048975 ) ) ;
#46244 = DIRECTION ( 'NONE',  ( 0.000000000000000000, 0.000000000000000000, 1.000000000000000000 ) ) ;
#46245 = CARTESIAN_POINT ( 'NONE',  ( 47.22775207516579599, -54.56828855535529499, -74.94674070344109396 ) ) ;
#46246 = CARTESIAN_POINT ( 'NONE',  ( 56.62345902695000177, 12.22720384556450135, -8.191343754504078589 ) ) ;
#46247 = DIRECTION ( 'NONE',  ( 0.000000000000000000, 0.000000000000000000, -1.000000000000000000 ) ) ;
#46248 = B_SPLINE_SURFACE_WITH_KNOTS ( 'NONE', 3, 3, ( 
 ( #7199, #23153, #35489, #31023, #39170, #27103, #19240, #35222 ),
 ( #7967, #51226, #31273, #43363, #15579, #39682, #31534, #19997 ),
 ( #35747, #41325, #2010, #44745, #9108, #29522, #21906, #9875 ),
 ( #21395, #13304, #9622, #20884, #25057, #45266, #25832, #5440 ),
 ( #21138, #41845, #49469, #48954, #37398, #33705, #41074, #49722 ),
 ( #13810, #1500, #32925, #29768, #979, #17737, #5948, #5187 ),
 ( #41583, #1242, #37917, #5694, #45786, #37652, #8850, #17485 ),
 ( #37145, #13056, #28746, #32657, #4911, #9379, #17231, #13560 ),
 ( #48688, #12788, #24800, #29264, #36879, #40811, #16979, #29009 ),
 ( #45005, #33191, #49211, #25322, #33449, #45527, #25578, #21647 ) ),
 .UNSPECIFIED., .F., .F., .F.,
 ( 4, 1, 1, 1, 1, 1, 1, 4 ),
 ( 4, 2, 2, 4 ),
 ( -3.286467431787650260E-05, 0.1428571428571430157, 0.2857142857142860315, 0.4285714285714289917, 0.5714285714285709528, 0.7142857142857139685, 0.8571428571428569843, 1.000000000000000000 ),
 ( -2.169191898319330125, -2.161509015541720036, -1.792610411306549967, -1.570647066508290113 ),
 .UNSPECIFIED. ) ;
#46249 = CARTESIAN_POINT ( 'NONE',  ( 52.01748107372789320, 19.87890217953579963, -76.09025191937530508 ) ) ;
#46250 = CARTESIAN_POINT ( 'NONE',  ( 61.50603079699979503, 13.91190901698290006, -28.03580912474989972 ) ) ;
#46251 = CARTESIAN_POINT ( 'NONE',  ( 10.13557796846099812, -10.55590907640169895, -78.51056856275729956 ) ) ;
#46252 = ORIENTED_EDGE ( 'NONE', *, *, #19706, .F. ) ;
#46253 = LINE ( 'NONE', #45725, #29686 ) ;
#46254 = CARTESIAN_POINT ( 'NONE',  ( 9.942311330327790131, -63.79309159654170003, -15.97126716329570151 ) ) ;
#46255 = DIRECTION ( 'NONE',  ( -1.000000000000000000, 0.000000000000000000, 0.000000000000000000 ) ) ;
#46256 = DIRECTION ( 'NONE',  ( -1.000000000000000000, 0.000000000000000000, 0.000000000000000000 ) ) ;
#46257 = PRODUCT_DEFINITION ( 'UNKNOWN', '', #35244, #35791 ) ;
#46258 = DIRECTION ( 'NONE',  ( 0.3294064756441091313, -0.9441882088883163382, 0.000000000000000000 ) ) ;
#46259 = CIRCLE ( 'NONE', #6935, 38.61618927352878217 ) ;
#46260 = B_SPLINE_CURVE_WITH_KNOTS ( 'NONE', 3,
 ( #42570, #14520, #19218, #26556, #15298, #48294, #20751, #844, #4782, #24148, #36738 ),
 .UNSPECIFIED., .F., .F.,
 ( 4, 1, 1, 1, 1, 1, 1, 1, 4 ),
 ( 0.000000000000000000, 0.1250003856707712080, 0.2500003305749467497, 0.3750002754791222914, 0.5000002203832978331, 0.6250001652874733749, 0.7500001101916489166, 0.8750000550958244583, 1.000000000000000000 ),
 .UNSPECIFIED. ) ;
#46261 = AXIS2_PLACEMENT_3D ( 'NONE', #2911, #23057, #51381 ) ;
#46262 = DIRECTION ( 'NONE',  ( 1.224648637339234427E-16, 1.000000000000000000, -6.470619327693536922E-12 ) ) ;
#46263 = CARTESIAN_POINT ( 'NONE',  ( 17.16942097546588641, -7.705179818260964097, -43.04929360077927925 ) ) ;
#46264 = DIRECTION ( 'NONE',  ( -0.7071067811865475727, 0.000000000000000000, 0.7071067811865475727 ) ) ;
#46265 = CARTESIAN_POINT ( 'NONE',  ( 42.33768682474920553, 11.92978350657940112, -3.566431340207619982 ) ) ;
#46266 = CARTESIAN_POINT ( 'NONE',  ( 9.221338892866903336, -11.63218626646301068, -58.95902533789330136 ) ) ;
#46267 = CARTESIAN_POINT ( 'NONE',  ( -18.86606260230360022, -50.61618894467959962, 16.21999999999999886 ) ) ;
#46268 = EDGE_CURVE ( 'NONE', #24662, #23989, #13179, .T. ) ;
#46269 = DIRECTION ( 'NONE',  ( 0.8732394366197182567, 0.4872913772396111343, 1.665334536937735304E-16 ) ) ;
#46270 = DIRECTION ( 'NONE',  ( 0.000000000000000000, -1.000000000000000000, 0.000000000000000000 ) ) ;
#46271 = ORIENTED_EDGE ( 'NONE', *, *, #32267, .T. ) ;
#46272 = EDGE_CURVE ( 'NONE', #727, #16578, #40889, .T. ) ;
#46273 = CARTESIAN_POINT ( 'NONE',  ( 11.03203224910719982, -10.18689265573519975, -58.32723503207409976 ) ) ;
#46274 = EDGE_CURVE ( 'NONE', #22043, #47824, #50966, .T. ) ;
#46275 = CARTESIAN_POINT ( 'NONE',  ( 63.54769155648281043, 1.017423949637539904, -61.78033243378509809 ) ) ;
#46276 = ORIENTED_EDGE ( 'NONE', *, *, #4303, .T. ) ;
#46277 = CARTESIAN_POINT ( 'NONE',  ( 0.5469381758899513057, -26.92474821800609064, -43.67210485577498957 ) ) ;
#46278 = DIRECTION ( 'NONE',  ( -1.000000000000000000, 0.000000000000000000, 0.000000000000000000 ) ) ;
#46279 = CARTESIAN_POINT ( 'NONE',  ( 8.133937397696209715, -59.33545798990849818, -21.14999999999999858 ) ) ;
#46280 = CARTESIAN_POINT ( 'NONE',  ( 16.62037960046279750, -23.51288716533397860, -61.98809266990242861 ) ) ;
#46281 = CARTESIAN_POINT ( 'NONE',  ( 22.90093739746964374, -14.73039726793156490, -74.41115356083933818 ) ) ;
#46282 = CARTESIAN_POINT ( 'NONE',  ( 9.187091958171290429, -16.78994149695390092, -81.23899999999999011 ) ) ;
#46283 = VERTEX_POINT ( 'NONE', #18954 ) ;
#46284 = ORIENTED_EDGE ( 'NONE', *, *, #46751, .T. ) ;
#46285 = ORIENTED_EDGE ( 'NONE', *, *, #21525, .T. ) ;
#46286 = CARTESIAN_POINT ( 'NONE',  ( -22.60072279458010058, -20.15755767129849829, -54.65015892017029842 ) ) ;
#46287 = CARTESIAN_POINT ( 'NONE',  ( 52.69317937239979699, -49.76927390646469718, -48.79657040945900803 ) ) ;
#46288 = CARTESIAN_POINT ( 'NONE',  ( 82.54524994490415679, -45.15149953693300944, -46.85688790748942978 ) ) ;
#46289 = ORIENTED_EDGE ( 'NONE', *, *, #11383, .F. ) ;
#46290 = B_SPLINE_CURVE_WITH_KNOTS ( 'NONE', 3,
 ( #32151, #48428, #12796, #32665, #16708, #40818, #27974, #43977, #20115, #48169, #8597, #44234, #36108, #8081, #8334, #24287, #4398, #20368, #12529, #28495, #24544, #4652, #20624, #4919, #20890, #15041, #50689, #2739, #18712, #43096, #38124, #42577, #14275, #13312, #18458 ),
 .UNSPECIFIED., .F., .F.,
 ( 4, 1, 1, 1, 2, 2, 2, 2, 1, 2, 2, 2, 1, 2, 2, 2, 2, 2, 2, 4 ),
 ( 0.000000000000000000, 0.06249999999973548936, 0.09374999999960900721, 0.1093749999995292238, 0.1171874999994964028, 0.1249999999994635680, 0.1874999999994682309, 0.2187499999994763356, 0.2343749999994887978, 0.2421874999994946820, 0.2499999999995005662, 0.3749999999996987410, 0.4374999999997912226, 0.4687499999998307465, 0.4999999999998703260, 0.6249999999999318323, 0.6874999999999624745, 0.7187499999999693578, 0.7499999999999762412, 1.000000000000000000 ),
 .UNSPECIFIED. ) ;
#46291 = EDGE_LOOP ( 'NONE', ( #13547, #20042, #40431, #46860 ) ) ;
#46292 = DIRECTION ( 'NONE',  ( 1.000000000000000000, -2.206290999999999941E-14, -3.490044999999999999E-12 ) ) ;
#46293 = CARTESIAN_POINT ( 'NONE',  ( 54.99091206896520134, -51.40428974184509769, -54.03945093368859887 ) ) ;
#46294 = ADVANCED_FACE ( 'NONE', ( #23130 ), #15029, .T. ) ;
#46295 = CARTESIAN_POINT ( 'NONE',  ( 21.54527723138343731, -11.45754348139197987, -54.24448937358901901 ) ) ;
#46296 = ORIENTED_EDGE ( 'NONE', *, *, #28364, .F. ) ;
#46297 = CARTESIAN_POINT ( 'NONE',  ( 9.366937397696199596, -15.61618894467949836, -28.45282021618999835 ) ) ;
#46299 = CARTESIAN_POINT ( 'NONE',  ( 53.07814503768779701, -50.87410907760390444, -76.24016814631330874 ) ) ;
#46298 = VECTOR ( 'NONE', #48408, 1000.000000000000000 ) ;
#46300 = CARTESIAN_POINT ( 'NONE',  ( 60.61844477880759996, 14.36317300640260086, -47.31023525542560293 ) ) ;
#46301 = CARTESIAN_POINT ( 'NONE',  ( 12.93456956912729972, -8.450242176170609909, -73.37883193416179495 ) ) ;
#46302 = LINE ( 'NONE', #5940, #45627 ) ;
#46303 = CARTESIAN_POINT ( 'NONE',  ( 43.71660380195360318, 13.90300536042119894, -6.831405570051200193 ) ) ;
#46304 = CARTESIAN_POINT ( 'NONE',  ( 42.63139189943180440, -42.85457206599819813, -3.312314667595840589 ) ) ;
#46305 = DIRECTION ( 'NONE',  ( 0.000000000000000000, -1.000000000000000000, 0.000000000000000000 ) ) ;
#46306 = FACE_OUTER_BOUND ( 'NONE', #50912, .T. ) ;
#46307 = CARTESIAN_POINT ( 'NONE',  ( 64.19260248505071331, 1.000485720979669813, -70.17481423849029909 ) ) ;
#46308 = DIRECTION ( 'NONE',  ( 0.000000000000000000, 0.7071067811865463515, -0.7071067811865487940 ) ) ;
#46309 = DIRECTION ( 'NONE',  ( 0.000000000000000000, -1.000000000000000000, 0.000000000000000000 ) ) ;
#46310 = CARTESIAN_POINT ( 'NONE',  ( 22.93787291984029864, -11.70553559853770054, -57.12145717557999802 ) ) ;
#46311 = VERTEX_POINT ( 'NONE', #31245 ) ;
#46312 = CARTESIAN_POINT ( 'NONE',  ( 14.48354644325280027, -52.62916658892859800, -76.03098605356829864 ) ) ;
#46313 = CIRCLE ( 'NONE', #1103, 5.999999999999998224 ) ;
#46314 = CARTESIAN_POINT ( 'NONE',  ( 57.38765468553089732, 19.36030170222889879, -53.60535509370559737 ) ) ;
#46315 = CARTESIAN_POINT ( 'NONE',  ( 44.73969310392494947, -40.01199137491765612, -63.07507009560972477 ) ) ;
#46316 = CARTESIAN_POINT ( 'NONE',  ( 11.36895923993938951, 33.23916916631637974, -44.41074867393047043 ) ) ;
#46317 = CARTESIAN_POINT ( 'NONE',  ( 47.13698192568809731, -54.70277146169920712, -74.81178025453719727 ) ) ;
#46318 = CARTESIAN_POINT ( 'NONE',  ( 63.52011431889719972, 1.391252479931859964, -68.77264296518760034 ) ) ;
#46319 = FACE_OUTER_BOUND ( 'NONE', #31586, .T. ) ;
#46320 = EDGE_CURVE ( 'NONE', #39256, #11348, #13183, .T. ) ;
#46321 = LINE ( 'NONE', #50760, #17550 ) ;
#46322 = CARTESIAN_POINT ( 'NONE',  ( 20.99559369598925329, -21.94237153941632457, -46.08404182597173104 ) ) ;
#46323 = CARTESIAN_POINT ( 'NONE',  ( 47.79465657660569633, 23.23647380393689943, -55.14967471148109723 ) ) ;
#46324 = EDGE_LOOP ( 'NONE', ( #48275, #39902, #32594, #39186, #23464 ) ) ;
#46325 = EDGE_CURVE ( 'NONE', #41111, #6409, #28089, .T. ) ;
#46326 = AXIS2_PLACEMENT_3D ( 'NONE', #33148, #32617, #939 ) ;
#46327 = CARTESIAN_POINT ( 'NONE',  ( 16.56130706594500168, -8.576308665788749508, -72.36647972087459380 ) ) ;
#46328 = ADVANCED_FACE ( 'NONE', ( #24923 ), #49990, .T. ) ;
#46329 = AXIS2_PLACEMENT_3D ( 'NONE', #35825, #11991, #11480 ) ;
#46330 = ORIENTED_EDGE ( 'NONE', *, *, #30602, .T. ) ;
#46331 = CARTESIAN_POINT ( 'NONE',  ( 71.34424925767550008, 1.265401080857980087, -70.52378931128949091 ) ) ;
#46332 = CIRCLE ( 'NONE', #45462, 6.766999999999998572 ) ;
#46333 = CARTESIAN_POINT ( 'NONE',  ( 17.63393739769629676, -7.616188944679219475, -35.14999999999999858 ) ) ;
#46334 = CARTESIAN_POINT ( 'NONE',  ( 16.13393739769620083, -15.61618894467929941, -76.14999999999999147 ) ) ;
#46335 = CARTESIAN_POINT ( 'NONE',  ( 24.04523903120960782, -15.61618918343368101, -41.50766953063602926 ) ) ;
#46337 = CARTESIAN_POINT ( 'NONE',  ( 54.86175021155899856, 16.01064883855890031, -25.75780955478559875 ) ) ;
#46336 = CARTESIAN_POINT ( 'NONE',  ( 83.33882225295539570, 13.76147914917100046, -47.09476873026769539 ) ) ;
#46338 = CARTESIAN_POINT ( 'NONE',  ( 22.53697538243309850, -12.65922166745750133, -80.31511008668059048 ) ) ;
#46340 = EDGE_CURVE ( 'NONE', #8663, #31804, #19465, .T. ) ;
#46339 = CARTESIAN_POINT ( 'NONE',  ( -0.4123484725610440105, -45.29119327467250145, -35.12503119152799513 ) ) ;
#46341 = CARTESIAN_POINT ( 'NONE',  ( 9.221472552717655091, -19.60042002319641341, -42.34100161347219426 ) ) ;
#46342 = CARTESIAN_POINT ( 'NONE',  ( 22.55531716423215016, -17.79663242155549696, -40.55696725089184440 ) ) ;
#46343 = ORIENTED_EDGE ( 'NONE', *, *, #22315, .F. ) ;
#46344 = DIRECTION ( 'NONE',  ( 1.000000000000000000, 0.000000000000000000, 0.000000000000000000 ) ) ;
#46345 = VERTEX_POINT ( 'NONE', #49595 ) ;
#46346 = ORIENTED_EDGE ( 'NONE', *, *, #46212, .T. ) ;
#46347 = FACE_OUTER_BOUND ( 'NONE', #46913, .T. ) ;
#46348 = CARTESIAN_POINT ( 'NONE',  ( 24.04334890807969316, -15.44487692207048823, -39.50078007227123322 ) ) ;
#46349 = CARTESIAN_POINT ( 'NONE',  ( -12.74484839417802640, 25.82459822544487693, -53.24848714985387943 ) ) ;
#46350 = DIRECTION ( 'NONE',  ( 1.000000000000000000, 0.000000000000000000, 0.000000000000000000 ) ) ;
#46351 = ORIENTED_EDGE ( 'NONE', *, *, #14117, .T. ) ;
#46352 = ORIENTED_EDGE ( 'NONE', *, *, #23410, .F. ) ;
#46353 = CARTESIAN_POINT ( 'NONE',  ( -3.783936937370389941, -48.92741940384860300, -38.05596390819669494 ) ) ;
#46354 = CARTESIAN_POINT ( 'NONE',  ( 64.93393739769740591, 11.38381105532059934, -69.34999999999999432 ) ) ;
#46355 = AXIS2_PLACEMENT_3D ( 'NONE', #24302, #51605, #31654 ) ;
#46356 = CARTESIAN_POINT ( 'NONE',  ( 9.813805456378791092, -13.11177490670652013, -45.57283591714075044 ) ) ;
#46357 = CARTESIAN_POINT ( 'NONE',  ( 62.46918019396079558, -1.552292481998720053, -16.13637721537210012 ) ) ;
#46358 = ADVANCED_FACE ( 'NONE', ( #41196 ), #5815, .F. ) ;
#46359 = CARTESIAN_POINT ( 'NONE',  ( 51.12155915768349246, -49.71343516829359999, -76.32652955267910500 ) ) ;
#46360 = CARTESIAN_POINT ( 'NONE',  ( 57.85642988081749394, -49.00357350458359917, -51.22892263933690060 ) ) ;
#46361 = ORIENTED_EDGE ( 'NONE', *, *, #268, .T. ) ;
#46362 = CARTESIAN_POINT ( 'NONE',  ( 14.83305478682455281, -7.784683102609005978, -33.23989205926810087 ) ) ;
#46363 = CARTESIAN_POINT ( 'NONE',  ( 68.13393739769706769, 17.98087126524919555, -68.79648330188412331 ) ) ;
#46364 = ORIENTED_EDGE ( 'NONE', *, *, #29327, .F. ) ;
#46365 = DIRECTION ( 'NONE',  ( 1.000000000000000000, 0.000000000000000000, 0.000000000000000000 ) ) ;
#46366 = CARTESIAN_POINT ( 'NONE',  ( 46.60731581406910351, -45.11618894467940066, -7.962945791737540802 ) ) ;
#46367 = CARTESIAN_POINT ( 'NONE',  ( 18.08605090678410221, -8.015136357095210329, -43.59251385424099823 ) ) ;
#46368 = CARTESIAN_POINT ( 'NONE',  ( 12.86000738318819892, -50.64304082809789520, -21.34825274859070277 ) ) ;
#46369 = CARTESIAN_POINT ( 'NONE',  ( 56.66430192519659670, 19.40095727286280081, -75.08551389032560053 ) ) ;
#46370 = TOROIDAL_SURFACE ( 'NONE', #1159, 2.500000000000000000, 0.5000000000000000000 ) ;
#46371 = CARTESIAN_POINT ( 'NONE',  ( 46.42817262113109678, -53.00400577820990122, -76.14999999999999147 ) ) ;
#46372 = CARTESIAN_POINT ( 'NONE',  ( 56.98602282140059572, 13.94694871494499999, -17.93020696514379964 ) ) ;
#46373 = CARTESIAN_POINT ( 'NONE',  ( 22.04685577009000852, -12.20821031989865979, -78.28615093498937938 ) ) ;
#46374 = AXIS2_PLACEMENT_3D ( 'NONE', #8661, #37474, #24616 ) ;
#46375 = CARTESIAN_POINT ( 'NONE',  ( 56.87927062415320023, -50.65046521877609820, -53.72034555678590806 ) ) ;
#46376 = AXIS2_PLACEMENT_3D ( 'NONE', #49193, #13287, #20595 ) ;
#46377 = EDGE_CURVE ( 'NONE', #44083, #43986, #5306, .T. ) ;
#46378 = CARTESIAN_POINT ( 'NONE',  ( 22.21314585784340068, -19.19191036455050181, -47.01642178051650234 ) ) ;
#46379 = CARTESIAN_POINT ( 'NONE',  ( 13.13393739769615820, -49.61618894467929408, -35.01561944896765510 ) ) ;
#46380 = ORIENTED_EDGE ( 'NONE', *, *, #8618, .F. ) ;
#46381 = EDGE_CURVE ( 'NONE', #31681, #29113, #21302, .T. ) ;
#46382 = CARTESIAN_POINT ( 'NONE',  ( 46.61291010390670664, 22.01119584692700215, -76.11300884098571373 ) ) ;
#46383 = CARTESIAN_POINT ( 'NONE',  ( 20.01239153654114133, -55.06729567945755832, -18.78855326316173091 ) ) ;
#46384 = CARTESIAN_POINT ( 'NONE',  ( 60.91959772890204050, -45.69583638042096396, -47.74153617882512179 ) ) ;
#46385 = CARTESIAN_POINT ( 'NONE',  ( 104.6856170952499951, -2.032350560839819131, -29.09832030244561807 ) ) ;
#46386 = DIRECTION ( 'NONE',  ( -1.000000000000000000, 0.000000000000000000, 0.000000000000000000 ) ) ;
#46387 = CARTESIAN_POINT ( 'NONE',  ( 82.57811023567160191, 13.96421234425040048, -47.00700744241340345 ) ) ;
#46388 = CIRCLE ( 'NONE', #48029, 10.00000000000000711 ) ;
#46389 = CARTESIAN_POINT ( 'NONE',  ( -21.03465488720650001, -4.042464877597000239, -53.05748812964859695 ) ) ;
#46391 = CARTESIAN_POINT ( 'NONE',  ( 56.92451318172422248, -22.90031634167878494, -41.48442968688959098 ) ) ;
#46390 = CARTESIAN_POINT ( 'NONE',  ( 47.64143405400680109, 23.30250925609140111, -74.14999999999999147 ) ) ;
#46392 = FACE_OUTER_BOUND ( 'NONE', #40569, .T. ) ;
#46393 = CARTESIAN_POINT ( 'NONE',  ( -17.64362745039410285, 19.90889109872690099, -52.54414402675289608 ) ) ;
#46394 = EDGE_LOOP ( 'NONE', ( #36777, #8105, #25833, #28851 ) ) ;
#46395 = EDGE_CURVE ( 'NONE', #19952, #50462, #25781, .T. ) ;
#46396 = CARTESIAN_POINT ( 'NONE',  ( 52.90334279678310736, -49.62746727120449464, -48.83356295429710059 ) ) ;
#46397 = ORIENTED_EDGE ( 'NONE', *, *, #51417, .F. ) ;
#46398 = CARTESIAN_POINT ( 'NONE',  ( 17.68281250479444111, 20.56215755416158686, -75.65677362358465530 ) ) ;
#46399 = CARTESIAN_POINT ( 'NONE',  ( 22.90093740771515840, -14.73039777584664201, -42.41115299789638726 ) ) ;
#46400 = CARTESIAN_POINT ( 'NONE',  ( 13.68007976385719893, 20.13478144958939708, -22.99347874021080074 ) ) ;
#46401 = CARTESIAN_POINT ( 'NONE',  ( 55.83218870901129804, 14.79097304268890056, -25.40764975850709817 ) ) ;
#46402 = CARTESIAN_POINT ( 'NONE',  ( 22.87897769365210010, -17.67701162083490019, -40.54720669274369982 ) ) ;
#46403 = CARTESIAN_POINT ( 'NONE',  ( 51.02818947082010226, 19.65064782392149567, -76.14999999999999147 ) ) ;
#46405 = EDGE_CURVE ( 'NONE', #29490, #48087, #10838, .T. ) ;
#46404 = CARTESIAN_POINT ( 'NONE',  ( 52.59812796910519950, 18.59560619956539895, -48.49245696013879581 ) ) ;
#46406 = CARTESIAN_POINT ( 'NONE',  ( 55.68556815085590017, -45.89590543237220288, -16.87789993209419848 ) ) ;
#46407 = CARTESIAN_POINT ( 'NONE',  ( 16.13393739769620083, -15.61618894467929941, -18.35000000000000142 ) ) ;
#46408 = EDGE_LOOP ( 'NONE', ( #35769, #16104, #6968, #20786, #49445, #32481 ) ) ;
#46409 = CARTESIAN_POINT ( 'NONE',  ( 19.75483718735349825, -8.653730120499389500, -34.94015647776650013 ) ) ;
#46410 = CARTESIAN_POINT ( 'NONE',  ( 72.72759757326660690, 1.395196698723390138, -68.83033655198650536 ) ) ;
#46411 = CARTESIAN_POINT ( 'NONE',  ( 10.60681015439949881, 33.67700033712320362, -47.04781549457079848 ) ) ;
#46412 = CARTESIAN_POINT ( 'NONE',  ( 72.78816252330430814, 1.385888765344509999, -62.64792042614379852 ) ) ;
#46413 = CARTESIAN_POINT ( 'NONE',  ( 10.85466640526500015, -64.96697012889119094, -17.55961383757770022 ) ) ;
#46414 = CARTESIAN_POINT ( 'NONE',  ( 53.23850466849069818, -49.52901910977941924, -49.17578823945778765 ) ) ;
#46415 = DIRECTION ( 'NONE',  ( 0.000000000000000000, -1.000000000000000000, 0.000000000000000000 ) ) ;
#46416 = CARTESIAN_POINT ( 'NONE',  ( 9.221435075809175430, -11.63202193102039494, -44.95897662767622904 ) ) ;
#46417 = CARTESIAN_POINT ( 'NONE',  ( 11.97539275157860850, -10.20477305846235794, -57.74448680029835401 ) ) ;
#46418 = ORIENTED_EDGE ( 'NONE', *, *, #43237, .T. ) ;
#46419 = CARTESIAN_POINT ( 'NONE',  ( 65.00323391584400667, 1.328073773609210084, -70.46779242537471077 ) ) ;
#46420 = ORIENTED_EDGE ( 'NONE', *, *, #39457, .F. ) ;
#46421 = CARTESIAN_POINT ( 'NONE',  ( 10.13631591262990028, -63.14180753440869154, -45.99667195303850065 ) ) ;
#46422 = CARTESIAN_POINT ( 'NONE',  ( 22.94861535714161249, -15.61996792560115388, -32.45282170169829783 ) ) ;
#46423 = VERTEX_POINT ( 'NONE', #45648 ) ;
#46424 = FACE_OUTER_BOUND ( 'NONE', #21648, .T. ) ;
#46425 = CARTESIAN_POINT ( 'NONE',  ( 57.03107157439150399, 18.99627872735710099, -52.68131390763750233 ) ) ;
#46426 = VECTOR ( 'NONE', #27958, 1000.000000000000000 ) ;
#46427 = CARTESIAN_POINT ( 'NONE',  ( 52.97782966775210411, 19.06886046639999677, -77.23919107660618977 ) ) ;
#46428 = VERTEX_POINT ( 'NONE', #29892 ) ;
#46429 = FACE_BOUND ( 'NONE', #50374, .T. ) ;
#46430 = CARTESIAN_POINT ( 'NONE',  ( 47.60722588394173727, -45.76208697842935891, 17.35000000000000142 ) ) ;
#46431 = CARTESIAN_POINT ( 'NONE',  ( 14.55219274796575313, 20.46959765477225091, -75.56421372419544014 ) ) ;
#46432 = CARTESIAN_POINT ( 'NONE',  ( 9.807738766467371860, -10.75455377863122131, -69.00066549479555533 ) ) ;
#46433 = CARTESIAN_POINT ( 'NONE',  ( 23.13768727496389843, -19.96707479845759892, -63.96927302813099203 ) ) ;
#46434 = DIRECTION ( 'NONE',  ( 1.000000000000000000, 0.000000000000000000, 0.000000000000000000 ) ) ;
#46435 = CARTESIAN_POINT ( 'NONE',  ( 44.64515780931174760, -37.99980088791255639, -67.09384305938301907 ) ) ;
#46436 = ORIENTED_EDGE ( 'NONE', *, *, #10725, .T. ) ;
#46437 = CARTESIAN_POINT ( 'NONE',  ( -22.60067283610179700, -11.07416626356550005, -54.64998264227110525 ) ) ;
#46438 = CARTESIAN_POINT ( 'NONE',  ( 8.765544488224740860, -14.51460838167160006, -57.27989503770729840 ) ) ;
#46439 = CARTESIAN_POINT ( 'NONE',  ( 53.02879952360030558, -49.61047114518110135, -49.09530619433559906 ) ) ;
#46440 = EDGE_CURVE ( 'NONE', #40276, #37478, #37556, .T. ) ;
#46441 = CARTESIAN_POINT ( 'NONE',  ( 10.66075870651240010, -11.36616899821419935, -32.14999999999999858 ) ) ;
#46442 = CIRCLE ( 'NONE', #35528, 33.00000000000000000 ) ;
#46443 = ADVANCED_FACE ( 'NONE', ( #30162 ), #17611, .T. ) ;
#46444 = DIRECTION ( 'NONE',  ( 0.000000000000000000, 0.000000000000000000, -1.000000000000000000 ) ) ;
#46445 = CIRCLE ( 'NONE', #6250, 6.999999999999999112 ) ;
#46446 = CARTESIAN_POINT ( 'NONE',  ( 14.35303864406479946, 20.08140804309819671, -75.03330975078259257 ) ) ;
#46447 = EDGE_CURVE ( 'NONE', #32778, #44695, #34390, .T. ) ;
#46448 = DIRECTION ( 'NONE',  ( 0.000000000000000000, 0.000000000000000000, -1.000000000000000000 ) ) ;
#46449 = CARTESIAN_POINT ( 'NONE',  ( 41.59982226866920030, -45.03802502177139644, -5.840267740712650202 ) ) ;
#46450 = DIRECTION ( 'NONE',  ( 1.000000000000000000, 2.460964292799963328E-14, 0.000000000000000000 ) ) ;
#46451 = CARTESIAN_POINT ( 'NONE',  ( 7.910943552303420390, -15.01195974345870177, -66.53101608161080094 ) ) ;
#46452 = VERTEX_POINT ( 'NONE', #24271 ) ;
#46453 = CARTESIAN_POINT ( 'NONE',  ( 53.95391475063919984, -48.32190372696410208, -26.18290555829409882 ) ) ;
#46454 = CARTESIAN_POINT ( 'NONE',  ( 56.18713067680260309, -50.81645256829099822, -74.69754235492649741 ) ) ;
#46456 = CARTESIAN_POINT ( 'NONE',  ( 41.86582274391710001, -39.74996327333580837, -76.97917529163896688 ) ) ;
#46455 = CARTESIAN_POINT ( 'NONE',  ( 10.89817501250260179, 33.55262736970569648, -16.84305400789989804 ) ) ;
#46457 = DIRECTION ( 'NONE',  ( 0.000000000000000000, 0.000000000000000000, 1.000000000000000000 ) ) ;
#46458 = CARTESIAN_POINT ( 'NONE',  ( 52.56521937542130019, 18.62941943741099848, -48.47378147059570352 ) ) ;
#46459 = ORIENTED_EDGE ( 'NONE', *, *, #40619, .T. ) ;
#46460 = CARTESIAN_POINT ( 'NONE',  ( 13.58441918655680247, -8.089074747756592743, -80.90380639364062176 ) ) ;
#46461 = CARTESIAN_POINT ( 'NONE',  ( 47.52047993193150432, 23.35084913806530338, -54.81408765803269745 ) ) ;
#46462 = CARTESIAN_POINT ( 'NONE',  ( -18.86606260230390220, 19.38381105532060289, 10.84999999999999964 ) ) ;
#46463 = LINE ( 'NONE', #42524, #15118 ) ;
#46464 = CARTESIAN_POINT ( 'NONE',  ( 57.25554329372283036, 13.89079948346292426, -25.31272176079182046 ) ) ;
#46465 = CARTESIAN_POINT ( 'NONE',  ( 12.01336145399789856, 34.10065735964469269, -17.10865966561200224 ) ) ;
#46466 = CARTESIAN_POINT ( 'NONE',  ( 51.75737834632590051, 17.97862913216729908, -76.97426711872269323 ) ) ;
#46468 = ADVANCED_FACE ( 'NONE', ( #14704 ), #7365, .T. ) ;
#46467 = CARTESIAN_POINT ( 'NONE',  ( 52.84702947235859938, 18.41949267415209945, -48.63861689686890344 ) ) ;
#46469 = CARTESIAN_POINT ( 'NONE',  ( 28.13393739769619728, -8.687985714403851034, -35.14999999999999858 ) ) ;
#46470 = CYLINDRICAL_SURFACE ( 'NONE', #50180, 5.499999999999998224 ) ;
#46471 = CARTESIAN_POINT ( 'NONE',  ( 54.62137568764190121, 16.83476236174520224, -26.74064760761449833 ) ) ;
#46472 = AXIS2_PLACEMENT_3D ( 'NONE', #507, #48475, #23306 ) ;
#46473 = CARTESIAN_POINT ( 'NONE',  ( 50.22318599631050517, 21.91893947206089877, -53.94766427587659763 ) ) ;
#46474 = CARTESIAN_POINT ( 'NONE',  ( 8.223596773276058869, -15.61622589296290009, -36.79233150823699816 ) ) ;
#46475 = CARTESIAN_POINT ( 'NONE',  ( 12.12757547495970023, -65.18777574590600921, -16.69244762554430039 ) ) ;
#46476 = CARTESIAN_POINT ( 'NONE',  ( 9.221395147010715831, -19.60028769851233932, -76.34101524102744918 ) ) ;
#46477 = CARTESIAN_POINT ( 'NONE',  ( 71.09473187122610227, 1.382830464309369844, -60.94559068149789738 ) ) ;
#46478 = CARTESIAN_POINT ( 'NONE',  ( 10.49497832658790131, 32.13626875971579722, -45.62743361653370044 ) ) ;
#46479 = FACE_OUTER_BOUND ( 'NONE', #17262, .T. ) ;
#46480 = CARTESIAN_POINT ( 'NONE',  ( 65.88232195992709705, -31.40292976940219916, -17.13915762891529937 ) ) ;
#46481 = CARTESIAN_POINT ( 'NONE',  ( 12.55379742719071423, 24.22322520218094510, -75.36448431259415770 ) ) ;
#46482 = VERTEX_POINT ( 'NONE', #4384 ) ;
#46483 = ORIENTED_EDGE ( 'NONE', *, *, #50213, .F. ) ;
#46484 = CARTESIAN_POINT ( 'NONE',  ( 22.90101955563642733, -15.61618902498797290, -36.84717743668400658 ) ) ;
#46485 = CARTESIAN_POINT ( 'NONE',  ( 76.64291727984071656, 3.898797979677915748, -13.84327006523654724 ) ) ;
#46486 = VERTEX_POINT ( 'NONE', #23310 ) ;
#46487 = CARTESIAN_POINT ( 'NONE',  ( 13.00893739769619906, -65.51843714052719747, -47.75434321273180416 ) ) ;
#46488 = CARTESIAN_POINT ( 'NONE',  ( 56.06952239910840063, -46.00521685138409822, -25.91862699754300081 ) ) ;
#46489 = CARTESIAN_POINT ( 'NONE',  ( 19.54191425816137340, -21.52910907363614967, -44.78617089442926158 ) ) ;
#46490 = DIRECTION ( 'NONE',  ( 1.000000000000000000, 0.000000000000000000, 0.000000000000000000 ) ) ;
#46491 = CARTESIAN_POINT ( 'NONE',  ( 68.13393739769618662, -1.166188944679350081, -65.65000000000000568 ) ) ;
#46492 = ORIENTED_EDGE ( 'NONE', *, *, #26165, .T. ) ;
#46493 = CARTESIAN_POINT ( 'NONE',  ( -0.007164427059776000244, -45.70803162167019451, -34.77269723891829756 ) ) ;
#46494 = CARTESIAN_POINT ( 'NONE',  ( 46.82606541379494303, 7.001739961803058243, -56.18931106192717095 ) ) ;
#46495 = CARTESIAN_POINT ( 'NONE',  ( 11.81052567943170040, 33.80623951028800178, -23.83776314781059824 ) ) ;
#46496 = EDGE_LOOP ( 'NONE', ( #980, #5813, #43571, #18813 ) ) ;
#46497 = CARTESIAN_POINT ( 'NONE',  ( 14.86813092202610065, -23.76360903163029903, -34.34139281033739621 ) ) ;
#46498 = LINE ( 'NONE', #10589, #1223 ) ;
#46499 = CARTESIAN_POINT ( 'NONE',  ( 15.49194271727560057, 19.88381105247059821, -21.93290768619809938 ) ) ;
#46500 = DIRECTION ( 'NONE',  ( 0.000000000000000000, 0.000000000000000000, -1.000000000000000000 ) ) ;
#46501 = CARTESIAN_POINT ( 'NONE',  ( 22.90093739753756807, -15.61847319962781455, -46.45292522842559890 ) ) ;
#46502 =( BOUNDED_CURVE ( )  B_SPLINE_CURVE ( 3, ( #16957, #20596, #9088, #1222 ),
 .UNSPECIFIED., .F., .T. ) 
 B_SPLINE_CURVE_WITH_KNOTS ( ( 4, 4 ),
 ( 5.387239059105120020, 5.497787143782099761 ),
 .UNSPECIFIED. ) 
 CURVE ( )  GEOMETRIC_REPRESENTATION_ITEM ( )  RATIONAL_B_SPLINE_CURVE ( ( 1.000000000000000000, 0.9989818526761096162, 0.9989818526761096162, 1.000000000000000000 ) ) 
 REPRESENTATION_ITEM ( '' )  );
#46503 = CARTESIAN_POINT ( 'NONE',  ( 73.07318775143950518, 0.8986939045430389905, -69.05651959838648679 ) ) ;
#46504 = CARTESIAN_POINT ( 'NONE',  ( 47.17277128744060377, -54.46428745205209765, -75.17211772295890171 ) ) ;
#46505 = CARTESIAN_POINT ( 'NONE',  ( 52.41232212662860235, 12.25270176512410103, -7.106922988313540301 ) ) ;
#46506 = CONICAL_SURFACE ( 'NONE', #37273, 0.6299999999999942313, 0.7853981633974476129 ) ;
#46507 = AXIS2_PLACEMENT_3D ( 'NONE', #8136, #45587, #45851 ) ;
#46508 = ADVANCED_FACE ( 'NONE', ( #46699 ), #11301, .T. ) ;
#46509 = CARTESIAN_POINT ( 'NONE',  ( 55.90187131499349960, 19.50246216333230009, -52.91463811749139978 ) ) ;
#46510 = CARTESIAN_POINT ( 'NONE',  ( 53.62559109437130189, 20.09832781307389737, -75.58097986859370110 ) ) ;
#46511 = CARTESIAN_POINT ( 'NONE',  ( 16.13393739769639623, 7.383811055320659733, -59.64999999999999147 ) ) ;
#46512 = CARTESIAN_POINT ( 'NONE',  ( 14.69232761031780043, -7.902001992735149472, -80.72869863253859535 ) ) ;
#46513 = VERTEX_POINT ( 'NONE', #10527 ) ;
#46514 = CARTESIAN_POINT ( 'NONE',  ( 53.59007319875249920, 18.17385789302069554, -49.22505640236219904 ) ) ;
#46515 = AXIS2_PLACEMENT_3D ( 'NONE', #39987, #15370, #3058 ) ;
#46516 = CARTESIAN_POINT ( 'NONE',  ( 5.758794882113630109, -59.74571218704659969, -13.93823224276430039 ) ) ;
#46517 = CARTESIAN_POINT ( 'NONE',  ( 76.80246720768819557, 9.534583119364619108, -14.53080372693380085 ) ) ;
#46518 = FACE_OUTER_BOUND ( 'NONE', #23049, .T. ) ;
#46519 = DIRECTION ( 'NONE',  ( 1.000000000000000000, 2.460964292799963328E-14, 0.000000000000000000 ) ) ;
#46520 = ADVANCED_FACE ( 'NONE', ( #50612 ), #22551, .T. ) ;
#46521 = CARTESIAN_POINT ( 'NONE',  ( 72.33393739769618946, 1.883811055320669947, -62.44999999999999574 ) ) ;
#46522 = LINE ( 'NONE', #22375, #48254 ) ;
#46523 = CARTESIAN_POINT ( 'NONE',  ( 82.13853704237929776, -45.14107598135520050, -46.70066698695239893 ) ) ;
#46524 = LINE ( 'NONE', #1254, #36513 ) ;
#46525 = CARTESIAN_POINT ( 'NONE',  ( 42.87450601175959974, 11.54281269022849798, -3.882344406277799642 ) ) ;
#46527 = EDGE_CURVE ( 'NONE', #31811, #13386, #47262, .T. ) ;
#46526 = CARTESIAN_POINT ( 'NONE',  ( 47.57068389241495510, -54.44477986412701398, -74.81178025424496525 ) ) ;
#46528 = CARTESIAN_POINT ( 'NONE',  ( 68.13393739769618662, -30.31618894467939995, -65.65000000000000568 ) ) ;
#46529 = CARTESIAN_POINT ( 'NONE',  ( 70.03247032090770574, -49.95860450174030376, -73.25000000000169109 ) ) ;
#46530 = CARTESIAN_POINT ( 'NONE',  ( 76.23482020618884292, -43.29050810403887795, -13.80236124015438826 ) ) ;
#46531 = CARTESIAN_POINT ( 'NONE',  ( 18.05524586885999838, -51.28949470891399898, -74.96248001586319276 ) ) ;
#46532 = EDGE_CURVE ( 'NONE', #9610, #10111, #10000, .T. ) ;
#46533 = CARTESIAN_POINT ( 'NONE',  ( 58.33770897141780409, -45.11618894467940066, -10.68148127205489928 ) ) ;
#46534 = ORIENTED_EDGE ( 'NONE', *, *, #9099, .T. ) ;
#46535 = CARTESIAN_POINT ( 'NONE',  ( 8.747686520039062330, -14.64151345475930022, -56.10910496229269739 ) ) ;
#46536 = CARTESIAN_POINT ( 'NONE',  ( 63.86141673131270835, 1.061268603384970088, -61.43724097146670005 ) ) ;
#46537 = ORIENTED_EDGE ( 'NONE', *, *, #30428, .F. ) ;
#46538 = CARTESIAN_POINT ( 'NONE',  ( 17.21347160910339724, 21.88381105532300097, -76.14999999999999147 ) ) ;
#46539 = FACE_BOUND ( 'NONE', #7413, .T. ) ;
#46540 = CARTESIAN_POINT ( 'NONE',  ( 22.90076005816202809, -15.61619656631699193, -74.84717351858182610 ) ) ;
#46541 = CARTESIAN_POINT ( 'NONE',  ( 7.635415421591210894, -60.86027260432054931, -20.56421356237310150 ) ) ;
#46542 = VECTOR ( 'NONE', #49215, 1000.000000000000114 ) ;
#46543 = DIRECTION ( 'NONE',  ( -1.000000000000000000, 0.000000000000000000, 0.000000000000000000 ) ) ;
#46544 = CARTESIAN_POINT ( 'NONE',  ( 43.05622625292409822, -45.98099562716309663, -7.622810454742059427 ) ) ;
#46545 = VERTEX_POINT ( 'NONE', #26483 ) ;
#46546 = AXIS2_PLACEMENT_3D ( 'NONE', #28233, #15174, #35070 ) ;
#46547 = ORIENTED_EDGE ( 'NONE', *, *, #10779, .F. ) ;
#46548 = ORIENTED_EDGE ( 'NONE', *, *, #16617, .F. ) ;
#46549 = CARTESIAN_POINT ( 'NONE',  ( 57.50723796702470025, -45.11618894467940066, -17.68293338560010142 ) ) ;
#46550 = CARTESIAN_POINT ( 'NONE',  ( 61.29995204656449914, -45.28261984157529696, -47.06184258649409458 ) ) ;
#46551 = CARTESIAN_POINT ( 'NONE',  ( 52.56521993351449851, 18.62941884369810097, -48.47378146976069502 ) ) ;
#46552 = ORIENTED_EDGE ( 'NONE', *, *, #34203, .F. ) ;
#46553 = ORIENTED_EDGE ( 'NONE', *, *, #37984, .T. ) ;
#46554 = CARTESIAN_POINT ( 'NONE',  ( 16.13393739769620083, -15.61618894467929941, -18.35000000000000142 ) ) ;
#46555 = CARTESIAN_POINT ( 'NONE',  ( 45.32648691190289725, -33.86100112340690771, -34.65030537679119504 ) ) ;
#46556 = EDGE_LOOP ( 'NONE', ( #25816, #41375, #47088, #38785 ) ) ;
#46557 = CARTESIAN_POINT ( 'NONE',  ( 46.25525774125583922, -33.99486860111965569, -54.56299356781535437 ) ) ;
#46558 = CARTESIAN_POINT ( 'NONE',  ( 51.76047954393799699, -51.31561834827489577, -76.04144536748918881 ) ) ;
#46559 = CARTESIAN_POINT ( 'NONE',  ( 60.23362534523680267, 14.54944813804890025, -47.26357634580340061 ) ) ;
#46560 = AXIS2_PLACEMENT_3D ( 'NONE', #41646, #5753, #6012 ) ;
#46561 = AXIS2_PLACEMENT_3D ( 'NONE', #3133, #40056, #35077 ) ;
#46562 = CARTESIAN_POINT ( 'NONE',  ( 78.22251691734010137, -33.11618894467940066, -20.65000000000000213 ) ) ;
#46563 = EDGE_CURVE ( 'NONE', #13523, #51599, #19410, .T. ) ;
#46564 = CARTESIAN_POINT ( 'NONE',  ( 42.53933706901050016, -43.26083871179729812, -4.182107870964270724 ) ) ;
#46565 = FACE_OUTER_BOUND ( 'NONE', #20059, .T. ) ;
#46566 = CARTESIAN_POINT ( 'NONE',  ( 74.93037820153030282, 13.88381105528979909, -15.31096251095349992 ) ) ;
#46567 = CARTESIAN_POINT ( 'NONE',  ( 64.26458081267169575, 1.017362664354699797, -70.23651179247990228 ) ) ;
#46568 = VECTOR ( 'NONE', #47861, 1000.000000000000000 ) ;
#46569 = CARTESIAN_POINT ( 'NONE',  ( 85.66799001034409855, -50.61618894467930119, -61.58097075742929860 ) ) ;
#46570 = CARTESIAN_POINT ( 'NONE',  ( 63.93393739769619089, 10.88381105532070059, -68.84999999999999432 ) ) ;
#46571 = CARTESIAN_POINT ( 'NONE',  ( 16.47608743815100141, -23.45644924220759719, -47.77362331007279295 ) ) ;
#46572 = ORIENTED_EDGE ( 'NONE', *, *, #45907, .F. ) ;
#46573 = CARTESIAN_POINT ( 'NONE',  ( 14.46756122145940004, -52.43578441516969946, -75.98739629952659413 ) ) ;
#46574 = CARTESIAN_POINT ( 'NONE',  ( 57.49472010668189625, 18.97758529344320166, -52.71592469185309682 ) ) ;
#46575 = CARTESIAN_POINT ( 'NONE',  ( 71.83679462228410273, 0.9486745332793860008, -70.37196876996070216 ) ) ;
#46576 = CARTESIAN_POINT ( 'NONE',  ( 45.68290005762235495, -40.07486829699336539, -58.49956670540637305 ) ) ;
#46577 = DIRECTION ( 'NONE',  ( 1.000000000000000000, 0.000000000000000000, 0.000000000000000000 ) ) ;
#46578 = CARTESIAN_POINT ( 'NONE',  ( 47.17210187534929844, -54.78212032244810104, -74.50474471063260751 ) ) ;
#46579 = CARTESIAN_POINT ( 'NONE',  ( 63.50659274611129490, 1.388313565858570131, -68.83005089568669632 ) ) ;
#46580 = CARTESIAN_POINT ( 'NONE',  ( 47.83393063578119353, -54.38673743207299793, -54.71871010756789389 ) ) ;
#46581 = CARTESIAN_POINT ( 'NONE',  ( 21.37438191210599925, -20.33663280004660123, -81.08056213787280342 ) ) ;
#46582 = CIRCLE ( 'NONE', #38231, 3.569999999987189199 ) ;
#46583 = CARTESIAN_POINT ( 'NONE',  ( 68.13393739769620083, 17.38381105532069881, -85.65000000000000568 ) ) ;
#46584 = EDGE_CURVE ( 'NONE', #33786, #17592, #35388, .T. ) ;
#46585 = CARTESIAN_POINT ( 'NONE',  ( 48.19394580060259869, 22.96827044948890162, -54.70769519783490153 ) ) ;
#46586 = ORIENTED_EDGE ( 'NONE', *, *, #43418, .F. ) ;
#46587 = CARTESIAN_POINT ( 'NONE',  ( 14.39186542499959920, -8.781882511953600812, -74.26773406640160147 ) ) ;
#46588 = ORIENTED_EDGE ( 'NONE', *, *, #11027, .T. ) ;
#46589 = CARTESIAN_POINT ( 'NONE',  ( 71.23750802749680133, 1.369613126987639928, -70.37582656035600337 ) ) ;
#46590 = CIRCLE ( 'NONE', #13159, 0.5000000000000004441 ) ;
#46591 = FACE_OUTER_BOUND ( 'NONE', #48329, .T. ) ;
#46592 = DIRECTION ( 'NONE',  ( -1.000000000000000000, 0.000000000000000000, 0.000000000000000000 ) ) ;
#46594 = CARTESIAN_POINT ( 'NONE',  ( 14.28038030992539476, 1.245406012443915467, -34.79644291222909658 ) ) ;
#46593 = CARTESIAN_POINT ( 'NONE',  ( 82.73840718283250339, 14.31743462620540086, -47.62304481396600409 ) ) ;
#46595 = CARTESIAN_POINT ( 'NONE',  ( 17.97980580075899937, -22.42319478683919698, -72.86853056670030071 ) ) ;
#46596 = DIRECTION ( 'NONE',  ( 0.000000000000000000, 0.000000000000000000, 1.000000000000000000 ) ) ;
#46597 = CARTESIAN_POINT ( 'NONE',  ( 20.11812210231799014, -8.703697681116109308, -67.45899657274037509 ) ) ;
#46598 = PLANE ( 'NONE',  #26966 ) ;
#46599 = ORIENTED_EDGE ( 'NONE', *, *, #41989, .F. ) ;
#46600 = DIRECTION ( 'NONE',  ( 1.000000000000000000, 0.000000000000000000, 0.000000000000000000 ) ) ;
#46601 = AXIS2_PLACEMENT_3D ( 'NONE', #45880, #2359, #38530 ) ;
#46602 = VERTEX_POINT ( 'NONE', #51388 ) ;
#46603 = ORIENTED_EDGE ( 'NONE', *, *, #31022, .T. ) ;
#46604 = CARTESIAN_POINT ( 'NONE',  ( 12.32380480341289974, -64.64187183429430661, -15.85794303741049838 ) ) ;
#46605 = CARTESIAN_POINT ( 'NONE',  ( 14.06318216190721948, -7.911108636151629625, -39.20899184368937540 ) ) ;
#46606 = CARTESIAN_POINT ( 'NONE',  ( 16.13393739769620083, -15.61618894467929941, -19.83999999999999986 ) ) ;
#46607 = CARTESIAN_POINT ( 'NONE',  ( 10.75232472717069854, -64.66152432599189126, -46.57791568324620357 ) ) ;
#46608 = AXIS2_PLACEMENT_3D ( 'NONE', #8086, #8600, #32671 ) ;
#46609 = ORIENTED_EDGE ( 'NONE', *, *, #39218, .T. ) ;
#46610 = ORIENTED_EDGE ( 'NONE', *, *, #34203, .T. ) ;
#46611 = CIRCLE ( 'NONE', #34000, 1.999999999999997558 ) ;
#46612 = LINE ( 'NONE', #6248, #26215 ) ;
#46613 = CARTESIAN_POINT ( 'NONE',  ( 50.28419523648629763, 21.33947418011459973, -52.92671477066360097 ) ) ;
#46614 = CARTESIAN_POINT ( 'NONE',  ( 62.52134720042879223, -1.849972813426850049, -16.13391758643249929 ) ) ;
#46615 = CARTESIAN_POINT ( 'NONE',  ( 50.77884678341099800, -50.22802738765170005, -76.16429375959108938 ) ) ;
#46616 = CARTESIAN_POINT ( 'NONE',  ( 59.16347915308939776, -47.65516984601120498, -49.82822139732490285 ) ) ;
#46617 = ORIENTED_EDGE ( 'NONE', *, *, #32368, .T. ) ;
#46618 = CARTESIAN_POINT ( 'NONE',  ( 23.91381703268126913, -14.11266047478952324, -33.73155400743178234 ) ) ;
#46619 = CARTESIAN_POINT ( 'NONE',  ( 9.367509130462650546, -15.61619940421079988, -51.84717978381009118 ) ) ;
#46620 = ORIENTED_EDGE ( 'NONE', *, *, #33745, .F. ) ;
#46621 = CYLINDRICAL_SURFACE ( 'NONE', #29369, 0.4999999999999967248 ) ;
#46622 = DIRECTION ( 'NONE',  ( -1.000000000000000000, 0.000000000000000000, 0.000000000000000000 ) ) ;
#46623 = CARTESIAN_POINT ( 'NONE',  ( 16.34117822573379897, -23.46117452980159968, -48.50408758018539146 ) ) ;
#46624 = CARTESIAN_POINT ( 'NONE',  ( 12.82931844094959928, -50.64771532553120181, -21.34049561054089850 ) ) ;
#46625 = AXIS2_PLACEMENT_3D ( 'NONE', #14451, #42764, #25257 ) ;
#46626 = CARTESIAN_POINT ( 'NONE',  ( 54.14333229794100077, 19.38381105532069881, -76.93437042524608671 ) ) ;
#46627 = EDGE_CURVE ( 'NONE', #50035, #31436, #23065, .T. ) ;
#46628 = CARTESIAN_POINT ( 'NONE',  ( 46.97184464991040187, -53.68621135916810516, -75.90842213619210099 ) ) ;
#46629 = CARTESIAN_POINT ( 'NONE',  ( 57.22120921428249574, 13.89541071290600094, -17.46027851202169856 ) ) ;
#46630 = CARTESIAN_POINT ( 'NONE',  ( 8.978915886419921222, 32.05342364452790349, -46.63388789120410394 ) ) ;
#46631 = ADVANCED_FACE ( 'NONE', ( #19148 ), #50429, .T. ) ;
#46632 = CARTESIAN_POINT ( 'NONE',  ( 71.01106396815980304, 1.383811055320669947, -70.34375346881599000 ) ) ;
#46633 = AXIS2_PLACEMENT_3D ( 'NONE', #13196, #36746, #36487 ) ;
#46634 = CARTESIAN_POINT ( 'NONE',  ( 10.38933687974309983, -19.70790301870550110, -47.65017322902549779 ) ) ;
#46635 = DIRECTION ( 'NONE',  ( 0.7071067811865487940, 0.000000000000000000, 0.7071067811865462405 ) ) ;
#46636 = EDGE_CURVE ( 'NONE', #33390, #727, #23321, .T. ) ;
#46637 = ORIENTED_EDGE ( 'NONE', *, *, #2069, .F. ) ;
#46638 = CARTESIAN_POINT ( 'NONE',  ( 47.51352477951299846, 23.17639757702380265, -74.95061759547310487 ) ) ;
#46639 = CARTESIAN_POINT ( 'NONE',  ( 64.82191989009379540, 0.9958340104639701318, -60.65579263520140074 ) ) ;
#46640 = CARTESIAN_POINT ( 'NONE',  ( 44.61938837358319887, -46.10030783221859707, -8.716654097462109618 ) ) ;
#46641 = CARTESIAN_POINT ( 'NONE',  ( 14.06335861420489586, -7.911062947393018518, -57.20899805696373619 ) ) ;
#46642 = CARTESIAN_POINT ( 'NONE',  ( 15.67962062493140074, -50.86266781791879765, -20.15000000000000213 ) ) ;
#46643 = CARTESIAN_POINT ( 'NONE',  ( 61.75019796695539753, -45.11618894467940066, -28.15000000000000213 ) ) ;
#46644 = VECTOR ( 'NONE', #25096, 1000.000000000000114 ) ;
#46645 = EDGE_CURVE ( 'NONE', #17870, #20534, #19015, .T. ) ;
#46646 = CARTESIAN_POINT ( 'NONE',  ( 46.50380985604989803, -53.09853600777310589, -76.13981661584659832 ) ) ;
#46647 = CARTESIAN_POINT ( 'NONE',  ( 82.54643970977650724, 14.35786247387079939, -47.66714700205459820 ) ) ;
#46648 = CARTESIAN_POINT ( 'NONE',  ( -0.2318988266004489984, 19.75091050890950228, -35.18657710974959230 ) ) ;
#46650 = CARTESIAN_POINT ( 'NONE',  ( 46.21341081811389984, -38.04634951012319988, -59.23843942165659371 ) ) ;
#46649 = FACE_OUTER_BOUND ( 'NONE', #17116, .T. ) ;
#46651 = CARTESIAN_POINT ( 'NONE',  ( 12.48250449044332910, -22.66554293210867499, -32.44440577955815996 ) ) ;
#46652 = ADVANCED_FACE ( 'NONE', ( #31824 ), #23442, .T. ) ;
#46653 = CARTESIAN_POINT ( 'NONE',  ( -33.14787555410379838, -5.864628912960290208, -57.37579723497079698 ) ) ;
#46654 = ORIENTED_EDGE ( 'NONE', *, *, #18550, .T. ) ;
#46655 = CARTESIAN_POINT ( 'NONE',  ( 52.66273262193210059, -49.77080232680150118, -48.50782009810659900 ) ) ;
#46656 = EDGE_LOOP ( 'NONE', ( #27434, #26948, #27476, #26385, #20210 ) ) ;
#46657 = CARTESIAN_POINT ( 'NONE',  ( 42.41448987238078416, 8.636218628778827622, -74.08055508994929994 ) ) ;
#46658 = CARTESIAN_POINT ( 'NONE',  ( 22.90119541241246637, -15.61618911972255930, -40.84718082130915207 ) ) ;
#46659 = CARTESIAN_POINT ( 'NONE',  ( 13.71439950624830040, 19.91720079445899927, -22.21277075379959953 ) ) ;
#46660 = CARTESIAN_POINT ( 'NONE',  ( 13.58669771564977502, 24.30199623652838881, -76.07908087647429340 ) ) ;
#46661 = CARTESIAN_POINT ( 'NONE',  ( 23.08048385509150080, -16.83604590837389736, -44.50815324592459632 ) ) ;
#46662 = CARTESIAN_POINT ( 'NONE',  ( 64.69570918563060502, 1.132579237369250036, -60.79187696645490036 ) ) ;
#46663 = CARTESIAN_POINT ( 'NONE',  ( 53.22811889490370163, 18.28257712635599930, -49.13101610134690134 ) ) ;
#46664 = CARTESIAN_POINT ( 'NONE',  ( 55.45160347463279749, -46.01556803493200221, -16.61970326677620236 ) ) ;
#46665 = DIRECTION ( 'NONE',  ( 0.000000000000000000, 0.000000000000000000, -1.000000000000000000 ) ) ;
#46666 = ORIENTED_EDGE ( 'NONE', *, *, #32723, .T. ) ;
#46667 = CARTESIAN_POINT ( 'NONE',  ( 11.43481287156209980, -9.834763918191741894, -80.35009786776028307 ) ) ;
#46668 = CARTESIAN_POINT ( 'NONE',  ( 72.81333620972418430, 1.370853092582090094, -68.86908206983169123 ) ) ;
#46669 = CARTESIAN_POINT ( 'NONE',  ( 46.63393739769619373, -15.61618894467929941, -35.14999999999999858 ) ) ;
#46670 = CARTESIAN_POINT ( 'NONE',  ( 72.77636315587029969, 1.387131204727290124, -62.61203846038919352 ) ) ;
#46671 = CARTESIAN_POINT ( 'NONE',  ( 11.11361097577930046, -65.20138656326300008, -17.79075125677969993 ) ) ;
#46672 = CARTESIAN_POINT ( 'NONE',  ( 52.56522529778620623, -49.86179102641759897, -48.47379134784809906 ) ) ;
#46673 = CARTESIAN_POINT ( 'NONE',  ( 9.561418032738805195, -17.80800118497800710, -67.74410178669948834 ) ) ;
#46674 = CARTESIAN_POINT ( 'NONE',  ( 16.04183317652673679, -8.830212154920634049, -61.94856816967541135 ) ) ;
#46675 = ADVANCED_FACE ( 'NONE', ( #3563 ), #2444, .F. ) ;
#46676 = CARTESIAN_POINT ( 'NONE',  ( 22.37272211114861520, -20.50159377728038734, -45.71923386948059687 ) ) ;
#46677 = ORIENTED_EDGE ( 'NONE', *, *, #2588, .T. ) ;
#46678 = CARTESIAN_POINT ( 'NONE',  ( 64.87536163491149921, 1.372372808637209785, -70.31281467067098845 ) ) ;
#46679 = VERTEX_POINT ( 'NONE', #15864 ) ;
#46680 = CARTESIAN_POINT ( 'NONE',  ( 10.48646698228519902, -63.14537606440271134, -45.62814768381470287 ) ) ;
#46681 = DIRECTION ( 'NONE',  ( -2.619602780254359830E-11, 3.858400438143729530E-12, 1.000000000000000000 ) ) ;
#46682 = VERTEX_POINT ( 'NONE', #19534 ) ;
#46683 = DIRECTION ( 'NONE',  ( 0.000000000000000000, 0.000000000000000000, 1.000000000000000000 ) ) ;
#46684 = CARTESIAN_POINT ( 'NONE',  ( 57.35094531453410127, 19.00534567308480050, -52.73804475687700233 ) ) ;
#46685 = CARTESIAN_POINT ( 'NONE',  ( 52.19766866516950188, 18.93657527451279776, -76.74438384267088509 ) ) ;
#46686 = ORIENTED_EDGE ( 'NONE', *, *, #20561, .F. ) ;
#46687 = FACE_OUTER_BOUND ( 'NONE', #46394, .T. ) ;
#46688 = PRODUCT ( 'Caster Wheel Tread', 'Caster Wheel Tread', '', ( #27779 ) ) ;
#46689 = FACE_BOUND ( 'NONE', #2252, .T. ) ;
#46690 = CARTESIAN_POINT ( 'NONE',  ( 9.366956702331082241, -16.36803544923866838, -33.41746239687156361 ) ) ;
#46691 = AXIS2_PLACEMENT_3D ( 'NONE', #44978, #36581, #36072 ) ;
#46692 = CARTESIAN_POINT ( 'NONE',  ( 57.35094531453579947, -50.23772356244409565, -52.73804475687759918 ) ) ;
#46693 = CARTESIAN_POINT ( 'NONE',  ( 9.304449704656880371, -20.23580125596250312, -64.60302447664000169 ) ) ;
#46694 = FACE_OUTER_BOUND ( 'NONE', #12760, .T. ) ;
#46695 = CARTESIAN_POINT ( 'NONE',  ( 43.64524006940550294, -37.86935080219515015, -72.09348446035122038 ) ) ;
#46696 = VECTOR ( 'NONE', #10811, 999.9999999999998863 ) ;
#46697 = ORIENTED_EDGE ( 'NONE', *, *, #36784, .F. ) ;
#46698 = ORIENTED_EDGE ( 'NONE', *, *, #46173, .F. ) ;
#46699 = FACE_OUTER_BOUND ( 'NONE', #32376, .T. ) ;
#46700 = CARTESIAN_POINT ( 'NONE',  ( 8.709652693353499231, -14.99434456381809966, -51.25925627687220043 ) ) ;
#46701 = CARTESIAN_POINT ( 'NONE',  ( 52.97667589433369528, -49.63212252085850196, -49.06651684377270328 ) ) ;
#46702 = CARTESIAN_POINT ( 'NONE',  ( 10.41617478728270108, -11.65339576855390114, -32.14999999999999858 ) ) ;
#46703 = ADVANCED_FACE ( 'NONE', ( #47081 ), #39716, .T. ) ;
#46704 = B_SPLINE_CURVE_WITH_KNOTS ( 'NONE', 3,
 ( #48900, #39732, #23719, #44174, #3837, #19810, #35798, #15886, #31839, #20055, #36046, #156, #8272, #24222, #4339, #13257, #9326, #5898, #17433, #25273, #17182, #37597, #33138 ),
 .UNSPECIFIED., .F., .F.,
 ( 4, 2, 2, 1, 1, 2, 2, 2, 2, 1, 1, 1, 2, 4 ),
 ( 0.000000000000000000, 0.1072084829650507831, 0.1608127244475765771, 0.1876148451888395019, 0.2010159055594712973, 0.2077164357447871257, 0.2144169659301028985, 0.3216254488951440504, 0.3752296903776636272, 0.4020318111189224441, 0.4154328714895532682, 0.4221334016748690687, 0.4254836667675259143, 0.4288339318601827599 ),
 .UNSPECIFIED. ) ;
#46705 = CARTESIAN_POINT ( 'NONE',  ( 9.668218123015291710, -13.53253765274168785, -61.55199406560768693 ) ) ;
#46706 = LINE ( 'NONE', #31443, #25045 ) ;
#46707 = DIRECTION ( 'NONE',  ( 0.000000000000000000, 0.000000000000000000, 1.000000000000000000 ) ) ;
#46708 = B_SPLINE_CURVE_WITH_KNOTS ( 'NONE', 3,
 ( #12467, #36297, #8019, #5135, #12736, #16651, #32609, #37094 ),
 .UNSPECIFIED., .F., .F.,
 ( 4, 2, 2, 4 ),
 ( 0.000000000000000000, 0.3707862687908220489, 0.9874243036154037867, 1.000000000000000000 ),
 .UNSPECIFIED. ) ;
#46709 = CARTESIAN_POINT ( 'NONE',  ( 45.47878560697390071, -45.37428362319629827, -8.420277137582820259 ) ) ;
#46710 = CARTESIAN_POINT ( 'NONE',  ( 24.04485473594626299, -15.57709046178206691, -61.50610320075744397 ) ) ;
#46711 = CARTESIAN_POINT ( 'NONE',  ( 15.42519564855719949, -23.83083475822490271, -60.03506373439409316 ) ) ;
#46712 = ORIENTED_EDGE ( 'NONE', *, *, #47661, .F. ) ;
#46713 = CARTESIAN_POINT ( 'NONE',  ( 21.08334951516359723, -21.61472930959210004, -32.14999999999999858 ) ) ;
#46714 = CARTESIAN_POINT ( 'NONE',  ( 53.64274194304960020, -51.26763427440859999, -75.63099620592139161 ) ) ;
#46716 = CARTESIAN_POINT ( 'NONE',  ( 41.52316232194336010, -39.71166745791303754, -78.63244444805715716 ) ) ;
#46715 = CARTESIAN_POINT ( 'NONE',  ( -0.8795253323679090851, 21.57280389172689894, -9.219647602998469083 ) ) ;
#46717 = CARTESIAN_POINT ( 'NONE',  ( 14.13393739769619906, -32.61307204591476250, -35.10658870008958843 ) ) ;
#46718 = DIRECTION ( 'NONE',  ( 0.000000000000000000, 0.000000000000000000, -1.000000000000000000 ) ) ;
#46719 = ORIENTED_EDGE ( 'NONE', *, *, #42677, .F. ) ;
#46720 = CYLINDRICAL_SURFACE ( 'NONE', #24748, 6.766999999999998572 ) ;
#46721 = CARTESIAN_POINT ( 'NONE',  ( 47.84139276221520021, 23.14568351075850217, -54.70178033708860710 ) ) ;
#46722 = CIRCLE ( 'NONE', #16540, 22.00000000000000355 ) ;
#46723 = CARTESIAN_POINT ( 'NONE',  ( 41.50323316430841203, -44.79455443392685510, -5.449105696209454841 ) ) ;
#46724 = CYLINDRICAL_SURFACE ( 'NONE', #48607, 6.766999999999998572 ) ;
#46725 = CARTESIAN_POINT ( 'NONE',  ( 61.29280341538199650, 14.32362702051400127, -47.63129005651870074 ) ) ;
#46726 = CARTESIAN_POINT ( 'NONE',  ( 11.81751872167160045, 34.08285254420739818, -17.14434883937219922 ) ) ;
#46727 = CARTESIAN_POINT ( 'NONE',  ( 51.78350020499539852, 17.91029486332229936, -77.04630018135540581 ) ) ;
#46728 = CARTESIAN_POINT ( 'NONE',  ( 52.93112653136360279, 18.37582452390590149, -48.77840570252370611 ) ) ;
#46729 = DIRECTION ( 'NONE',  ( 0.000000000000000000, 0.000000000000000000, -1.000000000000000000 ) ) ;
#46730 = CARTESIAN_POINT ( 'NONE',  ( 51.13393739769620083, 19.38381105532069881, 14.21249999999999858 ) ) ;
#46731 = CARTESIAN_POINT ( 'NONE',  ( 56.52276590765480080, 15.01206069354710060, -26.27186043794959858 ) ) ;
#46732 = CARTESIAN_POINT ( 'NONE',  ( 49.64260032845869830, 22.42839500882750059, -54.78414101162800165 ) ) ;
#46733 = CARTESIAN_POINT ( 'NONE',  ( 53.70440469537284400, -48.89725131568911820, -27.13824717588386903 ) ) ;
#46734 = CARTESIAN_POINT ( 'NONE',  ( 52.60294686985729840, 18.59530815018699812, -48.60888033553569443 ) ) ;
#46735 = CARTESIAN_POINT ( 'NONE',  ( 8.222931813264825252, -16.65169553128620450, -76.46600585124562599 ) ) ;
#46736 = CARTESIAN_POINT ( 'NONE',  ( 71.36799767121769378, 0.8859637708054489691, -60.59611492242089525 ) ) ;
#46737 = CARTESIAN_POINT ( 'NONE',  ( 10.77336949205099970, 32.10438947587439884, -45.20591960971059819 ) ) ;
#46738 = CARTESIAN_POINT ( 'NONE',  ( 72.70504696988909643, 1.400446703427080219, -62.40275391609110756 ) ) ;
#46739 = ADVANCED_FACE ( 'NONE', ( #3297 ), #4946, .F. ) ;
#46740 = DIRECTION ( 'NONE',  ( 0.000000000000000000, 0.000000000000000000, 1.000000000000000000 ) ) ;
#46741 = CARTESIAN_POINT ( 'NONE',  ( 8.332394648117634972, -14.10178411776632679, -80.56861278440374008 ) ) ;
#46742 = ORIENTED_EDGE ( 'NONE', *, *, #46958, .F. ) ;
#46743 = ADVANCED_FACE ( 'NONE', ( #23951 ), #27528, .T. ) ;
#46744 = ORIENTED_EDGE ( 'NONE', *, *, #14254, .F. ) ;
#46745 = CARTESIAN_POINT ( 'NONE',  ( 68.59772359096709238, -1.116188944679340045, -21.89807540431120358 ) ) ;
#46746 = CARTESIAN_POINT ( 'NONE',  ( 76.87859648677320479, 11.88381402801379849, -14.85884684523960075 ) ) ;
#46747 = VERTEX_POINT ( 'NONE', #23185 ) ;
#46748 = CARTESIAN_POINT ( 'NONE',  ( 10.97811661469409827, -63.90378363857650612, -45.04831364494010160 ) ) ;
#46749 = CARTESIAN_POINT ( 'NONE',  ( 57.51881368209140533, -45.19501142122329895, -25.74532814797139935 ) ) ;
#46750 = CARTESIAN_POINT ( 'NONE',  ( 16.13393739769620083, -15.61618894467929941, -18.58999999999999986 ) ) ;
#46751 = EDGE_CURVE ( 'NONE', #3494, #38460, #6074, .T. ) ;
#46752 = CYLINDRICAL_SURFACE ( 'NONE', #3052, 3.000000000000003997 ) ;
#46753 = CARTESIAN_POINT ( 'NONE',  ( 16.13393739769620083, -15.61618894467929941, -28.02168704970069868 ) ) ;
#46755 = ORIENTED_EDGE ( 'NONE', *, *, #6582, .T. ) ;
#46754 = B_SPLINE_CURVE_WITH_KNOTS ( 'NONE', 3,
 ( #11067, #14985, #22316, #46982, #42782, #42257, #42523, #34893, #18655, #50893, #43039, #10807, #46723, #14730 ),
 .UNSPECIFIED., .F., .F.,
 ( 4, 2, 2, 2, 2, 2, 4 ),
 ( 0.000000000000000000, 0.06287436669111368115, 0.3602487949084645091, 0.6184358969147355500, 0.8245813718801661141, 0.9276541093628823953, 1.000000000000000000 ),
 .UNSPECIFIED. ) ;
#46756 = CYLINDRICAL_SURFACE ( 'NONE', #46952, 7.910999999999997812 ) ;
#46757 = CARTESIAN_POINT ( 'NONE',  ( 42.91198480261937931, 6.532264137049844877, -75.75975149268437292 ) ) ;
#46758 = CARTESIAN_POINT ( 'NONE',  ( 12.05844419658449951, 34.05022214372210243, -23.57277994855740033 ) ) ;
#46759 = EDGE_LOOP ( 'NONE', ( #37833, #45141, #3095, #40944, #33230 ) ) ;
#46760 = CARTESIAN_POINT ( 'NONE',  ( 9.997500756706150682, -21.12317227560119903, -36.55952288011869911 ) ) ;
#46761 = DIRECTION ( 'NONE',  ( 0.000000000000000000, 0.000000000000000000, 1.000000000000000000 ) ) ;
#46762 = CARTESIAN_POINT ( 'NONE',  ( 8.223013028489239318, -15.61598591435789984, -40.50766849176299189 ) ) ;
#46763 = CARTESIAN_POINT ( 'NONE',  ( 9.543081973236891002, -13.84487673733323732, -63.53615373438451996 ) ) ;
#46764 = CARTESIAN_POINT ( 'NONE',  ( 46.81139557655359340, -53.78025948612990703, -75.90528168595349712 ) ) ;
#46765 = CARTESIAN_POINT ( 'NONE',  ( 52.39839370536370211, 12.55527397068519946, -7.161984143140530001 ) ) ;
#46766 = CIRCLE ( 'NONE', #35843, 12.50000000000000000 ) ;
#46767 = EDGE_CURVE ( 'NONE', #43323, #39742, #15355, .T. ) ;
#46768 = CARTESIAN_POINT ( 'NONE',  ( 16.13393739769620083, -15.61618894467929941, -32.14999999999999858 ) ) ;
#46769 = CARTESIAN_POINT ( 'NONE',  ( 65.03603135455020379, -32.24781572988710110, -17.83403478221860183 ) ) ;
#46770 = CARTESIAN_POINT ( 'NONE',  ( 22.98728463840710035, -20.20033033726479843, -37.69532517445340147 ) ) ;
#46771 = EDGE_LOOP ( 'NONE', ( #47787, #2333, #40129, #20651 ) ) ;
#46772 = CARTESIAN_POINT ( 'NONE',  ( 54.32193552160570249, -48.29328850758490432, -26.80441240787190083 ) ) ;
#46773 = CARTESIAN_POINT ( 'NONE',  ( 1.775250261842860056, -55.58081467171729884, -10.96136838756989818 ) ) ;
#46774 = CARTESIAN_POINT ( 'NONE',  ( 75.37466888843739810, -30.01699399069740082, -11.89334001646519923 ) ) ;
#46775 = B_SPLINE_CURVE_WITH_KNOTS ( 'NONE', 3,
 ( #7725, #30313, #33979, #26120, #27617, #3791, #7971, #23413 ),
 .UNSPECIFIED., .F., .F.,
 ( 4, 2, 2, 4 ),
 ( 0.04082353370410345822, 0.04299190937466709772, 0.06210110413228960013, 0.08070042245434939920 ),
 .UNSPECIFIED. ) ;
#46776 = DIRECTION ( 'NONE',  ( -1.000000000000000000, 0.000000000000000000, 0.000000000000000000 ) ) ;
#46777 = CARTESIAN_POINT ( 'NONE',  ( 19.61576842239554352, -55.46436179167167069, -75.47957398524580697 ) ) ;
#46778 = CARTESIAN_POINT ( 'NONE',  ( 14.28038030992539476, 1.245406012443915467, -34.79644291222909658 ) ) ;
#46779 = CARTESIAN_POINT ( 'NONE',  ( 23.04646436867740533, -19.60031334711585416, -35.95899589054670997 ) ) ;
#46780 = CARTESIAN_POINT ( 'NONE',  ( 82.33636376959559300, -45.53544251379970120, -47.60086788096420207 ) ) ;
#46781 = FACE_OUTER_BOUND ( 'NONE', #43657, .T. ) ;
#46782 = CARTESIAN_POINT ( 'NONE',  ( 40.60988597354600671, 13.46376186705429845, -4.337423628782890006 ) ) ;
#46783 = CARTESIAN_POINT ( 'NONE',  ( 39.88393739769619373, 30.88381105532059934, 16.35000000000000142 ) ) ;
#46784 = FACE_OUTER_BOUND ( 'NONE', #29550, .T. ) ;
#46785 = CARTESIAN_POINT ( 'NONE',  ( 68.13393739769745139, -49.21324915460109395, -75.95351669811962836 ) ) ;
#46786 = DIRECTION ( 'NONE',  ( 0.000000000000000000, -1.000000000000000000, 0.000000000000000000 ) ) ;
#46787 = CARTESIAN_POINT ( 'NONE',  ( 17.66909654327109536, -51.94403353591209793, -75.77396328158869210 ) ) ;
#46788 = CARTESIAN_POINT ( 'NONE',  ( 58.76844946023069838, -44.34544036321329941, -9.066887851337279258 ) ) ;
#46789 = ORIENTED_EDGE ( 'NONE', *, *, #38602, .F. ) ;
#46790 = CARTESIAN_POINT ( 'NONE',  ( 21.40914480240369855, -20.87726119049199980, -55.31691565165660052 ) ) ;
#46791 = CARTESIAN_POINT ( 'NONE',  ( 63.86404120422080410, 1.117797034538490220, -61.44141157926519980 ) ) ;
#46792 = VERTEX_POINT ( 'NONE', #29455 ) ;
#46793 = CARTESIAN_POINT ( 'NONE',  ( -7.152475357492779295, 15.01427191330900079, -6.869070896293750117 ) ) ;
#46794 = CARTESIAN_POINT ( 'NONE',  ( 60.83524288460380802, -45.71913028275810120, -47.74946701498309665 ) ) ;
#46795 = CARTESIAN_POINT ( 'NONE',  ( 73.20987945474540481, 1.101170701158060039, -68.76387392617688477 ) ) ;
#46796 = VECTOR ( 'NONE', #22926, 1000.000000000000000 ) ;
#46797 = CARTESIAN_POINT ( 'NONE',  ( 20.29261112856793758, -10.20487222028709695, -74.16115355788735997 ) ) ;
#46798 = AXIS2_PLACEMENT_3D ( 'NONE', #5293, #48528, #12634 ) ;
#46799 = CARTESIAN_POINT ( 'NONE',  ( 9.146229968232489682, -16.61861051933619748, -81.23899999999999011 ) ) ;
#46800 = CARTESIAN_POINT ( 'NONE',  ( 42.77858091870550084, -45.71739890479680213, -7.241831254560019637 ) ) ;
#46801 = ORIENTED_EDGE ( 'NONE', *, *, #22211, .F. ) ;
#46802 = EDGE_CURVE ( 'NONE', #47075, #12119, #40481, .T. ) ;
#46803 = EDGE_LOOP ( 'NONE', ( #45169, #5794, #36809, #49950, #12230 ) ) ;
#46804 = ORIENTED_EDGE ( 'NONE', *, *, #11383, .T. ) ;
#46805 = CARTESIAN_POINT ( 'NONE',  ( 29.13393739769619017, -1.673960226304022969, -42.42700139135352089 ) ) ;
#46806 = CARTESIAN_POINT ( 'NONE',  ( 23.35918962205809990, -13.17756933140159958, -81.23899999999999011 ) ) ;
#46807 = EDGE_CURVE ( 'NONE', #13573, #42105, #4122, .T. ) ;
#46808 = FACE_OUTER_BOUND ( 'NONE', #29799, .T. ) ;
#46809 =( BOUNDED_CURVE ( )  B_SPLINE_CURVE ( 3, ( #1331, #13396, #20195, #12347 ),
 .UNSPECIFIED., .F., .T. ) 
 B_SPLINE_CURVE_WITH_KNOTS ( ( 4, 4 ),
 ( 0.3752708228560562298, 1.160668986253397872 ),
 .UNSPECIFIED. ) 
 CURVE ( )  GEOMETRIC_REPRESENTATION_ITEM ( )  RATIONAL_B_SPLINE_CURVE ( ( 1.000000000000000000, 0.9492530216742047777, 0.9492530216742047777, 1.000000000000000000 ) ) 
 REPRESENTATION_ITEM ( '' )  );
#46810 = CARTESIAN_POINT ( 'NONE',  ( -2.938890781262444296, -49.79850883445518406, -37.77204286592886717 ) ) ;
#46811 = ORIENTED_EDGE ( 'NONE', *, *, #3957, .T. ) ;
#46812 = CARTESIAN_POINT ( 'NONE',  ( 12.14980047455250833, -8.703668882721308009, -52.84100284372439660 ) ) ;
#46813 = EDGE_LOOP ( 'NONE', ( #17009, #4496, #18556, #10324 ) ) ;
#46814 = DIRECTION ( 'NONE',  ( 0.000000000000000000, 1.000000000000000000, 0.000000000000000000 ) ) ;
#46815 = CARTESIAN_POINT ( 'NONE',  ( 45.34326386872739789, -33.92578000960650542, -34.65000321691689322 ) ) ;
#46816 = ORIENTED_EDGE ( 'NONE', *, *, #22325, .F. ) ;
#46817 = CARTESIAN_POINT ( 'NONE',  ( 44.85820924768243856, 1.972254910232243752, -41.02118509755829479 ) ) ;
#46818 = CARTESIAN_POINT ( 'NONE',  ( 51.30756349522820159, -50.82514498746949982, -76.17053261049738921 ) ) ;
#46819 = VECTOR ( 'NONE', #19144, 1000.000000000000000 ) ;
#46820 = CARTESIAN_POINT ( 'NONE',  ( 60.56605300001870518, 14.40753913078479975, -47.40713001077759969 ) ) ;
#46821 = EDGE_CURVE ( 'NONE', #51151, #18993, #36732, .T. ) ;
#46822 = CARTESIAN_POINT ( 'NONE',  ( 2.423250969874890082, -5.412656893201930330, -35.01387690002259490 ) ) ;
#46823 = EDGE_CURVE ( 'NONE', #22850, #38811, #37591, .T. ) ;
#46824 = CARTESIAN_POINT ( 'NONE',  ( 40.60804131356049851, -44.74569051554189514, -4.641941792357479279 ) ) ;
#46825 = DIRECTION ( 'NONE',  ( -1.000000000000000000, 0.000000000000000000, 0.000000000000000000 ) ) ;
#46826 = CARTESIAN_POINT ( 'NONE',  ( -6.415573901255199551, 15.04311249118519989, -5.150318756231260231 ) ) ;
#46827 = VECTOR ( 'NONE', #34991, 999.9999999999998863 ) ;
#46828 = CARTESIAN_POINT ( 'NONE',  ( 64.89936453248850512, 1.399477666643410112, -70.22527192354300496 ) ) ;
#46829 = LINE ( 'NONE', #51518, #22196 ) ;
#46830 = CARTESIAN_POINT ( 'NONE',  ( 59.13393739769620083, 1.883811055320659955, -34.64999999999999858 ) ) ;
#46831 = CARTESIAN_POINT ( 'NONE',  ( 17.43302574698969920, -23.35564096946199797, -51.73456986325390261 ) ) ;
#46832 = EDGE_LOOP ( 'NONE', ( #18795, #45834, #29566, #32763, #6642, #12045 ) ) ;
#46833 = DIRECTION ( 'NONE',  ( -0.005554557064135746090, -0.7535009559967822401, -0.6574233462600460598 ) ) ;
#46834 = CARTESIAN_POINT ( 'NONE',  ( 45.07858682377059978, 14.88010818488339915, -9.026855431852879974 ) ) ;
#46835 = PRODUCT_DEFINITION_CONTEXT ( 'detailed design', #35476, 'design' ) ;
#46836 = CARTESIAN_POINT ( 'NONE',  ( 71.55691549992010891, 1.416242794300029972, -70.15496246767990840 ) ) ;
#46837 = CARTESIAN_POINT ( 'NONE',  ( 45.02188872858284441, -40.03205829299434271, -61.70655696423168735 ) ) ;
#46838 = CARTESIAN_POINT ( 'NONE',  ( 14.70125025181300060, 19.30047638221009976, -20.74420046562330100 ) ) ;
#46839 = CARTESIAN_POINT ( 'NONE',  ( 22.04234237985629719, -11.89659550907480146, -32.14999999999999858 ) ) ;
#46840 = CARTESIAN_POINT ( 'NONE',  ( 22.90080846266944548, -15.61618871746016879, -44.84718732428002852 ) ) ;
#46841 = CARTESIAN_POINT ( 'NONE',  ( 61.08966779969438932, 14.10374125018732983, -46.92974023940308825 ) ) ;
#46842 = CARTESIAN_POINT ( 'NONE',  ( 48.05050519812169796, -54.35518933397780472, -55.13482086050959197 ) ) ;
#46843 = FACE_OUTER_BOUND ( 'NONE', #11547, .T. ) ;
#46844 = CARTESIAN_POINT ( 'NONE',  ( -6.554330339767415303, -46.10323663958071450, -4.693995882122231400 ) ) ;
#46845 = CARTESIAN_POINT ( 'NONE',  ( 23.04645369194869886, -19.60033335300210666, -45.95903034818195465 ) ) ;
#46846 = CARTESIAN_POINT ( 'NONE',  ( 47.79402269939749459, 23.21147026759410181, -54.88834611196039504 ) ) ;
#46847 = ORIENTED_EDGE ( 'NONE', *, *, #27392, .T. ) ;
#46848 = CARTESIAN_POINT ( 'NONE',  ( 19.32514136844950059, -21.90576575011689897, -69.19772247832989365 ) ) ;
#46849 = ORIENTED_EDGE ( 'NONE', *, *, #812, .T. ) ;
#46850 = CARTESIAN_POINT ( 'NONE',  ( 71.44595490529880522, 0.9958340104639701318, -70.64420736479868879 ) ) ;
#46851 = CARTESIAN_POINT ( 'NONE',  ( 60.23889825737560244, -45.78059604851859632, -47.30579064662349964 ) ) ;
#46852 = CARTESIAN_POINT ( 'NONE',  ( 57.08448514777830241, -47.43174880974720509, -47.79773139290959705 ) ) ;
#46853 = DIRECTION ( 'NONE',  ( 0.000000000000000000, 0.000000000000000000, 1.000000000000000000 ) ) ;
#46855 = CARTESIAN_POINT ( 'NONE',  ( 44.21750825437292320, -33.11618894467930119, -52.85396186151582754 ) ) ;
#46854 = CARTESIAN_POINT ( 'NONE',  ( 40.81680904382810837, 8.394903995891963788, -82.03934974883871689 ) ) ;
#46856 = CARTESIAN_POINT ( 'NONE',  ( 0.4394934780714550016, -22.38736998951459967, -35.02127583263639821 ) ) ;
#46857 = DIRECTION ( 'NONE',  ( 0.000000000000000000, -1.000000000000000000, 0.000000000000000000 ) ) ;
#46858 = ORIENTED_EDGE ( 'NONE', *, *, #21292, .F. ) ;
#46859 = DIRECTION ( 'NONE',  ( 1.000000000000000000, 0.000000000000000000, 0.000000000000000000 ) ) ;
#46860 = ORIENTED_EDGE ( 'NONE', *, *, #22824, .T. ) ;
#46861 = EDGE_CURVE ( 'NONE', #27066, #38190, #15834, .T. ) ;
#46862 = B_SPLINE_CURVE_WITH_KNOTS ( 'NONE', 3,
 ( #46834, #38707, #42373, #27400, #35269, #43401, #7501, #19542, #10921, #51522, #22427, #38435, #18514, #26885, #20553, #8006, #11694, #39724, #20044, #35789, #12201, #51772, #145, #28423, #27657, #44427, #43658, #3827, #16123, #19800, #31831, #12454, #8529, #32084 ),
 .UNSPECIFIED., .F., .F.,
 ( 4, 3, 3, 3, 3, 3, 3, 3, 3, 3, 3, 4 ),
 ( -6.893222615345909965, -6.545934836083509900, -5.829966074818360156, -5.113218181026589981, -4.902226309511959812, -4.188682698346940292, -3.475139087181930542, -2.862484081209690778, -2.335777911127269846, -1.843229489558059875, -1.766097323099939942, -1.366260745963329803 ),
 .UNSPECIFIED. ) ;
#46863 = VERTEX_POINT ( 'NONE', #49401 ) ;
#46864 = CARTESIAN_POINT ( 'NONE',  ( 12.29622276840649953, -64.73592984932109573, -15.96315064375670012 ) ) ;
#46865 = AXIS2_PLACEMENT_3D ( 'NONE', #26109, #22699, #51016 ) ;
#46866 = CARTESIAN_POINT ( 'NONE',  ( 9.807714802521521946, -10.75458453011491500, -39.00066019740137335 ) ) ;
#46867 = AXIS2_PLACEMENT_3D ( 'NONE', #39526, #42947, #7044 ) ;
#46868 = CYLINDRICAL_SURFACE ( 'NONE', #40299, 11.00000000000000000 ) ;
#46869 = CARTESIAN_POINT ( 'NONE',  ( 11.59770002601669958, -65.28329604816460119, -47.33594395550530720 ) ) ;
#46870 = VECTOR ( 'NONE', #14090, 1000.000000000000114 ) ;
#46871 = ORIENTED_EDGE ( 'NONE', *, *, #20485, .T. ) ;
#46872 = CIRCLE ( 'NONE', #18369, 2.700000000000230216 ) ;
#46873 = ORIENTED_EDGE ( 'NONE', *, *, #44355, .F. ) ;
#46874 = CARTESIAN_POINT ( 'NONE',  ( 24.04493739861623780, -15.61807028455928936, -55.50774772363322285 ) ) ;
#46875 = SPHERICAL_SURFACE ( 'NONE', #1121, 2.000000000000000000 ) ;
#46876 = CARTESIAN_POINT ( 'NONE',  ( 13.80275570120679340, -9.247983252851710745, -45.84118090379607935 ) ) ;
#46877 = CARTESIAN_POINT ( 'NONE',  ( 63.34240831626450330, -0.3547437479215780343, -16.56187347819639655 ) ) ;
#46878 = CARTESIAN_POINT ( 'NONE',  ( 56.91685934183519890, -50.04301054400669813, -52.37184532886749366 ) ) ;
#46879 = ORIENTED_EDGE ( 'NONE', *, *, #28669, .T. ) ;
#46880 = CARTESIAN_POINT ( 'NONE',  ( 24.00414318207540987, -14.78277253604543162, -33.75875707254959934 ) ) ;
#46881 = CARTESIAN_POINT ( 'NONE',  ( 9.367491665984019278, -15.61623476897930018, -53.45282021618999124 ) ) ;
#46882 = ORIENTED_EDGE ( 'NONE', *, *, #51515, .F. ) ;
#46883 = DIRECTION ( 'NONE',  ( 0.000000000000000000, -1.000000000000000000, 0.000000000000000000 ) ) ;
#46884 = DIRECTION ( 'NONE',  ( 0.000000000000000000, -1.000000000000000000, 0.000000000000000000 ) ) ;
#46885 = CARTESIAN_POINT ( 'NONE',  ( 12.57046430646940038, -22.60821348122700059, -48.66252544231259236 ) ) ;
#46886 = CARTESIAN_POINT ( 'NONE',  ( 13.99896632404920105, -51.14831594409909599, -22.43872229512260219 ) ) ;
#46887 = CARTESIAN_POINT ( 'NONE',  ( 57.21094436373439862, 19.38381105532069881, -74.14882592923370908 ) ) ;
#46888 = EDGE_CURVE ( 'NONE', #41446, #23485, #4321, .T. ) ;
#46889 = DIRECTION ( 'NONE',  ( 1.000000000000000000, 0.000000000000000000, 0.000000000000000000 ) ) ;
#46890 = CARTESIAN_POINT ( 'NONE',  ( 54.99584801749529817, 14.10383798426820157, -15.06529325330870073 ) ) ;
#46891 = CARTESIAN_POINT ( 'NONE',  ( 8.737696419500521117, 17.70577807492154321, -34.78557451168259718 ) ) ;
#46892 = CARTESIAN_POINT ( 'NONE',  ( 56.61697313395120545, -50.69523099840940006, -53.47849945248049863 ) ) ;
#46893 = CARTESIAN_POINT ( 'NONE',  ( 21.72984300404249680, -19.90902013391950121, -43.05547522733549926 ) ) ;
#46894 = VERTEX_POINT ( 'NONE', #4844 ) ;
#46895 = CARTESIAN_POINT ( 'NONE',  ( 47.21787081358019833, 22.79230847309320040, -75.61358154568520717 ) ) ;
#46896 = CARTESIAN_POINT ( 'NONE',  ( 65.01178944337650023, 1.369535599030039963, -60.93144909420819744 ) ) ;
#46897 = AXIS2_PLACEMENT_3D ( 'NONE', #21378, #37381, #33433 ) ;
#46898 = CARTESIAN_POINT ( 'NONE',  ( 23.57448381426044293, 17.62014253445614287, -34.86893418027934644 ) ) ;
#46899 = CARTESIAN_POINT ( 'NONE',  ( 53.63393739769619373, 21.88381105532059934, 10.84999999999999964 ) ) ;
#46900 = VECTOR ( 'NONE', #39541, 1000.000000000000000 ) ;
#46901 = CARTESIAN_POINT ( 'NONE',  ( 15.65806070092803992, -50.85540152079837384, -20.25522491696300875 ) ) ;
#46902 = CARTESIAN_POINT ( 'NONE',  ( 14.19855276898660001, 24.33696219936630101, -76.14999999999999147 ) ) ;
#46903 = CIRCLE ( 'NONE', #5882, 134.6233317251269739 ) ;
#46904 = CARTESIAN_POINT ( 'NONE',  ( 16.13393739769579582, -15.61618894467939889, -10.44999999999980034 ) ) ;
#46905 = CARTESIAN_POINT ( 'NONE',  ( 82.13853704237929776, 13.88834436876070200, -46.53690974066719832 ) ) ;
#46906 = CARTESIAN_POINT ( 'NONE',  ( -15.88273178560489818, 6.935963212412289636, -48.60151163369399541 ) ) ;
#46908 = CARTESIAN_POINT ( 'NONE',  ( 45.05991370691160824, -37.95321327874120243, -65.01221274611590673 ) ) ;
#46907 = CARTESIAN_POINT ( 'NONE',  ( 53.99784731903601909, 19.38381105527493986, -77.02981984151007566 ) ) ;
#46909 = CARTESIAN_POINT ( 'NONE',  ( 18.13393739769620083, -45.61618894467940066, -62.64999999999999858 ) ) ;
#46910 = CARTESIAN_POINT ( 'NONE',  ( 49.47774481438250405, 22.52031088949399873, -55.14135542417720615 ) ) ;
#46911 = VERTEX_POINT ( 'NONE', #647 ) ;
#46912 = CARTESIAN_POINT ( 'NONE',  ( 53.13943618043249728, -49.50838218133899460, -48.93645286566210473 ) ) ;
#46913 = EDGE_LOOP ( 'NONE', ( #30041, #47565, #43136, #6226 ) ) ;
#46914 = CARTESIAN_POINT ( 'NONE',  ( 44.75967145671651082, 8.877769785130974256, -62.58944400151567322 ) ) ;
#46915 = CARTESIAN_POINT ( 'NONE',  ( 46.27983543144652856, 15.85709954156585155, 17.35000000000000142 ) ) ;
#46916 = CARTESIAN_POINT ( 'NONE',  ( 13.61938558664210142, 20.19483563600030251, -23.00040036072980243 ) ) ;
#46917 = CARTESIAN_POINT ( 'NONE',  ( 51.90728548701680012, -49.37557664627889409, -77.08408650135000073 ) ) ;
#46918 = CARTESIAN_POINT ( 'NONE',  ( 18.46354428964319894, -22.27317703432000329, -50.84566773101410320 ) ) ;
#46919 = CARTESIAN_POINT ( 'NONE',  ( 52.74572841191380235, 18.49240759515019761, -48.77971847666659500 ) ) ;
#46920 = CARTESIAN_POINT ( 'NONE',  ( 55.49574894575610529, -45.93699121200089763, -16.59260285522099920 ) ) ;
#46921 = CARTESIAN_POINT ( 'NONE',  ( 16.57664560245815366, 19.88381105532340598, -15.67533231080279954 ) ) ;
#46922 = ORIENTED_EDGE ( 'NONE', *, *, #42111, .T. ) ;
#46923 = EDGE_CURVE ( 'NONE', #5062, #34403, #45995, .T. ) ;
#46924 = CARTESIAN_POINT ( 'NONE',  ( 17.48707020955630043, -23.34637521513419856, -35.73234578840269648 ) ) ;
#46925 = VERTEX_POINT ( 'NONE', #44419 ) ;
#46926 = EDGE_CURVE ( 'NONE', #48001, #29313, #30023, .T. ) ;
#46927 = CARTESIAN_POINT ( 'NONE',  ( 11.88601304140500048, -65.43528728455630983, -17.88642721559120119 ) ) ;
#46928 = CARTESIAN_POINT ( 'NONE',  ( 9.949440222175219617, 33.40288359707810173, -46.96299386755929817 ) ) ;
#46929 = CARTESIAN_POINT ( 'NONE',  ( 73.06536971133249381, 1.096932441169210071, -62.29998885741579784 ) ) ;
#46930 = CARTESIAN_POINT ( 'NONE',  ( 47.99888731038549849, -54.67877686907520030, -55.58081006888029663 ) ) ;
#46932 = EDGE_CURVE ( 'NONE', #3421, #48088, #40934, .T. ) ;
#46931 = CARTESIAN_POINT ( 'NONE',  ( 68.13393739769620083, 11.88381105532070059, -71.50000000000000000 ) ) ;
#46933 = CARTESIAN_POINT ( 'NONE',  ( 63.02122824129657630, -31.65172625870799195, -17.11446970408973201 ) ) ;
#46934 = CARTESIAN_POINT ( 'NONE',  ( 51.54415332628170177, -52.59067900109340599, -53.64346124582210251 ) ) ;
#46935 = EDGE_CURVE ( 'NONE', #5682, #39834, #18324, .T. ) ;
#46936 = ORIENTED_EDGE ( 'NONE', *, *, #10313, .F. ) ;
#46937 = CARTESIAN_POINT ( 'NONE',  ( 61.47023863363166640, 14.17716911753344888, -47.41726777464327114 ) ) ;
#46938 = ORIENTED_EDGE ( 'NONE', *, *, #11786, .F. ) ;
#46939 = CARTESIAN_POINT ( 'NONE',  ( 10.14330270683290181, -63.24555248048280021, -45.99329719495809599 ) ) ;
#46940 = CARTESIAN_POINT ( 'NONE',  ( 67.04038824939809160, 19.47158195952359705, -70.40645085170191919 ) ) ;
#46941 = ORIENTED_EDGE ( 'NONE', *, *, #50037, .F. ) ;
#46942 = CARTESIAN_POINT ( 'NONE',  ( 67.77185288443023126, -32.48144925312345777, -19.08055328465526301 ) ) ;
#46943 = CARTESIAN_POINT ( 'NONE',  ( 57.24718409514530038, 19.38381105959480166, -53.91456318647720281 ) ) ;
#46944 = CARTESIAN_POINT ( 'NONE',  ( 52.62506680556380445, 18.89058939249819957, -77.17021719700440485 ) ) ;
#46945 = ORIENTED_EDGE ( 'NONE', *, *, #47389, .F. ) ;
#46946 = CARTESIAN_POINT ( 'NONE',  ( 71.33393739775299025, 1.883811055181200178, -62.44999999988809236 ) ) ;
#46947 = DIRECTION ( 'NONE',  ( 1.000000000000000000, 0.000000000000000000, 0.000000000000000000 ) ) ;
#46948 = AXIS2_PLACEMENT_3D ( 'NONE', #7319, #11253, #51081 ) ;
#46949 = CARTESIAN_POINT ( 'NONE',  ( 11.84381659772448359, -20.90316959714175482, -33.16995766164247783 ) ) ;
#46950 = ADVANCED_FACE ( 'NONE', ( #12984 ), #3300, .T. ) ;
#46951 = CARTESIAN_POINT ( 'NONE',  ( 17.96595504107422059, -32.45848243737152217, -34.77490583097451093 ) ) ;
#46952 = AXIS2_PLACEMENT_3D ( 'NONE', #50416, #14246, #30472 ) ;
#46953 = AXIS2_PLACEMENT_3D ( 'NONE', #37385, #2723, #50423 ) ;
#46954 = CARTESIAN_POINT ( 'NONE',  ( 7.996487269003661247, -16.94458100238550102, -58.74082357793219700 ) ) ;
#46955 = CARTESIAN_POINT ( 'NONE',  ( -30.36606260230379917, -15.61618894467929941, 11.84999999999999964 ) ) ;
#46956 = CARTESIAN_POINT ( 'NONE',  ( 27.13393739769620083, -38.61618894467930119, -84.65000000000000568 ) ) ;
#46957 = ORIENTED_EDGE ( 'NONE', *, *, #3370, .T. ) ;
#46958 = EDGE_CURVE ( 'NONE', #30218, #25861, #49459, .T. ) ;
#46959 = ORIENTED_EDGE ( 'NONE', *, *, #26755, .T. ) ;
#46960 = CARTESIAN_POINT ( 'NONE',  ( -22.84309005266754511, -14.77827754098507818, -54.74605632281347312 ) ) ;
#46961 = CARTESIAN_POINT ( 'NONE',  ( 9.100096492641728929, -13.16022153293940100, -59.33958724536140039 ) ) ;
#46962 = CARTESIAN_POINT ( 'NONE',  ( 54.55527866260889880, 13.97782061053390024, -14.50547701147139890 ) ) ;
#46963 = CARTESIAN_POINT ( 'NONE',  ( 11.29194847953979952, -21.71414834165970120, -32.14999999999999858 ) ) ;
#46964 = LINE ( 'NONE', #50876, #19811 ) ;
#46965 = LINE ( 'NONE', #39595, #37640 ) ;
#46966 = B_SPLINE_CURVE_WITH_KNOTS ( 'NONE', 3,
 ( #44787, #35885, #28006, #40338, #8371, #494, #12564, #8890, #45045, #44013 ),
 .UNSPECIFIED., .F., .F.,
 ( 4, 2, 2, 2, 4 ),
 ( 0.000000000000000000, 0.2500000000000000000, 0.5000000000000000000, 0.7500000000000000000, 1.000000000000000000 ),
 .UNSPECIFIED. ) ;
#46967 = FACE_OUTER_BOUND ( 'NONE', #27718, .T. ) ;
#46968 = B_SPLINE_CURVE_WITH_KNOTS ( 'NONE', 3,
 ( #49022, #8653, #20685, #8922, #24868, #40879, #13125, #30359, #41393, #5509, #49787, #30102, #41655, #21717, #18063, #49537, #10472, #22496, #26427, #33778, #42445, #13631, #25905, #29589, #5758 ),
 .UNSPECIFIED., .F., .F.,
 ( 4, 3, 3, 3, 3, 3, 3, 3, 4 ),
 ( -0.0003379885557460000044, 0.000000000000000000, 0.01174556080967900130, 0.02341952721554300260, 0.03417459637594329885, 0.04370164535764300279, 0.05433935653199269827, 0.06272590451755999386, 0.06880987158481699506 ),
 .UNSPECIFIED. ) ;
#46969 = CARTESIAN_POINT ( 'NONE',  ( 12.24533245416119875, 33.66790095091289459, -16.17634614694899753 ) ) ;
#46970 = EDGE_CURVE ( 'NONE', #22246, #26340, #9144, .T. ) ;
#46971 = CARTESIAN_POINT ( 'NONE',  ( 10.48770214978459947, -9.607632692615419856, -58.76756083737620173 ) ) ;
#46972 = CARTESIAN_POINT ( 'NONE',  ( 22.24965316085219769, -20.21082810026819843, -32.14999999999999858 ) ) ;
#46973 = CARTESIAN_POINT ( 'NONE',  ( 54.01624284205600190, -50.84298546714590117, -76.06981002096979694 ) ) ;
#46975 = CARTESIAN_POINT ( 'NONE',  ( 10.72251786782789829, -11.45764625195264763, -59.66113601203608141 ) ) ;
#46974 = CARTESIAN_POINT ( 'NONE',  ( -9.775776935431979453, 11.10229679186929985, -4.376631905210299323 ) ) ;
#46976 = CARTESIAN_POINT ( 'NONE',  ( 65.13393739769620083, 1.383811055320669947, -65.65000000000000568 ) ) ;
#46977 = CARTESIAN_POINT ( 'NONE',  ( 44.13393739769620083, 4.883811055320659733, -35.14999999999999858 ) ) ;
#46978 = ORIENTED_EDGE ( 'NONE', *, *, #13021, .T. ) ;
#46979 = CARTESIAN_POINT ( 'NONE',  ( -7.651755816370680030, -45.25221342018689796, -4.961742078189089966 ) ) ;
#46980 = AXIS2_PLACEMENT_3D ( 'NONE', #35508, #50466, #30525 ) ;
#46981 = CARTESIAN_POINT ( 'NONE',  ( 47.53086264803540217, 23.35184965363709964, -54.93563586120320252 ) ) ;
#46982 = CARTESIAN_POINT ( 'NONE',  ( 45.24652675828470194, -45.11233960980349877, -7.238436661000799965 ) ) ;
#46983 = CARTESIAN_POINT ( 'NONE',  ( 16.13393739769620083, -15.61618894467929941, -28.45282021618999835 ) ) ;
#46984 = CARTESIAN_POINT ( 'NONE',  ( 61.50420652560170254, 14.14157561437649946, -47.35413546943329521 ) ) ;
#46985 = CIRCLE ( 'NONE', #41126, 13.50000000000000000 ) ;
#46986 = CARTESIAN_POINT ( 'NONE',  ( 11.43875273179329888, 33.77160878647529785, -16.70124317896340216 ) ) ;
#46987 = CARTESIAN_POINT ( 'NONE',  ( 51.12541109834690189, 17.80355093173099945, -76.44562399623239912 ) ) ;
#46988 = CARTESIAN_POINT ( 'NONE',  ( 52.88731326962020063, 18.39838686409170165, -48.71031098948949989 ) ) ;
#46989 = FACE_OUTER_BOUND ( 'NONE', #28796, .T. ) ;
#46990 = CARTESIAN_POINT ( 'NONE',  ( 52.98014239974310158, -49.58212897128409935, -48.77045029443840463 ) ) ;
#46991 = CARTESIAN_POINT ( 'NONE',  ( 55.58239951895799891, 15.93248589216560163, -26.45503902670689911 ) ) ;
#46992 = CARTESIAN_POINT ( 'NONE',  ( 51.37525108058719070, 21.43002075209610169, -53.68096604571569941 ) ) ;
#46993 = CARTESIAN_POINT ( 'NONE',  ( 11.13393739769619906, -63.52234721269329754, -43.76018303787720498 ) ) ;
#46994 = CARTESIAN_POINT ( 'NONE',  ( 52.95065142214180298, 18.41081157851500194, -49.05053735721260466 ) ) ;
#46995 = CARTESIAN_POINT ( 'NONE',  ( 64.42629863252790301, -31.83020107878950355, -17.29446360647740022 ) ) ;
#46997 = ADVANCED_FACE ( 'NONE', ( #41518 ), #50165, .T. ) ;
#46996 = CARTESIAN_POINT ( 'NONE',  ( 71.42298070439039748, 0.9242073871622918935, -60.63177898966700496 ) ) ;
#46998 = CARTESIAN_POINT ( 'NONE',  ( 11.13393739769619906, 32.17451011075910117, -43.75199058894809667 ) ) ;
#46999 = CARTESIAN_POINT ( 'NONE',  ( 72.29385319554739908, 1.443559558797639975, -61.62614672395329762 ) ) ;
#47000 = EDGE_CURVE ( 'NONE', #17463, #31353, #49334, .T. ) ;
#47001 = CARTESIAN_POINT ( 'NONE',  ( 31.13393739769620083, -36.11618894467930119, -81.65000000000000568 ) ) ;
#47002 = EDGE_LOOP ( 'NONE', ( #36651, #4182, #16703, #29847 ) ) ;
#47003 = VERTEX_POINT ( 'NONE', #22102 ) ;
#47004 = CARTESIAN_POINT ( 'NONE',  ( 42.78018059643970616, 11.47668021806869909, -3.187564294433590462 ) ) ;
#47005 = CARTESIAN_POINT ( 'NONE',  ( 49.22133579550766314, -2.537587427789457450, -15.68296696295392501 ) ) ;
#47006 = EDGE_LOOP ( 'NONE', ( #21937, #35655 ) ) ;
#47007 = CARTESIAN_POINT ( 'NONE',  ( 10.93332211232449858, -63.42973977545160125, -44.88523379654579770 ) ) ;
#47008 = CARTESIAN_POINT ( 'NONE',  ( 57.62157700287180262, -45.13389161508140290, -25.55380843324740070 ) ) ;
#47009 = CARTESIAN_POINT ( 'NONE',  ( 21.67357473421246183, -21.26394646704419600, -77.76073867017645114 ) ) ;
#47010 = CARTESIAN_POINT ( 'NONE',  ( 63.53329261246669546, 1.393731187554809958, -62.48946499964799983 ) ) ;
#47011 = ORIENTED_EDGE ( 'NONE', *, *, #30064, .T. ) ;
#47012 = CARTESIAN_POINT ( 'NONE',  ( 11.08507654941954534, 33.73697186712689700, -23.09805566017817569 ) ) ;
#47013 = CARTESIAN_POINT ( 'NONE',  ( 43.03331702636307199, 6.550456568673448388, -75.15310059331962123 ) ) ;
#47014 = CARTESIAN_POINT ( 'NONE',  ( 68.13393739769620083, 0.8838110553206759423, -65.65000000000000568 ) ) ;
#47015 = ORIENTED_EDGE ( 'NONE', *, *, #8252, .F. ) ;
#47016 = CARTESIAN_POINT ( 'NONE',  ( 22.90741988437979515, -20.31753503473960265, -37.98546363926389802 ) ) ;
#47017 = CARTESIAN_POINT ( 'NONE',  ( 16.13393739769620083, -15.61618894467929941, -54.64999999999999858 ) ) ;
#47018 = DIRECTION ( 'NONE',  ( 0.000000000000000000, 0.000000000000000000, 1.000000000000000000 ) ) ;
#47019 = EDGE_CURVE ( 'NONE', #8526, #23591, #50996, .T. ) ;
#47020 = CARTESIAN_POINT ( 'NONE',  ( 59.40244065973389809, -28.47955681903010117, -15.68910098019369848 ) ) ;
#47021 = AXIS2_PLACEMENT_3D ( 'NONE', #20698, #5002, #5526 ) ;
#47022 = CARTESIAN_POINT ( 'NONE',  ( 14.35343152256950994, 19.90989047429600944, -74.52173647802527512 ) ) ;
#47023 = CARTESIAN_POINT ( 'NONE',  ( 46.98322821459649390, -54.10563643341230033, -75.65564156953989539 ) ) ;
#47024 = AXIS2_PLACEMENT_3D ( 'NONE', #19182, #35163, #40133 ) ;
#47025 = CARTESIAN_POINT ( 'NONE',  ( 55.78773384471490004, 14.70281777721210048, -17.21511389756160071 ) ) ;
#47026 = AXIS2_PLACEMENT_3D ( 'NONE', #20250, #36242, #16336 ) ;
#47027 = CARTESIAN_POINT ( 'NONE',  ( 9.125156155671129810, 23.76650935141284648, -46.59639583156063480 ) ) ;
#47028 = CARTESIAN_POINT ( 'NONE',  ( 84.14547009360870788, -44.02225889889389521, -47.04794573760770504 ) ) ;
#47029 = CARTESIAN_POINT ( 'NONE',  ( 61.72354608828829470, 13.88380460775019998, -28.15154712750929988 ) ) ;
#47030 = EDGE_CURVE ( 'NONE', #40270, #2647, #13736, .T. ) ;
#47031 = CARTESIAN_POINT ( 'NONE',  ( 21.23527585712999866, -9.138607094074950865, -37.22001158807159271 ) ) ;
#47032 = ORIENTED_EDGE ( 'NONE', *, *, #42556, .F. ) ;
#47034 = EDGE_CURVE ( 'NONE', #47312, #25918, #38426, .T. ) ;
#47033 = CARTESIAN_POINT ( 'NONE',  ( 53.11151013220920447, -49.41761562391879892, -27.57048291557959985 ) ) ;
#47035 = CARTESIAN_POINT ( 'NONE',  ( 9.785108495119239080, -62.20228083952999754, -13.76464713449209931 ) ) ;
#47036 = CARTESIAN_POINT ( 'NONE',  ( 76.39184943767510561, -14.06485864167870048, -12.76139016365400103 ) ) ;
#47037 = CARTESIAN_POINT ( 'NONE',  ( 75.06368319349118678, 13.82630467214183412, -14.84994213268719498 ) ) ;
#47038 = DIRECTION ( 'NONE',  ( -1.000000000000000000, -5.465567116091310088E-15, 0.000000000000000000 ) ) ;
#47039 = CARTESIAN_POINT ( 'NONE',  ( 68.13393739769620083, -38.11618894467930119, -73.25000000000000000 ) ) ;
#47040 = CARTESIAN_POINT ( 'NONE',  ( 57.55751162087899786, 18.85811933572220056, -52.57651812407429759 ) ) ;
#47041 = CARTESIAN_POINT ( 'NONE',  ( 57.44002002155969677, -50.11795781616180534, -52.60481300423919748 ) ) ;
#47042 = CARTESIAN_POINT ( 'NONE',  ( 41.78486011480440254, 12.44044499274069970, -3.688051965452270320 ) ) ;
#47043 = CARTESIAN_POINT ( 'NONE',  ( 8.223528471986069732, -15.61608932669300032, -46.79233150823699816 ) ) ;
#47044 = CARTESIAN_POINT ( 'NONE',  ( 62.35658816052890074, -45.11618894467940066, -11.77117279798510019 ) ) ;
#47045 = CARTESIAN_POINT ( 'NONE',  ( 60.24058964203589994, -45.77817723718830223, -47.32689780713820227 ) ) ;
#47046 = CARTESIAN_POINT ( 'NONE',  ( -6.434040441868821958, -15.02156145381371388, 4.943674098299959851 ) ) ;
#47047 = CARTESIAN_POINT ( 'NONE',  ( 104.6856170952509757, -28.80002732851810521, -65.65000000000000568 ) ) ;
#47048 = CARTESIAN_POINT ( 'NONE',  ( 18.33110477860099863, -51.54257389744909545, -75.18091805976320074 ) ) ;
#47049 = CARTESIAN_POINT ( 'NONE',  ( 50.26724122796470340, -44.37275934281500156, -6.890686952535750365 ) ) ;
#47050 = ADVANCED_FACE ( 'NONE', ( #2460 ), #27574, .F. ) ;
#47051 = AXIS2_PLACEMENT_3D ( 'NONE', #8285, #35554, #51793 ) ;
#47052 = CARTESIAN_POINT ( 'NONE',  ( 22.26809483981789839, -19.84452275524870046, -69.25944751885360517 ) ) ;
#47053 = CARTESIAN_POINT ( 'NONE',  ( 63.86577392472210590, 1.451792515613489876, -61.80022504404329453 ) ) ;
#47054 = ORIENTED_EDGE ( 'NONE', *, *, #4554, .F. ) ;
#47055 = LINE ( 'NONE', #3794, #20876 ) ;
#47056 = AXIS2_PLACEMENT_3D ( 'NONE', #16532, #16027, #15768 ) ;
#47057 = CARTESIAN_POINT ( 'NONE',  ( 60.68789125469650259, -45.76122483411000275, -47.75606074947319968 ) ) ;
#47058 = CARTESIAN_POINT ( 'NONE',  ( 73.11081010690790549, 1.190292248953970011, -68.82164347790129000 ) ) ;
#47059 = CARTESIAN_POINT ( 'NONE',  ( 19.54197251953754133, -9.703303650694202531, -74.11948689072868035 ) ) ;
#47060 = CARTESIAN_POINT ( 'NONE',  ( 41.81949136886859719, -45.55672709288079858, -6.527086829740709639 ) ) ;
#47061 = EDGE_CURVE ( 'NONE', #13116, #35078, #18185, .T. ) ;
#47062 = ORIENTED_EDGE ( 'NONE', *, *, #51700, .F. ) ;
#47063 = CARTESIAN_POINT ( 'NONE',  ( 17.84878478542360014, 21.14718688187949880, -75.96082109999758814 ) ) ;
#47064 = ORIENTED_EDGE ( 'NONE', *, *, #2678, .T. ) ;
#47065 = ORIENTED_EDGE ( 'NONE', *, *, #51156, .F. ) ;
#47066 = ORIENTED_EDGE ( 'NONE', *, *, #7531, .T. ) ;
#47067 = CARTESIAN_POINT ( 'NONE',  ( 56.29021670269609956, -45.11618894467940066, -14.97294918829250143 ) ) ;
#47068 = CARTESIAN_POINT ( 'NONE',  ( 23.59606912666399836, -14.83744389001519970, -81.23899999999999011 ) ) ;
#47069 = B_SPLINE_CURVE_WITH_KNOTS ( 'NONE', 3,
 ( #37183, #25875, #49250, #36644, #45046, #750, #9149, #32699, #25100, #12828, #42413, #47131, #10961, #50278, #2053, #30068, #22980, #14365, #7029, #18804, #11217, #34784, #18549, #18284, #19064, #42675, #50531, #14622 ),
 .UNSPECIFIED., .F., .F.,
 ( 4, 3, 3, 3, 3, 3, 3, 3, 3, 4 ),
 ( -0.9179856196245679278, -0.8858225628240299354, -0.7263688044477000227, -0.6319066474211799678, -0.6008308638451469452, -0.4562725788532379645, -0.3116808554209890003, -0.1741802918957590096, -0.08002528894982974261, 1.110223024625156540E-14 ),
 .UNSPECIFIED. ) ;
#47070 = DIRECTION ( 'NONE',  ( -1.000000000000000000, 0.000000000000000000, 0.000000000000000000 ) ) ;
#47071 = ORIENTED_EDGE ( 'NONE', *, *, #6028, .F. ) ;
#47072 = ORIENTED_EDGE ( 'NONE', *, *, #3770, .T. ) ;
#47073 = CARTESIAN_POINT ( 'NONE',  ( 64.93393739769619799, 10.88381105532070059, -61.94999999999999574 ) ) ;
#47074 = DIRECTION ( 'NONE',  ( 0.000000000000000000, 1.000000000000000000, 0.000000000000000000 ) ) ;
#47075 = VERTEX_POINT ( 'NONE', #21583 ) ;
#47076 = CARTESIAN_POINT ( 'NONE',  ( 65.46029542295769943, -29.76883965895079953, -16.55376543218019947 ) ) ;
#47077 = CARTESIAN_POINT ( 'NONE',  ( 52.57481654442310059, -51.43204889509869560, -75.83555718502590537 ) ) ;
#47078 = CARTESIAN_POINT ( 'NONE',  ( 60.42999794199359798, 14.45817062996879976, -47.35267888851409879 ) ) ;
#47079 = CARTESIAN_POINT ( 'NONE',  ( 53.02886665414099809, -49.60598562230889996, -49.08317483300949391 ) ) ;
#47080 = DIRECTION ( 'NONE',  ( 0.000000000000000000, 0.000000000000000000, 1.000000000000000000 ) ) ;
#47081 = FACE_OUTER_BOUND ( 'NONE', #40205, .T. ) ;
#47082 = CARTESIAN_POINT ( 'NONE',  ( 68.13393739769618662, -30.31618894467939995, -65.65000000000000568 ) ) ;
#47083 = CARTESIAN_POINT ( 'NONE',  ( -6.439182911200170167, 15.15458290544269992, -5.455094394028799698 ) ) ;
#47084 = AXIS2_PLACEMENT_3D ( 'NONE', #444, #27706, #15415 ) ;
#47085 = CARTESIAN_POINT ( 'NONE',  ( 33.13393739769620083, -38.61618894467930119, -72.14999999999999147 ) ) ;
#47086 = CARTESIAN_POINT ( 'NONE',  ( 9.366359996283680545, -15.61618532483699973, -43.84717978381009118 ) ) ;
#47087 = CARTESIAN_POINT ( 'NONE',  ( 15.00841818149010010, -23.38278116244979898, -49.83331551772699441 ) ) ;
#47088 = ORIENTED_EDGE ( 'NONE', *, *, #20137, .T. ) ;
#47090 = ADVANCED_FACE ( 'NONE', ( #34152 ), #50679, .T. ) ;
#47089 = CARTESIAN_POINT ( 'NONE',  ( -4.666062602402590187, -15.61618894541809865, -10.44999999999999929 ) ) ;
#47091 = CARTESIAN_POINT ( 'NONE',  ( 57.49777519800270653, 18.87230500023909840, -52.59199339445650168 ) ) ;
#47092 = CARTESIAN_POINT ( 'NONE',  ( 71.95736036617928733, 1.400155911913200102, -70.02962653331499610 ) ) ;
#47093 = EDGE_CURVE ( 'NONE', #11926, #30658, #26034, .T. ) ;
#47094 = CARTESIAN_POINT ( 'NONE',  ( 45.10073672284692492, -40.03758267129227022, -61.32363707965989619 ) ) ;
#47095 = CARTESIAN_POINT ( 'NONE',  ( 71.71126032029680175, -47.11618894467930119, -46.37203261889099792 ) ) ;
#47096 = CARTESIAN_POINT ( 'NONE',  ( 22.27218754053109961, 22.60556764129909979, -34.69483829921999529 ) ) ;
#47097 = SURFACE_STYLE_FILL_AREA ( #43155 ) ;
#47098 = CARTESIAN_POINT ( 'NONE',  ( 12.71325777259860068, -22.74941205225429997, -32.14999999999999858 ) ) ;
#47099 = CARTESIAN_POINT ( 'NONE',  ( 55.98803936394586600, 22.91052256907554963, 17.35000000000000142 ) ) ;
#47100 = CARTESIAN_POINT ( 'NONE',  ( 48.21059767299840360, -54.29128262287709816, -55.22668602961379491 ) ) ;
#47101 = CARTESIAN_POINT ( 'NONE',  ( 18.38973105523400164, -21.99613282959019500, -81.23899999999999011 ) ) ;
#47102 = CARTESIAN_POINT ( 'NONE',  ( -2.623662905471100260, -48.66391853184789795, -4.296538310234220504 ) ) ;
#47103 = CARTESIAN_POINT ( 'NONE',  ( 15.09834328865568942, -7.705194580850375452, -71.25065062966832841 ) ) ;
#47104 = ORIENTED_EDGE ( 'NONE', *, *, #49527, .T. ) ;
#47105 = CARTESIAN_POINT ( 'NONE',  ( 10.65555890294879937, -10.56702432004940029, -36.30437219638799462 ) ) ;
#47106 =( BOUNDED_CURVE ( )  B_SPLINE_CURVE ( 3, ( #21339, #20821, #5128, #17430 ),
 .UNSPECIFIED., .F., .T. ) 
 B_SPLINE_CURVE_WITH_KNOTS ( ( 4, 4 ),
 ( 4.712388980384782045, 5.497787143782128183 ),
 .UNSPECIFIED. ) 
 CURVE ( )  GEOMETRIC_REPRESENTATION_ITEM ( )  RATIONAL_B_SPLINE_CURVE ( ( 1.000000000000000000, 0.9492530216742041116, 0.9492530216742041116, 1.000000000000000000 ) ) 
 REPRESENTATION_ITEM ( '' )  );
#47107 = EDGE_LOOP ( 'NONE', ( #45541, #38283, #44195, #3021 ) ) ;
#47108 = CARTESIAN_POINT ( 'NONE',  ( 71.31509885739851029, 1.369976237678190101, -70.34495568738229565 ) ) ;
#47109 = CARTESIAN_POINT ( 'NONE',  ( 24.04525281611314824, -15.61618915252426376, -57.50766930885080086 ) ) ;
#47110 = CARTESIAN_POINT ( 'NONE',  ( 57.68257350692169894, -47.11839356109889820, -47.67368955113449402 ) ) ;
#47111 = DIRECTION ( 'NONE',  ( 0.000000000000000000, 0.000000000000000000, 1.000000000000000000 ) ) ;
#47113 = CARTESIAN_POINT ( 'NONE',  ( 9.367334447929739127, -15.61631861598680082, -57.84717978380999170 ) ) ;
#47112 = DIRECTION ( 'NONE',  ( 0.000000000000000000, 0.000000000000000000, 1.000000000000000000 ) ) ;
#47114 = FACE_OUTER_BOUND ( 'NONE', #24299, .T. ) ;
#47115 = CARTESIAN_POINT ( 'NONE',  ( 14.06332941558105176, -23.32130738014068427, -42.09100129603611151 ) ) ;
#47116 = DIRECTION ( 'NONE',  ( 0.000000000000000000, 0.000000000000000000, -1.000000000000000000 ) ) ;
#47117 = EDGE_CURVE ( 'NONE', #45466, #15596, #32587, .T. ) ;
#47118 = ORIENTED_EDGE ( 'NONE', *, *, #18128, .F. ) ;
#47119 = CARTESIAN_POINT ( 'NONE',  ( 0.06741163554565170191, 19.71662681832729902, -34.75842043174770168 ) ) ;
#47120 = ORIENTED_EDGE ( 'NONE', *, *, #15240, .T. ) ;
#47121 = ORIENTED_EDGE ( 'NONE', *, *, #42111, .F. ) ;
#47122 = CARTESIAN_POINT ( 'NONE',  ( 53.63393739769619373, -62.82329572586585442, 17.05710678118654400 ) ) ;
#47123 = DIRECTION ( 'NONE',  ( -0.1594746274825657728, 0.3043827052124084553, -0.9391054317577303134 ) ) ;
#47124 = AXIS2_PLACEMENT_3D ( 'NONE', #48934, #37379, #13035 ) ;
#47125 = CARTESIAN_POINT ( 'NONE',  ( 13.00893739761190027, 34.28605925116320208, -47.75434321210310173 ) ) ;
#47126 = CARTESIAN_POINT ( 'NONE',  ( 13.00893739769619906, -65.51843714052719747, -47.75434321273180416 ) ) ;
#47127 = VECTOR ( 'NONE', #46047, 1000.000000000000000 ) ;
#47128 = VERTEX_POINT ( 'NONE', #18440 ) ;
#47129 = EDGE_LOOP ( 'NONE', ( #48179, #49776, #43910, #19053, #49167 ) ) ;
#47130 = CARTESIAN_POINT ( 'NONE',  ( 52.85039779125390424, 21.08368931838850102, -54.40094741851120119 ) ) ;
#47131 = CARTESIAN_POINT ( 'NONE',  ( 57.06093750417669952, 14.65527943800320010, -26.24896182640730302 ) ) ;
#47132 = CARTESIAN_POINT ( 'NONE',  ( 24.22410734144567357, -9.738336421754578254, -5.966499999999999915 ) ) ;
#47133 = CARTESIAN_POINT ( 'NONE',  ( 18.20216584027211226, -9.151158977368147873, -46.05145469637805888 ) ) ;
#47134 = CARTESIAN_POINT ( 'NONE',  ( 60.94255391806049715, -0.9960295973751170928, -16.13088049791909739 ) ) ;
#47135 = CARTESIAN_POINT ( 'NONE',  ( 0.1457841021255935343, -15.61618894467929941, -34.68167779225149161 ) ) ;
#47136 = ORIENTED_EDGE ( 'NONE', *, *, #17260, .F. ) ;
#47137 = PLANE ( 'NONE',  #32445 ) ;
#47138 = CARTESIAN_POINT ( 'NONE',  ( 72.18749078828946608, 11.23736444591397543, -62.44999999999999574 ) ) ;
#47139 = CARTESIAN_POINT ( 'NONE',  ( 14.36277846218990994, -9.025292797381190724, -51.86948580630411954 ) ) ;
#47140 = CARTESIAN_POINT ( 'NONE',  ( 58.40467996479630131, -46.88273201699870185, -48.03872346596099874 ) ) ;
#47141 = CARTESIAN_POINT ( 'NONE',  ( 23.57355577660240087, -13.11842475088059956, -43.90938957849549951 ) ) ;
#47142 = CARTESIAN_POINT ( 'NONE',  ( 13.44518348434099941, -50.59875081391439977, -21.34306233502189798 ) ) ;
#47143 = VECTOR ( 'NONE', #44684, 1000.000000000000000 ) ;
#47144 = CARTESIAN_POINT ( 'NONE',  ( 85.66799001034409855, 19.38381105532069881, -61.58097075742929860 ) ) ;
#47145 = CARTESIAN_POINT ( 'NONE',  ( 56.98602380624170394, 13.94694869911280044, -17.71226892537560005 ) ) ;
#47146 = CARTESIAN_POINT ( 'NONE',  ( 61.31744649544350523, -45.31589417655599306, -47.18592553472910822 ) ) ;
#47147 = CARTESIAN_POINT ( 'NONE',  ( 56.57438608668749680, -50.73277124350089906, -53.83822343189740423 ) ) ;
#47148 = CARTESIAN_POINT ( 'NONE',  ( 14.72053854714299881, -22.52595470508729747, -39.41140439840899745 ) ) ;
#47149 = CARTESIAN_POINT ( 'NONE',  ( 46.98749101202549383, 7.998570365497442936, -34.79644638567071269 ) ) ;
#47150 = ORIENTED_EDGE ( 'NONE', *, *, #11786, .T. ) ;
#47152 = EDGE_CURVE ( 'NONE', #41163, #37879, #29250, .T. ) ;
#47151 = CARTESIAN_POINT ( 'NONE',  ( 68.13393739769618662, -0.5161889446793590519, -51.14999999999999858 ) ) ;
#47153 = CARTESIAN_POINT ( 'NONE',  ( 64.90098062201279561, 0.9219904752505979628, -60.59541050710320320 ) ) ;
#47154 = B_SPLINE_CURVE_WITH_KNOTS ( 'NONE', 3,
 ( #14746, #22846, #22072, #2178 ),
 .UNSPECIFIED., .F., .F.,
 ( 4, 4 ),
 ( 3.672098967893400179, 3.795380006766150061 ),
 .UNSPECIFIED. ) ;
#47155 = CARTESIAN_POINT ( 'NONE',  ( 23.55667557762233244, 17.65459752315667430, -34.82978046822307761 ) ) ;
#47156 = CARTESIAN_POINT ( 'NONE',  ( 14.34417029198879945, -51.11618894467930119, -74.14999999999999147 ) ) ;
#47157 = AXIS2_PLACEMENT_3D ( 'NONE', #36918, #45825, #17017 ) ;
#47158 = CARTESIAN_POINT ( 'NONE',  ( 8.942300673233280150, -49.33122573608360284, -34.65000333295999724 ) ) ;
#47159 = DIRECTION ( 'NONE',  ( 0.000000000000000000, 0.000000000000000000, -1.000000000000000000 ) ) ;
#47160 = CARTESIAN_POINT ( 'NONE',  ( 82.24889378705110232, 13.88381105532070059, -46.39515231851169830 ) ) ;
#47161 = CARTESIAN_POINT ( 'NONE',  ( 21.21190018575672198, -9.527978319518107142, -65.22899277009032915 ) ) ;
#47163 = CARTESIAN_POINT ( 'NONE',  ( 44.83365995299240581, -37.92676521017259716, -66.14348151571169865 ) ) ;
#47162 = CARTESIAN_POINT ( 'NONE',  ( 53.48381654129486407, 19.28794686715378148, -77.13953808112664490 ) ) ;
#47164 = CARTESIAN_POINT ( 'NONE',  ( 8.639346811003365545, -18.23486530003722805, -32.68527743787428363 ) ) ;
#47165 = CARTESIAN_POINT ( 'NONE',  ( 8.222937397696199469, -15.61618894467929941, -32.14999999999999858 ) ) ;
#47166 = EDGE_CURVE ( 'NONE', #16412, #17711, #21946, .T. ) ;
#47167 = ORIENTED_EDGE ( 'NONE', *, *, #15430, .F. ) ;
#47168 = CARTESIAN_POINT ( 'NONE',  ( 53.05608043003729790, -49.55636941894550063, -48.95471306266509970 ) ) ;
#47169 = ORIENTED_EDGE ( 'NONE', *, *, #30493, .T. ) ;
#47170 = CARTESIAN_POINT ( 'NONE',  ( 44.36630888106301995, 6.521024588956093382, -68.44974023162843935 ) ) ;
#47171 = CARTESIAN_POINT ( 'NONE',  ( 19.13393739769620083, -49.61618894467939356, -83.01107220193038927 ) ) ;
#47172 = CARTESIAN_POINT ( 'NONE',  ( 13.97075918456510024, 19.71140667683069836, -21.74703671737670163 ) ) ;
#47173 = CARTESIAN_POINT ( 'NONE',  ( 47.04404845359660214, -39.25010480764659349, -34.85732842610099880 ) ) ;
#47174 = CARTESIAN_POINT ( 'NONE',  ( 21.04132893801929782, -20.68176561141629932, -56.70786862972200026 ) ) ;
#47175 = CARTESIAN_POINT ( 'NONE',  ( 53.11770069264709804, 18.32755088687749989, -49.09731758340100072 ) ) ;
#47176 = CARTESIAN_POINT ( 'NONE',  ( 55.48508049412749443, -46.00754199590999605, -16.66510032532799812 ) ) ;
#47177 = ADVANCED_FACE ( 'NONE', ( #6659 ), #6404, .F. ) ;
#47178 = CARTESIAN_POINT ( 'NONE',  ( 52.61984545813550085, 18.57124442378090023, -27.71374801268470023 ) ) ;
#47179 = AXIS2_PLACEMENT_3D ( 'NONE', #47679, #24559, #19876 ) ;
#47180 = ORIENTED_EDGE ( 'NONE', *, *, #48401, .T. ) ;
#47181 = CARTESIAN_POINT ( 'NONE',  ( 19.78225038875690345, -22.56432254316750274, -37.63360013392959758 ) ) ;
#47182 = EDGE_CURVE ( 'NONE', #31436, #45896, #39917, .T. ) ;
#47183 = ORIENTED_EDGE ( 'NONE', *, *, #32815, .F. ) ;
#47184 = CARTESIAN_POINT ( 'NONE',  ( 10.90442937958139957, -65.00486786560159658, -17.54871756388219950 ) ) ;
#47185 = CARTESIAN_POINT ( 'NONE',  ( 11.42615977560179985, 33.94857426019389379, -47.15336837400249692 ) ) ;
#47186 = CARTESIAN_POINT ( 'NONE',  ( 73.10855093309899644, 0.8936201581567889685, -62.29538467389520662 ) ) ;
#47187 = CYLINDRICAL_SURFACE ( 'NONE', #16812, 20.00000000000000355 ) ;
#47188 = CARTESIAN_POINT ( 'NONE',  ( 52.66149646884395708, -49.78765645775953885, -48.73888008360702173 ) ) ;
#47189 = CARTESIAN_POINT ( 'NONE',  ( 78.22251691734010137, 1.883811055320649963, -20.65000000000000213 ) ) ;
#47190 = CARTESIAN_POINT ( 'NONE',  ( 53.27999729874670010, -52.01684321318150239, -53.62834481722440216 ) ) ;
#47191 = VERTEX_POINT ( 'NONE', #43847 ) ;
#47192 = CARTESIAN_POINT ( 'NONE',  ( 61.35881578103422385, 14.29392436355511364, -47.58695754661491861 ) ) ;
#47193 = CARTESIAN_POINT ( 'NONE',  ( 10.14066804511660003, -63.20557169619659987, -45.99409303117819547 ) ) ;
#47194 = CARTESIAN_POINT ( 'NONE',  ( 65.43042069958036677, 17.98087126524680102, -74.20351669811765305 ) ) ;
#47195 = EDGE_LOOP ( 'NONE', ( #13746, #51244, #32337, #25789 ) ) ;
#47196 = CARTESIAN_POINT ( 'NONE',  ( 11.65682018745774862, -64.87102229922230379, -45.04374105511057991 ) ) ;
#47197 = CARTESIAN_POINT ( 'NONE',  ( 57.19888499978009833, 19.03589688392159829, -52.76365438364319260 ) ) ;
#47198 = CARTESIAN_POINT ( 'NONE',  ( 21.75943287738522969, -10.02997240260718392, -49.25881891216832287 ) ) ;
#47199 = CIRCLE ( 'NONE', #38816, 1.000000000000000888 ) ;
#47200 = ORIENTED_EDGE ( 'NONE', *, *, #32159, .F. ) ;
#47201 = CIRCLE ( 'NONE', #47157, 5.499999999999998224 ) ;
#47202 = CARTESIAN_POINT ( 'NONE',  ( 20.99561534953419439, -21.94235425079530089, -35.79933301742941865 ) ) ;
#47203 = DIRECTION ( 'NONE',  ( -0.6911981449639417185, -0.7226652920947607139, 0.000000000000000000 ) ) ;
#47204 = CARTESIAN_POINT ( 'NONE',  ( 83.89200044194980421, 17.38381105532069881, -53.92796738110899923 ) ) ;
#47205 = CARTESIAN_POINT ( 'NONE',  ( 17.16945288656774693, -7.705184376242745437, -69.33399987328904501 ) ) ;
#47206 = CARTESIAN_POINT ( 'NONE',  ( 24.24467483768560072, -17.09897626438820240, -59.84988861282279515 ) ) ;
#47207 = FACE_OUTER_BOUND ( 'NONE', #22595, .T. ) ;
#47208 = CARTESIAN_POINT ( 'NONE',  ( 46.43430893930594294, -38.19702260607925837, -58.14814218777431165 ) ) ;
#47209 = DIRECTION ( 'NONE',  ( 0.000000000000000000, 0.000000000000000000, 1.000000000000000000 ) ) ;
#47210 = VERTEX_POINT ( 'NONE', #19475 ) ;
#47211 = VERTEX_POINT ( 'NONE', #3243 ) ;
#47212 = CARTESIAN_POINT ( 'NONE',  ( 43.09344256554030750, -43.96039878386999789, -5.051331041927119792 ) ) ;
#47213 = CARTESIAN_POINT ( 'NONE',  ( 14.78897567340050045, -8.288312597105930379, -49.67487765559970114 ) ) ;
#47214 = CARTESIAN_POINT ( 'NONE',  ( 53.36461353568410004, -49.48324289032530032, -49.20419813977639478 ) ) ;
#47215 = CARTESIAN_POINT ( 'NONE',  ( 52.95374953453699618, 13.97573486333550008, -13.31304720699000121 ) ) ;
#47216 = TOROIDAL_SURFACE ( 'NONE', #25393, 19.50000000000000000, 0.5000000000000000000 ) ;
#47218 = EDGE_CURVE ( 'NONE', #22335, #29281, #11627, .T. ) ;
#47217 = CARTESIAN_POINT ( 'NONE',  ( 47.13235806812529916, 23.29804346876840171, -75.11910897646329488 ) ) ;
#47219 = CARTESIAN_POINT ( 'NONE',  ( 56.81484139663320576, 20.15189430791300040, -54.62103799614550326 ) ) ;
#47220 = CARTESIAN_POINT ( 'NONE',  ( 24.04463300525956981, -15.61618495692933273, -55.50767188603018809 ) ) ;
#47221 = CARTESIAN_POINT ( 'NONE',  ( 11.84964338388230054, 33.70977198295789634, -16.34215248989290004 ) ) ;
#47222 = CARTESIAN_POINT ( 'NONE',  ( 24.20737599035849996, -13.94217878954719936, -71.44258980755520838 ) ) ;
#47223 = CARTESIAN_POINT ( 'NONE',  ( 21.03039687228480048, -21.66520938706709742, -32.14999999999999858 ) ) ;
#47224 = CARTESIAN_POINT ( 'NONE',  ( 55.15102684342360106, -50.65538451641219808, -76.12015560185260199 ) ) ;
#47226 = CARTESIAN_POINT ( 'NONE',  ( 10.22096080473554558, -12.20830889007442721, -59.61947214002722006 ) ) ;
#47225 = CARTESIAN_POINT ( 'NONE',  ( -7.078151497284870253, 15.05307759385980049, -6.383383382925239324 ) ) ;
#47227 = FACE_OUTER_BOUND ( 'NONE', #18545, .T. ) ;
#47228 = DIRECTION ( 'NONE',  ( 0.000000000000000000, 0.7071067811865492381, -0.7071067811865457964 ) ) ;
#47229 = VECTOR ( 'NONE', #40501, 1000.000000000000000 ) ;
#47230 = ORIENTED_EDGE ( 'NONE', *, *, #836, .F. ) ;
#47231 = CARTESIAN_POINT ( 'NONE',  ( -11.32734370190460105, -41.88171845330919751, -6.430192534648670133 ) ) ;
#47232 = CARTESIAN_POINT ( 'NONE',  ( 47.58873109027090464, 23.32547039982940262, -55.09264702773990052 ) ) ;
#47233 = CARTESIAN_POINT ( 'NONE',  ( 8.330546865915890109, -14.12868128525956202, -64.85222125236775526 ) ) ;
#47234 = CARTESIAN_POINT ( 'NONE',  ( 63.23867883281550206, 0.9065823421260970072, -62.18054194328749418 ) ) ;
#47235 = CARTESIAN_POINT ( 'NONE',  ( 60.90934541243480282, 14.25332586616640107, -47.35593111936199762 ) ) ;
#47236 = CARTESIAN_POINT ( 'NONE',  ( 9.707462416632068880, -11.84695651314819997, -77.40150352786659482 ) ) ;
#47237 = CARTESIAN_POINT ( 'NONE',  ( 51.30983197266640161, 18.29914825542120127, -76.46178133104609742 ) ) ;
#47238 = CARTESIAN_POINT ( 'NONE',  ( 53.20890753634210313, 18.22989461729919825, -48.81584866255500543 ) ) ;
#47239 = DIRECTION ( 'NONE',  ( 0.000000000000000000, 0.000000000000000000, -1.000000000000000000 ) ) ;
#47240 = CARTESIAN_POINT ( 'NONE',  ( 53.18486246474859769, -49.47487039336269987, -48.80133351323340207 ) ) ;
#47241 = CARTESIAN_POINT ( 'NONE',  ( 56.18000000035269892, 15.25008180819560089, -26.28768301911490113 ) ) ;
#47242 = CARTESIAN_POINT ( 'NONE',  ( 51.12251285489129771, 21.70267151109249681, -54.06580525727419939 ) ) ;
#47243 = EDGE_CURVE ( 'NONE', #44797, #26214, #24206, .T. ) ;
#47244 = CARTESIAN_POINT ( 'NONE',  ( 24.02040458163389047, -16.29250541910551320, -61.53487776366242201 ) ) ;
#47245 = CARTESIAN_POINT ( 'NONE',  ( 23.04645858955461435, -11.63205371370243313, -37.62566744954315112 ) ) ;
#47246 = DIRECTION ( 'NONE',  ( 0.000000000000000000, -1.000000000000000000, 0.000000000000000000 ) ) ;
#47247 = CARTESIAN_POINT ( 'NONE',  ( 59.10134146846650083, -28.39131499980770101, -15.65497502716749878 ) ) ;
#47248 = CARTESIAN_POINT ( 'NONE',  ( 71.03155062328740144, 1.383928098097870096, -60.96256459357869772 ) ) ;
#47249 = CARTESIAN_POINT ( 'NONE',  ( 11.13393739769619906, 32.26595438701649243, -43.75820627627399517 ) ) ;
#47250 = CARTESIAN_POINT ( 'NONE',  ( 72.58908507643239716, 1.266076987107020102, -61.73296247052759611 ) ) ;
#47251 = PLANE ( 'NONE',  #22592 ) ;
#47252 = CARTESIAN_POINT ( 'NONE',  ( 20.30127474080349970, -42.11618894467939356, -34.64999999999999858 ) ) ;
#47253 = ORIENTED_EDGE ( 'NONE', *, *, #13678, .F. ) ;
#47254 = VERTEX_POINT ( 'NONE', #11113 ) ;
#47255 = AXIS2_PLACEMENT_3D ( 'NONE', #33635, #25504, #5623 ) ;
#47256 = CARTESIAN_POINT ( 'NONE',  ( 56.39270785951039500, 19.29512406318060158, -52.86271188469099513 ) ) ;
#47257 = CARTESIAN_POINT ( 'NONE',  ( 49.24615177809619837, -28.72712112006723473, -15.65000000390069701 ) ) ;
#47258 = ORIENTED_EDGE ( 'NONE', *, *, #46177, .T. ) ;
#47259 = CARTESIAN_POINT ( 'NONE',  ( 57.54769658797620480, -45.19536826720690215, -25.74814785595830102 ) ) ;
#47260 = CARTESIAN_POINT ( 'NONE',  ( 12.14977014199372007, -22.52869264618974299, -78.17430626959000506 ) ) ;
#47261 = DIRECTION ( 'NONE',  ( 1.000000000000000000, 0.000000000000000000, 0.000000000000000000 ) ) ;
#47262 =( BOUNDED_CURVE ( )  B_SPLINE_CURVE ( 3, ( #42500, #2661, #10785, #42761 ),
 .UNSPECIFIED., .F., .T. ) 
 B_SPLINE_CURVE_WITH_KNOTS ( ( 4, 4 ),
 ( 5.310633862803790350, 6.283185307179586232 ),
 .UNSPECIFIED. ) 
 CURVE ( )  GEOMETRIC_REPRESENTATION_ITEM ( )  RATIONAL_B_SPLINE_CURVE ( ( 1.000000000000000000, 0.9227196513546198631, 0.9227196513546198631, 1.000000000000000000 ) ) 
 REPRESENTATION_ITEM ( '' )  );
#47263 = EDGE_LOOP ( 'NONE', ( #29067, #8771, #16624, #6574 ) ) ;
#47264 = DIRECTION ( 'NONE',  ( 0.000000000000000000, 0.000000000000000000, 1.000000000000000000 ) ) ;
#47265 = CARTESIAN_POINT ( 'NONE',  ( 44.76553362146206894, 6.782212060689038147, -66.49196124640384653 ) ) ;
#47266 = CARTESIAN_POINT ( 'NONE',  ( 11.07146966777600028, 33.73992739275750097, -23.11170492349029715 ) ) ;
#47267 = AXIS2_PLACEMENT_3D ( 'NONE', #12269, #45011, #44233 ) ;
#47268 = ORIENTED_EDGE ( 'NONE', *, *, #3625, .T. ) ;
#47269 = CARTESIAN_POINT ( 'NONE',  ( 49.60975479659560250, -45.11618894467940066, -10.01352555590809956 ) ) ;
#47270 = CARTESIAN_POINT ( 'NONE',  ( 51.77632738753401753, 1.364313919546259690, -18.40931367100264282 ) ) ;
#47271 = AXIS2_PLACEMENT_3D ( 'NONE', #43033, #42517, #34887 ) ;
#47272 = CARTESIAN_POINT ( 'NONE',  ( 8.222920351416638240, -16.35567762970788408, -50.76256645574265747 ) ) ;
#47273 =( NAMED_UNIT ( * ) SI_UNIT ( $, .STERADIAN. ) SOLID_ANGLE_UNIT ( ) );
#47274 = CARTESIAN_POINT ( 'NONE',  ( 59.28498838297480233, -28.11220559536460328, -15.67198671759989814 ) ) ;
#47275 = CARTESIAN_POINT ( 'NONE',  ( 15.24817818853745699, -8.849184231705592651, -63.91115456625989566 ) ) ;
#47276 = CARTESIAN_POINT ( 'NONE',  ( 47.24371072983239372, -54.76060195732999603, -74.17405913703889553 ) ) ;
#47277 = CARTESIAN_POINT ( 'NONE',  ( 8.475754741739530473, -13.90184186731750060, -79.08259497074239164 ) ) ;
#47278 = CARTESIAN_POINT ( 'NONE',  ( 20.29258223004187656, -21.02752873420811852, -36.74448494115042507 ) ) ;
#47279 = CARTESIAN_POINT ( 'NONE',  ( 44.92064326928819895, 14.77810806019170009, -8.851633222648910504 ) ) ;
#47280 = ADVANCED_FACE ( 'NONE', ( #35199 ), #35462, .T. ) ;
#47281 = CARTESIAN_POINT ( 'NONE',  ( 8.784728771152170879, 23.70287936274029761, -46.67204636145419983 ) ) ;
#47282 = ADVANCED_FACE ( 'NONE', ( #19216 ), #39656, .T. ) ;
#47283 = CARTESIAN_POINT ( 'NONE',  ( 84.16059178761608450, -44.05199403092819210, -47.12825410637790213 ) ) ;
#47284 = CARTESIAN_POINT ( 'NONE',  ( 60.89367646889060381, 13.88379791406190122, -26.67319840941520326 ) ) ;
#47285 = ADVANCED_FACE ( 'NONE', ( #7177 ), #18957, .T. ) ;
#47286 = CARTESIAN_POINT ( 'NONE',  ( 21.82199750194000032, -10.20939643101050009, -81.04557435679289767 ) ) ;
#47287 = ORIENTED_EDGE ( 'NONE', *, *, #44030, .F. ) ;
#47288 = CARTESIAN_POINT ( 'NONE',  ( 52.86782176627269791, -49.62820118223199728, -27.93072220815099982 ) ) ;
#47289 = CIRCLE ( 'NONE', #24646, 5.499999999999998224 ) ;
#47290 = CARTESIAN_POINT ( 'NONE',  ( 6.488565178738439521, -58.66849328915790096, -10.99653483109780083 ) ) ;
#47291 = CARTESIAN_POINT ( 'NONE',  ( 76.16277554039029951, -12.50013975853289949, -12.12674910689150032 ) ) ;
#47292 = CARTESIAN_POINT ( 'NONE',  ( 75.29346835912031111, 13.39413235022868065, -14.05117889852984625 ) ) ;
#47293 = CARTESIAN_POINT ( 'NONE',  ( 13.04440776820920078, -50.02432107381629578, -21.04429564000059827 ) ) ;
#47294 = DIRECTION ( 'NONE',  ( 0.000000000000000000, 1.000000000000000000, 0.000000000000000000 ) ) ;
#47295 = CARTESIAN_POINT ( 'NONE',  ( 16.13393739769620083, -38.61618894467930119, -84.65000000000000568 ) ) ;
#47296 = EDGE_CURVE ( 'NONE', #44094, #26084, #44339, .T. ) ;
#47297 = CARTESIAN_POINT ( 'NONE',  ( 82.55449471509389525, -45.62610142152509951, -47.70626815655899833 ) ) ;
#47298 = CARTESIAN_POINT ( 'NONE',  ( 57.28394106512169515, -50.61203249062990039, -53.75940136370459754 ) ) ;
#47299 = CARTESIAN_POINT ( 'NONE',  ( 41.90536141990470043, 12.91317781275290066, -4.781910917352909962 ) ) ;
#47300 = CARTESIAN_POINT ( 'NONE',  ( 49.72648160330889766, -53.64673639094029767, -55.11972614036120177 ) ) ;
#47301 = CARTESIAN_POINT ( 'NONE',  ( 64.21673630462969129, 0.9952277120692989421, -61.10412195540050107 ) ) ;
#47302 = CARTESIAN_POINT ( 'NONE',  ( 56.28816863880509658, -47.87332787221669150, -48.23685133742169739 ) ) ;
#47303 = CARTESIAN_POINT ( 'NONE',  ( 65.43393739769584272, -48.11618894467832064, -70.54999999999975557 ) ) ;
#47304 = VECTOR ( 'NONE', #7510, 1000.000000000000114 ) ;
#47305 = CARTESIAN_POINT ( 'NONE',  ( 9.367462981151710721, -15.61611677545310073, -63.45282021618999124 ) ) ;
#47306 = CARTESIAN_POINT ( 'NONE',  ( 18.06700609687609926, -51.63908721605620400, -75.44171726276898937 ) ) ;
#47308 = EDGE_CURVE ( 'NONE', #37620, #17080, #38215, .T. ) ;
#47307 = CARTESIAN_POINT ( 'NONE',  ( 49.40539548398250247, -53.49785366680099941, -54.15746054658189479 ) ) ;
#47309 = CARTESIAN_POINT ( 'NONE',  ( 11.39453405654320051, -9.867732603346510700, -64.34787379290919773 ) ) ;
#47310 = CARTESIAN_POINT ( 'NONE',  ( 14.22007337546138217, 19.13837226738661101, -20.84587542004114269 ) ) ;
#47311 = CARTESIAN_POINT ( 'NONE',  ( 63.39852073786919817, 1.308983041454369944, -62.28353782724239807 ) ) ;
#47312 = VERTEX_POINT ( 'NONE', #10854 ) ;
#47313 = CARTESIAN_POINT ( 'NONE',  ( 11.13393739769619906, -63.48206547090349972, -24.15000000000000213 ) ) ;
#47314 = CARTESIAN_POINT ( 'NONE',  ( 12.06284766121009966, -63.44323389162830296, -22.25048313876769868 ) ) ;
#47315 = CARTESIAN_POINT ( 'NONE',  ( 72.82769086651219936, 1.383811055320669947, -68.52712657046359368 ) ) ;
#47316 = CARTESIAN_POINT ( 'NONE',  ( 46.11904533366443104, 8.867946641963873944, -56.38094778067191726 ) ) ;
#47317 = CARTESIAN_POINT ( 'NONE',  ( 11.29901709724989978, -9.719023915928469037, -81.23899999999999011 ) ) ;
#47318 = ORIENTED_EDGE ( 'NONE', *, *, #51590, .T. ) ;
#47319 = CARTESIAN_POINT ( 'NONE',  ( 17.62323348321739758, 20.99223335001410007, -75.94942944171690158 ) ) ;
#47320 = VERTEX_POINT ( 'NONE', #7434 ) ;
#47321 = VERTEX_POINT ( 'NONE', #23381 ) ;
#47322 = DIRECTION ( 'NONE',  ( 0.000000000000000000, 0.000000000000000000, -1.000000000000000000 ) ) ;
#47323 = CARTESIAN_POINT ( 'NONE',  ( 23.54267176174619891, -15.98686785723220005, -81.23899999999999011 ) ) ;
#47324 = ADVANCED_FACE ( 'NONE', ( #39404 ), #6065, .T. ) ;
#47325 = ORIENTED_EDGE ( 'NONE', *, *, #20093, .F. ) ;
#47326 = CARTESIAN_POINT ( 'NONE',  ( 6.133937397696199945, -15.61618894467930119, 17.35000000000000142 ) ) ;
#47327 = ORIENTED_EDGE ( 'NONE', *, *, #17194, .T. ) ;
#47328 = CARTESIAN_POINT ( 'NONE',  ( 23.04646809146690956, -11.63207151544812668, -63.62566669017797949 ) ) ;
#47329 = VECTOR ( 'NONE', #36409, 1000.000000000000000 ) ;
#47330 = CARTESIAN_POINT ( 'NONE',  ( 16.13393739769620083, -15.61618894467929941, -14.68999999999999950 ) ) ;
#47331 = ORIENTED_EDGE ( 'NONE', *, *, #24812, .F. ) ;
#47332 = CARTESIAN_POINT ( 'NONE',  ( 44.66807317952414991, 1.931744143413151038, -44.68675940148178682 ) ) ;
#47333 = CARTESIAN_POINT ( 'NONE',  ( 51.52597209567689873, -50.62283699257580594, -76.24693437788890549 ) ) ;
#47334 = CARTESIAN_POINT ( 'NONE',  ( 60.84128266275949670, 14.46818691485590058, -47.72667381315689994 ) ) ;
#47335 = CARTESIAN_POINT ( 'NONE',  ( 15.52232237619649879, 19.54251322374230071, -15.65194197319980063 ) ) ;
#47336 = CARTESIAN_POINT ( 'NONE',  ( 40.92757250301959715, -44.41382921904099845, -3.805845460188720164 ) ) ;
#47337 = CARTESIAN_POINT ( 'NONE',  ( -8.886174488814990724, 13.01408101563770003, -5.600219702328329774 ) ) ;
#47338 = ADVANCED_FACE ( 'NONE', ( #35396 ), #27271, .F. ) ;
#47339 = CARTESIAN_POINT ( 'NONE',  ( 47.18306311723954849, 23.57448638813150765, -74.19778950654082905 ) ) ;
#47340 = DIRECTION ( 'NONE',  ( 0.000000000000000000, 0.000000000000000000, -1.000000000000000000 ) ) ;
#47341 = ADVANCED_FACE ( 'NONE', ( #31696 ), #22553, .F. ) ;
#47342 = CARTESIAN_POINT ( 'NONE',  ( 21.74587401173889845, -10.13048792993660108, -49.04112620709079806 ) ) ;
#47343 = ORIENTED_EDGE ( 'NONE', *, *, #14660, .F. ) ;
#47344 = CARTESIAN_POINT ( 'NONE',  ( 55.55365133010059964, 13.88381105532070059, -14.32025150907159983 ) ) ;
#47345 = CARTESIAN_POINT ( 'NONE',  ( 57.27298807692499594, 19.38381105532069881, -53.86413101184700736 ) ) ;
#47346 = CARTESIAN_POINT ( 'NONE',  ( 11.77497055818396277, -65.42596200258911665, -22.36958828292143764 ) ) ;
#47347 = CARTESIAN_POINT ( 'NONE',  ( 45.86929072264158691, -40.08640120534250428, -57.59292921774597573 ) ) ;
#47348 = CARTESIAN_POINT ( 'NONE',  ( 15.67955243735830173, 19.63025192210979952, -20.14992656220960043 ) ) ;
#47349 = B_SPLINE_CURVE_WITH_KNOTS ( 'NONE', 3,
 ( #45544, #37671, #38722, #10157, #38450, #2818, #41864, #2554, #18531, #18785, #34763, #33977, #50769, #9639, #47363 ),
 .UNSPECIFIED., .F., .F.,
 ( 4, 1, 1, 1, 1, 1, 1, 1, 1, 3, 4 ),
 ( 0.000000000000000000, 0.1110915318836693672, 0.2222019412356212309, 0.3333123505875730808, 0.4444227599395249584, 0.5555331692914780017, 0.6666435786434299349, 0.7777539879953816460, 0.8888643973473335791, 0.9999748066992855122, 1.000000000000000000 ),
 .UNSPECIFIED. ) ;
#47350 = SURFACE_SIDE_STYLE ('',( #47097 ) ) ;
#47351 = AXIS2_PLACEMENT_3D ( 'NONE', #7641, #35918, #11573 ) ;
#47352 = CARTESIAN_POINT ( 'NONE',  ( 48.31539888355000301, -54.23126901101980479, -55.06275371778509964 ) ) ;
#47353 = CIRCLE ( 'NONE', #29742, 5.251829701412240148 ) ;
#47354 = CARTESIAN_POINT ( 'NONE',  ( -26.88703640771693770, -41.87805570297800273, -56.26548710561216637 ) ) ;
#47355 = CARTESIAN_POINT ( 'NONE',  ( 63.63393739769619373, -53.11618894467930119, 11.84999999999999964 ) ) ;
#47356 = CARTESIAN_POINT ( 'NONE',  ( 20.99565159046659701, -21.94232532607928476, -37.79933726366152058 ) ) ;
#47357 = CARTESIAN_POINT ( 'NONE',  ( 38.13393739769620083, -15.61618894467929941, -14.65000000000000036 ) ) ;
#47358 = ORIENTED_EDGE ( 'NONE', *, *, #16521, .F. ) ;
#47359 = CARTESIAN_POINT ( 'NONE',  ( 11.71654021571490034, -21.61563036701890184, -33.76936640235209808 ) ) ;
#47360 = ORIENTED_EDGE ( 'NONE', *, *, #37853, .F. ) ;
#47361 = CARTESIAN_POINT ( 'NONE',  ( 71.46697330897291067, 1.186614556332910020, -70.53308468150621025 ) ) ;
#47362 = CARTESIAN_POINT ( 'NONE',  ( 60.47158259472089981, -45.65949564325300258, -47.26531013111339519 ) ) ;
#47363 = CARTESIAN_POINT ( 'NONE',  ( 82.75389963950189554, 14.36256073625980001, -47.67227237920639737 ) ) ;
#47364 = DIRECTION ( 'NONE',  ( 0.000000000000000000, 0.000000000000000000, 1.000000000000000000 ) ) ;
#47366 = CARTESIAN_POINT ( 'NONE',  ( 14.30191975431828411, 1.226104548012949325, -34.77490583097451093 ) ) ;
#47365 = CARTESIAN_POINT ( 'NONE',  ( 83.36355911687300591, 14.11444734287620051, -47.55049236202179230 ) ) ;
#47367 = DIRECTION ( 'NONE',  ( 1.000000000000000000, 0.000000000000000000, 0.000000000000000000 ) ) ;
#47368 = CARTESIAN_POINT ( 'NONE',  ( 23.04647490150570732, -11.63208424308849409, -67.34099948691266491 ) ) ;
#47369 = ORIENTED_EDGE ( 'NONE', *, *, #45336, .T. ) ;
#47370 = CARTESIAN_POINT ( 'NONE',  ( 68.13393739769618662, 0.9838110553206419473, -80.15000000000000568 ) ) ;
#47371 = ORIENTED_EDGE ( 'NONE', *, *, #1368, .F. ) ;
#47372 = ORIENTED_EDGE ( 'NONE', *, *, #12349, .F. ) ;
#47373 = CARTESIAN_POINT ( 'NONE',  ( 16.13393739769620083, -15.61618894467929941, -40.14999999999999858 ) ) ;
#47374 = CARTESIAN_POINT ( 'NONE',  ( 16.13393739769620083, -15.61618894467929941, -4.296538310234230273 ) ) ;
#47375 = CARTESIAN_POINT ( 'NONE',  ( 76.43224147390343148, -23.40681064887490948, -12.93543775027620590 ) ) ;
#47376 = CARTESIAN_POINT ( 'NONE',  ( 11.39576525640170068, -65.16962161578030077, -47.14206625977179499 ) ) ;
#47377 = AXIS2_PLACEMENT_3D ( 'NONE', #11788, #5470, #29040 ) ;
#47378 = ORIENTED_EDGE ( 'NONE', *, *, #48211, .F. ) ;
#47379 = EDGE_CURVE ( 'NONE', #22075, #47835, #11433, .T. ) ;
#47380 = ORIENTED_EDGE ( 'NONE', *, *, #18309, .F. ) ;
#47381 = CARTESIAN_POINT ( 'NONE',  ( 23.64088771302849068, -18.16524997366306593, -55.61181301324595694 ) ) ;
#47382 = VECTOR ( 'NONE', #41995, 1000.000000000000114 ) ;
#47383 = CARTESIAN_POINT ( 'NONE',  ( 63.00666467042349694, 0.8838110553206759423, -62.53374032209040223 ) ) ;
#47384 = EDGE_CURVE ( 'NONE', #40276, #5858, #35663, .T. ) ;
#47385 = FACE_OUTER_BOUND ( 'NONE', #43184, .T. ) ;
#47386 = LINE ( 'NONE', #22982, #23552 ) ;
#47387 = CARTESIAN_POINT ( 'NONE',  ( 60.11982335476029959, -1.682419521057920031, -15.87057978292740223 ) ) ;
#47388 = CARTESIAN_POINT ( 'NONE',  ( 51.78790344664380285, -49.82581277545029508, -76.67262344587960854 ) ) ;
#47389 = EDGE_CURVE ( 'NONE', #11901, #18483, #40152, .T. ) ;
#47390 = CARTESIAN_POINT ( 'NONE',  ( 19.22157560178254698, 18.51631118994118808, -82.73668660645967066 ) ) ;
#47391 = ORIENTED_EDGE ( 'NONE', *, *, #9648, .T. ) ;
#47392 = FACE_OUTER_BOUND ( 'NONE', #11654, .T. ) ;
#47393 = CARTESIAN_POINT ( 'NONE',  ( 22.46012663862139291, -20.47783394216208919, -48.00066642373527515 ) ) ;
#47394 = DIRECTION ( 'NONE',  ( 0.000000000000000000, -1.000000000000000000, 0.000000000000000000 ) ) ;
#47395 = DIRECTION ( 'NONE',  ( 0.000000000000000000, 0.000000000000000000, -1.000000000000000000 ) ) ;
#47396 = AXIS2_PLACEMENT_3D ( 'NONE', #4403, #35858, #20894 ) ;
#47397 = CARTESIAN_POINT ( 'NONE',  ( 23.75919800905029788, -17.47149166944270249, -50.08846620145769890 ) ) ;
#47398 = AXIS2_PLACEMENT_3D ( 'NONE', #42811, #35182, #46490 ) ;
#47399 = CARTESIAN_POINT ( 'NONE',  ( 12.22498024391630089, -50.02555233757460229, -21.14999999988710400 ) ) ;
#47400 = LINE ( 'NONE', #39778, #32586 ) ;
#47401 = CARTESIAN_POINT ( 'NONE',  ( 57.07557850792819920, 13.89582767481270054, -16.81759313181460058 ) ) ;
#47402 = CARTESIAN_POINT ( 'NONE',  ( 8.942300673232759678, 18.09884784672440006, -34.65000333295999724 ) ) ;
#47403 = CARTESIAN_POINT ( 'NONE',  ( 56.72454650921010000, -50.66101676095649253, -53.46416969206939740 ) ) ;
#47404 = CARTESIAN_POINT ( 'NONE',  ( 22.40972105350460097, -18.83443360286479873, -56.99800709453259628 ) ) ;
#47405 = DIRECTION ( 'NONE',  ( -0.4999999999999995004, 0.8660254037844390407, 0.000000000000000000 ) ) ;
#47406 = EDGE_CURVE ( 'NONE', #47961, #48439, #33079, .T. ) ;
#47407 = ORIENTED_EDGE ( 'NONE', *, *, #30735, .F. ) ;
#47408 = DIRECTION ( 'NONE',  ( 0.000000000000000000, 0.000000000000000000, -1.000000000000000000 ) ) ;
#47409 = CARTESIAN_POINT ( 'NONE',  ( 65.03036676789569981, 1.369613126987639928, -60.92417343964400089 ) ) ;
#47410 = DIRECTION ( 'NONE',  ( 0.000000000000000000, 0.000000000000000000, -1.000000000000000000 ) ) ;
#47411 = CARTESIAN_POINT ( 'NONE',  ( 14.51932309042026503, -51.60941532109461605, -75.47165350116152638 ) ) ;
#47412 =( BOUNDED_CURVE ( )  B_SPLINE_CURVE ( 3, ( #2037, #33983, #30050, #2561 ),
 .UNSPECIFIED., .F., .T. ) 
 B_SPLINE_CURVE_WITH_KNOTS ( ( 4, 4 ),
 ( 1.570796326794901665, 2.356194490192332403 ),
 .UNSPECIFIED. ) 
 CURVE ( )  GEOMETRIC_REPRESENTATION_ITEM ( )  RATIONAL_B_SPLINE_CURVE ( ( 1.000000000000000000, 0.9492530216741933424, 0.9492530216741933424, 1.000000000000000000 ) ) 
 REPRESENTATION_ITEM ( '' )  );
#47413 = CARTESIAN_POINT ( 'NONE',  ( 46.51095038332250198, 13.88381105532070059, -7.695532444495968960 ) ) ;
#47414 = CIRCLE ( 'NONE', #42388, 12.00000000000000000 ) ;
#47415 = FACE_OUTER_BOUND ( 'NONE', #2138, .T. ) ;
#47416 = VECTOR ( 'NONE', #11527, 1000.000000000000000 ) ;
#47417 = CARTESIAN_POINT ( 'NONE',  ( 11.89539497636670085, 34.20383474698349602, -18.11027658847759980 ) ) ;
#47418 = CARTESIAN_POINT ( 'NONE',  ( 72.25791598168270014, 1.028300555801489935, -70.00885842708049722 ) ) ;
#47420 = CARTESIAN_POINT ( 'NONE',  ( 11.33851678214776904, 33.17161558030153401, -24.03999305115578622 ) ) ;
#47419 = CARTESIAN_POINT ( 'NONE',  ( 38.67452568954060155, -37.56081407618430035, -84.65000000000000568 ) ) ;
#47421 = CARTESIAN_POINT ( 'NONE',  ( -6.046668638016009290, -47.40279893552259693, -7.123474707974530418 ) ) ;
#47422 = CARTESIAN_POINT ( 'NONE',  ( 49.51533122679629884, 22.46701370878599846, -54.78532408268279852 ) ) ;
#47423 = ORIENTED_EDGE ( 'NONE', *, *, #34960, .T. ) ;
#47424 = CARTESIAN_POINT ( 'NONE',  ( 52.59421258935810073, -49.83180061336119593, -48.47378032971909789 ) ) ;
#47425 = ORIENTED_EDGE ( 'NONE', *, *, #7986, .T. ) ;
#47426 = CARTESIAN_POINT ( 'NONE',  ( 47.12223953835182755, 6.751577964446205726, -54.64278194131097166 ) ) ;
#47427 = CIRCLE ( 'NONE', #28997, 5.999999999999998224 ) ;
#47428 = CARTESIAN_POINT ( 'NONE',  ( 22.90122612410699077, -15.61618894223031440, -74.45282020639018583 ) ) ;
#47429 = CARTESIAN_POINT ( 'NONE',  ( 82.13853704237929776, -45.25223929932899125, -47.09707863094710945 ) ) ;
#47430 = CARTESIAN_POINT ( 'NONE',  ( 84.41931940662119871, 12.04917885348629980, -47.35294421590279512 ) ) ;
#47431 = CARTESIAN_POINT ( 'NONE',  ( 17.18162999253079803, -22.59077846115649990, -52.90535993866819808 ) ) ;
#47432 = DIRECTION ( 'NONE',  ( 0.000000000000000000, 0.000000000000000000, 1.000000000000000000 ) ) ;
#47433 = CARTESIAN_POINT ( 'NONE',  ( 55.01975381464660586, -46.11950308459810088, -16.15585483520260013 ) ) ;
#47434 = CARTESIAN_POINT ( 'NONE',  ( 46.63393739769619373, -36.11618894467930119, -34.64999999999999858 ) ) ;
#47435 = ORIENTED_EDGE ( 'NONE', *, *, #28683, .T. ) ;
#47436 = CARTESIAN_POINT ( 'NONE',  ( 8.827366647101261066, -18.47988795989260069, -40.16860592796539464 ) ) ;
#47437 = EDGE_LOOP ( 'NONE', ( #17565, #22304 ) ) ;
#47438 = CARTESIAN_POINT ( 'NONE',  ( 11.23165357234419837, -65.23063573490379952, -17.66286047794729797 ) ) ;
#47439 = CARTESIAN_POINT ( 'NONE',  ( 10.25855798689609877, 33.30687331164079978, -46.73983890664589325 ) ) ;
#47440 = CARTESIAN_POINT ( 'NONE',  ( 72.96845534527879806, 1.188860127980290171, -62.23803121388370130 ) ) ;
#47441 = CARTESIAN_POINT ( 'NONE',  ( 48.47947973770610020, -54.28987983540550033, -55.11210649539159334 ) ) ;
#47442 = FACE_OUTER_BOUND ( 'NONE', #4411, .T. ) ;
#47443 = LINE ( 'NONE', #10759, #41837 ) ;
#47444 = ORIENTED_EDGE ( 'NONE', *, *, #11486, .F. ) ;
#47445 = CARTESIAN_POINT ( 'NONE',  ( 8.223069265346360623, -15.61598766837350105, -56.50766849176299189 ) ) ;
#47446 = CARTESIAN_POINT ( 'NONE',  ( 11.13393739769619906, -63.16362662756800006, -43.74366009427609470 ) ) ;
#47447 = EDGE_CURVE ( 'NONE', #40665, #38928, #28069, .T. ) ;
#47448 = CARTESIAN_POINT ( 'NONE',  ( 20.13393739769620083, -28.89524513604070322, -39.64999999999999858 ) ) ;
#47449 = ORIENTED_EDGE ( 'NONE', *, *, #10112, .T. ) ;
#47450 = CARTESIAN_POINT ( 'NONE',  ( 23.96601493904643476, -16.76745162487207352, -43.83877825466511524 ) ) ;
#47451 = CARTESIAN_POINT ( 'NONE',  ( 9.577040858161863568, -11.12070122226039892, -76.69910475397914240 ) ) ;
#47452 = EDGE_CURVE ( 'NONE', #29481, #22521, #20868, .T. ) ;
#47453 = CARTESIAN_POINT ( 'NONE',  ( 17.75165935666287353, -7.846201640880932082, -49.07295956893727151 ) ) ;
#47454 = ORIENTED_EDGE ( 'NONE', *, *, #15850, .T. ) ;
#47455 = CARTESIAN_POINT ( 'NONE',  ( 8.223606718150689332, -15.61618413875730127, -36.50766849176289952 ) ) ;
#47456 = FACE_OUTER_BOUND ( 'NONE', #51366, .T. ) ;
#47458 = CARTESIAN_POINT ( 'NONE',  ( 16.13393739769620083, -15.61618894467929941, -9.392532499999980189 ) ) ;
#47457 = CONICAL_SURFACE ( 'NONE', #25641, 0.6299999999999866818, 0.7853981633974476129 ) ;
#47459 = CARTESIAN_POINT ( 'NONE',  ( 23.83903407973103228, -13.54549564773435222, -69.70900104909422623 ) ) ;
#47460 = CARTESIAN_POINT ( 'NONE',  ( 19.74175079524499665, -8.202255943660620829, -77.43649130894638688 ) ) ;
#47461 = DIRECTION ( 'NONE',  ( 1.000000000000000000, 0.000000000000000000, 0.000000000000000000 ) ) ;
#47462 = CARTESIAN_POINT ( 'NONE',  ( 16.13393739769620083, -15.61618894467929941, -28.45282021618999835 ) ) ;
#47463 = ORIENTED_EDGE ( 'NONE', *, *, #22147, .F. ) ;
#47464 = ORIENTED_EDGE ( 'NONE', *, *, #14713, .T. ) ;
#47465 = CARTESIAN_POINT ( 'NONE',  ( -22.84941414684771388, -15.61618224896967355, -54.74986855478772441 ) ) ;
#47466 = CARTESIAN_POINT ( 'NONE',  ( 23.56515851745149703, -15.08360423362579894, -52.20988344963559769 ) ) ;
#47467 = AXIS2_PLACEMENT_3D ( 'NONE', #15651, #15138, #35301 ) ;
#47468 = DIRECTION ( 'NONE',  ( 0.8090169943749473402, 0.5877852522924732481, 0.000000000000000000 ) ) ;
#47469 = CARTESIAN_POINT ( 'NONE',  ( 29.13393739769619728, -35.78776181993320193, -84.65000000000000568 ) ) ;
#47470 = EDGE_CURVE ( 'NONE', #19682, #35239, #23395, .T. ) ;
#47471 = CARTESIAN_POINT ( 'NONE',  ( 47.32878498007210055, 23.37072882834580057, -74.72254318496639769 ) ) ;
#47472 = ADVANCED_FACE ( 'NONE', ( #43024 ), #39091, .T. ) ;
#47473 = CARTESIAN_POINT ( 'NONE',  ( 0.1375253771463928743, 14.71649224688080082, -34.68482877647384299 ) ) ;
#47474 = DIRECTION ( 'NONE',  ( -0.7226652920947592706, -0.6911981449639433839, 0.000000000000000000 ) ) ;
#47475 = CARTESIAN_POINT ( 'NONE',  ( 12.09242720216389877, 33.69063605648580761, -16.23377612491680111 ) ) ;
#47476 = B_SPLINE_CURVE_WITH_KNOTS ( 'NONE', 3,
 ( #2704, #6635, #22598, #47005, #42023, #26531, #30723, #2435, #18679, #38873, #42282, #50914, #14239, #45956, #34394, #11090, #37832, #27057, #2961, #34652, #43061, #50406, #10050, #26012, #6123, #22079, #50659, #18935, #34916, #51436, #3221, #12118, #40144 ),
 .UNSPECIFIED., .F., .F.,
 ( 4, 2, 2, 1, 2, 2, 2, 2, 2, 2, 1, 2, 2, 2, 2, 2, 1, 4 ),
 ( 0.000000000000000000, 0.06597993765965722013, 0.09896990648948590652, 0.1154648909044010269, 0.1237123831118577544, 0.1319598753193144680, 0.1979398129789769478, 0.2309297818088088539, 0.2474247662237250012, 0.2515485123274531776, 0.2556722584311812985, 0.2639197506386373182, 0.3958796259579234755, 0.4618595636175666375, 0.4948495324473878298, 0.5030970246548429614, 0.5113445168622979820, 0.5278395012772089112 ),
 .UNSPECIFIED. ) ;
#47477 = CARTESIAN_POINT ( 'NONE',  ( 8.322288761255229872, -12.97784357498919938, -74.61134705009999379 ) ) ;
#47478 = CARTESIAN_POINT ( 'NONE',  ( 20.09253040080429997, -22.41528281924199817, -32.14999999999999858 ) ) ;
#47479 = CARTESIAN_POINT ( 'NONE',  ( 54.18612455227970059, -50.67005945099250397, -76.49079485251020571 ) ) ;
#47480 = CARTESIAN_POINT ( 'NONE',  ( -8.714254634004609201, 12.03702151998610148, -4.336387236750419483 ) ) ;
#47481 = CARTESIAN_POINT ( 'NONE',  ( 63.03407832914061260, 0.8840451408750739093, -68.81103260973570457 ) ) ;
#47482 = CARTESIAN_POINT ( 'NONE',  ( 67.78236843376264176, -1.116188944679348483, -17.74895402404429845 ) ) ;
#47483 = ORIENTED_EDGE ( 'NONE', *, *, #36763, .F. ) ;
#47484 = CARTESIAN_POINT ( 'NONE',  ( 53.20889695217059767, -49.46227805200189920, -48.81584933005299831 ) ) ;
#47485 = CARTESIAN_POINT ( 'NONE',  ( 47.66159700762720064, 23.24898935426730162, -54.69403258753950325 ) ) ;
#47486 = CARTESIAN_POINT ( 'NONE',  ( 57.82682226305900741, -45.74154291786189930, -26.33630567069459616 ) ) ;
#47487 = DIRECTION ( 'NONE',  ( -0.000000000000000000, 1.000000000000000000, 0.000000000000000000 ) ) ;
#47488 = CARTESIAN_POINT ( 'NONE',  ( 61.31744659937159980, 14.08351620583249897, -47.18592528150829679 ) ) ;
#47489 = CARTESIAN_POINT ( 'NONE',  ( 20.18579949284930208, -21.86831717169179967, -74.54962200957619700 ) ) ;
#47490 = CARTESIAN_POINT ( 'NONE',  ( 51.67724278084540401, 18.81853346939729832, -76.49491148620110437 ) ) ;
#47491 = CARTESIAN_POINT ( 'NONE',  ( 53.31242401630019145, 18.17684692666709978, -48.83993031500360615 ) ) ;
#47492 = CARTESIAN_POINT ( 'NONE',  ( 24.04490452168148451, -15.61618923948461557, -69.79232899952297942 ) ) ;
#47493 = CARTESIAN_POINT ( 'NONE',  ( -0.1963508450805951933, -45.46408278790535462, -34.93716512309965339 ) ) ;
#47494 = CARTESIAN_POINT ( 'NONE',  ( 68.13393739769624347, 0.8838110553206759423, -71.65000000000000568 ) ) ;
#47495 = CARTESIAN_POINT ( 'NONE',  ( 16.37276388111695624, -23.52373572102649746, -61.99806274663424688 ) ) ;
#47496 = CARTESIAN_POINT ( 'NONE',  ( 17.16946792601238059, -7.705186524535062809, -37.33399987008601073 ) ) ;
#47497 = CARTESIAN_POINT ( 'NONE',  ( 9.366426063424411197, -15.61626247110940113, -71.45282021618990598 ) ) ;
#47498 = CARTESIAN_POINT ( 'NONE',  ( 58.97981359800899526, -28.45462689055629824, -15.64989485168480066 ) ) ;
#47499 = CARTESIAN_POINT ( 'NONE',  ( 71.34267188602969156, 0.8850831926798630178, -60.57999765399179637 ) ) ;
#47500 = CARTESIAN_POINT ( 'NONE',  ( 11.13393739769619906, 32.05275509628890518, -43.74635191486320451 ) ) ;
#47501 = CARTESIAN_POINT ( 'NONE',  ( 72.61057233489319174, 1.185470598955660204, -61.69804660143999797 ) ) ;
#47502 = VECTOR ( 'NONE', #8821, 1000.000000000000114 ) ;
#47503 = DIRECTION ( 'NONE',  ( 0.1686178020941810352, -0.6660492713794512465, -0.7265992051412042407 ) ) ;
#47504 = DIRECTION ( 'NONE',  ( 0.000000000000000000, 1.000000000000000000, 0.000000000000000000 ) ) ;
#47505 = VERTEX_POINT ( 'NONE', #23317 ) ;
#47506 = ORIENTED_EDGE ( 'NONE', *, *, #7969, .T. ) ;
#47507 = CARTESIAN_POINT ( 'NONE',  ( 41.55663457306080488, 12.62725083537310056, -3.466044030332980252 ) ) ;
#47508 = EDGE_CURVE ( 'NONE', #51808, #11818, #19154, .T. ) ;
#47509 = CARTESIAN_POINT ( 'NONE',  ( 9.543101276256674481, -17.38757133593738047, -59.36948685926856939 ) ) ;
#47510 = VERTEX_POINT ( 'NONE', #18893 ) ;
#47511 = DIRECTION ( 'NONE',  ( -0.6676418852213141797, -0.2329255526946994725, -0.7071067811865463515 ) ) ;
#47512 = CARTESIAN_POINT ( 'NONE',  ( 8.222923464767577073, -16.65163797661076472, -78.46599076961739172 ) ) ;
#47513 = DIRECTION ( 'NONE',  ( -1.000000000000000000, 0.000000000000000000, 0.000000000000000000 ) ) ;
#47514 = VERTEX_POINT ( 'NONE', #34614 ) ;
#47515 = CARTESIAN_POINT ( 'NONE',  ( 17.94759653393067467, -22.18343915517746723, -80.86687695485406380 ) ) ;
#47516 = CARTESIAN_POINT ( 'NONE',  ( 44.64206215848041381, 6.767191847450578557, -67.10931550608336238 ) ) ;
#47517 = FACE_OUTER_BOUND ( 'NONE', #40779, .T. ) ;
#47518 = CARTESIAN_POINT ( 'NONE',  ( 8.133937397696209715, 23.57564693985150228, -21.14999999999999858 ) ) ;
#47519 = CARTESIAN_POINT ( 'NONE',  ( 71.33393739769628894, 10.88381105532070059, -61.44999999999999574 ) ) ;
#47520 = CARTESIAN_POINT ( 'NONE',  ( 17.73895862251804800, -23.38184506017118380, -50.22737503043536123 ) ) ;
#47521 = CARTESIAN_POINT ( 'NONE',  ( 22.55207325930935625, -17.84354922411136357, -50.55919571307475735 ) ) ;
#47522 = CARTESIAN_POINT ( 'NONE',  ( 65.43690392504990427, -30.18759754294940123, -16.56995554360160128 ) ) ;
#47523 = CARTESIAN_POINT ( 'NONE',  ( 22.72481167109963351, -13.84494687364363408, -64.36948891632977166 ) ) ;
#47524 = CARTESIAN_POINT ( 'NONE',  ( 47.27157043358619859, -54.25876962900459688, -75.35700034530711378 ) ) ;
#47525 = CARTESIAN_POINT ( 'NONE',  ( 8.380091037990700542, -16.82640141431589953, -74.96321055543440082 ) ) ;
#47526 = CARTESIAN_POINT ( 'NONE',  ( 57.77564497937559906, -28.11618894467929763, -20.65000000000000213 ) ) ;
#47527 = CARTESIAN_POINT ( 'NONE',  ( 41.19620264348169769, 14.26403794320130025, -6.107565110250690488 ) ) ;
#47528 = EDGE_CURVE ( 'NONE', #17711, #24756, #18368, .T. ) ;
#47529 = CARTESIAN_POINT ( 'NONE',  ( 15.05440318628110141, 21.88381105532300097, -76.14999999999999147 ) ) ;
#47530 = CARTESIAN_POINT ( 'NONE',  ( 82.96870692852718321, -45.28007837109379352, -47.29707907477579454 ) ) ;
#47531 = TOROIDAL_SURFACE ( 'NONE', #2330, 19.50000000000000000, 0.5000000000000000000 ) ;
#47532 = DIRECTION ( 'NONE',  ( -0.8732394366197168134, -0.4872913772396139098, 0.000000000000000000 ) ) ;
#47533 = CARTESIAN_POINT ( 'NONE',  ( 13.96167471279819949, -23.57005564816219945, -46.09253186719709561 ) ) ;
#47534 = VERTEX_POINT ( 'NONE', #50617 ) ;
#47535 = CARTESIAN_POINT ( 'NONE',  ( 4.133937397696209715, -8.687985714403833271, -35.01561944896766221 ) ) ;
#47536 = CARTESIAN_POINT ( 'NONE',  ( 16.22101879094850219, -51.07051632261300256, -20.26096174765880065 ) ) ;
#47537 = CARTESIAN_POINT ( 'NONE',  ( 75.15216820663748365, -30.02682016727950298, -11.82535899278000002 ) ) ;
#47538 = AXIS2_PLACEMENT_3D ( 'NONE', #13972, #22329, #10037 ) ;
#47539 = DIRECTION ( 'NONE',  ( 0.000000000000000000, 0.000000000000000000, 1.000000000000000000 ) ) ;
#47540 = DIRECTION ( 'NONE',  ( 0.5198294763375396199, 0.8542087557464956848, -0.01023313914021957947 ) ) ;
#47541 = ORIENTED_EDGE ( 'NONE', *, *, #31307, .F. ) ;
#47542 = CARTESIAN_POINT ( 'NONE',  ( 15.31199894099709979, -16.87369336301570044, -35.14999999999999858 ) ) ;
#47543 = FACE_OUTER_BOUND ( 'NONE', #26576, .T. ) ;
#47544 = DIRECTION ( 'NONE',  ( 0.000000000000000000, 0.000000000000000000, 1.000000000000000000 ) ) ;
#47545 = CARTESIAN_POINT ( 'NONE',  ( 63.17872741171709805, 1.188582381068110205, -62.44003653085279382 ) ) ;
#47546 = CARTESIAN_POINT ( 'NONE',  ( 57.35071418803849497, -50.23458714926779578, -52.74072012029530043 ) ) ;
#47547 = CARTESIAN_POINT ( 'NONE',  ( 42.20562667456769645, 13.08589554890109952, -5.077271921742569916 ) ) ;
#47548 = DIRECTION ( 'NONE',  ( 1.000000000000000000, 0.000000000000000000, 0.000000000000000000 ) ) ;
#47549 = DIRECTION ( 'NONE',  ( 1.000000000000000000, 0.000000000000000000, 0.000000000000000000 ) ) ;
#47550 = CARTESIAN_POINT ( 'NONE',  ( 0.5406133260286669628, -43.55985091651039909, -20.15000000000000213 ) ) ;
#47551 = CARTESIAN_POINT ( 'NONE',  ( -0.1944835411611390841, -20.56321558487172751, -34.93556154945131453 ) ) ;
#47552 = CARTESIAN_POINT ( 'NONE',  ( 9.366927950383001189, -16.50191825106599808, -63.41115275078119851 ) ) ;
#47553 = CARTESIAN_POINT ( 'NONE',  ( 18.32697385714070037, -51.82372487085179813, -75.44171726276898937 ) ) ;
#47554 = CARTESIAN_POINT ( 'NONE',  ( 49.94506962897090574, -45.11618894467940066, -8.192301891433340089 ) ) ;
#47555 = CARTESIAN_POINT ( 'NONE',  ( 10.40593262108130013, -10.85208823022969860, -62.28818158525499626 ) ) ;
#47556 = CARTESIAN_POINT ( 'NONE',  ( 18.20466015165334639, -7.911101059566782112, -77.37566301139611369 ) ) ;
#47557 =( BOUNDED_CURVE ( )  B_SPLINE_CURVE ( 3, ( #639, #40476, #28666, #24199 ),
 .UNSPECIFIED., .F., .T. ) 
 B_SPLINE_CURVE_WITH_KNOTS ( ( 4, 4 ),
 ( 4.712388980593780197, 6.283185307179586232 ),
 .UNSPECIFIED. ) 
 CURVE ( )  GEOMETRIC_REPRESENTATION_ITEM ( )  RATIONAL_B_SPLINE_CURVE ( ( 1.000000000000000000, 0.8047378541736481816, 0.8047378541736481816, 1.000000000000000000 ) ) 
 REPRESENTATION_ITEM ( '' )  );
#47558 = CARTESIAN_POINT ( 'NONE',  ( 52.56658475560080035, -54.17900319927549191, -56.87455298638129619 ) ) ;
#47559 = ORIENTED_EDGE ( 'NONE', *, *, #22027, .F. ) ;
#47560 = CARTESIAN_POINT ( 'NONE',  ( 22.13393739769619728, -54.15188668067469990, -35.09469305598949518 ) ) ;
#47561 = DIRECTION ( 'NONE',  ( 1.000000000000000000, 0.000000000000000000, 0.000000000000000000 ) ) ;
#47562 = CARTESIAN_POINT ( 'NONE',  ( 72.91520214831270152, 1.373356196620449943, -68.60593141770759473 ) ) ;
#47563 = FACE_OUTER_BOUND ( 'NONE', #16108, .T. ) ;
#47564 = CARTESIAN_POINT ( 'NONE',  ( 8.985990923957119847, -15.50133730118559861, -81.23899999999999011 ) ) ;
#47565 = ORIENTED_EDGE ( 'NONE', *, *, #30644, .T. ) ;
#47566 = CARTESIAN_POINT ( 'NONE',  ( 18.19627591683260093, 21.04516553096049947, -75.75221093576890041 ) ) ;
#47567 = ORIENTED_EDGE ( 'NONE', *, *, #38110, .F. ) ;
#47568 = EDGE_CURVE ( 'NONE', #48985, #21823, #47676, .T. ) ;
#47569 = EDGE_LOOP ( 'NONE', ( #31663, #34131, #6237, #16309 ) ) ;
#47570 = CARTESIAN_POINT ( 'NONE',  ( 52.10267382257649871, 1.883811055284760005, -77.60820171200670359 ) ) ;
#47571 = CARTESIAN_POINT ( 'NONE',  ( 23.46520187981169769, -13.64785293624529849, -81.23899999999999011 ) ) ;
#47572 = LINE ( 'NONE', #15341, #34838 ) ;
#47573 = EDGE_CURVE ( 'NONE', #39379, #27118, #46706, .T. ) ;
#47574 = CARTESIAN_POINT ( 'NONE',  ( 61.74755533198759849, 13.88658087425049992, -46.49353895741179343 ) ) ;
#47575 = EDGE_CURVE ( 'NONE', #4191, #27635, #46965, .T. ) ;
#47576 = ORIENTED_EDGE ( 'NONE', *, *, #14001, .F. ) ;
#47577 = EDGE_CURVE ( 'NONE', #34457, #29477, #20036, .T. ) ;
#47578 = CARTESIAN_POINT ( 'NONE',  ( 15.78285172300917694, -8.812156430328993650, -79.93657430706403488 ) ) ;
#47579 = ORIENTED_EDGE ( 'NONE', *, *, #50624, .T. ) ;
#47580 = FACE_OUTER_BOUND ( 'NONE', #36565, .T. ) ;
#47581 = CARTESIAN_POINT ( 'NONE',  ( 64.93393739769619799, 11.23736444591397543, -69.70355339059327093 ) ) ;
#47582 = ORIENTED_EDGE ( 'NONE', *, *, #28109, .F. ) ;
#47583 = CARTESIAN_POINT ( 'NONE',  ( 45.06234682331504615, 2.029620634295568937, -36.93999394477614828 ) ) ;
#47584 = CARTESIAN_POINT ( 'NONE',  ( 51.93758451744589877, -50.81981950107080337, -76.23465793669190305 ) ) ;
#47585 = CARTESIAN_POINT ( 'NONE',  ( 60.50469153357809660, 14.48475327612959873, -47.56295389503220150 ) ) ;
#47586 = CARTESIAN_POINT ( 'NONE',  ( 15.67962062511290000, 19.63028992866140143, -15.65622423491010196 ) ) ;
#47587 = ADVANCED_FACE ( 'NONE', ( #28550 ), #20949, .T. ) ;
#47588 = CARTESIAN_POINT ( 'NONE',  ( 40.95606683356889732, -44.38928517632400172, -3.881684254074280194 ) ) ;
#47589 = CARTESIAN_POINT ( 'NONE',  ( -7.093926665547340527, 14.66186757398629936, -5.595729436106440247 ) ) ;
#47590 = CARTESIAN_POINT ( 'NONE',  ( 46.35275103504439898, 21.67755452994670406, -76.14999999999999147 ) ) ;
#47591 = CARTESIAN_POINT ( 'NONE',  ( -11.32734370190460105, -41.88171845330919751, -6.430192534648670133 ) ) ;
#47592 = CARTESIAN_POINT ( 'NONE',  ( 8.337315010399510840, -16.51029605967550040, -64.25116097130579362 ) ) ;
#47593 = ORIENTED_EDGE ( 'NONE', *, *, #11733, .F. ) ;
#47594 = CARTESIAN_POINT ( 'NONE',  ( 54.20961013379049831, 17.70559848872130360, -48.50941760523620161 ) ) ;
#47595 = CARTESIAN_POINT ( 'NONE',  ( 9.366365918819754555, -15.58120503557203484, -75.84882408509788831 ) ) ;
#47596 = CARTESIAN_POINT ( 'NONE',  ( 71.71411752565128950, 0.9618757110835569613, -70.46515124295960675 ) ) ;
#47597 = CARTESIAN_POINT ( 'NONE',  ( 42.43635952588410731, -39.81067629326607005, -74.22320020691999787 ) ) ;
#47598 = DIRECTION ( 'NONE',  ( -1.000000000000000000, -1.006844464268868150E-16, 0.000000000000000000 ) ) ;
#47600 = EDGE_CURVE ( 'NONE', #30115, #16412, #23364, .T. ) ;
#47599 = CYLINDRICAL_SURFACE ( 'NONE', #49909, 1.999999999999999112 ) ;
#47601 = CARTESIAN_POINT ( 'NONE',  ( 12.89656437218379992, 18.76901985379959825, -21.06838189303089948 ) ) ;
#47602 = LINE ( 'NONE', #31327, #47304 ) ;
#47603 = CARTESIAN_POINT ( 'NONE',  ( 48.84331286892799540, -53.99784967936330560, -54.98158588870150254 ) ) ;
#47604 = CARTESIAN_POINT ( 'NONE',  ( 24.04493292379381231, -15.60707448483026738, -45.50730927894573341 ) ) ;
#47605 = DIRECTION ( 'NONE',  ( -1.000000000000000000, 0.000000000000000000, 0.000000000000000000 ) ) ;
#47606 = CARTESIAN_POINT ( 'NONE',  ( 47.71251016117639665, 23.27152831638220221, -55.11640457198600274 ) ) ;
#47607 = ORIENTED_EDGE ( 'NONE', *, *, #12523, .T. ) ;
#47608 = CARTESIAN_POINT ( 'NONE',  ( 18.38973105523419704, -21.99613282959019500, -81.23899999999999011 ) ) ;
#47609 = CARTESIAN_POINT ( 'NONE',  ( 15.24809864170513052, -22.38318404622074098, -76.99450079008921932 ) ) ;
#47610 = VERTEX_POINT ( 'NONE', #40618 ) ;
#47611 = CARTESIAN_POINT ( 'NONE',  ( 71.52584472686049821, 1.187931651339009909, -70.49707891402350413 ) ) ;
#47612 = CARTESIAN_POINT ( 'NONE',  ( 60.26025110216870218, -45.78774436170850493, -47.43140372362439905 ) ) ;
#47613 = CARTESIAN_POINT ( 'NONE',  ( 55.49599478882979753, -48.26400341526489512, -48.16694294531149723 ) ) ;
#47614 = CARTESIAN_POINT ( 'NONE',  ( 83.62039299881514864, 13.30922359856841908, -46.55140764634001016 ) ) ;
#47616 = LINE ( 'NONE', #15127, #33137 ) ;
#47615 = CARTESIAN_POINT ( 'NONE',  ( 42.72653070048255586, 8.607061861151045434, -72.82242792000907627 ) ) ;
#47617 = FACE_OUTER_BOUND ( 'NONE', #10080, .T. ) ;
#47618 = CARTESIAN_POINT ( 'NONE',  ( 38.67452568954060155, 4.883811055320659733, -81.65000000000000568 ) ) ;
#47619 = VERTEX_POINT ( 'NONE', #48229 ) ;
#47620 = CARTESIAN_POINT ( 'NONE',  ( 16.13393739769620083, -15.61618894467929941, -7.225658350974740074 ) ) ;
#47621 = VERTEX_POINT ( 'NONE', #16001 ) ;
#47622 = VERTEX_POINT ( 'NONE', #1046 ) ;
#47623 = CARTESIAN_POINT ( 'NONE',  ( 0.1457841021255935343, -26.78123956999450428, -34.68167779225149161 ) ) ;
#47624 = CARTESIAN_POINT ( 'NONE',  ( 8.428810482305360452, -13.54560713631422963, -38.87566260121617034 ) ) ;
#47625 = FACE_OUTER_BOUND ( 'NONE', #17137, .T. ) ;
#47626 = CARTESIAN_POINT ( 'NONE',  ( 9.127478409050889141, -63.94375969884499966, -46.75102855002580071 ) ) ;
#47627 = AXIS2_PLACEMENT_3D ( 'NONE', #19660, #50869, #15225 ) ;
#47628 = ORIENTED_EDGE ( 'NONE', *, *, #17574, .T. ) ;
#47629 = ADVANCED_FACE ( 'NONE', ( #8139 ), #17039, .F. ) ;
#47630 = CARTESIAN_POINT ( 'NONE',  ( -20.29802031372836524, -1.697423245748443943, -52.67334128422192663 ) ) ;
#47631 = CARTESIAN_POINT ( 'NONE',  ( 56.50306487293649838, -50.76048388989789828, -53.80671209316210479 ) ) ;
#47632 = CARTESIAN_POINT ( 'NONE',  ( 22.89540641129645948, -15.32079363685985030, -46.43893137664500870 ) ) ;
#47633 = CARTESIAN_POINT ( 'NONE',  ( 58.97986318629950375, -2.782461215938549781, -15.64991376612959861 ) ) ;
#47634 = CARTESIAN_POINT ( 'NONE',  ( 51.69077941763050177, -49.33148676370400665, -76.83272514207421011 ) ) ;
#47635 = CARTESIAN_POINT ( 'NONE',  ( 64.93393739769619799, 10.88381105532070059, -69.34999999999999432 ) ) ;
#47636 = ORIENTED_EDGE ( 'NONE', *, *, #6862, .F. ) ;
#47637 = CARTESIAN_POINT ( 'NONE',  ( 16.13393739769620083, -15.61618894467929941, -2.149999999999999911 ) ) ;
#47638 = CARTESIAN_POINT ( 'NONE',  ( 23.04647732774926183, -19.60028910769844757, -47.95899984034043939 ) ) ;
#47639 = CARTESIAN_POINT ( 'NONE',  ( 60.32372535534924651, 14.61230269747045440, -47.67141866289382079 ) ) ;
#47640 = AXIS2_PLACEMENT_3D ( 'NONE', #24728, #20545, #16374 ) ;
#47641 = CARTESIAN_POINT ( 'NONE',  ( 8.222476383702659319, -15.61632876086509825, -54.50766849176299900 ) ) ;
#47642 = AXIS2_PLACEMENT_3D ( 'NONE', #51592, #15948, #28234 ) ;
#47643 = CIRCLE ( 'NONE', #5775, 1.000000000000000888 ) ;
#47644 = CARTESIAN_POINT ( 'NONE',  ( 21.94814240175420039, -20.88703022120900243, -50.24690406358499217 ) ) ;
#47645 = CARTESIAN_POINT ( 'NONE',  ( 12.91624052176669935, -50.10753798784559621, -21.10293742790859994 ) ) ;
#47646 = CARTESIAN_POINT ( 'NONE',  ( 54.86383200389320081, 19.39201119830140030, -76.47890740922589714 ) ) ;
#47647 = ADVANCED_FACE ( 'NONE', ( #8397 ), #12080, .T. ) ;
#47648 = DIRECTION ( 'NONE',  ( 0.000000000000000000, 0.000000000000000000, 1.000000000000000000 ) ) ;
#47649 = CARTESIAN_POINT ( 'NONE',  ( 57.33235504379430125, 13.88381105532070059, -16.73838572529449920 ) ) ;
#47650 = CARTESIAN_POINT ( 'NONE',  ( 8.787528872099951371, 17.80194031521759968, -34.71551406240389781 ) ) ;
#47651 = LINE ( 'NONE', #3887, #19560 ) ;
#47652 = CARTESIAN_POINT ( 'NONE',  ( 22.91931868946720030, -13.69234906055819856, -48.75923826391610305 ) ) ;
#47653 = CARTESIAN_POINT ( 'NONE',  ( 11.13393739769619906, -63.52234721269329754, -43.76018303787720498 ) ) ;
#47654 = EDGE_LOOP ( 'NONE', ( #25436, #44597, #43644, #14780, #9075 ) ) ;
#47655 = CARTESIAN_POINT ( 'NONE',  ( 46.61750669718259843, 22.00845647425120077, -76.11314270330180420 ) ) ;
#47656 = DIRECTION ( 'NONE',  ( -1.000000000000000000, 0.000000000000000000, 0.000000000000000000 ) ) ;
#47657 = CARTESIAN_POINT ( 'NONE',  ( 8.223606718150689332, -15.61618413875730127, -36.50766849176289952 ) ) ;
#47658 = CARTESIAN_POINT ( 'NONE',  ( 11.19893373200904740, -19.20167898366336345, -8.849999999999999645 ) ) ;
#47659 = CARTESIAN_POINT ( 'NONE',  ( 14.70129800643555740, -50.53293986238711710, -20.74427331569097177 ) ) ;
#47660 = CARTESIAN_POINT ( 'NONE',  ( 8.222476383702659319, -15.61632876086509825, -54.50766849176299900 ) ) ;
#47661 = EDGE_CURVE ( 'NONE', #15006, #10642, #7492, .T. ) ;
#47662 = CARTESIAN_POINT ( 'NONE',  ( 47.13393739769619373, -36.11618894467930119, -54.64999999999999858 ) ) ;
#47664 = EDGE_CURVE ( 'NONE', #19127, #46545, #33129, .T. ) ;
#47663 = CARTESIAN_POINT ( 'NONE',  ( 10.83005342333859922, 33.77654421452230338, -17.86451960232090030 ) ) ;
#47665 = DIRECTION ( 'NONE',  ( 0.5765530599821108160, 0.1342272854595029929, -0.8059588108975778153 ) ) ;
#47667 = CARTESIAN_POINT ( 'NONE',  ( 14.06335050055401936, -23.32131284038766950, -58.37566472363047154 ) ) ;
#47666 = CARTESIAN_POINT ( 'NONE',  ( 0.4420762188774280399, -8.844152220602129688, -35.01387690002259490 ) ) ;
#47668 = CARTESIAN_POINT ( 'NONE',  ( 14.80173184006769382, -52.40467206551404189, -76.02665054607155071 ) ) ;
#47669 = DIRECTION ( 'NONE',  ( 0.000000000000000000, 0.000000000000000000, 1.000000000000000000 ) ) ;
#47670 = CARTESIAN_POINT ( 'NONE',  ( 49.04086831984160000, 22.53609092988610030, -54.46858570338200423 ) ) ;
#47671 = VECTOR ( 'NONE', #50234, 1000.000000000000000 ) ;
#47672 = ORIENTED_EDGE ( 'NONE', *, *, #28323, .F. ) ;
#47673 = VECTOR ( 'NONE', #25111, 1000.000000000000000 ) ;
#47674 = CARTESIAN_POINT ( 'NONE',  ( 52.96692110958939992, -49.60671036882420282, -48.95117873441440537 ) ) ;
#47675 = EDGE_LOOP ( 'NONE', ( #2890, #16352, #23937, #8025 ) ) ;
#47676 = CIRCLE ( 'NONE', #6674, 4.065467063327089292 ) ;
#47677 = CARTESIAN_POINT ( 'NONE',  ( 46.20542188648048665, 6.681296133090609324, -59.23417205188202672 ) ) ;
#47678 = CARTESIAN_POINT ( 'NONE',  ( 21.54530251441495992, -19.77479970165442325, -74.66115355887134797 ) ) ;
#47679 = CARTESIAN_POINT ( 'NONE',  ( 16.13393739769620083, -15.61618894467929941, -48.64999999999999858 ) ) ;
#47680 = CYLINDRICAL_SURFACE ( 'NONE', #29031, 7.910999999999997812 ) ;
#47681 = CARTESIAN_POINT ( 'NONE',  ( 21.89967498990359829, -19.67806396915169742, -54.64817642206789827 ) ) ;
#47682 = CARTESIAN_POINT ( 'NONE',  ( 52.77399500191609860, 18.49248106158579930, -48.90117827005099826 ) ) ;
#47683 = CARTESIAN_POINT ( 'NONE',  ( 56.63448749956920381, -45.12949307036979718, -15.89371657090130086 ) ) ;
#47684 = CYLINDRICAL_SURFACE ( 'NONE', #47377, 10.00000000000000711 ) ;
#47685 = EDGE_LOOP ( 'NONE', ( #20148, #20004, #40207, #2436 ) ) ;
#47686 = CARTESIAN_POINT ( 'NONE',  ( 10.06545220148790065, -10.64022314831530025, -46.50612041305500099 ) ) ;
#47687 = EDGE_LOOP ( 'NONE', ( #26596, #29984 ) ) ;
#47688 = CARTESIAN_POINT ( 'NONE',  ( 11.44080321505469833, -65.29620232506569266, -17.48917031883349793 ) ) ;
#47689 = CARTESIAN_POINT ( 'NONE',  ( 11.47750026906150111, 33.80079264447829956, -46.66654629083320316 ) ) ;
#47690 = CARTESIAN_POINT ( 'NONE',  ( 73.04558532727548936, 1.003508719580009867, -62.21555175845400498 ) ) ;
#47691 = EDGE_CURVE ( 'NONE', #51177, #46163, #33439, .T. ) ;
#47692 = CARTESIAN_POINT ( 'NONE',  ( 53.41103307671369294, -49.40180341210120218, -49.08863635434799733 ) ) ;
#47693 = CARTESIAN_POINT ( 'NONE',  ( 10.96077434704564801, -64.78872648947765356, -23.23801892677574088 ) ) ;
#47694 = CARTESIAN_POINT ( 'NONE',  ( 13.04629919360955448, -49.74868907930030559, -82.73668660645857642 ) ) ;
#47695 = ORIENTED_EDGE ( 'NONE', *, *, #20164, .F. ) ;
#47696 = EDGE_CURVE ( 'NONE', #28243, #11637, #24344, .T. ) ;
#47697 = CARTESIAN_POINT ( 'NONE',  ( 64.91441195039600132, 1.390806392144110060, -70.26251807531768634 ) ) ;
#47698 = CARTESIAN_POINT ( 'NONE',  ( 11.13393739769619906, -63.47497630073510777, -43.75645565886269850 ) ) ;
#47699 = CARTESIAN_POINT ( 'NONE',  ( 13.42155525365338065, 20.57173965391032411, -74.52173647802152345 ) ) ;
#47700 = ORIENTED_EDGE ( 'NONE', *, *, #19416, .F. ) ;
#47701 = CARTESIAN_POINT ( 'NONE',  ( 84.13393739769618662, -0.5161889446793590519, -65.65000000000000568 ) ) ;
#47702 = CARTESIAN_POINT ( 'NONE',  ( 56.57206750253590855, 19.50115452726630139, -53.72158482572499594 ) ) ;
#47703 = B_SPLINE_CURVE_WITH_KNOTS ( 'NONE', 3,
 ( #23297, #43261, #39318, #51627, #15982, #46942, #3422, #31678, #14948, #11803 ),
 .UNSPECIFIED., .F., .F.,
 ( 4, 1, 1, 1, 1, 1, 1, 4 ),
 ( 0.000000000000000000, 0.1428420414407585159, 0.2857017012006322632, 0.4285613609605059549, 0.5714210207203787029, 0.7142806804802525056, 0.8571403402401261973, 1.000000000000000000 ),
 .UNSPECIFIED. ) ;
#47704 = CARTESIAN_POINT ( 'NONE',  ( 17.08918660137072720, -7.732233853712758176, -49.04612841921350963 ) ) ;
#47705 = ORIENTED_EDGE ( 'NONE', *, *, #1281, .F. ) ;
#47706 = DIRECTION ( 'NONE',  ( 0.7071067811865475727, -0.7071067811865475727, 0.000000000000000000 ) ) ;
#47707 = CARTESIAN_POINT ( 'NONE',  ( 51.08534821908290269, 19.80328544295542770, -76.14824059617301089 ) ) ;
#47708 = CARTESIAN_POINT ( 'NONE',  ( 8.223069265346360623, -15.61598766837350105, -56.50766849176299189 ) ) ;
#47709 = CARTESIAN_POINT ( 'NONE',  ( 10.63467927709140071, -9.472828286302069856, -75.05992337703769124 ) ) ;
#47710 = DIRECTION ( 'NONE',  ( 1.000000000000000000, 0.000000000000000000, 0.000000000000000000 ) ) ;
#47711 = CARTESIAN_POINT ( 'NONE',  ( 46.48050859836360615, -38.20152441653880260, -57.91714385711884461 ) ) ;
#47712 = ORIENTED_EDGE ( 'NONE', *, *, #23096, .F. ) ;
#47713 = ORIENTED_EDGE ( 'NONE', *, *, #31267, .F. ) ;
#47714 = AXIS2_PLACEMENT_3D ( 'NONE', #31621, #39520, #22989 ) ;
#47715 = CARTESIAN_POINT ( 'NONE',  ( 19.77582419784589973, -9.116700169395430819, -67.89523180023219595 ) ) ;
#47716 = VECTOR ( 'NONE', #14747, 1000.000000000000000 ) ;
#47717 = DIRECTION ( 'NONE',  ( 0.3863301728269245006, -0.9223605572461989199, -3.608224830031755305E-16 ) ) ;
#47718 = VECTOR ( 'NONE', #42674, 1000.000000000000000 ) ;
#47719 = CARTESIAN_POINT ( 'NONE',  ( 12.40813258608080005, -22.56902654875089809, -32.14999999999999858 ) ) ;
#47720 = AXIS2_PLACEMENT_3D ( 'NONE', #29037, #29547, #5211 ) ;
#47721 = CARTESIAN_POINT ( 'NONE',  ( 46.66794420925759823, 22.33509408192179890, -76.02748009641369720 ) ) ;
#47722 = DIRECTION ( 'NONE',  ( 0.000000000000000000, 0.000000000000000000, 1.000000000000000000 ) ) ;
#47723 = CARTESIAN_POINT ( 'NONE',  ( 9.916610038436060037, 22.42506970168800251, -34.65028073423250277 ) ) ;
#47724 = CARTESIAN_POINT ( 'NONE',  ( 11.90346178787130071, 33.73586922521850084, -16.35924802166870151 ) ) ;
#47725 = CARTESIAN_POINT ( 'NONE',  ( 13.58396071722250120, -7.775248973093270344, -68.90758401351938289 ) ) ;
#47726 = CARTESIAN_POINT ( 'NONE',  ( 23.43844683284619990, -16.50873768209440229, -32.14999999999999858 ) ) ;
#47727 = EDGE_CURVE ( 'NONE', #10101, #21277, #13715, .T. ) ;
#47728 = CARTESIAN_POINT ( 'NONE',  ( 56.02466961400099876, -50.67465440105149810, -75.43166099610559172 ) ) ;
#47730 = CARTESIAN_POINT ( 'NONE',  ( 22.90093741614429135, -14.73038836730692580, -60.41114393275640282 ) ) ;
#47729 = CARTESIAN_POINT ( 'NONE',  ( 1.192719620188050111, 22.32378988226099992, -7.795412869570020220 ) ) ;
#47731 = CARTESIAN_POINT ( 'NONE',  ( 63.09723768121719445, 1.097895768572089814, -68.83057487531520735 ) ) ;
#47732 = CARTESIAN_POINT ( 'NONE',  ( 61.41101597850759930, 13.95334023698869963, -46.65852037685949938 ) ) ;
#47733 = CARTESIAN_POINT ( 'NONE',  ( -30.36606260230379917, -53.11618894467930119, 11.84999999999999964 ) ) ;
#47734 = EDGE_CURVE ( 'NONE', #38545, #24575, #6277, .T. ) ;
#47735 = ORIENTED_EDGE ( 'NONE', *, *, #41234, .T. ) ;
#47736 = CARTESIAN_POINT ( 'NONE',  ( 52.96420272660349582, -49.59048021264120365, -48.77461995705460396 ) ) ;
#47737 = CARTESIAN_POINT ( 'NONE',  ( 61.43364071597069653, -45.16647806383540598, -28.15110207759829919 ) ) ;
#47738 = CARTESIAN_POINT ( 'NONE',  ( 14.06314509805251411, -23.32125965905213150, -72.37568720284336621 ) ) ;
#47739 = CARTESIAN_POINT ( 'NONE',  ( 60.96771750282989899, 14.26879997633939823, -47.44758383409369884 ) ) ;
#47740 = CARTESIAN_POINT ( 'NONE',  ( 15.79570006403920068, -23.05878857862889930, -70.74711331852249430 ) ) ;
#47741 = CARTESIAN_POINT ( 'NONE',  ( 51.62537654974559587, 17.96288684338239960, -76.81862610352639820 ) ) ;
#47742 = CARTESIAN_POINT ( 'NONE',  ( 52.74228737775210618, 18.48090198830360009, -48.57744821062869534 ) ) ;
#47743 = CARTESIAN_POINT ( 'NONE',  ( 12.14985788165700420, -22.52874148118596054, -70.45899922006387328 ) ) ;
#47744 = CARTESIAN_POINT ( 'NONE',  ( 53.05372066228549954, -49.54357925801589602, -48.79446872794070345 ) ) ;
#47745 = ORIENTED_EDGE ( 'NONE', *, *, #5067, .T. ) ;
#47746 = CYLINDRICAL_SURFACE ( 'NONE', #7084, 0.9999999999999988898 ) ;
#47747 = TOROIDAL_SURFACE ( 'NONE', #5061, 2.500000000000000000, 0.5000000000000000000 ) ;
#47748 = CARTESIAN_POINT ( 'NONE',  ( 47.63173516101420546, -54.51015595446700246, -54.75624560665560381 ) ) ;
#47749 = CARTESIAN_POINT ( 'NONE',  ( 0.1155610841158959956, 19.94237700917059897, -35.14999985728680088 ) ) ;
#47750 = TOROIDAL_SURFACE ( 'NONE', #36848, 9.000000000000000000, 1.000000000000000000 ) ;
#47751 = CARTESIAN_POINT ( 'NONE',  ( 12.95491128060830022, 18.65448050664010182, -82.14319696191608955 ) ) ;
#47752 = CARTESIAN_POINT ( 'NONE',  ( 61.44797978346510803, -30.90289317591489748, -16.49569814832250003 ) ) ;
#47753 = CARTESIAN_POINT ( 'NONE',  ( 71.46697330897291067, 1.186614556332910020, -60.76691531849380112 ) ) ;
#47754 = CARTESIAN_POINT ( 'NONE',  ( 11.13393739769619906, 32.13925317360830292, -43.75007275908160409 ) ) ;
#47755 = CARTESIAN_POINT ( 'NONE',  ( 72.62016429705300880, 1.099201050715839845, -61.67264653093729976 ) ) ;
#47756 = VECTOR ( 'NONE', #20721, 1000.000000000000114 ) ;
#47757 = FACE_OUTER_BOUND ( 'NONE', #15391, .T. ) ;
#47758 = EDGE_CURVE ( 'NONE', #15596, #42552, #33259, .T. ) ;
#47759 = DIRECTION ( 'NONE',  ( 1.000000000000000000, 0.000000000000000000, 0.000000000000000000 ) ) ;
#47760 = ORIENTED_EDGE ( 'NONE', *, *, #43328, .F. ) ;
#47761 = ORIENTED_EDGE ( 'NONE', *, *, #49918, .F. ) ;
#47762 = DIRECTION ( 'NONE',  ( 0.000000000000000000, 1.377023495004005809E-11, 1.000000000000000000 ) ) ;
#47763 = ADVANCED_FACE ( 'NONE', ( #25133 ), #10257, .T. ) ;
#47764 = CARTESIAN_POINT ( 'NONE',  ( 87.61621807841599718, -33.11618894467940066, -61.12885639714370001 ) ) ;
#47765 = ORIENTED_EDGE ( 'NONE', *, *, #39396, .F. ) ;
#47766 = CARTESIAN_POINT ( 'NONE',  ( 56.67587010945499770, -45.29461281360359948, -25.29358288562269763 ) ) ;
#47767 = CARTESIAN_POINT ( 'NONE',  ( 16.47165959384855682, -23.52718952250380369, -77.99408671543044136 ) ) ;
#47768 = ORIENTED_EDGE ( 'NONE', *, *, #44911, .F. ) ;
#47769 = CARTESIAN_POINT ( 'NONE',  ( 11.41737698698953629, 34.03946597324494405, -22.74029088214029670 ) ) ;
#47770 = CARTESIAN_POINT ( 'NONE',  ( 44.39412272499598799, 6.736181560341522712, -68.34907281161095227 ) ) ;
#47771 = CARTESIAN_POINT ( 'NONE',  ( 12.14989278840985598, -8.703616661238887886, -34.84100081756681533 ) ) ;
#47772 = CARTESIAN_POINT ( 'NONE',  ( 21.91218854648699832, -21.49790074630919889, -40.04515584691789343 ) ) ;
#47773 = CARTESIAN_POINT ( 'NONE',  ( 20.11807550982419102, -22.52870806245297786, -67.84099995454940313 ) ) ;
#47774 = CARTESIAN_POINT ( 'NONE',  ( 24.04493642151950539, -15.62074925824641980, -49.79251394409821785 ) ) ;
#47775 =( LENGTH_UNIT ( ) NAMED_UNIT ( * ) SI_UNIT ( .MILLI., .METRE. ) );
#47776 = CARTESIAN_POINT ( 'NONE',  ( 59.79173912391249246, -28.94653353880099900, -15.75539910036690294 ) ) ;
#47777 = CARTESIAN_POINT ( 'NONE',  ( 63.00666467042349694, 0.8838110553206759423, -62.53374032209040223 ) ) ;
#47778 = CARTESIAN_POINT ( 'NONE',  ( 17.24979877144579987, -7.848203483545518999, -79.55790855712419329 ) ) ;
#47779 = CARTESIAN_POINT ( 'NONE',  ( 55.83251375037820452, 14.69215176195739936, -17.34604097549789969 ) ) ;
#47780 = CARTESIAN_POINT ( 'NONE',  ( 41.62257857717389697, 13.94622149448480108, -6.029585542484710459 ) ) ;
#47781 = CARTESIAN_POINT ( 'NONE',  ( 14.97490622639899982, 21.71079195693500097, -76.14999999999999147 ) ) ;
#47782 = AXIS2_PLACEMENT_3D ( 'NONE', #8274, #7771, #27920 ) ;
#47783 = CARTESIAN_POINT ( 'NONE',  ( 82.84359872746441056, -45.06894711141969623, -46.75796921614900015 ) ) ;
#47784 = CARTESIAN_POINT ( 'NONE',  ( 64.89936453248850512, 1.399477666643410112, -70.22527192354300496 ) ) ;
#47785 = CIRCLE ( 'NONE', #50301, 17.39999999999999503 ) ;
#47786 = CARTESIAN_POINT ( 'NONE',  ( 20.40418685453369818, -8.562984688076911155, -41.18095814125259579 ) ) ;
#47787 = ORIENTED_EDGE ( 'NONE', *, *, #48280, .T. ) ;
#47788 = CARTESIAN_POINT ( 'NONE',  ( 85.66799001034409855, -48.61618894467930119, -61.58097075742929860 ) ) ;
#47789 = B_SPLINE_CURVE_WITH_KNOTS ( 'NONE', 3,
 ( #24245, #32630, #4360, #16416, #178, #51804 ),
 .UNSPECIFIED., .F., .F.,
 ( 4, 2, 4 ),
 ( 0.5025462808315325214, 0.7512731404157662052, 1.000000000000000000 ),
 .UNSPECIFIED. ) ;
#47790 = EDGE_CURVE ( 'NONE', #6571, #43625, #43874, .T. ) ;
#47791 = CARTESIAN_POINT ( 'NONE',  ( 15.65736449272620057, -50.94086818095720304, -20.65166207265509968 ) ) ;
#47792 = CARTESIAN_POINT ( 'NONE',  ( 50.92696022065899086, -35.35053649607394988, -76.36237708703390581 ) ) ;
#47793 = CARTESIAN_POINT ( 'NONE',  ( 22.90092413496008561, -15.63002623182754824, -56.45347593842252110 ) ) ;
#47794 = CARTESIAN_POINT ( 'NONE',  ( 13.29196628753849829, -50.07647855290770167, -21.00283603508880148 ) ) ;
#47795 = ORIENTED_EDGE ( 'NONE', *, *, #5638, .F. ) ;
#47796 = CARTESIAN_POINT ( 'NONE',  ( 26.93010376912529935, -27.85143120648099924, -35.14999999999999858 ) ) ;
#47797 = CARTESIAN_POINT ( 'NONE',  ( 47.21472468777420062, 23.54994789198669736, -54.62442519253269779 ) ) ;
#47798 = FACE_OUTER_BOUND ( 'NONE', #12753, .T. ) ;
#47799 = CARTESIAN_POINT ( 'NONE',  ( 63.48441347673288959, 1.386342629514219826, -62.63353618948930546 ) ) ;
#47800 = CARTESIAN_POINT ( 'NONE',  ( 57.46727618224160494, -50.61618894467939356, -53.87377490133690117 ) ) ;
#47801 = CARTESIAN_POINT ( 'NONE',  ( 42.11495618719890643, 12.77424371615120080, -4.742906899983229785 ) ) ;
#47802 = CARTESIAN_POINT ( 'NONE',  ( 24.04487853986463008, -15.61618860033810030, -61.79233400586811342 ) ) ;
#47803 = DIRECTION ( 'NONE',  ( -1.000000000000000000, 0.000000000000000000, 0.000000000000000000 ) ) ;
#47804 = CARTESIAN_POINT ( 'NONE',  ( 68.13393739769630031, -48.11618894467930119, -73.25000000000000000 ) ) ;
#47805 = CARTESIAN_POINT ( 'NONE',  ( 23.94343461585225086, -14.32673262226892064, -75.74025377681455495 ) ) ;
#47806 = CARTESIAN_POINT ( 'NONE',  ( 17.01970573595322378, -22.38319328302324251, -62.91115104534193847 ) ) ;
#47807 = CARTESIAN_POINT ( 'NONE',  ( 20.47328261930400473, -41.85765695298069033, -34.70142521051216988 ) ) ;
#47808 = B_SPLINE_SURFACE_WITH_KNOTS ( 'NONE', 3, 3, ( 
 ( #21299, #49634, #9536, #44392, #1140, #40974, #32823, #37043 ),
 ( #24699, #24440, #13216, #40454, #36514, #37304, #17652, #29167 ),
 ( #45168, #4547, #17136, #17391, #44645, #33356, #33087, #49118 ),
 ( #20519, #8751, #40718, #13472, #16875, #29428, #21559, #5604 ),
 ( #25487, #4814, #20781, #36773, #38083, #26007, #38867, #50909 ),
 ( #46220, #6118, #18414, #2179, #45690, #29934, #34125, #46480 ),
 ( #26268, #10043, #9791, #14233, #18927, #34646, #22073, #25742 ),
 ( #1921, #50135, #22847, #37827, #34911, #41749, #13978, #38609 ),
 ( #2956, #17899, #29679, #5856, #42275, #21819, #6629, #33871 ),
 ( #26787, #22593, #49882, #42800, #45951, #34388, #42016, #18159 ) ),
 .UNSPECIFIED., .F., .F., .F.,
 ( 4, 1, 1, 1, 1, 1, 1, 4 ),
 ( 4, 2, 2, 4 ),
 ( -3.285243819981630014E-05, 0.1428571428571430157, 0.2857142857142860315, 0.4285714285714289917, 0.5714285714285709528, 0.7142857142857139685, 0.8571428571428569843, 1.000000000000000000 ),
 ( 1.570647095086020073, 1.792618180878300160, 2.161517997136110036, 2.169191869667270289 ),
 .UNSPECIFIED. ) ;
#47809 = EDGE_CURVE ( 'NONE', #40337, #7646, #13374, .T. ) ;
#47810 = CARTESIAN_POINT ( 'NONE',  ( 9.225026380130959325, -12.82806360859640016, -64.18943593078189735 ) ) ;
#47811 = CARTESIAN_POINT ( 'NONE',  ( 15.67962062493570130, 19.63028992856250099, -20.15000000000000213 ) ) ;
#47812 = CARTESIAN_POINT ( 'NONE',  ( 60.36614594669769929, -45.86778937511110144, -47.74314716484730070 ) ) ;
#47813 = ORIENTED_EDGE ( 'NONE', *, *, #48872, .T. ) ;
#47814 = CARTESIAN_POINT ( 'NONE',  ( 8.802044555037090490, 31.97380483823370056, -46.67015369154350424 ) ) ;
#47815 = CARTESIAN_POINT ( 'NONE',  ( 38.67452568954050207, 4.883811055320659733, -81.65000000000000568 ) ) ;
#47816 = CARTESIAN_POINT ( 'NONE',  ( 73.14840136429539541, 1.194703186106690129, -68.75325824359919125 ) ) ;
#47817 = CARTESIAN_POINT ( 'NONE',  ( 68.13393739769620083, -50.61618894467930119, -65.65000000000000568 ) ) ;
#47818 = CARTESIAN_POINT ( 'NONE',  ( 9.002563573228689719, -15.69178742396579906, -81.23899999999999011 ) ) ;
#47819 = VERTEX_POINT ( 'NONE', #8485 ) ;
#47820 = EDGE_CURVE ( 'NONE', #42604, #49152, #1818, .T. ) ;
#47821 = CARTESIAN_POINT ( 'NONE',  ( 17.35064738833469988, 21.75175735174070013, -76.14999999999999147 ) ) ;
#47822 = ORIENTED_EDGE ( 'NONE', *, *, #48877, .T. ) ;
#47823 = ADVANCED_FACE ( 'NONE', ( #34575 ), #11828, .T. ) ;
#47824 = VERTEX_POINT ( 'NONE', #4937 ) ;
#47825 = DIRECTION ( 'NONE',  ( 0.7165155114351267063, -0.6975711590030502229, 0.000000000000000000 ) ) ;
#47826 = CARTESIAN_POINT ( 'NONE',  ( 23.60004879085900242, -15.23558838188970022, -81.23899999999999011 ) ) ;
#47827 = CARTESIAN_POINT ( 'NONE',  ( 24.04527493495583457, -15.61618894149694192, -73.79233149842438877 ) ) ;
#47828 = AXIS2_PLACEMENT_3D ( 'NONE', #3283, #39187, #27631 ) ;
#47829 = ORIENTED_EDGE ( 'NONE', *, *, #27906, .F. ) ;
#47830 = VECTOR ( 'NONE', #39245, 1000.000000000000000 ) ;
#47831 = CARTESIAN_POINT ( 'NONE',  ( 11.27225130591669178, -9.290029843429451262, -52.79933604972921302 ) ) ;
#47832 = ORIENTED_EDGE ( 'NONE', *, *, #32140, .T. ) ;
#47833 = CARTESIAN_POINT ( 'NONE',  ( 11.37681742080861724, -64.48564029933889685, -24.02179917343915605 ) ) ;
#47834 = ORIENTED_EDGE ( 'NONE', *, *, #2592, .T. ) ;
#47835 = VERTEX_POINT ( 'NONE', #37171 ) ;
#47836 = LINE ( 'NONE', #14828, #7430 ) ;
#47837 = CARTESIAN_POINT ( 'NONE',  ( -31.07316938349034885, -15.61618894467929941, 11.14289321881345174 ) ) ;
#47838 = CARTESIAN_POINT ( 'NONE',  ( 60.76566018258669999, 14.49059974634529979, -47.73209457277470591 ) ) ;
#47839 = DIRECTION ( 'NONE',  ( 0.3863301728269245006, -0.9223605572461989199, -3.608224830031755305E-16 ) ) ;
#47840 = DIRECTION ( 'NONE',  ( 1.000000000000000000, 0.000000000000000000, 0.000000000000000000 ) ) ;
#47841 = CARTESIAN_POINT ( 'NONE',  ( -7.613869289485230674, 14.13164915896370033, -5.447993287580489508 ) ) ;
#47842 = DIRECTION ( 'NONE',  ( 0.000000000000000000, -1.000000000000000000, 0.000000000000000000 ) ) ;
#47843 = CARTESIAN_POINT ( 'NONE',  ( 61.28586840673359859, 13.99814824549559944, -28.15105127600999779 ) ) ;
#47844 = CARTESIAN_POINT ( 'NONE',  ( 22.70037966282230002, -11.31867987988980140, -67.10304248959599249 ) ) ;
#47845 = EDGE_LOOP ( 'NONE', ( #29833, #9797, #9699, #42802, #28488, #38742, #45314 ) ) ;
#47846 = CARTESIAN_POINT ( 'NONE',  ( 10.13393739769619906, -54.15188668067469990, -54.64999999999999858 ) ) ;
#47847 = EDGE_CURVE ( 'NONE', #49612, #11422, #26746, .T. ) ;
#47848 = CARTESIAN_POINT ( 'NONE',  ( 9.367334447929739127, -15.61631861598680082, -57.84717978380999170 ) ) ;
#47849 = CARTESIAN_POINT ( 'NONE',  ( 11.13287445219570060, 32.39951296077789777, -43.97623713944630452 ) ) ;
#47850 = CARTESIAN_POINT ( 'NONE',  ( 72.40383359117168993, 1.117797034538490220, -69.85858842073480446 ) ) ;
#47851 = CARTESIAN_POINT ( 'NONE',  ( 42.23404623588641016, -39.78951633867036719, -75.20128091132379211 ) ) ;
#47852 = EDGE_CURVE ( 'NONE', #2182, #19450, #36246, .T. ) ;
#47853 = VECTOR ( 'NONE', #23214, 1000.000000000000000 ) ;
#47854 =( BOUNDED_CURVE ( )  B_SPLINE_CURVE ( 3, ( #128, #16618, #32062, #16892 ),
 .UNSPECIFIED., .F., .T. ) 
 B_SPLINE_CURVE_WITH_KNOTS ( ( 4, 4 ),
 ( 4.774929739927229910, 4.797305365512180231 ),
 .UNSPECIFIED. ) 
 CURVE ( )  GEOMETRIC_REPRESENTATION_ITEM ( )  RATIONAL_B_SPLINE_CURVE ( ( 1.000000000000000000, 0.9999582780501610202, 0.9999582780501610202, 1.000000000000000000 ) ) 
 REPRESENTATION_ITEM ( '' )  );
#47855 = CIRCLE ( 'NONE', #26062, 1.994283377130261936 ) ;
#47856 =( NAMED_UNIT ( * ) SI_UNIT ( $, .STERADIAN. ) SOLID_ANGLE_UNIT ( ) );
#47857 = AXIS2_PLACEMENT_3D ( 'NONE', #44206, #186, #32381 ) ;
#47858 = FACE_OUTER_BOUND ( 'NONE', #27926, .T. ) ;
#47859 = CARTESIAN_POINT ( 'NONE',  ( -1.143840380081567076, -15.61618894467929941, -35.76111111111109864 ) ) ;
#47860 = CARTESIAN_POINT ( 'NONE',  ( 48.30230902372879598, -54.16106876602380282, -54.73485062140290580 ) ) ;
#47861 = DIRECTION ( 'NONE',  ( -1.000000000000000000, 0.000000000000000000, 0.000000000000000000 ) ) ;
#47862 = CARTESIAN_POINT ( 'NONE',  ( -18.86606260230360022, -50.61618894467959962, 16.85000000000000142 ) ) ;
#47863 = DIRECTION ( 'NONE',  ( -1.000000000000000000, 0.000000000000000000, 0.000000000000000000 ) ) ;
#47864 = CARTESIAN_POINT ( 'NONE',  ( 47.79361911714689626, 23.20098628971269861, -54.82768723803160071 ) ) ;
#47865 = ORIENTED_EDGE ( 'NONE', *, *, #10833, .F. ) ;
#47866 = CARTESIAN_POINT ( 'NONE',  ( 9.612189680941000347, -12.93116213325089880, -79.97149710298209868 ) ) ;
#47867 = DIRECTION ( 'NONE',  ( 0.1686178020941689892, -0.6660492713794449182, -0.7265992051412129005 ) ) ;
#47868 = ORIENTED_EDGE ( 'NONE', *, *, #25470, .T. ) ;
#47869 = CARTESIAN_POINT ( 'NONE',  ( 71.33379467969419352, 1.389468113695450091, -70.26995969721829738 ) ) ;
#47870 = CARTESIAN_POINT ( 'NONE',  ( 60.60270475073690477, -45.62234656557190249, -47.40029600766140305 ) ) ;
#47871 = CARTESIAN_POINT ( 'NONE',  ( 48.44331161791654239, -54.05217057865579022, -54.60670978497837069 ) ) ;
#47872 = DIRECTION ( 'NONE',  ( 0.5877852522924733591, -0.8090169943749473402, 0.000000000000000000 ) ) ;
#47874 = DIRECTION ( 'NONE',  ( 0.000000000000000000, 1.000000000000000000, 0.000000000000000000 ) ) ;
#47873 = CARTESIAN_POINT ( 'NONE',  ( 42.43805389010415041, 8.578463427208918191, -74.21497205410845766 ) ) ;
#47875 = CARTESIAN_POINT ( 'NONE',  ( 63.34104417888273986, -53.11618894467930119, 17.05710678118654755 ) ) ;
#47876 = CARTESIAN_POINT ( 'NONE',  ( 8.222959511069191763, -14.58047957805684902, -66.54933504152046453 ) ) ;
#47877 = ORIENTED_EDGE ( 'NONE', *, *, #27178, .T. ) ;
#47878 = CARTESIAN_POINT ( 'NONE',  ( 8.133937397696209715, -63.11543068638779630, -43.74348518090240390 ) ) ;
#47879 = EDGE_LOOP ( 'NONE', ( #51742, #8503, #11802, #16205, #46052 ) ) ;
#47880 = EDGE_CURVE ( 'NONE', #26299, #49499, #28416, .T. ) ;
#47881 = ORIENTED_EDGE ( 'NONE', *, *, #17029, .T. ) ;
#47882 = CARTESIAN_POINT ( 'NONE',  ( 68.13393739769620083, 0.8838110553206759423, -65.65000000000000568 ) ) ;
#47883 = CARTESIAN_POINT ( 'NONE',  ( 52.28356688864503354, -49.79961370504300078, -77.20029278302882858 ) ) ;
#47884 = CARTESIAN_POINT ( 'NONE',  ( 76.39135428410857287, -16.88413607353903956, -12.75926757094217834 ) ) ;
#47885 = ORIENTED_EDGE ( 'NONE', *, *, #31858, .T. ) ;
#47886 = ORIENTED_EDGE ( 'NONE', *, *, #13964, .T. ) ;
#47887 = CARTESIAN_POINT ( 'NONE',  ( -0.1122294247164806885, 14.32548074922725867, -34.86373113243160304 ) ) ;
#47888 = CARTESIAN_POINT ( 'NONE',  ( 57.40229053555950145, -45.11825314355339600, -25.32419692437829895 ) ) ;
#47889 = CARTESIAN_POINT ( 'NONE',  ( 56.46192173573589912, -50.77770442342179535, -53.81433447105879253 ) ) ;
#47890 = CARTESIAN_POINT ( 'NONE',  ( 19.31296351478360052, 18.65448050664020130, -82.14319696191608955 ) ) ;
#47891 = CARTESIAN_POINT ( 'NONE',  ( 63.27737188425489023, -0.05603756615965699989, -16.72622626800460210 ) ) ;
#47892 = CARTESIAN_POINT ( 'NONE',  ( 51.62357988847099932, -48.69300505533869483, -76.93789418233480149 ) ) ;
#47893 = B_SPLINE_CURVE_WITH_KNOTS ( 'NONE', 3,
 ( #17793, #2328, #21967, #6268, #37715, #14639, #10716, #30609, #37977, #46630, #6524 ),
 .UNSPECIFIED., .F., .F.,
 ( 4, 1, 1, 1, 1, 1, 1, 1, 4 ),
 ( 0.000000000000000000, 0.1250000000000000000, 0.2500000000000000000, 0.3750000000000000000, 0.5000000000000000000, 0.6250000000000000000, 0.7500000000000000000, 0.8750000000000000000, 1.000000000000000000 ),
 .UNSPECIFIED. ) ;
#47894 = AXIS2_PLACEMENT_3D ( 'NONE', #50065, #10237, #6826 ) ;
#47895 = EDGE_LOOP ( 'NONE', ( #50463, #22912, #41697, #23430 ) ) ;
#47896 = FACE_OUTER_BOUND ( 'NONE', #42279, .T. ) ;
#47898 = CARTESIAN_POINT ( 'NONE',  ( 52.34620911275789723, -49.91415201639770771, -77.13858419677869449 ) ) ;
#47897 = CIRCLE ( 'NONE', #38699, 7.910999999999997812 ) ;
#47899 = DIRECTION ( 'NONE',  ( 1.071169953407190059E-15, 3.740764114965449782E-16, -1.000000000000000000 ) ) ;
#47900 = CARTESIAN_POINT ( 'NONE',  ( 0.3209249304026170480, -4.754491132419490285, -34.64999999999999858 ) ) ;
#47901 = CARTESIAN_POINT ( 'NONE',  ( 22.17654210678049864, -10.60882677270349994, -55.79222923803829559 ) ) ;
#47902 = CARTESIAN_POINT ( 'NONE',  ( 13.68912331542219896, -50.41132277470529743, -21.10135350628850048 ) ) ;
#47903 = LINE ( 'NONE', #20875, #11285 ) ;
#47904 = CARTESIAN_POINT ( 'NONE',  ( 11.64736116878922800, -10.17438842308481561, -64.12771089026477966 ) ) ;
#47905 = CARTESIAN_POINT ( 'NONE',  ( 56.87728296015039575, 13.88381105532070059, -15.74456185640559980 ) ) ;
#47906 = CARTESIAN_POINT ( 'NONE',  ( 60.86534162328889863, -45.45085216985310694, -47.04167545792570593 ) ) ;
#47907 = CARTESIAN_POINT ( 'NONE',  ( 17.90522632298731764, -22.20705046304115626, -38.86948870843807669 ) ) ;
#47908 = CARTESIAN_POINT ( 'NONE',  ( 9.727227354358010558, -18.56519311474089662, -49.70986543667950031 ) ) ;
#47909 = CARTESIAN_POINT ( 'NONE',  ( 11.97521819796847886, -10.20490511463765593, -43.74446124033270422 ) ) ;
#47910 = ORIENTED_EDGE ( 'NONE', *, *, #20030, .T. ) ;
#47911 = CARTESIAN_POINT ( 'NONE',  ( 13.48116687393109991, -51.59710020169690381, -74.14993170018701107 ) ) ;
#47912 = EDGE_CURVE ( 'NONE', #24768, #13283, #10650, .T. ) ;
#47913 = CARTESIAN_POINT ( 'NONE',  ( 47.40275506224949709, -54.64653644620720030, -54.66607417010540360 ) ) ;
#47914 =( NAMED_UNIT ( * ) PLANE_ANGLE_UNIT ( ) SI_UNIT ( $, .RADIAN. ) );
#47915 = CARTESIAN_POINT ( 'NONE',  ( 8.222938026844484938, -14.58063686431121120, -36.54933528226675321 ) ) ;
#47916 = EDGE_CURVE ( 'NONE', #3482, #31302, #38776, .T. ) ;
#47917 = LINE ( 'NONE', #42960, #10377 ) ;
#47918 = EDGE_CURVE ( 'NONE', #25861, #35823, #30580, .T. ) ;
#47919 = DIRECTION ( 'NONE',  ( 0.000000000000000000, 0.000000000000000000, -1.000000000000000000 ) ) ;
#47920 = CARTESIAN_POINT ( 'NONE',  ( 47.02070054993090054, -53.74782267376620126, -75.86501933388160523 ) ) ;
#47921 = EDGE_CURVE ( 'NONE', #2764, #46028, #22965, .T. ) ;
#47922 = CARTESIAN_POINT ( 'NONE',  ( 11.46916641887110089, 34.13456839452390312, -17.97103954068960263 ) ) ;
#47923 = CARTESIAN_POINT ( 'NONE',  ( 19.90518632087238515, -8.638643742139599624, -65.16544870160124958 ) ) ;
#47925 = CARTESIAN_POINT ( 'NONE',  ( -5.738263256628330033, -47.06162393351850426, -5.576567369078139436 ) ) ;
#47924 = DIRECTION ( 'NONE',  ( 1.000000000000000000, 0.000000000000000000, 0.000000000000000000 ) ) ;
#47926 = DIRECTION ( 'NONE',  ( 1.000000000000000000, 0.000000000000000000, 0.000000000000000000 ) ) ;
#47927 = DIRECTION ( 'NONE',  ( -0.2267461507313160984, 0.9739538916850897232, -3.885780586188046377E-13 ) ) ;
#47928 = CARTESIAN_POINT ( 'NONE',  ( 48.98237048593380649, 22.65102318943320014, -54.72464718890729785 ) ) ;
#47929 = ORIENTED_EDGE ( 'NONE', *, *, #42050, .T. ) ;
#47930 = VECTOR ( 'NONE', #39901, 1000.000000000000114 ) ;
#47931 = CARTESIAN_POINT ( 'NONE',  ( 52.98400451483280449, -49.60704343698500196, -48.99793967229260261 ) ) ;
#47932 = ORIENTED_EDGE ( 'NONE', *, *, #11059, .F. ) ;
#47933 = CARTESIAN_POINT ( 'NONE',  ( 45.96971012568268833, 6.673253363729896748, -60.41974218095914040 ) ) ;
#47934 = CARTESIAN_POINT ( 'NONE',  ( 12.72604000439749505, -21.52915361658608617, -75.11948688679269992 ) ) ;
#47935 = CARTESIAN_POINT ( 'NONE',  ( 16.13393739769620083, -15.61618894467929941, -20.58999999999999986 ) ) ;
#47936 = CARTESIAN_POINT ( 'NONE',  ( 83.56294434887010425, 13.44742886806319859, -46.81484486652620092 ) ) ;
#47937 = CARTESIAN_POINT ( 'NONE',  ( 9.507110174141249814, -18.03025597891349818, -57.34162007823109519 ) ) ;
#47938 = CARTESIAN_POINT ( 'NONE',  ( 52.70127179790330274, 18.52894807824059953, -48.78999762614679980 ) ) ;
#47939 = CARTESIAN_POINT ( 'NONE',  ( 56.17223871318630302, -45.28676914461929925, -16.17739736399530059 ) ) ;
#47940 = CARTESIAN_POINT ( 'NONE',  ( 53.63393739769619373, -62.11618894467930119, 16.35000000000000142 ) ) ;
#47941 = VERTEX_POINT ( 'NONE', #30051 ) ;
#47942 = CARTESIAN_POINT ( 'NONE',  ( 22.91038278696110098, -11.65809141310010055, -41.11923310072890558 ) ) ;
#47943 = EDGE_CURVE ( 'NONE', #23957, #24198, #38986, .T. ) ;
#47944 = EDGE_LOOP ( 'NONE', ( #35034, #35063, #33036, #42194 ) ) ;
#47945 = CARTESIAN_POINT ( 'NONE',  ( 11.22384634879449905, -65.01277928531338546, -16.94931743789749845 ) ) ;
#47946 = CARTESIAN_POINT ( 'NONE',  ( 12.41878523604639994, 34.20092968456749816, -47.33836379614209733 ) ) ;
#47947 = CARTESIAN_POINT ( 'NONE',  ( 72.77520546617009245, 1.386446979194299933, -62.50785065198430601 ) ) ;
#47948 = CARTESIAN_POINT ( 'NONE',  ( 50.15663463400569810, -52.84355308394439987, -53.36882020266619975 ) ) ;
#47949 = CARTESIAN_POINT ( 'NONE',  ( 11.02457163261952822, -64.89120435510172058, -23.16550869442561833 ) ) ;
#47950 = CARTESIAN_POINT ( 'NONE',  ( 51.35983792756474742, 3.333806696842658290, -76.65609622433946413 ) ) ;
#47951 = VERTEX_POINT ( 'NONE', #10164 ) ;
#47952 = DIRECTION ( 'NONE',  ( 1.000000000000000000, 0.000000000000000000, 0.000000000000000000 ) ) ;
#47953 = CARTESIAN_POINT ( 'NONE',  ( 11.13393739769619906, -63.20944975704810531, -43.74432592331839942 ) ) ;
#47954 = AXIS2_PLACEMENT_3D ( 'NONE', #21200, #33256, #17295 ) ;
#47955 = CARTESIAN_POINT ( 'NONE',  ( 68.13393739769810509, 19.38381105532030091, -71.50000000000198952 ) ) ;
#47956 = ORIENTED_EDGE ( 'NONE', *, *, #29513, .F. ) ;
#47957 = CARTESIAN_POINT ( 'NONE',  ( 8.222937397696199469, -15.61618894467929941, -32.14999999999999858 ) ) ;
#47958 = CARTESIAN_POINT ( 'NONE',  ( 56.73072851102580216, 19.11736299019269936, -52.75329813363410381 ) ) ;
#47959 = CARTESIAN_POINT ( 'NONE',  ( 12.13393739769638913, 24.18330853958551074, -22.88372919474997857 ) ) ;
#47960 = CARTESIAN_POINT ( 'NONE',  ( 8.412057011451022248, -13.65889379580994145, -48.58652191394980946 ) ) ;
#47961 = VERTEX_POINT ( 'NONE', #3082 ) ;
#47962 = CARTESIAN_POINT ( 'NONE',  ( 17.16948262820418236, -23.52718926469356120, -35.96600018786083552 ) ) ;
#47963 = CARTESIAN_POINT ( 'NONE',  ( 19.13393739769620083, -49.61618894467939356, -83.01107220193038927 ) ) ;
#47964 = CARTESIAN_POINT ( 'NONE',  ( 9.366715917462860475, -15.61603296970410071, -51.45282021618999835 ) ) ;
#47965 = CARTESIAN_POINT ( 'NONE',  ( 51.97663139176439984, 19.86204042051310026, -51.25532567384490079 ) ) ;
#47966 = EDGE_CURVE ( 'NONE', #32793, #19147, #29386, .T. ) ;
#47967 = CARTESIAN_POINT ( 'NONE',  ( 19.25379761885410446, -7.984073100670400436, -71.41585254811130312 ) ) ;
#47968 = CARTESIAN_POINT ( 'NONE',  ( 53.29384558423090112, 19.31433099946569953, -28.15000000000000213 ) ) ;
#47969 = CARTESIAN_POINT ( 'NONE',  ( 73.38393739769610136, 4.883811055320659733, -84.94863984844540994 ) ) ;
#47970 = APPLICATION_PROTOCOL_DEFINITION ( 'draft international standard', 'automotive_design', 1998, #19408 ) ;
#47971 = VERTEX_POINT ( 'NONE', #51546 ) ;
#47972 = CARTESIAN_POINT ( 'NONE',  ( 9.936147368269889313, -11.48168866577140079, -67.41991821385050798 ) ) ;
#47973 = AXIS2_PLACEMENT_3D ( 'NONE', #19845, #24268, #35836 ) ;
#47974 = CARTESIAN_POINT ( 'NONE',  ( 1.027904703268269992, 11.45423359053189927, -15.65000000000000036 ) ) ;
#47975 = CARTESIAN_POINT ( 'NONE',  ( 9.944491257508540016, -20.09032267960250095, -32.14999999999999858 ) ) ;
#47976 = CARTESIAN_POINT ( 'NONE',  ( 47.27371103217519988, 23.27521486086419955, -75.00312280669810150 ) ) ;
#47977 = DIRECTION ( 'NONE',  ( -0.7071067811865492381, 0.000000000000000000, 0.7071067811865457964 ) ) ;
#47978 = CARTESIAN_POINT ( 'NONE',  ( 0.1457840807894888180, 19.59951024407514097, -34.68167773519660813 ) ) ;
#47979 = EDGE_CURVE ( 'NONE', #3425, #28507, #4353, .T. ) ;
#47980 = CARTESIAN_POINT ( 'NONE',  ( 12.06706412657739946, 33.80468957826779786, -16.41672221714649993 ) ) ;
#47981 = CARTESIAN_POINT ( 'NONE',  ( 20.73645074902539776, -22.45721164306379691, -73.81915773946390402 ) ) ;
#47982 = EDGE_CURVE ( 'NONE', #25965, #4949, #8392, .T. ) ;
#47983 = AXIS2_PLACEMENT_3D ( 'NONE', #3655, #31913, #39805 ) ;
#47984 = CARTESIAN_POINT ( 'NONE',  ( 57.13425863431969987, -50.61839434688920392, -74.14885654434310425 ) ) ;
#47985 = B_SPLINE_CURVE_WITH_KNOTS ( 'NONE', 3,
 ( #48173, #36892, #32672, #44236, #20631, #4404, #48700, #20372, #16456, #16200, #51848, #36361, #9119, #992, #15952, #25069, #43982, #32410 ),
 .UNSPECIFIED., .F., .F.,
 ( 4, 2, 2, 2, 2, 2, 2, 2, 4 ),
 ( 0.4999996453781777039, 0.5624996897059054701, 0.6249997340336331808, 0.6874997783613608915, 0.7499998226890887132, 0.8124998670168164239, 0.8749999113445443566, 0.9374999556722721783, 1.000000000000000000 ),
 .UNSPECIFIED. ) ;
#47987 = CARTESIAN_POINT ( 'NONE',  ( 22.72480800315950233, -13.84492856927137794, -60.36947377164519679 ) ) ;
#47986 =( NAMED_UNIT ( * ) SI_UNIT ( $, .STERADIAN. ) SOLID_ANGLE_UNIT ( ) );
#47988 = CARTESIAN_POINT ( 'NONE',  ( 63.11172336169240538, 1.097085799869280009, -68.85468201266050414 ) ) ;
#47989 = CARTESIAN_POINT ( 'NONE',  ( 61.25468486569459969, 14.04656514930960043, -46.98529749939520173 ) ) ;
#47990 = LINE ( 'NONE', #44048, #6373 ) ;
#47991 = ORIENTED_EDGE ( 'NONE', *, *, #24833, .T. ) ;
#47992 = CARTESIAN_POINT ( 'NONE',  ( 52.81905794073989568, -49.66695704333110228, -48.62057682596950059 ) ) ;
#47993 = CARTESIAN_POINT ( 'NONE',  ( 57.34862278082039921, -45.74573972699900537, -26.25059263399790410 ) ) ;
#47994 = CARTESIAN_POINT ( 'NONE',  ( 17.37335237021048684, -23.49782243706750862, -66.24288056328899188 ) ) ;
#47995 = CARTESIAN_POINT ( 'NONE',  ( 56.98351099668879982, 14.61386344210539789, -26.22547853219269953 ) ) ;
#47996 = CARTESIAN_POINT ( 'NONE',  ( 20.18929396301779988, -9.366326791539540508, -73.91587056106729392 ) ) ;
#47997 = CARTESIAN_POINT ( 'NONE',  ( 51.46000097675949547, 18.08790154638520065, -76.62475863243518859 ) ) ;
#47998 = CARTESIAN_POINT ( 'NONE',  ( 53.33641448323419354, 18.17849414707670164, -48.94981348398439991 ) ) ;
#47999 = CARTESIAN_POINT ( 'NONE',  ( 71.28186865452410359, 1.191644800533229853, -70.64005307315129301 ) ) ;
#48000 = CARTESIAN_POINT ( 'NONE',  ( 53.06963669637619319, -49.53524040181889632, -48.79723990372919218 ) ) ;
#48001 = VERTEX_POINT ( 'NONE', #23733 ) ;
#48002 = DIRECTION ( 'NONE',  ( 0.000000000000000000, 0.000000000000000000, -1.000000000000000000 ) ) ;
#48003 = VECTOR ( 'NONE', #44964, 1000.000000000000000 ) ;
#48004 = CARTESIAN_POINT ( 'NONE',  ( 47.75094631897339781, -54.46528010514310125, -54.88743874810780454 ) ) ;
#48005 = CARTESIAN_POINT ( 'NONE',  ( 9.367580626013266354, -15.02763158364818352, -67.87485971631076609 ) ) ;
#48006 = FACE_OUTER_BOUND ( 'NONE', #3723, .T. ) ;
#48007 = CARTESIAN_POINT ( 'NONE',  ( 61.28317973945440400, -30.65315163351740324, -16.34104759998400169 ) ) ;
#48008 = CARTESIAN_POINT ( 'NONE',  ( 71.58179376171669617, 0.9036513197889520788, -60.73950228677190211 ) ) ;
#48009 = DIRECTION ( 'NONE',  ( 1.000000000000000000, 0.000000000000000000, 0.000000000000000000 ) ) ;
#48010 = AXIS2_PLACEMENT_3D ( 'NONE', #26530, #50404, #51435 ) ;
#48011 = CARTESIAN_POINT ( 'NONE',  ( 72.18916782744800287, 1.409272994606969975, -61.45923610184129871 ) ) ;
#48012 = CARTESIAN_POINT ( 'NONE',  ( 50.97850582344351977, -35.25929517202420271, -76.38917648635938917 ) ) ;
#48013 = CARTESIAN_POINT ( 'NONE',  ( 61.26569908036744039, -45.23341354807755721, -27.95968211902695799 ) ) ;
#48014 = ORIENTED_EDGE ( 'NONE', *, *, #35749, .T. ) ;
#48015 = EDGE_LOOP ( 'NONE', ( #30414, #21096, #35248, #49757 ) ) ;
#48016 = CARTESIAN_POINT ( 'NONE',  ( 16.13393739769599833, 14.38381105532070059, -59.64999999999999147 ) ) ;
#48017 = PLANE ( 'NONE',  #13531 ) ;
#48018 = EDGE_LOOP ( 'NONE', ( #23209, #27109, #11671, #39696, #16227, #36973 ) ) ;
#48019 = CARTESIAN_POINT ( 'NONE',  ( 20.11802340169658265, -8.703638663582415447, -59.17429998693496884 ) ) ;
#48020 = CARTESIAN_POINT ( 'NONE',  ( 15.69633972878563632, -8.840832517840322424, -49.93237391020534943 ) ) ;
#48021 = VERTEX_POINT ( 'NONE', #47875 ) ;
#48022 = CARTESIAN_POINT ( 'NONE',  ( -5.055476499123447098, 11.23874896328612571, -39.16253382332155297 ) ) ;
#48023 = CARTESIAN_POINT ( 'NONE',  ( 17.87670698131379865, 1.145880372109089995, -34.70985242058479514 ) ) ;
#48024 = CARTESIAN_POINT ( 'NONE',  ( 22.46011990848845130, -10.75453471358487434, -35.29933276554705657 ) ) ;
#48025 = EDGE_CURVE ( 'NONE', #35705, #2432, #859, .T. ) ;
#48026 = CARTESIAN_POINT ( 'NONE',  ( 8.005967485763431313, -17.00140559439540056, -42.73859950308099798 ) ) ;
#48027 = CARTESIAN_POINT ( 'NONE',  ( 52.71325343205820246, -49.75453022050439955, -48.80820688877259528 ) ) ;
#48028 = EDGE_CURVE ( 'NONE', #19317, #8526, #26873, .T. ) ;
#48029 = AXIS2_PLACEMENT_3D ( 'NONE', #45050, #41627, #20664 ) ;
#48030 = DIRECTION ( 'NONE',  ( 1.000000000000000000, 0.000000000000000000, 0.000000000000000000 ) ) ;
#48031 = CARTESIAN_POINT ( 'NONE',  ( 10.85466640524320070, 33.73459223951330443, -17.55961383757199812 ) ) ;
#48032 = DIRECTION ( 'NONE',  ( 1.000000000000000000, 0.000000000000000000, 0.000000000000000000 ) ) ;
#48033 = EDGE_CURVE ( 'NONE', #8205, #30697, #17601, .T. ) ;
#48034 = ORIENTED_EDGE ( 'NONE', *, *, #30165, .F. ) ;
#48035 = CARTESIAN_POINT ( 'NONE',  ( 11.59229128443909929, -65.37912454849278276, -22.55625441136039910 ) ) ;
#48036 = CARTESIAN_POINT ( 'NONE',  ( 8.929533209956950657, -12.50435150369649939, -81.14228717839660021 ) ) ;
#48037 = CARTESIAN_POINT ( 'NONE',  ( 43.41855353999969935, 14.15426166984780032, -7.209154067359100360 ) ) ;
#48038 = B_SPLINE_CURVE_WITH_KNOTS ( 'NONE', 3,
 ( #30124, #46921, #34576, #11007, #37750, #38009, #30641, #21742, #18082, #26450 ),
 .UNSPECIFIED., .F., .F.,
 ( 4, 2, 2, 2, 4 ),
 ( 0.000000000000000000, 0.2493604919034558554, 0.3740407378551894313, 0.4363808608310561499, 0.4987209838069229795 ),
 .UNSPECIFIED. ) ;
#48039 = CARTESIAN_POINT ( 'NONE',  ( 13.96110342106720026, 21.00531966820119933, -75.65676662446109901 ) ) ;
#48040 = CARTESIAN_POINT ( 'NONE',  ( 52.08783364885010059, 18.38123939400390228, -77.13960933460720071 ) ) ;
#48041 = CARTESIAN_POINT ( 'NONE',  ( 83.30156758793411598, -44.93098646499529991, -46.93423283396209911 ) ) ;
#48042 = CARTESIAN_POINT ( 'NONE',  ( 16.13393739769620083, -15.61618894467929941, -32.14999999999999858 ) ) ;
#48043 = CARTESIAN_POINT ( 'NONE',  ( 7.905295319356000050, -16.13788833661330102, -38.48751448508949835 ) ) ;
#48044 = EDGE_CURVE ( 'NONE', #13074, #16879, #16864, .T. ) ;
#48045 = ORIENTED_EDGE ( 'NONE', *, *, #25486, .T. ) ;
#48046 = CARTESIAN_POINT ( 'NONE',  ( 53.56320387222690016, -48.99516858426609645, -27.18005901862589724 ) ) ;
#48047 = CARTESIAN_POINT ( 'NONE',  ( 14.01533392342379969, -50.49302913403720083, -21.05253849812260114 ) ) ;
#48048 = CARTESIAN_POINT ( 'NONE',  ( 18.08024390712562024, -23.31108359709902800, -39.92886493447741714 ) ) ;
#48049 = CARTESIAN_POINT ( 'NONE',  ( 20.11812365984145146, -22.52867927707677254, -64.12566632045644610 ) ) ;
#48050 = CARTESIAN_POINT ( 'NONE',  ( 22.87920530775617323, -16.16928024828671084, -56.47886066825785178 ) ) ;
#48051 = CARTESIAN_POINT ( 'NONE',  ( 33.13393739769620083, 7.383811055320659733, -72.14999999999999147 ) ) ;
#48052 = ORIENTED_EDGE ( 'NONE', *, *, #9245, .F. ) ;
#48053 = DIRECTION ( 'NONE',  ( 0.000000000000000000, 0.000000000000000000, 1.000000000000000000 ) ) ;
#48054 = CARTESIAN_POINT ( 'NONE',  ( 47.32853495261879573, 23.46463025610070119, -54.63689417515509916 ) ) ;
#48055 = CARTESIAN_POINT ( 'NONE',  ( 16.38470059807072943, 18.38381071981026693, -83.24417156243271165 ) ) ;
#48056 = CARTESIAN_POINT ( 'NONE',  ( 63.20675433611359750, 1.270877794983130027, -62.54449628245689752 ) ) ;
#48057 = CARTESIAN_POINT ( 'NONE',  ( 57.46594764351250006, -50.61618894467939356, -53.92796738109959875 ) ) ;
#48058 = CARTESIAN_POINT ( 'NONE',  ( 41.74202016262009352, 12.84695517036499979, -4.572451372512130519 ) ) ;
#48059 = DIRECTION ( 'NONE',  ( 0.000000000000000000, 0.000000000000000000, -1.000000000000000000 ) ) ;
#48060 = DIRECTION ( 'NONE',  ( 1.000000000000000000, 0.000000000000000000, 0.000000000000000000 ) ) ;
#48061 = CARTESIAN_POINT ( 'NONE',  ( 55.06144681897199433, -48.49167527187719884, -48.36672530871140196 ) ) ;
#48062 = CARTESIAN_POINT ( 'NONE',  ( 68.13393739769840352, -50.61618894467879670, -73.25000000000220268 ) ) ;
#48063 = AXIS2_PLACEMENT_3D ( 'NONE', #17530, #36923, #33499 ) ;
#48064 = CARTESIAN_POINT ( 'NONE',  ( 68.13393739769598767, -2.032350560840590070, -29.09832030244560741 ) ) ;
#48065 = CARTESIAN_POINT ( 'NONE',  ( 17.21347160910390173, -53.11618894467930119, -76.14999999999999147 ) ) ;
#48066 = CARTESIAN_POINT ( 'NONE',  ( 20.11812447700029693, -8.703699102511096797, -73.17433468560057008 ) ) ;
#48067 = DIRECTION ( 'NONE',  ( 0.000000000000000000, 0.000000000000000000, -1.000000000000000000 ) ) ;
#48068 = ORIENTED_EDGE ( 'NONE', *, *, #23765, .T. ) ;
#48069 = CARTESIAN_POINT ( 'NONE',  ( -0.1114929980067364962, -10.52519485297225366, -34.86345228575846988 ) ) ;
#48070 = FACE_OUTER_BOUND ( 'NONE', #28615, .T. ) ;
#48071 = CARTESIAN_POINT ( 'NONE',  ( 68.13393739769618662, -0.5161889446793590519, -65.65000000000000568 ) ) ;
#48072 = CARTESIAN_POINT ( 'NONE',  ( 12.06548384426220011, -9.083113220787328856, -81.23899999999999011 ) ) ;
#48073 = ORIENTED_EDGE ( 'NONE', *, *, #26191, .T. ) ;
#48074 = CARTESIAN_POINT ( 'NONE',  ( 18.30677137431719714, 21.00531966820109986, -75.65676662446099954 ) ) ;
#48075 = ORIENTED_EDGE ( 'NONE', *, *, #50747, .F. ) ;
#48076 = AXIS2_PLACEMENT_3D ( 'NONE', #41424, #26200, #37243 ) ;
#48077 = ORIENTED_EDGE ( 'NONE', *, *, #44165, .F. ) ;
#48078 = CARTESIAN_POINT ( 'NONE',  ( 56.62831714707169795, -46.14027970578780469, -26.25643374699650323 ) ) ;
#48079 = CARTESIAN_POINT ( 'NONE',  ( 23.40109865623389851, -16.77414853570180142, -81.23899999999999011 ) ) ;
#48080 = CIRCLE ( 'NONE', #47056, 0.5000000000000045519 ) ;
#48081 = CARTESIAN_POINT ( 'NONE',  ( 18.62287818089072644, -13.80786761600151102, -22.14999999999999858 ) ) ;
#48082 = CARTESIAN_POINT ( 'NONE',  ( 12.13393739769649926, 24.18330853958550364, -74.14999999999999147 ) ) ;
#48083 = CARTESIAN_POINT ( 'NONE',  ( 13.88552899772848015, -22.30103889375535431, -35.45045784522820753 ) ) ;
#48084 = ORIENTED_EDGE ( 'NONE', *, *, #49341, .T. ) ;
#48085 = DIRECTION ( 'NONE',  ( 1.000000000000000000, 0.000000000000000000, 0.000000000000000000 ) ) ;
#48086 = EDGE_CURVE ( 'NONE', #7993, #6837, #31778, .T. ) ;
#48087 = VERTEX_POINT ( 'NONE', #23475 ) ;
#48088 = VERTEX_POINT ( 'NONE', #48125 ) ;
#48089 = DIRECTION ( 'NONE',  ( -1.000000000000000000, 0.000000000000000000, 0.000000000000000000 ) ) ;
#48090 = FACE_OUTER_BOUND ( 'NONE', #10952, .T. ) ;
#48091 = CARTESIAN_POINT ( 'NONE',  ( 60.30540951500729818, 14.59285682385899996, -47.61343627861140249 ) ) ;
#48092 = CARTESIAN_POINT ( 'NONE',  ( 14.89345596857563869, -8.902066654702450066, -39.89498197283463554 ) ) ;
#48093 = VECTOR ( 'NONE', #17667, 1000.000000000000000 ) ;
#48094 = CARTESIAN_POINT ( 'NONE',  ( 40.50275677532349761, -44.77423425411610225, -4.148922563335220026 ) ) ;
#48095 = CARTESIAN_POINT ( 'NONE',  ( -2.629620175395499970, 17.44203635409839848, -4.565428260498799240 ) ) ;
#48096 = CARTESIAN_POINT ( 'NONE',  ( 0.6320745533423832718, -22.45076187167874338, -34.77490583097448962 ) ) ;
#48097 = CARTESIAN_POINT ( 'NONE',  ( 61.28594175748709461, 13.99813740456359845, -28.10457713912520106 ) ) ;
#48098 = CARTESIAN_POINT ( 'NONE',  ( 22.40813251518540028, -10.90224963547539971, -61.08240372876090163 ) ) ;
#48099 = EDGE_CURVE ( 'NONE', #13493, #45507, #7572, .T. ) ;
#48100 = ORIENTED_EDGE ( 'NONE', *, *, #39936, .T. ) ;
#48101 = CARTESIAN_POINT ( 'NONE',  ( 57.27937794702199170, 16.09726112234089968, -47.83631691340819714 ) ) ;
#48102 = CIRCLE ( 'NONE', #25492, 0.9999999999999964473 ) ;
#48103 = LINE ( 'NONE', #11954, #11882 ) ;
#48104 = CARTESIAN_POINT ( 'NONE',  ( 12.75847677699380078, 34.25788405236250611, -47.26854789447209271 ) ) ;
#48105 = EDGE_CURVE ( 'NONE', #34841, #51612, #40197, .T. ) ;
#48106 = CARTESIAN_POINT ( 'NONE',  ( 72.45273174173409814, 1.404167647216130188, -69.55372334320209404 ) ) ;
#48107 = CARTESIAN_POINT ( 'NONE',  ( 43.32052231349704385, -39.89583416345196554, -69.94913773093004750 ) ) ;
#48108 = DIRECTION ( 'NONE',  ( 0.000000000000000000, -1.000000000000000000, 0.000000000000000000 ) ) ;
#48109 = CARTESIAN_POINT ( 'NONE',  ( 46.70834335223779732, 22.49584860873379810, -75.96332501265769110 ) ) ;
#48110 = CARTESIAN_POINT ( 'NONE',  ( 48.54167993331880382, -54.06704517894050355, -54.75887336934849259 ) ) ;
#48111 = CARTESIAN_POINT ( 'NONE',  ( -8.870287765918970280, 13.09110620826400151, -5.844096418666690163 ) ) ;
#48112 = CARTESIAN_POINT ( 'NONE',  ( 63.83267354985670750, 1.033012681683380007, -69.83402047387519929 ) ) ;
#48113 = DIRECTION ( 'NONE',  ( 0.000000000000000000, 0.000000000000000000, 1.000000000000000000 ) ) ;
#48114 = CARTESIAN_POINT ( 'NONE',  ( 71.33393739769650210, 1.396834109478129804, -61.06337307536569625 ) ) ;
#48115 = ORIENTED_EDGE ( 'NONE', *, *, #50166, .T. ) ;
#48116 = CARTESIAN_POINT ( 'NONE',  ( 11.31465934174710064, -9.934475242017009933, -32.34342564320699864 ) ) ;
#48117 = CARTESIAN_POINT ( 'NONE',  ( 64.64722926691220550, 0.9479899806831150189, -60.76708149872590070 ) ) ;
#48118 = ORIENTED_EDGE ( 'NONE', *, *, #22207, .F. ) ;
#48119 = FACE_OUTER_BOUND ( 'NONE', #4151, .T. ) ;
#48120 = CARTESIAN_POINT ( 'NONE',  ( 60.39135641171679936, -45.74253818135839822, -47.49811677804770227 ) ) ;
#48121 = LINE ( 'NONE', #40257, #2812 ) ;
#48122 = CYLINDRICAL_SURFACE ( 'NONE', #25239, 39.00000000000000711 ) ;
#48124 = CARTESIAN_POINT ( 'NONE',  ( 18.20459725043313526, -23.32129460736597082, -78.20899634472944228 ) ) ;
#48123 = CARTESIAN_POINT ( 'NONE',  ( 41.84854853683915366, 8.515723429679729506, -77.06240910697275126 ) ) ;
#48125 = CARTESIAN_POINT ( 'NONE',  ( 16.15069456443260520, -51.05177125324679110, -20.15000000000000213 ) ) ;
#48126 = CARTESIAN_POINT ( 'NONE',  ( 23.04646243352704005, -19.60031697277015539, -51.67433271905296976 ) ) ;
#48127 = ORIENTED_EDGE ( 'NONE', *, *, #43237, .F. ) ;
#48128 = CARTESIAN_POINT ( 'NONE',  ( 83.05638573198200447, -45.46258680162930688, -47.55746740334460299 ) ) ;
#48129 = AXIS2_PLACEMENT_3D ( 'NONE', #51383, #8131, #39584 ) ;
#48130 = EDGE_LOOP ( 'NONE', ( #8247, #44649, #25792, #11343, #40991, #14304, #5889, #46420 ) ) ;
#48131 = VERTEX_POINT ( 'NONE', #19825 ) ;
#48132 = FACE_OUTER_BOUND ( 'NONE', #43001, .T. ) ;
#48133 = CARTESIAN_POINT ( 'NONE',  ( 52.38380618068715933, -49.88586802196508785, -77.22917115513992314 ) ) ;
#48134 = CARTESIAN_POINT ( 'NONE',  ( 76.39110052345097301, -16.48608635013552615, -12.75816298384496683 ) ) ;
#48135 = CARTESIAN_POINT ( 'NONE',  ( 49.44978923146539529, -53.54099393320139910, -54.25462396068540016 ) ) ;
#48136 = ORIENTED_EDGE ( 'NONE', *, *, #50771, .T. ) ;
#48137 = ORIENTED_EDGE ( 'NONE', *, *, #36167, .T. ) ;
#48138 = CARTESIAN_POINT ( 'NONE',  ( 47.81335647225210295, 23.16511464041720103, -54.71582838624409817 ) ) ;
#48139 = CARTESIAN_POINT ( 'NONE',  ( 57.45483112941150239, -45.11618894539299873, -25.32823465277989783 ) ) ;
#48140 = CARTESIAN_POINT ( 'NONE',  ( 56.38083218843890165, -50.72507171055699615, -53.29065863793299229 ) ) ;
#48141 = ADVANCED_FACE ( 'NONE', ( #47617 ), #44370, .T. ) ;
#48142 = CARTESIAN_POINT ( 'NONE',  ( 14.13393739769640156, 10.38381105532060111, -35.14999999999999858 ) ) ;
#48143 = CARTESIAN_POINT ( 'NONE',  ( 52.13393739769618662, -30.31618894467939995, -65.65000000000000568 ) ) ;
#48144 = CARTESIAN_POINT ( 'NONE',  ( -18.86606260230390220, 19.38381105532060289, 14.21249999999999858 ) ) ;
#48145 = B_SPLINE_CURVE_WITH_KNOTS ( 'NONE', 3,
 ( #23912, #11645, #15821, #43616, #15316, #39938 ),
 .UNSPECIFIED., .F., .F.,
 ( 4, 2, 4 ),
 ( -0.0006077122342960819372, 0.000000000000000000, 0.03318971727292711893 ),
 .UNSPECIFIED. ) ;
#48146 = EDGE_LOOP ( 'NONE', ( #35443, #2257, #36786, #32414, #17751 ) ) ;
#48147 = DIRECTION ( 'NONE',  ( -1.000000000000000000, 0.000000000000000000, 0.000000000000000000 ) ) ;
#48148 = CARTESIAN_POINT ( 'NONE',  ( 52.78679729302229617, -50.32040557307429651, -76.98734330441610041 ) ) ;
#48149 = CARTESIAN_POINT ( 'NONE',  ( 60.23130391297029718, 14.55066440145539985, -47.24246919202519734 ) ) ;
#48150 = DIRECTION ( 'NONE',  ( 0.000000000000000000, 0.000000000000000000, -1.000000000000000000 ) ) ;
#48151 = CARTESIAN_POINT ( 'NONE',  ( 14.37574545305890084, -23.26442460248919986, -56.58441854867449905 ) ) ;
#48152 = CARTESIAN_POINT ( 'NONE',  ( 12.32752820270880001, -50.13317366860820101, -21.15176873371889954 ) ) ;
#48153 = CARTESIAN_POINT ( 'NONE',  ( 18.80380761535086265, -51.60309332616136402, -15.76544335866666913 ) ) ;
#48154 = CARTESIAN_POINT ( 'NONE',  ( -0.007164427059776000244, -27.04615419348650107, -34.77269723891829756 ) ) ;
#48155 = CARTESIAN_POINT ( 'NONE',  ( 61.31460642264700311, -45.57262733401680777, -47.65164362830709877 ) ) ;
#48156 =( BOUNDED_CURVE ( )  B_SPLINE_CURVE ( 2, ( #36190, #15521, #47751 ),
 .UNSPECIFIED., .F., .T. ) 
 B_SPLINE_CURVE_WITH_KNOTS ( ( 3, 3 ),
 ( 1.923142637335169880, 4.853851569642519515 ),
 .UNSPECIFIED. ) 
 CURVE ( )  GEOMETRIC_REPRESENTATION_ITEM ( )  RATIONAL_B_SPLINE_CURVE ( ( 1.003436844930660099, 1.004455541116340056, 1.000597593688439924 ) ) 
 REPRESENTATION_ITEM ( '' )  );
#48157 = FACE_OUTER_BOUND ( 'NONE', #22704, .T. ) ;
#48158 = CARTESIAN_POINT ( 'NONE',  ( 10.98133074358459993, -10.80025665254149914, -52.08643336858800410 ) ) ;
#48159 = AXIS2_PLACEMENT_3D ( 'NONE', #9383, #29774, #25327 ) ;
#48160 = CARTESIAN_POINT ( 'NONE',  ( 23.83903855266338923, -13.54551783030957779, -41.70899764726264891 ) ) ;
#48161 = VERTEX_POINT ( 'NONE', #31341 ) ;
#48162 = AXIS2_PLACEMENT_3D ( 'NONE', #15739, #44284, #11563 ) ;
#48163 = CARTESIAN_POINT ( 'NONE',  ( 13.78482046302009856, -51.32863061914500236, -74.59027663913769857 ) ) ;
#48164 = CARTESIAN_POINT ( 'NONE',  ( 47.31045676778030185, -54.71408003619829685, -54.75273663584969341 ) ) ;
#48165 = EDGE_CURVE ( 'NONE', #6375, #51520, #12583, .T. ) ;
#48166 = CARTESIAN_POINT ( 'NONE',  ( 17.90517255728681434, -9.025312231919581762, -38.03615537510474809 ) ) ;
#48167 = TOROIDAL_SURFACE ( 'NONE', #25554, 31.45861873485090143, 3.000000000000000000 ) ;
#48168 = CARTESIAN_POINT ( 'NONE',  ( 20.75744454082159862, -20.94213870710139958, -77.11961558469170086 ) ) ;
#48169 = CARTESIAN_POINT ( 'NONE',  ( 60.88209114001612932, -45.44978581739131585, -47.12495023380284920 ) ) ;
#48170 = CARTESIAN_POINT ( 'NONE',  ( 10.22095790285375294, -12.20831385113555889, -75.61947464293628229 ) ) ;
#48171 = DIRECTION ( 'NONE',  ( 0.000000000000000000, -1.000000000000000000, 0.000000000000000000 ) ) ;
#48173 = CARTESIAN_POINT ( 'NONE',  ( 24.04526354826459666, -15.61618910718878794, -73.50766907743336276 ) ) ;
#48172 = CARTESIAN_POINT ( 'NONE',  ( 64.93393739769619799, 11.38381105532070059, -69.34999999999999432 ) ) ;
#48174 = AXIS2_PLACEMENT_3D ( 'NONE', #35794, #3832, #11185 ) ;
#48175 = CARTESIAN_POINT ( 'NONE',  ( 14.55219295556159409, -51.70197612871098869, -75.56421430877743717 ) ) ;
#48176 = CARTESIAN_POINT ( 'NONE',  ( 48.56282070406520290, 22.79147592108370191, -54.65722455203289343 ) ) ;
#48177 = ORIENTED_EDGE ( 'NONE', *, *, #49527, .F. ) ;
#48178 = CARTESIAN_POINT ( 'NONE',  ( 52.64536150580070029, -49.78637824963190184, -48.56191546059360320 ) ) ;
#48179 = ORIENTED_EDGE ( 'NONE', *, *, #34207, .T. ) ;
#48180 = CARTESIAN_POINT ( 'NONE',  ( 45.61405083969839325, 7.915465039487636467, -62.73908642572272498 ) ) ;
#48181 = CARTESIAN_POINT ( 'NONE',  ( 14.13393739769619906, -41.61618894467930119, -35.14999999999999858 ) ) ;
#48183 = CARTESIAN_POINT ( 'NONE',  ( 53.22743915834050199, 17.91784085086679923, -26.91023106930159869 ) ) ;
#48182 = CARTESIAN_POINT ( 'NONE',  ( 83.09574564639500238, 13.66248835152879870, -46.39644155595900799 ) ) ;
#48184 = CARTESIAN_POINT ( 'NONE',  ( 23.07179105164740207, -16.88455221006540086, -60.51037732077569586 ) ) ;
#48185 = CARTESIAN_POINT ( 'NONE',  ( 52.82750199176329886, 18.46317551911579713, -48.94276306907110552 ) ) ;
#48186 = CARTESIAN_POINT ( 'NONE',  ( 56.73667485601559690, -45.26434324106369900, -17.73083290624459707 ) ) ;
#48187 = CARTESIAN_POINT ( 'NONE',  ( 14.34417029198879945, -51.11618894467930119, -22.49240188329099865 ) ) ;
#48188 = CIRCLE ( 'NONE', #38166, 1.000000000000000000 ) ;
#48189 = ORIENTED_EDGE ( 'NONE', *, *, #11891, .T. ) ;
#48190 = CARTESIAN_POINT ( 'NONE',  ( 12.71275554691149878, -8.553451307824580852, -40.64391951434709682 ) ) ;
#48191 = ORIENTED_EDGE ( 'NONE', *, *, #8979, .F. ) ;
#48192 = CARTESIAN_POINT ( 'NONE',  ( 11.06646970394739959, -65.01491572843740130, -17.18453585839250053 ) ) ;
#48193 = CARTESIAN_POINT ( 'NONE',  ( 10.31246831649800022, 32.20023774900970182, -45.84855598906619889 ) ) ;
#48194 = DIRECTION ( 'NONE',  ( 0.000000000000000000, 1.000000000000000000, 0.000000000000000000 ) ) ;
#48195 = CARTESIAN_POINT ( 'NONE',  ( 52.30324767688179577, -50.21879278929849733, -49.47276378316949774 ) ) ;
#48196 = CARTESIAN_POINT ( 'NONE',  ( 8.813920544456330219, 32.04044820803110127, -46.67144773886860065 ) ) ;
#48197 = CARTESIAN_POINT ( 'NONE',  ( 64.93393739769578588, 0.9098571636355720083, -70.12325384926869276 ) ) ;
#48198 = AXIS2_PLACEMENT_3D ( 'NONE', #37927, #21919, #22176 ) ;
#48199 = ORIENTED_EDGE ( 'NONE', *, *, #3370, .F. ) ;
#48200 = CARTESIAN_POINT ( 'NONE',  ( 11.07421741897729284, 24.06268098812965306, -44.42833502052770456 ) ) ;
#48201 = AXIS2_PLACEMENT_3D ( 'NONE', #21979, #2086, #26172 ) ;
#48202 = CARTESIAN_POINT ( 'NONE',  ( 11.10547680587540142, -63.25111298948629468, -44.25103578592439391 ) ) ;
#48203 = EDGE_CURVE ( 'NONE', #24462, #37740, #8032, .T. ) ;
#48204 = CARTESIAN_POINT ( 'NONE',  ( 41.61626771661330082, 6.328436186825659782, -82.23834840541459812 ) ) ;
#48205 = EDGE_LOOP ( 'NONE', ( #48389, #8213, #19253, #25430 ) ) ;
#48206 = CARTESIAN_POINT ( 'NONE',  ( 71.33393739769650210, 1.396834109478129804, -70.23662692463440749 ) ) ;
#48207 = CARTESIAN_POINT ( 'NONE',  ( 50.21099649970649637, -49.38019754356140112, -76.14999999999999147 ) ) ;
#48208 = ADVANCED_FACE ( 'NONE', ( #33152 ), #13783, .T. ) ;
#48209 = CARTESIAN_POINT ( 'NONE',  ( 18.97410177224724137, -8.205170569095422195, -49.12422271383822903 ) ) ;
#48210 = ORIENTED_EDGE ( 'NONE', *, *, #48086, .T. ) ;
#48211 = EDGE_CURVE ( 'NONE', #45437, #24734, #4318, .T. ) ;
#48212 = LINE ( 'NONE', #15726, #11581 ) ;
#48213 = CARTESIAN_POINT ( 'NONE',  ( 18.09749211374579758, -32.57607267493840197, -34.95504743437649608 ) ) ;
#48214 = CARTESIAN_POINT ( 'NONE',  ( 85.38000601716228743, 17.38381105532069881, -60.34000486924599471 ) ) ;
#48215 = CARTESIAN_POINT ( 'NONE',  ( 54.87556897361960040, 20.83392887628360057, -54.55337246671039964 ) ) ;
#48216 = EDGE_CURVE ( 'NONE', #25427, #41238, #29738, .T. ) ;
#48217 = CARTESIAN_POINT ( 'NONE',  ( 18.29630866101669895, -7.659627465277500491, -75.37679910129210725 ) ) ;
#48218 = DIRECTION ( 'NONE',  ( 0.000000000000000000, 0.000000000000000000, -1.000000000000000000 ) ) ;
#48219 = CARTESIAN_POINT ( 'NONE',  ( 53.80998019303380175, 20.00543317080720129, -75.59559825915250997 ) ) ;
#48220 = APPLICATION_PROTOCOL_DEFINITION ( 'draft international standard', 'automotive_design', 1998, #3339 ) ;
#48221 = ORIENTED_EDGE ( 'NONE', *, *, #36658, .T. ) ;
#48222 = CARTESIAN_POINT ( 'NONE',  ( 17.61790714432060057, -8.315193971646580806, -69.79648614575899046 ) ) ;
#48223 = VECTOR ( 'NONE', #22816, 1000.000000000000114 ) ;
#48224 = EDGE_CURVE ( 'NONE', #32046, #26382, #1016, .T. ) ;
#48225 = CARTESIAN_POINT ( 'NONE',  ( 0.08961746015897878448, -8.352138177767987059, -34.70268271585497644 ) ) ;
#48226 = DIRECTION ( 'NONE',  ( 0.000000000000000000, 0.000000000000000000, 1.000000000000000000 ) ) ;
#48227 = AXIS2_PLACEMENT_3D ( 'NONE', #18853, #42466, #6301 ) ;
#48228 = CARTESIAN_POINT ( 'NONE',  ( 47.22777443111749562, 23.33595295215160093, -74.94663380581128820 ) ) ;
#48229 = CARTESIAN_POINT ( 'NONE',  ( 65.46029542295769943, -29.76883965895079953, -16.55376543218019947 ) ) ;
#48230 = EDGE_CURVE ( 'NONE', #47951, #20243, #5402, .T. ) ;
#48231 = CARTESIAN_POINT ( 'NONE',  ( 58.92073349695134965, -28.77068650667426652, -15.64999999999993463 ) ) ;
#48232 = CARTESIAN_POINT ( 'NONE',  ( 41.30532100959469943, -44.77888729448210370, -5.382426867826140438 ) ) ;
#48233 = CARTESIAN_POINT ( 'NONE',  ( 69.73393739769620936, 10.88381105532070059, -61.94999999999999574 ) ) ;
#48234 = AXIS2_PLACEMENT_3D ( 'NONE', #37539, #14216, #10025 ) ;
#48235 = CARTESIAN_POINT ( 'NONE',  ( 15.90134539241399736, -23.85807111248870171, -70.01664904841000237 ) ) ;
#48236 = CIRCLE ( 'NONE', #13902, 34.55616290057869833 ) ;
#48237 = CARTESIAN_POINT ( 'NONE',  ( 57.14052290629950193, -50.61618793416369755, -74.67958084187151258 ) ) ;
#48239 = CARTESIAN_POINT ( 'NONE',  ( 41.95231199169119662, -39.81623677285271867, -76.32572085277173812 ) ) ;
#48238 = SURFACE_SIDE_STYLE ('',( #8927 ) ) ;
#48240 = CARTESIAN_POINT ( 'NONE',  ( 63.14388432454488509, 1.191644800533210091, -68.79793125682789423 ) ) ;
#48241 = CARTESIAN_POINT ( 'NONE',  ( 61.28176046677850053, 14.00199778307229970, -46.64755189084589659 ) ) ;
#48242 = DIRECTION ( 'NONE',  ( 0.000000000000000000, 0.000000000000000000, -1.000000000000000000 ) ) ;
#48243 = ORIENTED_EDGE ( 'NONE', *, *, #2657, .T. ) ;
#48244 = CARTESIAN_POINT ( 'NONE',  ( 52.83236148840860125, -49.65955553127109567, -48.53481065559509489 ) ) ;
#48245 = EDGE_CURVE ( 'NONE', #25374, #6898, #30103, .T. ) ;
#48246 = CARTESIAN_POINT ( 'NONE',  ( 61.51111410063019491, -45.14410897695700697, -28.03257470884280167 ) ) ;
#48247 = PLANE ( 'NONE',  #9302 ) ;
#48248 = CARTESIAN_POINT ( 'NONE',  ( 56.81905678432669760, 14.35807671477110148, -26.04401432792739968 ) ) ;
#48249 = CARTESIAN_POINT ( 'NONE',  ( 18.08784342482760010, -8.426686525020091523, -75.81712490659408843 ) ) ;
#48250 = CARTESIAN_POINT ( 'NONE',  ( 50.84617524826920487, 17.60923104663729788, -76.31370213949210779 ) ) ;
#48251 = CARTESIAN_POINT ( 'NONE',  ( 52.94386159154990423, 18.37106777961130177, -48.82486937432109642 ) ) ;
#48252 = CARTESIAN_POINT ( 'NONE',  ( 71.24781132387310834, 1.101170701158060039, -70.72594205704909598 ) ) ;
#48253 = CARTESIAN_POINT ( 'NONE',  ( 41.50224532540739375, -43.90848951166570657, -3.489448901339209819 ) ) ;
#48254 = VECTOR ( 'NONE', #2742, 1000.000000000000114 ) ;
#48255 = ORIENTED_EDGE ( 'NONE', *, *, #18160, .F. ) ;
#48256 = DIRECTION ( 'NONE',  ( 0.000000000000000000, -1.000000000000000000, 0.000000000000000000 ) ) ;
#48257 = CARTESIAN_POINT ( 'NONE',  ( 47.61941804400159839, -54.52212999301320195, -54.78915954509680120 ) ) ;
#48258 = CARTESIAN_POINT ( 'NONE',  ( 20.57457857590170036, -10.13683997779680013, -68.56397102982089109 ) ) ;
#48259 = CARTESIAN_POINT ( 'NONE',  ( 14.36273137698815461, -22.20707289941944040, -71.03615485597320856 ) ) ;
#48260 = CARTESIAN_POINT ( 'NONE',  ( 58.90205675725459145, 16.74204408721319837, -50.17799186399640377 ) ) ;
#48261 = CARTESIAN_POINT ( 'NONE',  ( 71.40428550048659417, 1.263903724274369811, -60.80800729848100161 ) ) ;
#48262 = CARTESIAN_POINT ( 'NONE',  ( 46.70917532059600319, 7.904099119542530083, -34.65437117444129456 ) ) ;
#48263 = CARTESIAN_POINT ( 'NONE',  ( 71.86947670220010309, 0.9561296872641509292, -60.95384405884309587 ) ) ;
#48264 = VECTOR ( 'NONE', #11900, 1000.000000000000000 ) ;
#48265 = DIRECTION ( 'NONE',  ( 0.8445834565878902467, -0.5331027592246893043, -0.04980193736265902532 ) ) ;
#48266 = CARTESIAN_POINT ( 'NONE',  ( 64.90098062201279561, 0.9219904752505849732, -70.70458949289690054 ) ) ;
#48267 = ORIENTED_EDGE ( 'NONE', *, *, #7745, .F. ) ;
#48268 = VERTEX_POINT ( 'NONE', #45233 ) ;
#48269 = FACE_OUTER_BOUND ( 'NONE', #9017, .T. ) ;
#48270 = CARTESIAN_POINT ( 'NONE',  ( 9.367243689500000414, -15.61633989587210003, -59.45282021618999835 ) ) ;
#48271 = ORIENTED_EDGE ( 'NONE', *, *, #20614, .T. ) ;
#48272 = DIRECTION ( 'NONE',  ( -0.1961161351381831008, 1.073215590470984393E-15, -0.9805806756909204447 ) ) ;
#48273 = CARTESIAN_POINT ( 'NONE',  ( 11.83663281541470091, -65.04952182729299182, -45.42313283646279842 ) ) ;
#48274 = CARTESIAN_POINT ( 'NONE',  ( 51.13393739769659874, -45.11618894467899565, 11.34999999999999964 ) ) ;
#48275 = ORIENTED_EDGE ( 'NONE', *, *, #8398, .T. ) ;
#48276 = CARTESIAN_POINT ( 'NONE',  ( 68.13393739769620083, -43.11618894467930119, -73.25000000000000000 ) ) ;
#48277 = LINE ( 'NONE', #13175, #24254 ) ;
#48278 = CIRCLE ( 'NONE', #47467, 36.55167969755429880 ) ;
#48279 = CARTESIAN_POINT ( 'NONE',  ( 16.07824235657712109, -23.60611652474380762, -66.00953593440993927 ) ) ;
#48280 = EDGE_CURVE ( 'NONE', #38817, #36774, #50221, .T. ) ;
#48281 = CARTESIAN_POINT ( 'NONE',  ( 14.12315431978420044, -7.619972872716400225, -43.21391308946279963 ) ) ;
#48282 = CIRCLE ( 'NONE', #9793, 36.50000000000000711 ) ;
#48283 = CARTESIAN_POINT ( 'NONE',  ( 76.30797822825405774, 13.29802461769379818, -14.99128760117880432 ) ) ;
#48284 = CARTESIAN_POINT ( 'NONE',  ( 43.20303852803674971, -37.80742877201157626, -74.30445077681486055 ) ) ;
#48285 =( NAMED_UNIT ( * ) PLANE_ANGLE_UNIT ( ) SI_UNIT ( $, .RADIAN. ) );
#48286 = ORIENTED_EDGE ( 'NONE', *, *, #1027, .T. ) ;
#48287 = CARTESIAN_POINT ( 'NONE',  ( 11.99583947690149976, -64.75022670770579225, -24.44537524834330355 ) ) ;
#48288 = CARTESIAN_POINT ( 'NONE',  ( 11.28980945888330112, -9.441723080053581185, -81.30072504052380111 ) ) ;
#48289 = CARTESIAN_POINT ( 'NONE',  ( 41.81948262126999794, 14.32434734326079884, -6.527080060687969976 ) ) ;
#48290 = CARTESIAN_POINT ( 'NONE',  ( 13.93534818368129891, 20.80550406818660036, -75.55956264724760274 ) ) ;
#48291 = CARTESIAN_POINT ( 'NONE',  ( 24.04181170281000135, -15.85636501970542867, -59.80198823605401515 ) ) ;
#48292 = CARTESIAN_POINT ( 'NONE',  ( 82.81259997840240317, -45.03397381929850241, -46.56543266184489482 ) ) ;
#48293 = AXIS2_PLACEMENT_3D ( 'NONE', #37282, #24678, #40691 ) ;
#48294 = CARTESIAN_POINT ( 'NONE',  ( 11.35626934711086911, 34.06258129802085222, -17.73521848465946249 ) ) ;
#48295 = CARTESIAN_POINT ( 'NONE',  ( 24.37435181540019613, -15.89599411523789918, -47.51847262634210267 ) ) ;
#48296 = VERTEX_POINT ( 'NONE', #943 ) ;
#48297 = CARTESIAN_POINT ( 'NONE',  ( 52.81005256294240269, -49.67124369057780342, -28.09291909505480334 ) ) ;
#48298 = CARTESIAN_POINT ( 'NONE',  ( 13.79543417967100005, -50.43786691665530242, -21.08562091374989933 ) ) ;
#48299 = DIRECTION ( 'NONE',  ( 0.000000000000000000, 0.000000000000000000, -1.000000000000000000 ) ) ;
#48300 = CARTESIAN_POINT ( 'NONE',  ( 19.54188187493409146, -21.52912850391220090, -56.78610451874590836 ) ) ;
#48301 = CYLINDRICAL_SURFACE ( 'NONE', #17293, 1.999999999999996669 ) ;
#48302 = ORIENTED_EDGE ( 'NONE', *, *, #36134, .F. ) ;
#48303 = CARTESIAN_POINT ( 'NONE',  ( -3.519180701196159777, -48.70869051177000131, -5.604219821670230139 ) ) ;
#48304 = CARTESIAN_POINT ( 'NONE',  ( 47.40246354955809949, 23.42001344289909781, -54.74579969459569639 ) ) ;
#48305 = AXIS2_PLACEMENT_3D ( 'NONE', #7535, #39244, #10954 ) ;
#48306 = EDGE_CURVE ( 'NONE', #32526, #41688, #41549, .T. ) ;
#48307 = CARTESIAN_POINT ( 'NONE',  ( 15.63241099694714542, 18.38381172634125704, -83.24416995785023232 ) ) ;
#48308 = CARTESIAN_POINT ( 'NONE',  ( 63.07039345372018602, 1.099973129953850215, -62.51484271732719833 ) ) ;
#48309 = CARTESIAN_POINT ( 'NONE',  ( 18.13393739769620083, -41.61618894467939356, -35.01561944896766221 ) ) ;
#48310 = CARTESIAN_POINT ( 'NONE',  ( 41.06416708622129619, 13.46295351750030100, -5.123099498004559216 ) ) ;
#48311 = DIRECTION ( 'NONE',  ( 0.000000000000000000, 0.000000000000000000, -1.000000000000000000 ) ) ;
#48312 = CARTESIAN_POINT ( 'NONE',  ( 9.807807174049782972, -10.75446600372985628, -61.00066419533776241 ) ) ;
#48313 = DIRECTION ( 'NONE',  ( 0.000000000000000000, -1.000000000000000000, 0.000000000000000000 ) ) ;
#48314 = CARTESIAN_POINT ( 'NONE',  ( 55.64908854110159808, -48.32622745761450034, -48.64133301306080170 ) ) ;
#48315 = CARTESIAN_POINT ( 'NONE',  ( -0.2246626217552654958, -20.50318462115538765, -34.96184000430482541 ) ) ;
#48316 = EDGE_CURVE ( 'NONE', #16787, #9287, #18412, .T. ) ;
#48317 = CARTESIAN_POINT ( 'NONE',  ( 64.74203006853200293, 1.187931651339009909, -60.80292108597650014 ) ) ;
#48318 = CARTESIAN_POINT ( 'NONE',  ( 17.59215364258619729, -52.29221104373319662, -75.97756937697440094 ) ) ;
#48319 = EDGE_CURVE ( 'NONE', #49834, #43383, #6192, .T. ) ;
#48320 = CARTESIAN_POINT ( 'NONE',  ( 68.13393739769620083, 1.383811055320669947, -65.65000000000000568 ) ) ;
#48321 = CYLINDRICAL_SURFACE ( 'NONE', #10723, 5.499999999999998224 ) ;
#48322 = ORIENTED_EDGE ( 'NONE', *, *, #13025, .F. ) ;
#48323 = CARTESIAN_POINT ( 'NONE',  ( -0.3016046179078940015, -10.91500322974829906, -35.02873218748179340 ) ) ;
#48324 = CARTESIAN_POINT ( 'NONE',  ( 9.273487956746869543, 31.88305279702909800, -46.53410025525219851 ) ) ;
#48325 = CARTESIAN_POINT ( 'NONE',  ( 51.63351621991599671, -50.61618894467930119, -66.86356675664690385 ) ) ;
#48326 = CARTESIAN_POINT ( 'NONE',  ( 9.667674752789849890, -11.97066205877570155, -81.23899999999999011 ) ) ;
#48327 = ORIENTED_EDGE ( 'NONE', *, *, #11436, .F. ) ;
#48328 = CARTESIAN_POINT ( 'NONE',  ( 18.74040570297340125, 20.57970132932399920, -74.87640169473949925 ) ) ;
#48329 = EDGE_LOOP ( 'NONE', ( #46617, #16561, #8124, #16473, #7289 ) ) ;
#48330 = ORIENTED_EDGE ( 'NONE', *, *, #13223, .F. ) ;
#48331 = ORIENTED_EDGE ( 'NONE', *, *, #23034, .T. ) ;
#48332 = DIRECTION ( 'NONE',  ( -0.1999849291396485207, 0.9797989733190221040, 0.000000000000000000 ) ) ;
#48333 = CARTESIAN_POINT ( 'NONE',  ( 20.99657455844219811, -20.65612899709289962, -81.23899999999999011 ) ) ;
#48334 = CYLINDRICAL_SURFACE ( 'NONE', #35670, 0.4999999999999990008 ) ;
#48335 = DIRECTION ( 'NONE',  ( -1.000000000000000000, 0.000000000000000000, 0.000000000000000000 ) ) ;
#48336 = ORIENTED_EDGE ( 'NONE', *, *, #40504, .F. ) ;
#48337 = CARTESIAN_POINT ( 'NONE',  ( 9.366504787982940172, -15.61629640169840094, -69.84717978381009118 ) ) ;
#48338 = B_SPLINE_SURFACE_WITH_KNOTS ( 'NONE', 3, 3, ( 
 ( #22461, #33490, #41885, #26135, #33741, #2048, #42146, #5984, #29301, #13593, #45302, #33994, #25360, #5477, #50009, #3606, #27176, #47626, #26649, #35567, #31609, #51039 ),
 ( #42668, #19577, #27432, #30838, #34521, #43435, #46869, #7538, #3091, #3346, #2834, #31096, #23744, #23483, #18799, #35033, #38996, #51554, #39506, #31351, #42926, #26920 ),
 ( #47126, #6768, #15653, #11731, #27693, #10956, #43691, #47376, #7024, #11213, #7793, #7276, #15397, #23229, #22976, #2572, #19322, #18544, #50526, #43183, #50785, #22720 ),
 ( #38738, #51301, #14875, #14617, #19060, #15140, #30587, #39246, #35303, #11475, #34778, #46607, #10694, #1147, #9543, #1670, #5611, #16607, #9798, #32829, #17397, #17658 ),
 ( #37051, #33365, #9020, #21308, #25234, #48596, #33624, #45698, #41241, #5354, #1410, #48855, #45176, #21048, #13732, #49641, #5094, #37310, #17144, #41497, #24964, #888 ),
 ( #12961, #40982, #49382, #21566, #32565, #33095, #13478, #36520, #29435, #12696, #28650, #49126, #44652, #4820, #45441, #39758, #8759, #24707, #4556, #40725, #9288, #25495 ),
 ( #20788, #624, #28913, #36780, #37561, #16883, #29688, #13225, #29174, #20525, #44918, #6637, #18167, #6125, #41756, #1928, #38348, #46748, #38875, #42808, #17910, #47007 ),
 ( #46487, #10316, #10577, #34918, #10052, #34654, #45958, #26014, #26277, #26533, #42547, #14495, #22601, #18937, #22854, #33879, #29944, #2438, #22081, #49892, #5862, #13987 ),
 ( #26796, #34133, #38091, #50916, #25748, #42025, #42284, #2187, #37834, #2963, #38616, #2706, #18681, #15010, #50142, #34396, #50661, #6381, #14755, #30725, #30211, #30980 ),
 ( #14241, #46227, #22342, #18421, #50408, #10830, #30467, #15533, #4760, #13416, #32767, #48792, #5550, #12901, #29118, #40661, #28592, #12368, #24388, #8963, #17341, #9484 ) ),
 .UNSPECIFIED., .F., .F., .F.,
 ( 4, 1, 1, 1, 1, 1, 1, 4 ),
 ( 4, 2, 2, 2, 2, 2, 2, 2, 2, 2, 4 ),
 ( -2.340994999999999938E-10, 0.1428571428571430157, 0.2857142857142860315, 0.4285714285714289917, 0.5714285714285709528, 0.7142857142857139685, 0.8571428571428569843, 1.000000707733940120 ),
 ( -8.605215962919450234, -8.065295817754250862, -6.871057666229980043, -6.124658821527319219, -5.378259976824650401, -4.302607981459720676, -3.764781983777250041, -2.904260387485310346, -2.013455357812269586, -0.8451718638598000322, 7.077339579999999566E-07 ),
 .UNSPECIFIED. ) ;
#48339 = ADVANCED_FACE ( 'NONE', ( #21103 ), #5666, .F. ) ;
#48340 = PLANE ( 'NONE',  #14044 ) ;
#48341 = VERTEX_POINT ( 'NONE', #37889 ) ;
#48342 = CARTESIAN_POINT ( 'NONE',  ( 9.367812230547961860, -14.91300876115404606, -41.88025658668828299 ) ) ;
#48343 = CARTESIAN_POINT ( 'NONE',  ( 16.13393739769620083, -15.61618894467929941, -18.58999999999999986 ) ) ;
#48344 = ORIENTED_EDGE ( 'NONE', *, *, #1727, .F. ) ;
#48345 = VERTEX_POINT ( 'NONE', #22136 ) ;
#48346 = CARTESIAN_POINT ( 'NONE',  ( 61.75019796695539753, -46.11618894467930119, -28.15000000000000213 ) ) ;
#48347 = DIRECTION ( 'NONE',  ( -1.000000000000000000, 0.000000000000000000, 0.000000000000000000 ) ) ;
#48348 = CARTESIAN_POINT ( 'NONE',  ( 61.24574273693410476, 14.30988654607880051, -47.60649862612909544 ) ) ;
#48349 = TOROIDAL_SURFACE ( 'NONE', #4014, 36.00000000000000000, 2.000000000000000000 ) ;
#48350 = CARTESIAN_POINT ( 'NONE',  ( 52.57642278611140085, 14.37083706895390023, -13.82862052991180057 ) ) ;
#48351 = AXIS2_PLACEMENT_3D ( 'NONE', #6360, #18659, #37813 ) ;
#48352 = CARTESIAN_POINT ( 'NONE',  ( 12.14984841769559765, -22.52873612623772104, -68.45899737382208627 ) ) ;
#48353 = CARTESIAN_POINT ( 'NONE',  ( -7.078137695061969659, 14.49478530863819969, -5.101446175793999949 ) ) ;
#48354 = DIRECTION ( 'NONE',  ( -0.1961161351381840445, -2.837236618486509954E-16, -0.9805806756909201116 ) ) ;
#48355 = CARTESIAN_POINT ( 'NONE',  ( 61.30494512497919857, 13.98627961912009887, -28.05574256500980113 ) ) ;
#48356 = CARTESIAN_POINT ( 'NONE',  ( 23.69882969085709945, -13.52833052609389952, -65.20178814406908430 ) ) ;
#48357 = VERTEX_POINT ( 'NONE', #6437 ) ;
#48358 = CARTESIAN_POINT ( 'NONE',  ( 54.27527969986719114, 17.69567147495890325, -48.75594442643640036 ) ) ;
#48359 = CARTESIAN_POINT ( 'NONE',  ( 23.52343111712058032, -48.95118247924429511, -34.77532226276708371 ) ) ;
#48360 = CARTESIAN_POINT ( 'NONE',  ( 11.19262701750870015, 32.79550126274290278, -44.18375550860420020 ) ) ;
#48361 = CARTESIAN_POINT ( 'NONE',  ( 72.36591324851900708, 1.277721627657099956, -69.81671480277449859 ) ) ;
#48362 = CARTESIAN_POINT ( 'NONE',  ( 43.68052723063104281, -39.92785622281377300, -68.20639724664832215 ) ) ;
#48363 = CARTESIAN_POINT ( 'NONE',  ( 9.807791109152047326, -20.47789127149569310, -36.58399760381443144 ) ) ;
#48364 = CARTESIAN_POINT ( 'NONE',  ( 47.20319459038839227, 23.55908258955629719, -74.14999581977149035 ) ) ;
#48365 = CARTESIAN_POINT ( 'NONE',  ( 48.63379746627050082, -53.98620851929000253, -54.63257371341549629 ) ) ;
#48366 = CARTESIAN_POINT ( 'NONE',  ( 16.13393739769620083, -45.61618894467940066, -34.64999999999999858 ) ) ;
#48367 = EDGE_CURVE ( 'NONE', #18539, #3226, #6178, .T. ) ;
#48368 = CARTESIAN_POINT ( 'NONE',  ( 64.39815381769149383, 0.9561815866734399982, -70.34594416269000305 ) ) ;
#48369 = CARTESIAN_POINT ( 'NONE',  ( 24.04493739769619864, -15.61618894467929941, -32.14999999999999858 ) ) ;
#48370 = DIRECTION ( 'NONE',  ( 0.000000000000000000, 0.000000000000000000, -1.000000000000000000 ) ) ;
#48371 = EDGE_CURVE ( 'NONE', #8235, #39828, #42339, .T. ) ;
#48372 = ORIENTED_EDGE ( 'NONE', *, *, #51653, .F. ) ;
#48373 = CARTESIAN_POINT ( 'NONE',  ( 23.14732642514769978, -18.12996472783180124, -45.17689247551339804 ) ) ;
#48374 = CARTESIAN_POINT ( 'NONE',  ( 22.04684393501796080, -19.02418972032391764, -76.61949155326421135 ) ) ;
#48375 = ORIENTED_EDGE ( 'NONE', *, *, #40678, .F. ) ;
#48376 = DIRECTION ( 'NONE',  ( 0.000000000000000000, 1.000000000000000000, 0.000000000000000000 ) ) ;
#48377 = CARTESIAN_POINT ( 'NONE',  ( 60.35316404808119728, -45.72939249500469572, -47.36338488644539524 ) ) ;
#48378 = CARTESIAN_POINT ( 'NONE',  ( 23.34813653593170102, 18.05571844226370004, -34.65024031912469837 ) ) ;
#48379 = AXIS2_PLACEMENT_3D ( 'NONE', #20688, #16780, #6285 ) ;
#48380 = CARTESIAN_POINT ( 'NONE',  ( 75.47966807050509885, -43.37310274687460065, -13.40512917118210012 ) ) ;
#48382 = CARTESIAN_POINT ( 'NONE',  ( 0.2019507440921957664, -22.94509536330835786, -34.66067286864802099 ) ) ;
#48381 = CARTESIAN_POINT ( 'NONE',  ( 41.49123592270440497, 8.475614001362112404, -78.78653678967756946 ) ) ;
#48383 = CARTESIAN_POINT ( 'NONE',  ( 31.39802437502155286, 4.622311496553142440, -84.65000000000000568 ) ) ;
#48384 = CARTESIAN_POINT ( 'NONE',  ( 37.88393739769619373, -42.11618894467939356, -35.14999999999999858 ) ) ;
#48385 = ORIENTED_EDGE ( 'NONE', *, *, #19676, .F. ) ;
#48386 = CARTESIAN_POINT ( 'NONE',  ( 83.98295738300248559, -44.57976106941110572, -47.35112499062080360 ) ) ;
#48387 = ORIENTED_EDGE ( 'NONE', *, *, #29261, .T. ) ;
#48388 = ORIENTED_EDGE ( 'NONE', *, *, #31521, .F. ) ;
#48389 = ORIENTED_EDGE ( 'NONE', *, *, #1110, .T. ) ;
#48390 = PLANE ( 'NONE',  #40361 ) ;
#48391 = CARTESIAN_POINT ( 'NONE',  ( 11.27229735085614593, -9.289995009674603565, -79.08399885391317241 ) ) ;
#48392 = CARTESIAN_POINT ( 'NONE',  ( 76.39982225080902367, -19.43572751922974362, -12.79577862347393058 ) ) ;
#48393 = CARTESIAN_POINT ( 'NONE',  ( 54.02518786316219490, -51.81565143108780092, -54.18996768095620098 ) ) ;
#48394 = ORIENTED_EDGE ( 'NONE', *, *, #48306, .F. ) ;
#48395 = ORIENTED_EDGE ( 'NONE', *, *, #5169, .F. ) ;
#48396 = EDGE_CURVE ( 'NONE', #18232, #36393, #16776, .T. ) ;
#48397 = DIRECTION ( 'NONE',  ( 0.000000000000000000, 0.000000000000000000, -1.000000000000000000 ) ) ;
#48398 = CARTESIAN_POINT ( 'NONE',  ( 10.03393739769619941, -15.61618894467929941, 14.34999999999999964 ) ) ;
#48399 = CARTESIAN_POINT ( 'NONE',  ( 13.13393739769600010, 18.38381105532060289, -83.01107220193038927 ) ) ;
#48400 = DIRECTION ( 'NONE',  ( -0.6911981449639439390, -0.7226652920947588266, 0.000000000000000000 ) ) ;
#48401 = EDGE_CURVE ( 'NONE', #46428, #51503, #15912, .T. ) ;
#48402 = CARTESIAN_POINT ( 'NONE',  ( 64.56306260708079492, 0.8160381106275480523, -17.55137208659099812 ) ) ;
#48403 = CARTESIAN_POINT ( 'NONE',  ( 51.95832570932330441, -49.45171451879549807, -77.09974002837380169 ) ) ;
#48404 = ORIENTED_EDGE ( 'NONE', *, *, #18180, .T. ) ;
#48405 = CARTESIAN_POINT ( 'NONE',  ( 3.754239621849577713, 24.69916076480114242, -9.121771190811498897 ) ) ;
#48406 = CARTESIAN_POINT ( 'NONE',  ( 54.14345801646960155, -50.61618316771350834, -76.93443301864958528 ) ) ;
#48407 = CARTESIAN_POINT ( 'NONE',  ( 60.23362534523688794, 14.54944813804885229, -47.26357634580340061 ) ) ;
#48408 = DIRECTION ( 'NONE',  ( -0.8732394366197178126, 0.4872913772396119114, 0.000000000000000000 ) ) ;
#48409 = CARTESIAN_POINT ( 'NONE',  ( 10.93745414090779988, -21.49694649396669988, -56.74285641080179943 ) ) ;
#48410 = CARTESIAN_POINT ( 'NONE',  ( -18.86606260230360022, -50.61618894467959962, 17.35000000000000142 ) ) ;
#48411 = B_SPLINE_CURVE_WITH_KNOTS ( 'NONE', 3,
 ( #26248, #46460, #26504, #7385, #38588, #42520, #38320, #23334, #42255, #18390 ),
 .UNSPECIFIED., .F., .F.,
 ( 4, 2, 2, 2, 4 ),
 ( 0.5000000023607420463, 0.6250000017705563682, 0.7500000011803709121, 0.8750000005901854561, 1.000000000000000000 ),
 .UNSPECIFIED. ) ;
#48412 = CARTESIAN_POINT ( 'NONE',  ( 42.42327894872600069, -43.80073867009950561, -4.706996717213810300 ) ) ;
#48413 = CARTESIAN_POINT ( 'NONE',  ( 68.13393739771727553, -29.66618894467940137, -81.65000000000000568 ) ) ;
#48414 = CARTESIAN_POINT ( 'NONE',  ( 60.83133137330749918, -45.46867109277970087, -47.01992810568810199 ) ) ;
#48415 = CARTESIAN_POINT ( 'NONE',  ( 68.36163520449862574, -0.4430167382633080631, -18.19591820036098895 ) ) ;
#48416 = CARTESIAN_POINT ( 'NONE',  ( -0.1295185695944109927, -31.87964491196989414, -59.64999999999999147 ) ) ;
#48417 = AXIS2_PLACEMENT_3D ( 'NONE', #8308, #24521, #24265 ) ;
#48418 = CARTESIAN_POINT ( 'NONE',  ( 13.90590011285059902, -8.924521810714191261, -52.24487123071539685 ) ) ;
#48419 = CARTESIAN_POINT ( 'NONE',  ( 17.21347160910390173, -53.11618894467930119, -76.14999999999999147 ) ) ;
#48420 = AXIS2_PLACEMENT_3D ( 'NONE', #34847, #11017, #43502 ) ;
#48421 = ORIENTED_EDGE ( 'NONE', *, *, #14892, .F. ) ;
#48422 = CARTESIAN_POINT ( 'NONE',  ( 14.24028704233020015, -52.17195122215589720, -75.81086730487160708 ) ) ;
#48424 = VECTOR ( 'NONE', #22322, 999.9999999999998863 ) ;
#48423 = CARTESIAN_POINT ( 'NONE',  ( 47.31562538347599656, -54.71039600610800591, -54.74027837518219997 ) ) ;
#48425 = CARTESIAN_POINT ( 'NONE',  ( 16.13393739769620083, -15.61618894467929941, -11.65000000000000036 ) ) ;
#48426 = CARTESIAN_POINT ( 'NONE',  ( 23.04646185301237438, -11.63205982887159173, -37.34100430183969621 ) ) ;
#48427 = CARTESIAN_POINT ( 'NONE',  ( 56.84932592767840021, 19.42421310868259354, -63.99406948319570887 ) ) ;
#48428 = CARTESIAN_POINT ( 'NONE',  ( 60.83844611352238019, -45.46494382793184741, -47.03527794730813127 ) ) ;
#48429 = CARTESIAN_POINT ( 'NONE',  ( 11.89321892219109955, 34.20364954172590188, -18.16392793332829925 ) ) ;
#48430 = B_SPLINE_CURVE_WITH_KNOTS ( 'NONE', 3,
 ( #37896, #33936, #1988, #33160, #33682, #41557, #1470, #41300 ),
 .UNSPECIFIED., .F., .F.,
 ( 4, 2, 2, 4 ),
 ( 0.000000000000000000, 0.3677848396155383170, 0.7599019565052781422, 1.000000000000000000 ),
 .UNSPECIFIED. ) ;
#48432 = CARTESIAN_POINT ( 'NONE',  ( -2.927979189508790103, -49.19984425798019601, -5.740620115512199639 ) ) ;
#48431 = LINE ( 'NONE', #16712, #4719 ) ;
#48433 = EDGE_CURVE ( 'NONE', #29027, #3978, #35168, .T. ) ;
#48434 = CARTESIAN_POINT ( 'NONE',  ( 15.05440318628160057, -53.11618894467930119, -76.14999999999999147 ) ) ;
#48435 = DIRECTION ( 'NONE',  ( 0.000000000000000000, -1.377023495004005809E-11, -1.000000000000000000 ) ) ;
#48436 = CARTESIAN_POINT ( 'NONE',  ( 48.84657211724849901, 22.78726586394800080, -55.19002503342879606 ) ) ;
#48437 = ORIENTED_EDGE ( 'NONE', *, *, #42229, .T. ) ;
#48438 = CARTESIAN_POINT ( 'NONE',  ( 52.73507376017240489, -49.73068395995180424, -48.76329240581910085 ) ) ;
#48439 = VERTEX_POINT ( 'NONE', #17960 ) ;
#48440 = CARTESIAN_POINT ( 'NONE',  ( 2.470463535281291367, -5.638681249711038568, -34.75586992539663811 ) ) ;
#48441 = DIRECTION ( 'NONE',  ( 0.000000000000000000, 0.000000000000000000, -1.000000000000000000 ) ) ;
#48442 = FACE_OUTER_BOUND ( 'NONE', #5083, .T. ) ;
#48444 = CARTESIAN_POINT ( 'NONE',  ( 52.72675226946439864, 18.45992442769729891, -27.59442653021299918 ) ) ;
#48443 = CARTESIAN_POINT ( 'NONE',  ( 83.96875769672529088, 13.10122437207289892, -47.04741150093960300 ) ) ;
#48445 = CARTESIAN_POINT ( 'NONE',  ( 22.12488360164890011, -19.33789853544120163, -64.62976173608399222 ) ) ;
#48446 = CARTESIAN_POINT ( 'NONE',  ( 52.88663098474060575, 18.43548364359019942, -48.99336406855329784 ) ) ;
#48447 = CARTESIAN_POINT ( 'NONE',  ( 55.17415142466310130, -45.32842442549269890, -15.17933028536879903 ) ) ;
#48448 = DIRECTION ( 'NONE',  ( -0.8224686640529101922, -0.3976080002595576146, -0.4067593573362719428 ) ) ;
#48449 = ORIENTED_EDGE ( 'NONE', *, *, #38834, .F. ) ;
#48450 = VERTEX_POINT ( 'NONE', #38402 ) ;
#48451 = CARTESIAN_POINT ( 'NONE',  ( 11.62518889158189950, -65.06178593564310120, -16.65848135031670196 ) ) ;
#48452 = CARTESIAN_POINT ( 'NONE',  ( 9.904144631292190581, 32.27789939431119848, -46.22502649936210162 ) ) ;
#48453 = CARTESIAN_POINT ( 'NONE',  ( 18.69872345376407807, 20.24981416582376070, -15.74255600669635236 ) ) ;
#48454 = CARTESIAN_POINT ( 'NONE',  ( 47.21685942418269377, -54.78066203677720125, -54.66846264793990429 ) ) ;
#48455 = CARTESIAN_POINT ( 'NONE',  ( 11.28041403274951548, -65.17108450666793829, -22.88566713088593119 ) ) ;
#48456 = DIRECTION ( 'NONE',  ( 1.000000000000000000, 0.000000000000000000, 0.000000000000000000 ) ) ;
#48457 = AXIS2_PLACEMENT_3D ( 'NONE', #20805, #5112, #24463 ) ;
#48458 = AXIS2_PLACEMENT_3D ( 'NONE', #50447, #14534, #26571 ) ;
#48459 = VECTOR ( 'NONE', #9152, 1000.000000000000000 ) ;
#48460 = ORIENTED_EDGE ( 'NONE', *, *, #11428, .T. ) ;
#48461 = CARTESIAN_POINT ( 'NONE',  ( 29.63393739769620083, -15.61618894467929941, -11.11999999999999922 ) ) ;
#48462 = CARTESIAN_POINT ( 'NONE',  ( 10.97797866599409922, -63.15395481739809469, -44.74230776638400187 ) ) ;
#48463 = CARTESIAN_POINT ( 'NONE',  ( 40.00893739769619373, -16.26570799751769769, -35.14999999999999858 ) ) ;
#48464 = EDGE_CURVE ( 'NONE', #33306, #5521, #50969, .T. ) ;
#48465 = LINE ( 'NONE', #25103, #13303 ) ;
#48466 = CARTESIAN_POINT ( 'NONE',  ( 63.46757340380580814, 1.384887413063070172, -62.68544474927200127 ) ) ;
#48467 = CARTESIAN_POINT ( 'NONE',  ( 22.46010119316818887, -20.47786885658587153, -43.71601729080407495 ) ) ;
#48468 =( BOUNDED_CURVE ( )  B_SPLINE_CURVE ( 3, ( #1673, #21831, #7416, #3225 ),
 .UNSPECIFIED., .F., .T. ) 
 B_SPLINE_CURVE_WITH_KNOTS ( ( 4, 4 ),
 ( 5.070260775219133542, 5.428132570053642247 ),
 .UNSPECIFIED. ) 
 CURVE ( )  GEOMETRIC_REPRESENTATION_ITEM ( )  RATIONAL_B_SPLINE_CURVE ( ( 1.000000000000000000, 0.9893557610490317789, 0.9893557610490317789, 1.000000000000000000 ) ) 
 REPRESENTATION_ITEM ( '' )  );
#48469 = ORIENTED_EDGE ( 'NONE', *, *, #1942, .F. ) ;
#48470 = CARTESIAN_POINT ( 'NONE',  ( 9.366958635467167227, -14.73023523842327265, -67.49448678272128177 ) ) ;
#48471 = DIRECTION ( 'NONE',  ( 0.8090169943749525583, 0.5877852522924661427, 0.000000000000000000 ) ) ;
#48472 = CARTESIAN_POINT ( 'NONE',  ( 56.39270784227079503, -50.52750194671250483, -52.86271187454359932 ) ) ;
#48473 = CARTESIAN_POINT ( 'NONE',  ( 53.24328890024050054, 22.35687538065929658, -56.22661043126620228 ) ) ;
#48474 = CARTESIAN_POINT ( 'NONE',  ( 9.585777066488809339, -10.60576817065870081, -73.00023116938359635 ) ) ;
#48475 = DIRECTION ( 'NONE',  ( 0.000000000000000000, 0.000000000000000000, 1.000000000000000000 ) ) ;
#48476 = PLANE ( 'NONE',  #12492 ) ;
#48477 = APPLICATION_PROTOCOL_DEFINITION ( 'draft international standard', 'automotive_design', 1998, #6017 ) ;
#48478 = CARTESIAN_POINT ( 'NONE',  ( 46.59688917077139791, -53.29855585819780117, -76.10130133987269119 ) ) ;
#48479 = ORIENTED_EDGE ( 'NONE', *, *, #17789, .F. ) ;
#48480 = CARTESIAN_POINT ( 'NONE',  ( 15.36594091644890092, -23.02678104045260099, -60.76552800450640035 ) ) ;
#48481 = DIRECTION ( 'NONE',  ( -0.5000000000000003331, -0.8660254037844384856, 0.000000000000000000 ) ) ;
#48482 = CARTESIAN_POINT ( 'NONE',  ( 13.00893796619580023, 34.28605843179359880, -23.32157451048000141 ) ) ;
#48483 = CARTESIAN_POINT ( 'NONE',  ( 47.36067941193029895, 23.15755082926289887, -75.11690455987650239 ) ) ;
#48484 = CARTESIAN_POINT ( 'NONE',  ( 19.55308497633217968, -53.75077074604085681, -16.86504912222391184 ) ) ;
#48485 = PRODUCT_DEFINITION ( 'UNKNOWN', '', #13492, #16384 ) ;
#48486 = CARTESIAN_POINT ( 'NONE',  ( 10.47385409520754784, -55.21366976880749888, -45.62050209441289894 ) ) ;
#48487 = CARTESIAN_POINT ( 'NONE',  ( 0.1457841021255935343, -15.61618894467929941, -34.68167779225149161 ) ) ;
#48488 = AXIS2_PLACEMENT_3D ( 'NONE', #24986, #29193, #48618 ) ;
#48489 = CARTESIAN_POINT ( 'NONE',  ( 15.26510710965380113, -49.61613877435842568, -83.22678919103138639 ) ) ;
#48490 = LINE ( 'NONE', #41657, #975 ) ;
#48492 = CYLINDRICAL_SURFACE ( 'NONE', #38174, 6.766999999999998572 ) ;
#48491 = LINE ( 'NONE', #28817, #14006 ) ;
#48493 = EDGE_CURVE ( 'NONE', #26115, #19986, #10108, .T. ) ;
#48494 = CARTESIAN_POINT ( 'NONE',  ( 63.39699138880700247, 1.369885150286779929, -68.72489565442110404 ) ) ;
#48495 = CARTESIAN_POINT ( 'NONE',  ( 61.32101085468809742, 13.98954918084040067, -46.71870344728709767 ) ) ;
#48496 = CARTESIAN_POINT ( 'NONE',  ( -26.59371227466860077, -41.52207930017120674, -54.97277084359720334 ) ) ;
#48497 = EDGE_CURVE ( 'NONE', #45497, #14613, #42379, .T. ) ;
#48498 = VERTEX_POINT ( 'NONE', #13725 ) ;
#48499 = CARTESIAN_POINT ( 'NONE',  ( 52.83531802359640039, -49.65800651964969603, -48.55820785177999710 ) ) ;
#48500 = ADVANCED_FACE ( 'NONE', ( #41490 ), #12953, .T. ) ;
#48501 = CARTESIAN_POINT ( 'NONE',  ( 61.72368837927260188, -45.11618267598419862, -28.01092661157059993 ) ) ;
#48502 = CARTESIAN_POINT ( 'NONE',  ( 24.04493741894995296, -16.65173984875949031, -71.83400671401952309 ) ) ;
#48503 = CARTESIAN_POINT ( 'NONE',  ( 56.38589515732069657, 14.45185451966650092, -25.89150152932120363 ) ) ;
#48504 = CARTESIAN_POINT ( 'NONE',  ( 11.53513604979039897, -9.754423462944890488, -81.52088794317478460 ) ) ;
#48505 = ADVANCED_FACE ( 'NONE', ( #5087 ), #27603, .T. ) ;
#48506 = CARTESIAN_POINT ( 'NONE',  ( 50.76151235490149816, 18.34449058292550205, -76.22310723605730232 ) ) ;
#48507 = CARTESIAN_POINT ( 'NONE',  ( 52.80018040210159569, 18.44894719811759742, -48.71454912288499628 ) ) ;
#48508 = CARTESIAN_POINT ( 'NONE',  ( 71.37757697660960332, 1.096291039689149871, -70.64841943982850125 ) ) ;
#48509 = FACE_OUTER_BOUND ( 'NONE', #30173, .T. ) ;
#48510 = FACE_OUTER_BOUND ( 'NONE', #5156, .T. ) ;
#48511 = ORIENTED_EDGE ( 'NONE', *, *, #36959, .F. ) ;
#48512 = CARTESIAN_POINT ( 'NONE',  ( 54.47259832750690123, -46.25232753665150653, -15.76422791930239953 ) ) ;
#48513 = CARTESIAN_POINT ( 'NONE',  ( 47.59376055414519868, -54.54431305457409707, -54.85521038714039577 ) ) ;
#48514 = CARTESIAN_POINT ( 'NONE',  ( -4.848012345405839696, 16.07167109151949802, -4.416243737290190374 ) ) ;
#48515 = CARTESIAN_POINT ( 'NONE',  ( 41.83063930790589779, 12.37849180622510126, -3.362295849109719903 ) ) ;
#48516 = CARTESIAN_POINT ( 'NONE',  ( 60.41972385647800081, 15.56736444559500043, -48.98660369848109752 ) ) ;
#48517 = CARTESIAN_POINT ( 'NONE',  ( 71.44853510719140388, 1.186515949276290227, -60.75583815301620660 ) ) ;
#48518 = DIRECTION ( 'NONE',  ( -0.7071067811865475727, 0.000000000000000000, 0.7071067811865475727 ) ) ;
#48519 = CARTESIAN_POINT ( 'NONE',  ( 71.68799458498580179, 0.9577391936072879863, -60.81570214284359821 ) ) ;
#48520 = CARTESIAN_POINT ( 'NONE',  ( 18.20454996519679725, -23.32130808853898074, -71.92427505145974465 ) ) ;
#48521 = CARTESIAN_POINT ( 'NONE',  ( 64.89987712417480736, 0.8859637708054489691, -70.70388507757908769 ) ) ;
#48522 = ORIENTED_EDGE ( 'NONE', *, *, #20200, .T. ) ;
#48523 = ORIENTED_EDGE ( 'NONE', *, *, #27723, .T. ) ;
#48524 = CARTESIAN_POINT ( 'NONE',  ( 71.83406239765474766, 11.38381103969560471, -61.94987500004191361 ) ) ;
#48525 = CARTESIAN_POINT ( 'NONE',  ( 16.00829429484023692, -51.00984973828658298, -15.66512534869403694 ) ) ;
#48526 = ORIENTED_EDGE ( 'NONE', *, *, #22325, .T. ) ;
#48527 = EDGE_CURVE ( 'NONE', #33944, #12367, #12690, .T. ) ;
#48528 = DIRECTION ( 'NONE',  ( 0.000000000000000000, 0.000000000000000000, -1.000000000000000000 ) ) ;
#48529 = CARTESIAN_POINT ( 'NONE',  ( 55.89446496821490484, -45.93182254271150100, -25.32793047687500021 ) ) ;
#48530 = DIRECTION ( 'NONE',  ( 0.000000000000000000, -1.000000000000000000, 0.000000000000000000 ) ) ;
#48531 = CIRCLE ( 'NONE', #25904, 5.999999999999998224 ) ;
#48532 = ORIENTED_EDGE ( 'NONE', *, *, #32623, .T. ) ;
#48533 = DIRECTION ( 'NONE',  ( 3.302498000000000159E-18, -1.533299999999999999E-17, -1.000000000000000000 ) ) ;
#48534 = AXIS2_PLACEMENT_3D ( 'NONE', #49910, #17676, #6145 ) ;
#48535 = CARTESIAN_POINT ( 'NONE',  ( 16.97480724641878425, -8.843458757663720249, -71.99243736330308252 ) ) ;
#48536 = CARTESIAN_POINT ( 'NONE',  ( 60.96148484106869603, 14.45202308121209889, -47.73691995860960446 ) ) ;
#48537 = AXIS2_PLACEMENT_3D ( 'NONE', #34449, #42860, #6433 ) ;
#48538 = CARTESIAN_POINT ( 'NONE',  ( 23.16791630292550153, -19.91803283035480021, -47.96704895327989959 ) ) ;
#48539 = DIRECTION ( 'NONE',  ( 0.000000000000000000, 0.000000000000000000, 1.000000000000000000 ) ) ;
#48540 = VECTOR ( 'NONE', #30650, 1000.000000000000000 ) ;
#48541 = CARTESIAN_POINT ( 'NONE',  ( 42.62079769550818042, -37.72101637537727470, -77.21563321993323825 ) ) ;
#48542 = B_SPLINE_CURVE_WITH_KNOTS ( 'NONE', 3,
 ( #7956, #6938, #51470, #19744, #27859, #15814, #22891, #43098, #23656, #7189, #101, #11386, #43353, #10866, #7446, #43609, #3255, #23145 ),
 .UNSPECIFIED., .F., .F.,
 ( 4, 2, 2, 2, 2, 2, 2, 2, 4 ),
 ( 0.000000000000000000, 0.06249980440203799226, 0.1249996088040759845, 0.1874994132061139629, 0.2499992176081519690, 0.3124990220101899752, 0.3749988264122279258, 0.4374986308142659319, 0.4999984352163039381 ),
 .UNSPECIFIED. ) ;
#48543 = ORIENTED_EDGE ( 'NONE', *, *, #45311, .T. ) ;
#48544 = B_SPLINE_CURVE_WITH_KNOTS ( 'NONE', 3,
 ( #23603, #39622, #44575, #20708, #800, #3725, #19698, #35689, #51674, #34512, #6236, #9901, #41874, #46342, #30052, #38729, #2563, #50518, #10428, #22192, #30318, #17762, #46081, #26380, #2825, #12880, #33733, #6494, #30576 ),
 .UNSPECIFIED., .F., .F.,
 ( 4, 2, 1, 1, 1, 1, 1, 2, 2, 2, 2, 2, 2, 2, 2, 2, 4 ),
 ( 0.5000036335122389763, 0.5002477723630629480, 0.5004919112138870307, 0.5009801889155351962, 0.5019567443188316380, 0.5039098551254245217, 0.5078160767386101782, 0.5156285199649813800, 0.5312534064177240056, 0.5625031793232091459, 0.6250027251341792045, 0.6875022709451493741, 0.7500018167561195437, 0.8125013625670896023, 0.8750009083780597718, 0.9375004541890299414, 1.000000000000000000 ),
 .UNSPECIFIED. ) ;
#48545 = CARTESIAN_POINT ( 'NONE',  ( 22.90093739769620029, -15.61618894467913243, -28.45282021618999835 ) ) ;
#48546 = CARTESIAN_POINT ( 'NONE',  ( 19.96627852001369874, -22.46453588084860087, -80.35009786776049623 ) ) ;
#48547 = ADVANCED_FACE ( 'NONE', ( #9280 ), #47808, .T. ) ;
#48548 = CARTESIAN_POINT ( 'NONE',  ( 16.13393739769620083, -15.61618894467929941, -22.14999999999999858 ) ) ;
#48549 = CARTESIAN_POINT ( 'NONE',  ( 13.89974045593869967, 20.77108261440800163, -75.51240970683940645 ) ) ;
#48550 = CARTESIAN_POINT ( 'NONE',  ( 51.67587649748560352, 17.38381105532069881, -77.01363636363639387 ) ) ;
#48551 = CARTESIAN_POINT ( 'NONE',  ( 83.66401895982360770, -44.51498057501240169, -46.61643406624109787 ) ) ;
#48552 = CARTESIAN_POINT ( 'NONE',  ( 23.83903845189011150, -13.54551734412039465, -57.70899791543581614 ) ) ;
#48553 = CARTESIAN_POINT ( 'NONE',  ( 24.37516582201759974, -15.36148368927210051, -41.49783386550709707 ) ) ;
#48554 = ORIENTED_EDGE ( 'NONE', *, *, #15659, .T. ) ;
#48555 = CARTESIAN_POINT ( 'NONE',  ( 53.88285922114570070, -48.70220139524560210, -27.00085731554899837 ) ) ;
#48556 = CARTESIAN_POINT ( 'NONE',  ( 14.09495638488309943, -50.67789608235420218, -21.23638623580770357 ) ) ;
#48557 = CARTESIAN_POINT ( 'NONE',  ( 17.16957436647078694, -23.52717616726175720, -64.25066604316528185 ) ) ;
#48558 = CARTESIAN_POINT ( 'NONE',  ( 75.44813142283744867, 12.59560967597626657, -13.51485765024892771 ) ) ;
#48559 = CARTESIAN_POINT ( 'NONE',  ( 16.13393739769620083, -15.61618894467929941, -35.12503119152809461 ) ) ;
#48560 = VECTOR ( 'NONE', #13490, 1000.000000000000114 ) ;
#48561 = EDGE_CURVE ( 'NONE', #51663, #44651, #35983, .T. ) ;
#48562 = EDGE_LOOP ( 'NONE', ( #40786, #20084 ) ) ;
#48563 = CIRCLE ( 'NONE', #50250, 0.5000000000000004441 ) ;
#48564 = CARTESIAN_POINT ( 'NONE',  ( -7.616042036189179854, -45.40507477012349824, -5.569053195681480162 ) ) ;
#48565 = ADVANCED_FACE ( 'NONE', ( #6372 ), #22334, .F. ) ;
#48566 = AXIS2_PLACEMENT_3D ( 'NONE', #39749, #36310, #27933 ) ;
#48567 = CARTESIAN_POINT ( 'NONE',  ( 47.28643180688370506, 23.49801600062669849, -54.74208605995080035 ) ) ;
#48569 = AXIS2_PLACEMENT_3D ( 'NONE', #12689, #21558, #37042 ) ;
#48568 = DIRECTION ( 'NONE',  ( 0.000000000000000000, 0.000000000000000000, 1.000000000000000000 ) ) ;
#48570 = CARTESIAN_POINT ( 'NONE',  ( 63.02699984107479025, 0.9952464559119579279, -62.51628753338329858 ) ) ;
#48571 = CARTESIAN_POINT ( 'NONE',  ( 54.63655771189059607, 16.82059223505549994, -26.73578643762699869 ) ) ;
#48572 = CIRCLE ( 'NONE', #21772, 1.999999999999996669 ) ;
#48573 = CARTESIAN_POINT ( 'NONE',  ( 11.23165351422320057, 33.99825783758829800, -17.66286062877820129 ) ) ;
#48574 = ADVANCED_FACE ( 'NONE', ( #26525 ), #50400, .T. ) ;
#48575 = CARTESIAN_POINT ( 'NONE',  ( 20.63393739769620083, -41.61618894467930119, -34.64999999999999858 ) ) ;
#48576 = CARTESIAN_POINT ( 'NONE',  ( 9.366959236597619309, -16.50214705144793470, -65.41115364195393056 ) ) ;
#48577 = CARTESIAN_POINT ( 'NONE',  ( 72.72056432233058842, 1.396834109478129804, -62.44999999999999574 ) ) ;
#48578 = CARTESIAN_POINT ( 'NONE',  ( 54.33046565385170368, -48.97104959639300148, -48.91876050846019552 ) ) ;
#48579 = CARTESIAN_POINT ( 'NONE',  ( 23.79191343808687620, -13.56498988170000608, -75.70900991007390246 ) ) ;
#48580 = CARTESIAN_POINT ( 'NONE',  ( 9.367786036389057713, -14.73543740969510374, -79.88861889020083140 ) ) ;
#48581 = CARTESIAN_POINT ( 'NONE',  ( 56.42542598226509654, 19.53946997070610081, -53.51082495327469246 ) ) ;
#48582 = FACE_OUTER_BOUND ( 'NONE', #15806, .T. ) ;
#48583 = CARTESIAN_POINT ( 'NONE',  ( 16.22164304676950408, -22.66849390760810223, -80.94886153518950778 ) ) ;
#48584 = PLANE ( 'NONE',  #16546 ) ;
#48585 = VERTEX_POINT ( 'NONE', #30457 ) ;
#48586 = CARTESIAN_POINT ( 'NONE',  ( 20.12219014770483483, 24.14963702508532606, -19.95441604237223743 ) ) ;
#48587 = CARTESIAN_POINT ( 'NONE',  ( 10.48584413461309950, 31.89781099419320043, -45.62883909305980268 ) ) ;
#48588 = CARTESIAN_POINT ( 'NONE',  ( 44.76368420724840291, 13.86998310020809910, -7.024004829805569727 ) ) ;
#48589 = CARTESIAN_POINT ( 'NONE',  ( -21.36606260230379917, -53.11618894467930119, 16.35000000000000142 ) ) ;
#48590 = ORIENTED_EDGE ( 'NONE', *, *, #29319, .T. ) ;
#48591 = CARTESIAN_POINT ( 'NONE',  ( 17.86297238746119831, 20.47201121247589839, -75.55956264724760274 ) ) ;
#48592 = EDGE_LOOP ( 'NONE', ( #41247, #12754, #28982, #33720, #41551, #44489, #3279, #4118 ) ) ;
#48593 = ORIENTED_EDGE ( 'NONE', *, *, #10787, .T. ) ;
#48594 = ORIENTED_EDGE ( 'NONE', *, *, #11084, .T. ) ;
#48595 = EDGE_CURVE ( 'NONE', #22140, #25228, #34289, .T. ) ;
#48596 = CARTESIAN_POINT ( 'NONE',  ( 12.01839223830350001, -65.30369916784260909, -47.05360386500180425 ) ) ;
#48597 = CARTESIAN_POINT ( 'NONE',  ( 23.06214062797170072, -27.61618894467930119, -32.14999999999999858 ) ) ;
#48598 = CARTESIAN_POINT ( 'NONE',  ( 22.35028251693639945, -19.17153531005600087, -81.23899999999999011 ) ) ;
#48599 = CARTESIAN_POINT ( 'NONE',  ( 61.67010585289130375, 13.90326159682560103, -46.64609547319909666 ) ) ;
#48600 = ORIENTED_EDGE ( 'NONE', *, *, #49341, .F. ) ;
#48601 = ORIENTED_EDGE ( 'NONE', *, *, #6621, .T. ) ;
#48602 = ORIENTED_EDGE ( 'NONE', *, *, #42489, .F. ) ;
#48603 = CARTESIAN_POINT ( 'NONE',  ( 9.651154978174693255, -13.08642360888446987, -41.96614601027561520 ) ) ;
#48604 = CARTESIAN_POINT ( 'NONE',  ( 61.33486291256839706, -45.61980825670960371, -47.69940288585109300 ) ) ;
#48605 = CARTESIAN_POINT ( 'NONE',  ( 14.63393739769640156, 10.88381105532070059, -34.64999999999999858 ) ) ;
#48606 = EDGE_LOOP ( 'NONE', ( #37918, #18382, #34243, #40656, #6240 ) ) ;
#48607 = AXIS2_PLACEMENT_3D ( 'NONE', #46983, #39360, #38851 ) ;
#48608 = EDGE_LOOP ( 'NONE', ( #44915, #16013, #30652, #20787 ) ) ;
#48609 = CARTESIAN_POINT ( 'NONE',  ( -18.86606260230390220, 19.38381105532060289, 11.34999999999999964 ) ) ;
#48610 = DIRECTION ( 'NONE',  ( 0.9083627212242635363, -0.3704194192529762786, -0.1940789028471121280 ) ) ;
#48611 = VECTOR ( 'NONE', #31808, 1000.000000000000000 ) ;
#48612 = CARTESIAN_POINT ( 'NONE',  ( 71.10514731706700786, 12.15699934429280127, -12.15279640865730038 ) ) ;
#48613 = EDGE_CURVE ( 'NONE', #50703, #37063, #30718, .T. ) ;
#48614 = VECTOR ( 'NONE', #45835, 1000.000000000000000 ) ;
#48615 = ADVANCED_FACE ( 'NONE', ( #44072 ), #25079, .F. ) ;
#48616 = CARTESIAN_POINT ( 'NONE',  ( 49.63401988979710211, 13.97123100121650197, -10.90947558922509941 ) ) ;
#48617 = B_SPLINE_CURVE_WITH_KNOTS ( 'NONE', 3,
 ( #21160, #17251, #27360, #19244, #46072, #43623, #2033, #18013, #10421, #43367, #2292, #34233, #31277, #10159, #23669, #35751, #39686, #46335 ),
 .UNSPECIFIED., .F., .F.,
 ( 4, 2, 2, 2, 2, 2, 2, 2, 4 ),
 ( 0.000000000000000000, 0.06249992064097868727, 0.1249998412819573745, 0.1874997619229360479, 0.2499996825639147491, 0.3124996032048934502, 0.3749995238458720959, 0.4374994444868507970, 0.4999993651278294982 ),
 .UNSPECIFIED. ) ;
#48618 = DIRECTION ( 'NONE',  ( 1.000000000000000000, 0.000000000000000000, 0.000000000000000000 ) ) ;
#48619 = CARTESIAN_POINT ( 'NONE',  ( -6.140345869213950536, 15.17335822531540046, -4.613862302043099994 ) ) ;
#48620 = CARTESIAN_POINT ( 'NONE',  ( 22.90067702240739322, -15.61618873416334807, -54.84718332859007006 ) ) ;
#48621 = CARTESIAN_POINT ( 'NONE',  ( 58.29889914173639909, 14.43956164479439863, -26.41833035305619859 ) ) ;
#48622 = CARTESIAN_POINT ( 'NONE',  ( 15.45935907336719950, -23.43486480875809974, -59.81490083174309547 ) ) ;
#48623 = ORIENTED_EDGE ( 'NONE', *, *, #9876, .T. ) ;
#48624 = CYLINDRICAL_SURFACE ( 'NONE', #5433, 6.766999999999998572 ) ;
#48625 = CARTESIAN_POINT ( 'NONE',  ( 23.37006864188879973, -49.24610395064770074, -34.65445009297679491 ) ) ;
#48626 = CARTESIAN_POINT ( 'NONE',  ( 12.96176040339469893, 34.28310491318730158, -47.67058438006289833 ) ) ;
#48627 = CARTESIAN_POINT ( 'NONE',  ( 72.43509047223609798, 1.031856533264720266, -69.83351529264139401 ) ) ;
#48628 = CARTESIAN_POINT ( 'NONE',  ( 43.21150532606133510, -39.88589448485808475, -70.47653842715691042 ) ) ;
#48629 = EDGE_CURVE ( 'NONE', #6528, #11300, #28067, .T. ) ;
#48630 = CARTESIAN_POINT ( 'NONE',  ( 15.09840986696447729, -23.52719135345972390, -36.33399691850734570 ) ) ;
#48631 = EDGE_CURVE ( 'NONE', #20276, #13824, #27424, .T. ) ;
#48632 = CARTESIAN_POINT ( 'NONE',  ( 49.35390693627829961, -53.59897724190700075, -54.31982765639760657 ) ) ;
#48633 = CARTESIAN_POINT ( 'NONE',  ( -5.431977005845720186, 16.07634798542799714, -5.576406780277120667 ) ) ;
#48634 = B_SPLINE_CURVE_WITH_KNOTS ( 'NONE', 3,
 ( #4340, #35280, #31841, #23459, #48368, #51535, #15632, #20056, #11705, #27667, #31330, #48112, #12211, #27153, #43161, #23204, #39224, #43669, #3319, #23721 ),
 .UNSPECIFIED., .F., .F.,
 ( 4, 2, 2, 2, 2, 2, 2, 2, 2, 4 ),
 ( -1.826162956740689847, -1.707995156971769957, -1.458514671262659990, -1.209832958840709960, -1.027216663166639954, -0.9130814783703469217, -0.6848111087777599693, -0.4130647882495273038, -0.1614699006445539098, 0.000000000000000000 ),
 .UNSPECIFIED. ) ;
#48635 = CARTESIAN_POINT ( 'NONE',  ( 18.57796361324281520, -23.17930195404681015, -33.90807609102002829 ) ) ;
#48636 = CYLINDRICAL_SURFACE ( 'NONE', #7047, 40.00000000000000000 ) ;
#48637 = LINE ( 'NONE', #8020, #18891 ) ;
#48638 = EDGE_LOOP ( 'NONE', ( #42659, #33921, #17022, #9806 ) ) ;
#48639 = CARTESIAN_POINT ( 'NONE',  ( 19.97308036710279922, -22.00114592173070349, -47.39502254529469383 ) ) ;
#48640 = CARTESIAN_POINT ( 'NONE',  ( 63.95563233927359192, 1.117804454683279936, -61.34981482092570104 ) ) ;
#48641 = ORIENTED_EDGE ( 'NONE', *, *, #11364, .T. ) ;
#48642 = CARTESIAN_POINT ( 'NONE',  ( 54.53726589893891230, -46.02701840152597157, -15.67785061177839978 ) ) ;
#48643 = AXIS2_PLACEMENT_3D ( 'NONE', #33566, #41964, #1866 ) ;
#48644 = CARTESIAN_POINT ( 'NONE',  ( 61.03140963465120450, -45.55308648458009912, -47.57043735694709596 ) ) ;
#48645 = CARTESIAN_POINT ( 'NONE',  ( 9.903866441572990453, -10.68225490921047971, -81.00563702421779055 ) ) ;
#48646 = CARTESIAN_POINT ( 'NONE',  ( 50.29495134167750336, 18.68575087643539945, -76.14999999999999147 ) ) ;
#48648 = CARTESIAN_POINT ( 'NONE',  ( 44.66545912666861540, -33.16365024224258917, -44.73623550635601731 ) ) ;
#48647 = CARTESIAN_POINT ( 'NONE',  ( 42.13187174340301766, 8.546205365918842389, -75.69530005827525088 ) ) ;
#48649 = CIRCLE ( 'NONE', #46157, 3.000000000000000000 ) ;
#48650 = CARTESIAN_POINT ( 'NONE',  ( 52.57481654442310059, -51.43204889509869560, -75.83555718502590537 ) ) ;
#48651 = LINE ( 'NONE', #29227, #31959 ) ;
#48652 = ORIENTED_EDGE ( 'NONE', *, *, #2718, .F. ) ;
#48653 = CARTESIAN_POINT ( 'NONE',  ( 83.30448183675909490, -45.24061545150300390, -47.41172112684520101 ) ) ;
#48654 = ORIENTED_EDGE ( 'NONE', *, *, #23115, .F. ) ;
#48655 = ORIENTED_EDGE ( 'NONE', *, *, #28769, .F. ) ;
#48656 = VERTEX_POINT ( 'NONE', #3989 ) ;
#48657 = DIRECTION ( 'NONE',  ( 0.000000000000000000, 0.000000000000000000, 1.000000000000000000 ) ) ;
#48658 = CARTESIAN_POINT ( 'NONE',  ( 52.47677897125242197, -49.96156889689471114, -77.24546347434363724 ) ) ;
#48659 = CARTESIAN_POINT ( 'NONE',  ( 76.44816630901640053, -6.457295309286853247, -13.00405914655548578 ) ) ;
#48660 = CARTESIAN_POINT ( 'NONE',  ( 49.64260032845790249, -53.66077289818650087, -54.78414101162699978 ) ) ;
#48661 = ORIENTED_EDGE ( 'NONE', *, *, #25274, .T. ) ;
#48662 = ORIENTED_EDGE ( 'NONE', *, *, #45668, .F. ) ;
#48663 = LINE ( 'NONE', #40020, #2520 ) ;
#48664 = DIRECTION ( 'NONE',  ( -0.000000000000000000, 1.000000000000000000, 0.000000000000000000 ) ) ;
#48665 = CYLINDRICAL_SURFACE ( 'NONE', #36205, 31.00000000000000000 ) ;
#48666 = FACE_OUTER_BOUND ( 'NONE', #29140, .T. ) ;
#48667 = CARTESIAN_POINT ( 'NONE',  ( 64.04792041323590013, 0.7580616222945849580, -17.48146414341379895 ) ) ;
#48668 = CARTESIAN_POINT ( 'NONE',  ( 11.63393739769600010, 10.38381105532060111, -54.64999999999999858 ) ) ;
#48669 = ORIENTED_EDGE ( 'NONE', *, *, #48869, .T. ) ;
#48670 = CARTESIAN_POINT ( 'NONE',  ( 25.43010376912519988, -1.113097814880039893, -35.14999999999999858 ) ) ;
#48671 = CARTESIAN_POINT ( 'NONE',  ( 53.53698447494460311, -50.55136415298420616, -77.03764851654500490 ) ) ;
#48672 = CARTESIAN_POINT ( 'NONE',  ( 64.97290478796050195, 0.8840451408750739093, -70.74985906855570761 ) ) ;
#48673 = CARTESIAN_POINT ( 'NONE',  ( 60.71265700703109758, 14.29847002888300089, -47.11594162556460219 ) ) ;
#48674 = EDGE_CURVE ( 'NONE', #24567, #17140, #32407, .T. ) ;
#48675 = CARTESIAN_POINT ( 'NONE',  ( 16.23592030529090025, -7.769129171863720096, -67.51663103545399736 ) ) ;
#48676 = EDGE_CURVE ( 'NONE', #39784, #27219, #43568, .T. ) ;
#48677 = CARTESIAN_POINT ( 'NONE',  ( 14.04950511168917515, -17.13061764721083335, -40.14999999999999858 ) ) ;
#48678 = CARTESIAN_POINT ( 'NONE',  ( 41.98453321725290266, -44.09319621180809889, -4.765379593933540825 ) ) ;
#48679 = DIRECTION ( 'NONE',  ( 0.000000000000000000, 0.000000000000000000, 1.000000000000000000 ) ) ;
#48680 = ADVANCED_FACE ( 'NONE', ( #47757 ), #20083, .F. ) ;
#48681 = CARTESIAN_POINT ( 'NONE',  ( 57.14903038794999901, 13.88381105532070059, -16.26185532857629923 ) ) ;
#48682 = CARTESIAN_POINT ( 'NONE',  ( 61.44133198084610115, -45.34716915528590420, -47.30158679574340397 ) ) ;
#48683 = CONICAL_SURFACE ( 'NONE', #36135, 1.942499999999999227, 0.8266833912447979493 ) ;
#48684 = TOROIDAL_SURFACE ( 'NONE', #33192, 9.000000000000000000, 1.000000000000000000 ) ;
#48685 = CARTESIAN_POINT ( 'NONE',  ( 64.03708764054000824, 1.112169578473010123, -70.02730617886231812 ) ) ;
#48686 = DIRECTION ( 'NONE',  ( 0.7071067811865475727, -0.7071067811865475727, 0.000000000000000000 ) ) ;
#48687 = AXIS2_PLACEMENT_3D ( 'NONE', #17976, #33688, #33942 ) ;
#48688 = CARTESIAN_POINT ( 'NONE',  ( 65.13280820348710165, 0.9471869900316070012, -17.73393088427939901 ) ) ;
#48689 = ORIENTED_EDGE ( 'NONE', *, *, #9567, .T. ) ;
#48690 = CARTESIAN_POINT ( 'NONE',  ( 13.72816481212180051, -51.57539031256769846, -74.98719232987430416 ) ) ;
#48691 = CARTESIAN_POINT ( 'NONE',  ( 47.33080767030429570, -54.69887959644039910, -54.70291218041550252 ) ) ;
#48692 = CARTESIAN_POINT ( 'NONE',  ( 17.16948702526555337, -7.705189252755917373, -37.04933676831282696 ) ) ;
#48693 = CARTESIAN_POINT ( 'NONE',  ( 68.13393739769618662, -0.5161889446793590519, -65.65000000000000568 ) ) ;
#48694 = CARTESIAN_POINT ( 'NONE',  ( 41.61626771661330082, -37.56081407618439982, -82.23834840541459812 ) ) ;
#48695 = CARTESIAN_POINT ( 'NONE',  ( 22.12600828401099662, -12.01106615515799980, -32.14999999999999858 ) ) ;
#48696 = CARTESIAN_POINT ( 'NONE',  ( 8.223247527389670353, -15.61637340300369914, -74.79233150823711185 ) ) ;
#48697 = EDGE_CURVE ( 'NONE', #35884, #46345, #39123, .T. ) ;
#48698 = CARTESIAN_POINT ( 'NONE',  ( 47.70337372003230314, -54.50475343038620224, -55.04617154330599504 ) ) ;
#48700 = CARTESIAN_POINT ( 'NONE',  ( 20.11811409522369587, -22.52868499068620167, -73.84100135226722728 ) ) ;
#48699 = FACE_OUTER_BOUND ( 'NONE', #31801, .T. ) ;
#48701 = CARTESIAN_POINT ( 'NONE',  ( 64.93393739769619799, 10.88381105532070059, -62.44999999999999574 ) ) ;
#48702 = CARTESIAN_POINT ( 'NONE',  ( 48.73758251462950142, 22.81230782973970150, -55.00444999029969750 ) ) ;
#48703 = ORIENTED_EDGE ( 'NONE', *, *, #23634, .F. ) ;
#48704 = CARTESIAN_POINT ( 'NONE',  ( 18.25866816536740345, -8.891006542739390284, -64.44458661451268711 ) ) ;
#48705 = ORIENTED_EDGE ( 'NONE', *, *, #3829, .F. ) ;
#48706 = DIRECTION ( 'NONE',  ( 0.000000000000000000, 0.000000000000000000, 1.000000000000000000 ) ) ;
#48707 = DIRECTION ( 'NONE',  ( 0.000000000000000000, -0.7071067811865492381, 0.7071067811865457964 ) ) ;
#48708 = CARTESIAN_POINT ( 'NONE',  ( 16.13393739769620083, -15.61618894467929941, -35.14999999999999858 ) ) ;
#48710 = CARTESIAN_POINT ( 'NONE',  ( 53.51583085569070164, 17.59825481099489863, -26.65935230799360056 ) ) ;
#48709 = CARTESIAN_POINT ( 'NONE',  ( 84.22920232233479965, 12.56550928184170068, -47.02060905303799387 ) ) ;
#48711 = CARTESIAN_POINT ( 'NONE',  ( 10.26677323880680071, -11.70224675945619985, -67.64008111650149146 ) ) ;
#48712 = DIRECTION ( 'NONE',  ( 0.000000000000000000, -1.000000000000000000, 0.000000000000000000 ) ) ;
#48713 = CARTESIAN_POINT ( 'NONE',  ( 55.78663148921049952, -45.30254049228850732, -15.70162090623030160 ) ) ;
#48714 = CYLINDRICAL_SURFACE ( 'NONE', #28937, 6.049999999999999822 ) ;
#48715 = EDGE_LOOP ( 'NONE', ( #16876, #34189, #20939, #21571 ) ) ;
#48716 = ORIENTED_EDGE ( 'NONE', *, *, #28778, .F. ) ;
#48717 = CARTESIAN_POINT ( 'NONE',  ( 11.65450058716879944, -65.12719674309839490, -16.76600934541859900 ) ) ;
#48718 = CARTESIAN_POINT ( 'NONE',  ( 11.95077454560339980, 34.11711772380790109, -47.35066886291930643 ) ) ;
#48719 = DIRECTION ( 'NONE',  ( 0.000000000000000000, -0.7071067811865466846, -0.7071067811865483499 ) ) ;
#48720 = AXIS2_PLACEMENT_3D ( 'NONE', #6500, #9906, #25864 ) ;
#48721 = CARTESIAN_POINT ( 'NONE',  ( 50.39481201540360189, -52.19103705647920322, -52.11755584844750189 ) ) ;
#48722 = CARTESIAN_POINT ( 'NONE',  ( 74.17629866868290378, 1.883811055320649963, -65.34607522167520699 ) ) ;
#48723 = VECTOR ( 'NONE', #6758, 1000.000000000000000 ) ;
#48724 = VERTEX_POINT ( 'NONE', #35698 ) ;
#48725 = CARTESIAN_POINT ( 'NONE',  ( 23.04644875934005555, -11.63203529592211893, -75.34097925061534795 ) ) ;
#48726 = CARTESIAN_POINT ( 'NONE',  ( 53.11475001244221517, 18.18247718396222368, -27.56270898827361293 ) ) ;
#48727 = CARTESIAN_POINT ( 'NONE',  ( 50.39592751844079999, 21.35098830175070006, -53.02100607687120259 ) ) ;
#48728 = CARTESIAN_POINT ( 'NONE',  ( 72.54418616719020463, 1.434949534324099885, -69.27291511353429598 ) ) ;
#48729 = CARTESIAN_POINT ( 'NONE',  ( 50.31585484890159421, -48.88982717754599605, -76.16276048729439196 ) ) ;
#48730 = DIRECTION ( 'NONE',  ( 0.8545454545454611583, 0.000000000000000000, -0.5193766129849238800 ) ) ;
#48731 = ORIENTED_EDGE ( 'NONE', *, *, #5712, .T. ) ;
#48732 = DIRECTION ( 'NONE',  ( 0.000000000000000000, 1.000000000000000000, 0.000000000000000000 ) ) ;
#48733 = DIRECTION ( 'NONE',  ( 0.000000000000000000, 0.000000000000000000, -1.000000000000000000 ) ) ;
#48734 = ORIENTED_EDGE ( 'NONE', *, *, #48230, .T. ) ;
#48735 = CARTESIAN_POINT ( 'NONE',  ( 57.27851914992729832, -50.15376702335620251, -52.63313635724109929 ) ) ;
#48736 = CARTESIAN_POINT ( 'NONE',  ( 55.91507730363359485, 15.44714545385880022, -45.94138956033829402 ) ) ;
#48737 = CARTESIAN_POINT ( 'NONE',  ( 14.81467456660999993, -7.815966731016759539, -81.23899999999999011 ) ) ;
#48738 = ADVANCED_FACE ( 'NONE', ( #31730, #11863 ), #47251, .T. ) ;
#48739 = CARTESIAN_POINT ( 'NONE',  ( 14.30978967243840039, -51.11618894516979594, -22.40422843537090003 ) ) ;
#48740 = CARTESIAN_POINT ( 'NONE',  ( 55.28540664048680497, 19.68320257923529937, -75.28129500772568861 ) ) ;
#48741 = CONTEXT_DEPENDENT_SHAPE_REPRESENTATION ( #30096, #1434 ) ;
#48742 = CARTESIAN_POINT ( 'NONE',  ( 47.36065766533170063, -54.38989670583089975, -75.11697231728020085 ) ) ;
#48743 = ORIENTED_EDGE ( 'NONE', *, *, #3736, .F. ) ;
#48744 = DIRECTION ( 'NONE',  ( -1.000000000000000000, 0.000000000000000000, 0.000000000000000000 ) ) ;
#48745 = CARTESIAN_POINT ( 'NONE',  ( 9.681283356623689329, -11.89195081703809898, -61.39927945301539580 ) ) ;
#48746 = CARTESIAN_POINT ( 'NONE',  ( 53.12230990226080252, -49.57349283027179609, -49.13891823708339501 ) ) ;
#48747 = DIRECTION ( 'NONE',  ( 1.000000000000000000, 0.000000000000000000, 0.000000000000000000 ) ) ;
#48748 = CARTESIAN_POINT ( 'NONE',  ( 47.39179696941629771, 23.33325173635930128, -74.72254318496639769 ) ) ;
#48749 = CARTESIAN_POINT ( 'NONE',  ( 47.13393739769619373, -38.94772025634554780, -54.35302954682959609 ) ) ;
#48750 = EDGE_CURVE ( 'NONE', #43415, #26981, #39377, .T. ) ;
#48751 = CARTESIAN_POINT ( 'NONE',  ( 29.13393739769619728, -4.468739684871080087, -35.14999999999999858 ) ) ;
#48752 = AXIS2_PLACEMENT_3D ( 'NONE', #1867, #41185, #46166 ) ;
#48753 = AXIS2_PLACEMENT_3D ( 'NONE', #10453, #10192, #14634 ) ;
#48754 = LINE ( 'NONE', #48487, #12702 ) ;
#48755 = CARTESIAN_POINT ( 'NONE',  ( 24.04490452168148451, -15.61618923948461557, -69.79232899952297942 ) ) ;
#48756 = ADVANCED_FACE ( 'NONE', ( #23612 ), #40182, .F. ) ;
#48757 = CYLINDRICAL_SURFACE ( 'NONE', #23579, 7.910999999999997812 ) ;
#48759 = CARTESIAN_POINT ( 'NONE',  ( 0.4047412638265869833, -22.38804348994680282, -35.14999999999999858 ) ) ;
#48758 = SURFACE_STYLE_USAGE ( .BOTH. , #48238 ) ;
#48761 = EDGE_CURVE ( 'NONE', #50288, #6764, #46903, .T. ) ;
#48760 = CARTESIAN_POINT ( 'NONE',  ( 63.49388541862201407, 1.387412027389909985, -68.69511434646409498 ) ) ;
#48762 = CARTESIAN_POINT ( 'NONE',  ( 61.32020094034120916, 13.98164174484680089, -46.53643907696579873 ) ) ;
#48763 = CARTESIAN_POINT ( 'NONE',  ( -33.07468191286329784, -25.33318566548249962, -56.92399776842329828 ) ) ;
#48764 = ORIENTED_EDGE ( 'NONE', *, *, #30074, .T. ) ;
#48765 = CARTESIAN_POINT ( 'NONE',  ( 53.45012425295129788, -49.34429749072780425, -48.87690323766360478 ) ) ;
#48766 = CARTESIAN_POINT ( 'NONE',  ( 61.72858909456450505, -45.11618897281839935, -27.86494589658979848 ) ) ;
#48767 = DIRECTION ( 'NONE',  ( 0.000000000000000000, 0.000000000000000000, -1.000000000000000000 ) ) ;
#48768 = CARTESIAN_POINT ( 'NONE',  ( 56.96266382495790026, 14.69614837228800042, -26.24591337028120108 ) ) ;
#48769 = CARTESIAN_POINT ( 'NONE',  ( 10.09870140130719918, -19.26563892577449977, -39.27970379572569470 ) ) ;
#48770 = CARTESIAN_POINT ( 'NONE',  ( 50.62541591231190097, 17.89847220828429997, -76.22054775280069805 ) ) ;
#48771 = CARTESIAN_POINT ( 'NONE',  ( 52.69435528435500515, 18.51371064498010099, -48.50601979887200343 ) ) ;
#48772 = CARTESIAN_POINT ( 'NONE',  ( 71.36799767121769378, 0.8859637708054489691, -70.70388507757908769 ) ) ;
#48773 = DIRECTION ( 'NONE',  ( -1.224646799147355179E-16, 1.000000000000000000, -2.054487543405498457E-16 ) ) ;
#48774 = CARTESIAN_POINT ( 'NONE',  ( 47.06135413360298259, 22.56673458786644559, -75.82639806858723830 ) ) ;
#48775 = EDGE_LOOP ( 'NONE', ( #2254, #48623 ) ) ;
#48776 = CYLINDRICAL_SURFACE ( 'NONE', #4377, 7.910999999999997812 ) ;
#48777 = CARTESIAN_POINT ( 'NONE',  ( 9.865947636674368582, -11.58890714499520058, -66.24912813843610593 ) ) ;
#48778 = CARTESIAN_POINT ( 'NONE',  ( 73.05322604375929529, 1.097545367735389910, -69.01875481685119951 ) ) ;
#48779 = CARTESIAN_POINT ( 'NONE',  ( 47.74639995886609967, -54.45100479285450490, -54.79047585474189930 ) ) ;
#48780 = CARTESIAN_POINT ( 'NONE',  ( 72.91520214831270152, 1.373356196620459935, -62.69406858229250901 ) ) ;
#48781 =( BOUNDED_CURVE ( )  B_SPLINE_CURVE ( 3, ( #8792, #44688, #12208, #43919 ),
 .UNSPECIFIED., .F., .T. ) 
 B_SPLINE_CURVE_WITH_KNOTS ( ( 4, 4 ),
 ( 1.195525503939052436, 1.980923667336377703 ),
 .UNSPECIFIED. ) 
 CURVE ( )  GEOMETRIC_REPRESENTATION_ITEM ( )  RATIONAL_B_SPLINE_CURVE ( ( 1.000000000000000000, 0.9492530216742067761, 0.9492530216742067761, 1.000000000000000000 ) ) 
 REPRESENTATION_ITEM ( '' )  );
#48782 = CARTESIAN_POINT ( 'NONE',  ( 71.15040120820690106, 1.386342629514219826, -61.00047607903670155 ) ) ;
#48783 = CARTESIAN_POINT ( 'NONE',  ( 46.94631559364368911, 7.984621261935255454, -34.75526898281330546 ) ) ;
#48784 = CARTESIAN_POINT ( 'NONE',  ( 72.18870199502219975, 1.048861872235970161, -61.22695438956509406 ) ) ;
#48785 = DIRECTION ( 'NONE',  ( -1.000000000000000000, 0.000000000000000000, 0.000000000000000000 ) ) ;
#48786 = CARTESIAN_POINT ( 'NONE',  ( 64.89029781878299730, 1.096291039689149871, -70.64841943982850125 ) ) ;
#48787 = ORIENTED_EDGE ( 'NONE', *, *, #20785, .T. ) ;
#48788 = EDGE_LOOP ( 'NONE', ( #28334, #8729, #17850, #9076 ) ) ;
#48789 = CARTESIAN_POINT ( 'NONE',  ( 18.20458331782904793, -7.911079347056140243, -55.37565539348986476 ) ) ;
#48790 = DIRECTION ( 'NONE',  ( 0.000000000000000000, 0.7071067811865521247, 0.7071067811865429098 ) ) ;
#48791 = ORIENTED_EDGE ( 'NONE', *, *, #30363, .T. ) ;
#48792 = CARTESIAN_POINT ( 'NONE',  ( 11.70307022357610016, -64.92107323957129950, -45.14224943014770020 ) ) ;
#48793 = CARTESIAN_POINT ( 'NONE',  ( 17.90516122990442227, -9.025309029999688093, -70.03615537855314699 ) ) ;
#48794 = CARTESIAN_POINT ( 'NONE',  ( 19.08568541577971800, -9.510811376752775104, -50.09616398158074446 ) ) ;
#48795 = CARTESIAN_POINT ( 'NONE',  ( 51.93051863921090217, 19.02772527816939885, -76.53037500023199868 ) ) ;
#48796 = AXIS2_PLACEMENT_3D ( 'NONE', #23087, #10288, #22829 ) ;
#48797 = ORIENTED_EDGE ( 'NONE', *, *, #16648, .T. ) ;
#48798 = VECTOR ( 'NONE', #17474, 1000.000000000000227 ) ;
#48799 = DIRECTION ( 'NONE',  ( 0.1686178020941670186, 0.6660492713794450292, -0.7265992051412130115 ) ) ;
#48800 = CARTESIAN_POINT ( 'NONE',  ( 21.52719323332197732, -11.43332263511563518, -72.24312383686958583 ) ) ;
#48801 = CARTESIAN_POINT ( 'NONE',  ( 24.03335507664926141, -16.05328977305849136, -65.52525647391593111 ) ) ;
#48802 = CARTESIAN_POINT ( 'NONE',  ( 20.96782168322129891, -8.936646836863200605, -47.49173536689819741 ) ) ;
#48803 = EDGE_CURVE ( 'NONE', #51503, #15968, #20458, .T. ) ;
#48804 = DIRECTION ( 'NONE',  ( 1.000000000000000000, 2.460964292799963328E-14, 0.000000000000000000 ) ) ;
#48805 = CARTESIAN_POINT ( 'NONE',  ( 43.03680859621228905, -37.78309590381571326, -75.13564474923592229 ) ) ;
#48806 = B_SPLINE_CURVE_WITH_KNOTS ( 'NONE', 3,
 ( #24558, #17755, #40832, #25345, #1774, #37417, #36900, #29286 ),
 .UNSPECIFIED., .F., .F.,
 ( 4, 1, 3, 4 ),
 ( 0.000000000000000000, 0.4999600334511122846, 0.9999200669022245691, 1.000000000000000000 ),
 .UNSPECIFIED. ) ;
#48807 = ORIENTED_EDGE ( 'NONE', *, *, #25587, .F. ) ;
#48808 = CARTESIAN_POINT ( 'NONE',  ( 11.44746559451110102, -65.00817642577131039, -23.48109952293140168 ) ) ;
#48809 = CARTESIAN_POINT ( 'NONE',  ( 18.40131669078889942, -8.519310590983641518, -33.83109144287589487 ) ) ;
#48810 = CARTESIAN_POINT ( 'NONE',  ( 11.57646884939659948, -10.52741891998659973, -32.14999999999999858 ) ) ;
#48811 = CIRCLE ( 'NONE', #32013, 24.90000000000000213 ) ;
#48812 = CARTESIAN_POINT ( 'NONE',  ( 14.83771907029349890, 21.57872223484060115, -76.12922349804929922 ) ) ;
#48813 = CARTESIAN_POINT ( 'NONE',  ( 52.25095813476680462, 18.53891199752670005, -77.19024044419620623 ) ) ;
#48814 = CARTESIAN_POINT ( 'NONE',  ( 16.13393739769620083, -29.47259540523039689, -47.64999999999999858 ) ) ;
#48815 = CARTESIAN_POINT ( 'NONE',  ( 13.52923768432050089, -7.793257261984160245, -52.90535993866839704 ) ) ;
#48816 = ORIENTED_EDGE ( 'NONE', *, *, #6734, .T. ) ;
#48817 = CARTESIAN_POINT ( 'NONE',  ( 52.98091703242110384, -49.46538585664740140, -27.45852672937839856 ) ) ;
#48818 = CARTESIAN_POINT ( 'NONE',  ( 14.72196958648260079, -51.10496628337289593, -22.05098504494149836 ) ) ;
#48819 = CARTESIAN_POINT ( 'NONE',  ( 24.04493739427486076, -15.63665726277926460, -39.50849474849957232 ) ) ;
#48820 = CARTESIAN_POINT ( 'NONE',  ( 57.15189004838642717, 12.22388545694372475, -8.325998452327215915 ) ) ;
#48821 = TOROIDAL_SURFACE ( 'NONE', #30400, 40.00000000000310507, 2.000000000000059952 ) ;
#48823 = EDGE_CURVE ( 'NONE', #13190, #34524, #306, .T. ) ;
#48822 = CARTESIAN_POINT ( 'NONE',  ( 22.90011000694050480, -14.71637116526028422, -52.80484287475383809 ) ) ;
#48824 = CARTESIAN_POINT ( 'NONE',  ( 16.13393739769620083, -15.61618894467929941, 7.849999999999999645 ) ) ;
#48825 = CIRCLE ( 'NONE', #22050, 20.00000000000000000 ) ;
#48826 = ORIENTED_EDGE ( 'NONE', *, *, #21347, .T. ) ;
#48827 = CARTESIAN_POINT ( 'NONE',  ( -10.42019467055720128, -42.80886955819109829, -6.071270369134899703 ) ) ;
#48828 = VECTOR ( 'NONE', #30722, 1000.000000000000000 ) ;
#48829 = CARTESIAN_POINT ( 'NONE',  ( 47.29954908011710302, 23.48849187898310120, -54.71030354338810042 ) ) ;
#48830 = CARTESIAN_POINT ( 'NONE',  ( 41.64265090550279780, 15.19461330350340056, -4.296538310234330638 ) ) ;
#48831 = CARTESIAN_POINT ( 'NONE',  ( 63.15932386229340523, 0.8936201581567979613, -62.29538467389520662 ) ) ;
#48832 = FACE_OUTER_BOUND ( 'NONE', #32497, .T. ) ;
#48833 = CARTESIAN_POINT ( 'NONE',  ( 11.49541394825649832, 34.11692877016390213, -17.78290644886299887 ) ) ;
#48834 = DIRECTION ( 'NONE',  ( 1.000000000000000000, 0.000000000000000000, 0.000000000000000000 ) ) ;
#48835 = CARTESIAN_POINT ( 'NONE',  ( 9.221442873511705329, -11.63200860059268393, -60.95899765791760672 ) ) ;
#48836 = CARTESIAN_POINT ( 'NONE',  ( 71.33393739769650210, 1.396834109478129804, -61.06337307536569625 ) ) ;
#48837 = CARTESIAN_POINT ( 'NONE',  ( 56.37928484793929584, -47.94447020180829355, -48.46568738789210329 ) ) ;
#48838 = CARTESIAN_POINT ( 'NONE',  ( 9.752391369101644614, -17.94198506269301774, -67.34148719073695588 ) ) ;
#48839 = CARTESIAN_POINT ( 'NONE',  ( 46.25525774125586054, 2.762490711761019568, -54.56299356781535437 ) ) ;
#48840 = CARTESIAN_POINT ( 'NONE',  ( 17.28435301021069748, -52.93377250084219554, -76.14999999999999147 ) ) ;
#48841 = DIRECTION ( 'NONE',  ( 0.000000000000000000, 0.000000000000000000, -1.000000000000000000 ) ) ;
#48842 = FACE_OUTER_BOUND ( 'NONE', #30631, .T. ) ;
#48843 = DIRECTION ( 'NONE',  ( 0.000000000000000000, -1.000000000000000000, 0.000000000000000000 ) ) ;
#48844 = ORIENTED_EDGE ( 'NONE', *, *, #25101, .F. ) ;
#48845 = CARTESIAN_POINT ( 'NONE',  ( 34.13393739769599478, 17.88381105532079829, -35.14999999999999858 ) ) ;
#48846 = CARTESIAN_POINT ( 'NONE',  ( 10.14833759260570112, 32.09291264738480010, -45.99364918638399757 ) ) ;
#48847 = CYLINDRICAL_SURFACE ( 'NONE', #4195, 0.4999999999999994449 ) ;
#48848 = CARTESIAN_POINT ( 'NONE',  ( 13.34706694256989756, -8.327013639518519028, -81.23899999999999011 ) ) ;
#48849 = EDGE_LOOP ( 'NONE', ( #34849, #3024, #5851, #1992, #39576, #45711, #5834, #3599 ) ) ;
#48850 = CARTESIAN_POINT ( 'NONE',  ( 17.88374330215040331, 20.42705216602020357, -75.51240970683940645 ) ) ;
#48851 = VERTEX_POINT ( 'NONE', #17334 ) ;
#48852 = ORIENTED_EDGE ( 'NONE', *, *, #37263, .T. ) ;
#48853 = VECTOR ( 'NONE', #27871, 1000.000000000000000 ) ;
#48854 = ORIENTED_EDGE ( 'NONE', *, *, #18086, .T. ) ;
#48855 = CARTESIAN_POINT ( 'NONE',  ( 10.98852721706949964, -64.64787429366180049, -46.31523117561389569 ) ) ;
#48856 = CARTESIAN_POINT ( 'NONE',  ( 57.21760545298290879, -45.83745218208000693, -26.25839754709659957 ) ) ;
#48857 = CARTESIAN_POINT ( 'NONE',  ( 20.43018706615270119, -21.07797482358570207, -81.23899999999999011 ) ) ;
#48858 = CARTESIAN_POINT ( 'NONE',  ( 61.68928001772049896, 13.92480326227030041, -46.77635756133729927 ) ) ;
#48859 = B_SPLINE_CURVE_WITH_KNOTS ( 'NONE', 3,
 ( #33, #43541, #43032, #15502, #7891, #35142, #23838, #3707, #39860, #51401 ),
 .UNSPECIFIED., .F., .F.,
 ( 4, 2, 2, 2, 4 ),
 ( 0.000000000000000000, 0.2484741911312051410, 0.3727112866968076976, 0.4348298344796093229, 0.4969483822624109481 ),
 .UNSPECIFIED. ) ;
#48860 = ORIENTED_EDGE ( 'NONE', *, *, #3260, .F. ) ;
#48861 = ORIENTED_EDGE ( 'NONE', *, *, #26587, .F. ) ;
#48862 = CARTESIAN_POINT ( 'NONE',  ( 14.34417029198879945, -52.11618894467940066, -76.14999999999999147 ) ) ;
#48863 = ORIENTED_EDGE ( 'NONE', *, *, #3144, .T. ) ;
#48864 = CARTESIAN_POINT ( 'NONE',  ( 11.23834934692502152, -64.16154010852214640, -24.08812103644450886 ) ) ;
#48865 = EDGE_CURVE ( 'NONE', #16787, #49612, #33298, .T. ) ;
#48866 = CARTESIAN_POINT ( 'NONE',  ( 19.28172483834588391, 18.60725077530870664, -82.44267625235052321 ) ) ;
#48867 = CARTESIAN_POINT ( 'NONE',  ( 9.446522296386651973, -55.05387195732045313, -46.46219560139201121 ) ) ;
#48868 = ORIENTED_EDGE ( 'NONE', *, *, #47979, .F. ) ;
#48869 = EDGE_CURVE ( 'NONE', #50553, #34442, #25125, .T. ) ;
#48870 = VECTOR ( 'NONE', #18840, 1000.000000000000114 ) ;
#48871 = ORIENTED_EDGE ( 'NONE', *, *, #25566, .T. ) ;
#48872 = EDGE_CURVE ( 'NONE', #25645, #6190, #22410, .T. ) ;
#48873 = DIRECTION ( 'NONE',  ( 0.000000000000000000, 0.000000000000000000, 1.000000000000000000 ) ) ;
#48875 = FACE_OUTER_BOUND ( 'NONE', #40916, .T. ) ;
#48874 = AXIS2_PLACEMENT_3D ( 'NONE', #42607, #15339, #38681 ) ;
#48876 = DIRECTION ( 'NONE',  ( 0.000000000000000000, 1.000000000000000000, 0.000000000000000000 ) ) ;
#48877 = EDGE_CURVE ( 'NONE', #260, #37257, #44585, .T. ) ;
#48878 = CARTESIAN_POINT ( 'NONE',  ( 54.71777084300830296, 14.38502104920799951, -15.43676058607329971 ) ) ;
#48879 = CARTESIAN_POINT ( 'NONE',  ( 18.20465300147069243, -23.32127884851029620, -68.20899677301083841 ) ) ;
#48880 = CARTESIAN_POINT ( 'NONE',  ( -5.330649352083970172, 15.78836655736939854, -4.865133846375759852 ) ) ;
#48881 = CARTESIAN_POINT ( 'NONE',  ( 7.530128794764829436, -59.71029400208423965, -11.77223857309723876 ) ) ;
#48882 = EDGE_CURVE ( 'NONE', #45245, #23772, #14263, .T. ) ;
#48883 = CARTESIAN_POINT ( 'NONE',  ( 55.91595795151388160, 14.67227240940072619, -17.77972436534847489 ) ) ;
#48884 = CARTESIAN_POINT ( 'NONE',  ( 12.19403623553569993, -22.40323005370389708, -69.95492400788630505 ) ) ;
#48885 = ORIENTED_EDGE ( 'NONE', *, *, #50483, .T. ) ;
#48886 = CARTESIAN_POINT ( 'NONE',  ( 60.31639983755090384, 14.60307186445300154, -47.65366050515999774 ) ) ;
#48887 = CIRCLE ( 'NONE', #7031, 20.00000000000000355 ) ;
#48888 = CARTESIAN_POINT ( 'NONE',  ( -9.460678678543580133, -42.97416197475250499, -4.641705569678379106 ) ) ;
#48889 = CARTESIAN_POINT ( 'NONE',  ( 12.91457160164050144, 34.27847415573319978, -47.58661663221230498 ) ) ;
#48890 = PRODUCT_DEFINITION_CONTEXT ( 'detailed design', #33465, 'design' ) ;
#48892 = ADVANCED_FACE ( 'NONE', ( #8691 ), #40395, .T. ) ;
#48891 = CARTESIAN_POINT ( 'NONE',  ( 72.25791598168270014, 1.028300555801489935, -70.00885842708049722 ) ) ;
#48893 = CIRCLE ( 'NONE', #43871, 12.00000000000000000 ) ;
#48894 = CARTESIAN_POINT ( 'NONE',  ( 40.87754521028758603, -39.63528059274995741, -81.74477356559056318 ) ) ;
#48895 = CARTESIAN_POINT ( 'NONE',  ( 9.367509130462650546, -15.61619940421079988, -51.84717978381009118 ) ) ;
#48896 = CARTESIAN_POINT ( 'NONE',  ( 72.98949351566130872, 0.9150552061895679268, -69.17495778280330399 ) ) ;
#48897 = CARTESIAN_POINT ( 'NONE',  ( 13.73527021832360084, 18.97497658011020150, -20.93080062246889739 ) ) ;
#48898 = CARTESIAN_POINT ( 'NONE',  ( 47.18058539754699865, 23.56890317375210131, -74.36261486341250304 ) ) ;
#48899 = CARTESIAN_POINT ( 'NONE',  ( 49.29272341951170233, -53.68831444397299890, -54.48007718848410263 ) ) ;
#48900 = CARTESIAN_POINT ( 'NONE',  ( 52.10267380154080286, -33.11618894367330057, -20.65000000000000213 ) ) ;
#48901 = CIRCLE ( 'NONE', #32968, 0.9999999999999964473 ) ;
#48902 = CARTESIAN_POINT ( 'NONE',  ( 23.14749236991919901, -19.39874071289914781, -33.66528814357884158 ) ) ;
#48903 = CARTESIAN_POINT ( 'NONE',  ( 14.63393739769620083, -42.11618894467930119, -34.64999999999999858 ) ) ;
#48904 = CARTESIAN_POINT ( 'NONE',  ( 57.20485010882750743, 13.88381105532070059, -16.39258517501439982 ) ) ;
#48905 = ORIENTED_EDGE ( 'NONE', *, *, #6688, .T. ) ;
#48906 = CIRCLE ( 'NONE', #31294, 1.999999999999999778 ) ;
#48907 = CARTESIAN_POINT ( 'NONE',  ( 9.582260743677990078, -19.16333249400659966, -43.90938957849540003 ) ) ;
#48908 = B_SPLINE_CURVE_WITH_KNOTS ( 'NONE', 3,
 ( #25302, #29503, #10380, #17718, #33941, #18494, #42348, #37377, #45249, #33686, #38156, #34464, #50474, #49704, #26080, #41307, #5416, #1479, #17974, #49958, #13543, #30008, #10124, #17464, #49449, #9606, #25559, #6191 ),
 .UNSPECIFIED., .F., .F.,
 ( 4, 2, 1, 1, 1, 1, 2, 2, 2, 2, 2, 2, 2, 2, 2, 4 ),
 ( 0.5000038014739186520, 0.5004920790115416906, 0.5009803565491648403, 0.5019569116244110285, 0.5039100217749037380, 0.5078162420758888240, 0.5156286826778588850, 0.5312535638817990069, 0.5625033262896789177, 0.6250028511054390723, 0.6875023759211991159, 0.7500019007369591595, 0.8125014255527194251, 0.8750009503684796908, 0.9375004751842397344, 1.000000000000000000 ),
 .UNSPECIFIED. ) ;
#48909 = CARTESIAN_POINT ( 'NONE',  ( 64.18198399913551100, 1.185470598955730148, -61.17336506280369690 ) ) ;
#48910 = EDGE_LOOP ( 'NONE', ( #50572, #20539, #22197, #15649 ) ) ;
#48911 = CARTESIAN_POINT ( 'NONE',  ( 22.90100569266936148, -15.61618883250986300, -34.84718217067427304 ) ) ;
#48912 = CARTESIAN_POINT ( 'NONE',  ( 61.03746773581080021, -45.60543099132259925, -47.65219250438730825 ) ) ;
#48913 = CARTESIAN_POINT ( 'NONE',  ( 23.52343111712034585, 17.71880458988573892, -34.77532226276709793 ) ) ;
#48914 = CARTESIAN_POINT ( 'NONE',  ( 50.95182575631829991, 19.71852405838109945, -76.14999999999999147 ) ) ;
#48916 = CARTESIAN_POINT ( 'NONE',  ( 20.11804734517991022, -22.52872490663017757, -78.12566274994264859 ) ) ;
#48915 = CARTESIAN_POINT ( 'NONE',  ( 43.98637686555271387, 8.721229771107395834, -66.72543627791436904 ) ) ;
#48917 = EDGE_CURVE ( 'NONE', #5478, #6259, #4490, .T. ) ;
#48918 = CARTESIAN_POINT ( 'NONE',  ( 21.77263034913930184, -11.37971624043620089, -60.64207792345899151 ) ) ;
#48919 = CARTESIAN_POINT ( 'NONE',  ( -21.36606260230379917, -53.11618894467930119, 16.35000000000000142 ) ) ;
#48920 = ORIENTED_EDGE ( 'NONE', *, *, #30622, .T. ) ;
#48921 = CARTESIAN_POINT ( 'NONE',  ( 83.47359158205320284, -45.21853209118459915, -47.48415154309300590 ) ) ;
#48922 = ORIENTED_EDGE ( 'NONE', *, *, #17468, .T. ) ;
#48923 = ORIENTED_EDGE ( 'NONE', *, *, #51114, .F. ) ;
#48924 = VERTEX_POINT ( 'NONE', #1079 ) ;
#48925 = CARTESIAN_POINT ( 'NONE',  ( 61.75020040397059518, -45.11618894740859531, -46.37192837855609895 ) ) ;
#48926 = CARTESIAN_POINT ( 'NONE',  ( 8.223571189834400386, -15.61612039429540033, -78.79233150823698395 ) ) ;
#48927 = CARTESIAN_POINT ( 'NONE',  ( 76.44636440943230582, -6.604755038381281196, -12.99629449306532258 ) ) ;
#48928 = CARTESIAN_POINT ( 'NONE',  ( 55.95663929814069348, -50.71146718310139789, -52.90773913244279214 ) ) ;
#48929 = ORIENTED_EDGE ( 'NONE', *, *, #2459, .F. ) ;
#48930 = ORIENTED_EDGE ( 'NONE', *, *, #32314, .T. ) ;
#48931 = CARTESIAN_POINT ( 'NONE',  ( 15.09828469353879044, -23.52717631300025403, -56.04926988608728067 ) ) ;
#48932 = CARTESIAN_POINT ( 'NONE',  ( 23.51915272595648432, -12.68635589971720457, -77.38738348931531164 ) ) ;
#48933 = CARTESIAN_POINT ( 'NONE',  ( 82.75389963950189554, 14.36256073625980001, -47.67227237920639737 ) ) ;
#48934 = CARTESIAN_POINT ( 'NONE',  ( 16.13393739769620083, -15.61618894467929941, 14.62639320225000006 ) ) ;
#48935 = CARTESIAN_POINT ( 'NONE',  ( 19.54197002857337040, -9.703302158787252552, -36.11948505536842191 ) ) ;
#48936 = CARTESIAN_POINT ( 'NONE',  ( 16.13393739769620083, -15.61618894467929941, -10.44999999999999929 ) ) ;
#48937 = CYLINDRICAL_SURFACE ( 'NONE', #19227, 5.499999999999998224 ) ;
#48938 = ORIENTED_EDGE ( 'NONE', *, *, #46440, .F. ) ;
#48939 = CARTESIAN_POINT ( 'NONE',  ( 8.900684698812471041, -48.14181044607449422, -48.24693240290979190 ) ) ;
#48940 = CARTESIAN_POINT ( 'NONE',  ( 62.99574006268588988, -29.46349362153740259, -16.20168838671330036 ) ) ;
#48941 = CARTESIAN_POINT ( 'NONE',  ( 14.25914812751957506, -32.49681002921884954, -34.81767276520687915 ) ) ;
#48942 = AXIS2_PLACEMENT_3D ( 'NONE', #36353, #32403, #12528 ) ;
#48943 = EDGE_CURVE ( 'NONE', #9734, #27459, #40654, .T. ) ;
#48944 = CARTESIAN_POINT ( 'NONE',  ( 21.87691169841230021, -10.26782529091599905, -65.77381455205440375 ) ) ;
#48945 = CARTESIAN_POINT ( 'NONE',  ( 66.10673863877181589, -15.61618894467929941, -16.72118890776879852 ) ) ;
#48946 = CARTESIAN_POINT ( 'NONE',  ( 14.13393739769640156, 10.38381105532060111, -35.14999999999999858 ) ) ;
#48947 = VECTOR ( 'NONE', #42049, 1000.000000000000000 ) ;
#48948 = CARTESIAN_POINT ( 'NONE',  ( 43.13712996743589656, -43.01636457780150380, -4.491635650860489548 ) ) ;
#48949 = CARTESIAN_POINT ( 'NONE',  ( 47.18325654339099628, 23.57487866773040253, -54.61058579560449289 ) ) ;
#48950 = CARTESIAN_POINT ( 'NONE',  ( 68.13393739769790614, -49.95860450174320277, -71.35146707679190570 ) ) ;
#48951 = CARTESIAN_POINT ( 'NONE',  ( 53.48663704682130771, 18.10898805450162641, -49.00013169075777597 ) ) ;
#48952 = CARTESIAN_POINT ( 'NONE',  ( 64.14219431282829476, 1.270921660756489935, -70.04197312588519253 ) ) ;
#48953 = CARTESIAN_POINT ( 'NONE',  ( 18.12477645186772079, -52.38391192226545456, -75.82251645564105047 ) ) ;
#48954 = CARTESIAN_POINT ( 'NONE',  ( 66.48976749052368973, 0.09766644518992799451, -17.32442665463599951 ) ) ;
#48955 = EDGE_LOOP ( 'NONE', ( #7020, #1205, #31398, #15736 ) ) ;
#48956 = CARTESIAN_POINT ( 'NONE',  ( 14.44096052350820081, -51.53888401296669741, -75.38689171750549178 ) ) ;
#48957 = CARTESIAN_POINT ( 'NONE',  ( 47.35766191916879819, -54.68311227971920374, -54.77973256522179923 ) ) ;
#48958 = CYLINDRICAL_SURFACE ( 'NONE', #28048, 7.910999999999997812 ) ;
#48959 = FACE_OUTER_BOUND ( 'NONE', #34197, .T. ) ;
#48960 = CARTESIAN_POINT ( 'NONE',  ( 24.04463300525956981, -15.61618495692933273, -55.50767188603018809 ) ) ;
#48961 = CARTESIAN_POINT ( 'NONE',  ( 23.37822663296399739, -17.15971063053670065, -32.14999999999999858 ) ) ;
#48962 = CARTESIAN_POINT ( 'NONE',  ( 55.63793626104714463, -45.97093497612764423, -16.89987028075756825 ) ) ;
#48963 = CARTESIAN_POINT ( 'NONE',  ( 8.133937397696213267, -59.85907068714528378, -21.15000000000000213 ) ) ;
#48964 = CIRCLE ( 'NONE', #46472, 9.000000000000007105 ) ;
#48966 = CARTESIAN_POINT ( 'NONE',  ( 11.31889512729030045, 33.13089011102178461, -24.04922472088885499 ) ) ;
#48965 = CARTESIAN_POINT ( 'NONE',  ( 13.68997053917030016, 20.12589560518139820, -23.13969474027650364 ) ) ;
#48967 = CARTESIAN_POINT ( 'NONE',  ( 9.366365007129969555, -15.61616877484880028, -59.84717978381009118 ) ) ;
#48968 = CARTESIAN_POINT ( 'NONE',  ( -30.36606260230379917, 21.88381105532059934, 16.35000000000000142 ) ) ;
#48969 = CARTESIAN_POINT ( 'NONE',  ( 48.76071015510490270, 22.82394617647319990, -55.20190746668970405 ) ) ;
#48970 = VERTEX_POINT ( 'NONE', #45372 ) ;
#48971 = CARTESIAN_POINT ( 'NONE',  ( 19.72595728692159867, -21.68578137661910077, -63.17708371749489515 ) ) ;
#48972 = ORIENTED_EDGE ( 'NONE', *, *, #42774, .F. ) ;
#48973 = CARTESIAN_POINT ( 'NONE',  ( 18.45989064939156421, -52.11463163841762736, -75.47165350116151217 ) ) ;
#48974 = CARTESIAN_POINT ( 'NONE',  ( 0.4142048468712421494, -22.38257968772852635, -35.10658870009286403 ) ) ;
#48976 = CARTESIAN_POINT ( 'NONE',  ( 53.35110984091899411, 17.85830479598100240, -27.09316622667170193 ) ) ;
#48975 = CARTESIAN_POINT ( 'NONE',  ( 84.12790934798559306, 12.74340675664220157, -46.91176635807769912 ) ) ;
#48977 = EDGE_CURVE ( 'NONE', #29501, #2815, #34587, .T. ) ;
#48978 = CARTESIAN_POINT ( 'NONE',  ( 20.66817066224499655, -10.21403313433049931, -70.17508691053730274 ) ) ;
#48979 = CARTESIAN_POINT ( 'NONE',  ( 10.97564820803404828, 33.77114500669411967, -17.33480536923671167 ) ) ;
#48980 = CARTESIAN_POINT ( 'NONE',  ( 57.41961354596299572, -45.11618894467940066, -17.68838722488590065 ) ) ;
#48981 = B_SPLINE_SURFACE_WITH_KNOTS ( 'NONE', 3, 3, ( 
 ( #22943, #51269, #34489, #15366, #14585, #26620, #38962, #42637, #2798 ),
 ( #30808, #31321, #51523, #39210, #35535, #18515, #11181, #11443, #3575 ),
 ( #50494, #22689, #35270, #34742, #15624, #3055, #19025, #47596, #35001 ),
 ( #46836, #18770, #2536, #30551, #51009, #7502, #31575, #11696, #46575 ),
 ( #10922, #27401, #27658, #43402, #26886, #19289, #23450, #43659, #39475 ),
 ( #31066, #38708, #10664, #7764, #42896, #38436, #50749, #27147, #14845 ),
 ( #6991, #15105, #47092, #43151, #7246, #23194, #3311, #20047, #32860 ),
 ( #11956, #40240, #147, #35792, #4853, #40491, #44429, #8532, #48891 ),
 ( #32342, #16639, #8263, #24478, #656, #28164, #36815, #23963, #3828 ),
 ( #12994, #44949, #920, #24741, #48361, #16915, #47850, #20819, #28944 ),
 ( #32600, #44168, #4584, #20555, #31833, #23712, #39725, #36552, #48627 ),
 ( #12727, #39984, #400, #19802, #28682, #4076, #4332, #44685, #51774 ),
 ( #24216, #12205, #48106, #20300, #8789, #16125, #15879, #40752, #32086 ),
 ( #36290, #27913, #36039, #16386, #43914, #8009, #12456, #28426, #1961 ),
 ( #1181, #13511, #49414, #33395, #29465, #41786, #42053, #37083, #45470 ),
 ( #17429, #26042, #37864, #37342, #37589, #14013, #13760, #21338, #1443 ),
 ( #22112, #9828, #6155, #41015, #33655, #17937, #38123, #29973, #21080 ),
 ( #5893, #5381, #2218, #9570, #25524, #18196, #41528, #21857, #5645 ),
 ( #24997, #17176, #21591, #45991, #34160, #50175, #33128, #30239, #1702 ),
 ( #14273, #49922, #17684, #33907, #10084, #9049, #5127, #49671, #29718 ) ),
 .UNSPECIFIED., .F., .F., .F.,
 ( 4, 2, 2, 2, 2, 2, 2, 2, 2, 4 ),
 ( 4, 1, 1, 1, 1, 1, 4 ),
 ( -1.826192301619919967, -1.664708266407020076, -1.413116924488160064, -1.141370188512450090, -0.9130961508099589841, -0.7989591319587140417, -0.6163399017967220450, -0.3681920442832050111, -0.1161770321783029969, 0.000000000000000000 ),
 ( 0.000000000000000000, 0.1666666666666670182, 0.3333333333333329818, 0.5000000000000000000, 0.6666666666666670737, 0.8333333333333330373, 1.000000000000000000 ),
 .UNSPECIFIED. ) ;
#48982 = DIRECTION ( 'NONE',  ( 0.000000000000000000, 0.000000000000000000, -1.000000000000000000 ) ) ;
#48983 = ADVANCED_FACE ( 'NONE', ( #50073 ), #18347, .T. ) ;
#48984 = EDGE_LOOP ( 'NONE', ( #24959, #37374, #31079, #30522 ) ) ;
#48985 = VERTEX_POINT ( 'NONE', #10762 ) ;
#48986 = EDGE_CURVE ( 'NONE', #31691, #50433, #12393, .T. ) ;
#48987 = CARTESIAN_POINT ( 'NONE',  ( 11.79626796993740001, -64.91451392858408553, -16.32611600088480230 ) ) ;
#48988 = CARTESIAN_POINT ( 'NONE',  ( 11.16916691016460028, 32.84040665082629573, -44.61689804176330654 ) ) ;
#48989 = DIRECTION ( 'NONE',  ( -0.7226652920947586045, -0.6911981449639438280, 0.000000000000000000 ) ) ;
#48990 = CARTESIAN_POINT ( 'NONE',  ( 51.50963138327329460, -50.97627007566619994, -50.14470441323439331 ) ) ;
#48991 = CARTESIAN_POINT ( 'NONE',  ( 51.67587649748470113, 2.735120682347050192, -77.01363636363508647 ) ) ;
#48992 = ORIENTED_EDGE ( 'NONE', *, *, #46320, .T. ) ;
#48993 = CARTESIAN_POINT ( 'NONE',  ( 24.04466642925503095, -15.61618863334376250, -55.79233649161735542 ) ) ;
#48994 = DIRECTION ( 'NONE',  ( 0.000000000000000000, 1.000000000000000000, 0.000000000000000000 ) ) ;
#48995 = CARTESIAN_POINT ( 'NONE',  ( 68.13393739769618662, 0.9838110553206419473, -65.65000000000000568 ) ) ;
#48996 = LINE ( 'NONE', #8894, #25831 ) ;
#48997 = CARTESIAN_POINT ( 'NONE',  ( 50.62459508413220277, -49.95149871030799460, -76.16377488398599382 ) ) ;
#48998 = DIRECTION ( 'NONE',  ( -1.000000000000000000, 0.000000000000000000, 0.000000000000000000 ) ) ;
#48999 = ORIENTED_EDGE ( 'NONE', *, *, #14896, .T. ) ;
#49000 = FACE_OUTER_BOUND ( 'NONE', #42384, .T. ) ;
#49001 = FACE_OUTER_BOUND ( 'NONE', #21213, .T. ) ;
#49002 = ORIENTED_EDGE ( 'NONE', *, *, #7118, .F. ) ;
#49003 = CARTESIAN_POINT ( 'NONE',  ( 56.22026493956754933, -50.82405358938415674, -74.67349521025255399 ) ) ;
#49004 = DIRECTION ( 'NONE',  ( -1.000000000000000000, 0.000000000000000000, 0.000000000000000000 ) ) ;
#49005 = ADVANCED_FACE ( 'NONE', ( #34063 ), #45624, .F. ) ;
#49006 = CARTESIAN_POINT ( 'NONE',  ( 13.52049491622099886, -8.034853201522141219, -81.18618737929101314 ) ) ;
#49007 = AXIS2_PLACEMENT_3D ( 'NONE', #23440, #39972, #15862 ) ;
#49008 = CARTESIAN_POINT ( 'NONE',  ( 13.68007965596629916, -51.36715864978960155, -22.99348026275350065 ) ) ;
#49009 = DIRECTION ( 'NONE',  ( 0.000000000000000000, 0.000000000000000000, -1.000000000000000000 ) ) ;
#49010 = CARTESIAN_POINT ( 'NONE',  ( 47.33318413658150092, -54.47214429496199983, -75.00321679105040573 ) ) ;
#49011 = ORIENTED_EDGE ( 'NONE', *, *, #47384, .T. ) ;
#49012 = CARTESIAN_POINT ( 'NONE',  ( 55.26140197345470284, 14.75560134660129918, -16.31640509964899977 ) ) ;
#49013 = CIRCLE ( 'NONE', #3813, 0.9999999999999964473 ) ;
#49014 = B_SPLINE_CURVE_WITH_KNOTS ( 'NONE', 3,
 ( #37559, #9541, #5609, #21563 ),
 .UNSPECIFIED., .F., .F.,
 ( 4, 4 ),
 ( 0.000000000000000000, 1.000000000000000000 ),
 .UNSPECIFIED. ) ;
#49015 = CARTESIAN_POINT ( 'NONE',  ( 20.16990914961741055, -9.832289637797707371, -46.54110819413472200 ) ) ;
#49016 = DIRECTION ( 'NONE',  ( -1.000000000000000000, 0.000000000000000000, 0.000000000000000000 ) ) ;
#49017 = CARTESIAN_POINT ( 'NONE',  ( 68.13393739769618662, -0.1661889446793599900, -31.09383709942130380 ) ) ;
#49018 = VERTEX_POINT ( 'NONE', #22011 ) ;
#49019 = CARTESIAN_POINT ( 'NONE',  ( 47.44054024740749753, 23.27512645068789610, -74.80705470093730014 ) ) ;
#49020 = DIRECTION ( 'NONE',  ( 0.3918900565003997638, 0.9200120562341090880, -1.214306433184117618E-13 ) ) ;
#49021 = CARTESIAN_POINT ( 'NONE',  ( 16.13393739769620083, -15.61618894467929941, -1.149999999999999911 ) ) ;
#49022 = CARTESIAN_POINT ( 'NONE',  ( 28.63393739769619728, -4.678675331415849570, -34.64999999999999858 ) ) ;
#49023 = CARTESIAN_POINT ( 'NONE',  ( 52.10267380154080286, -33.11618894367330057, -20.65000000000000213 ) ) ;
#49024 = CARTESIAN_POINT ( 'NONE',  ( 83.89200044194980421, -50.09049722508079583, -52.57651812407429759 ) ) ;
#49025 = FACE_OUTER_BOUND ( 'NONE', #50981, .T. ) ;
#49026 = CARTESIAN_POINT ( 'NONE',  ( 43.34618191712553426, -39.98291268152190980, -69.47739009628490692 ) ) ;
#49027 = CARTESIAN_POINT ( 'NONE',  ( 61.24618047107790630, 14.01894199962020160, -46.62624509076869828 ) ) ;
#49028 = CARTESIAN_POINT ( 'NONE',  ( 12.76594342643529956, -64.30274611092340820, -45.89070534480079999 ) ) ;
#49029 = ORIENTED_EDGE ( 'NONE', *, *, #19205, .T. ) ;
#49030 = CARTESIAN_POINT ( 'NONE',  ( 53.01430333496330860, -49.56473660178939866, -48.82220832852659953 ) ) ;
#49031 = DIRECTION ( 'NONE',  ( 1.000000000000000000, 0.000000000000000000, 0.000000000000000000 ) ) ;
#49032 = CARTESIAN_POINT ( 'NONE',  ( 8.428884743720756134, -17.68704076488086230, -74.70899817588775704 ) ) ;
#49033 = CARTESIAN_POINT ( 'NONE',  ( 56.04052241335789830, 14.81222946749389990, -25.92335767470229868 ) ) ;
#49034 = CARTESIAN_POINT ( 'NONE',  ( 23.56842915955159867, -16.10099296214760400, -80.25338504615679369 ) ) ;
#49035 = CARTESIAN_POINT ( 'NONE',  ( 51.25913404859330313, 18.70661076787169819, -76.33308050540989598 ) ) ;
#49036 = CARTESIAN_POINT ( 'NONE',  ( 53.46721369579029925, 18.16710752707049892, -49.11454780549119903 ) ) ;
#49037 = CARTESIAN_POINT ( 'NONE',  ( 71.36689417337970553, 0.9219904752505979628, -70.70458949289690054 ) ) ;
#49038 = FACE_OUTER_BOUND ( 'NONE', #42986, .T. ) ;
#49039 = CARTESIAN_POINT ( 'NONE',  ( 46.40621397443668172, 21.74426215006149121, -76.14873014702847343 ) ) ;
#49040 = EDGE_CURVE ( 'NONE', #13057, #4375, #30135, .T. ) ;
#49041 = VERTEX_POINT ( 'NONE', #18609 ) ;
#49042 = CARTESIAN_POINT ( 'NONE',  ( 23.42904929335390207, -14.10356315877740130, -71.00226400225309931 ) ) ;
#49043 = ORIENTED_EDGE ( 'NONE', *, *, #30028, .F. ) ;
#49044 = EDGE_CURVE ( 'NONE', #49799, #20360, #7396, .T. ) ;
#49045 = CARTESIAN_POINT ( 'NONE',  ( 72.86255183691179127, 1.369664981662529923, -68.74641178933899255 ) ) ;
#49046 = CARTESIAN_POINT ( 'NONE',  ( 47.38650124322969504, -54.66575521192519460, -54.85296598789229705 ) ) ;
#49047 = CARTESIAN_POINT ( 'NONE',  ( 21.93491326470667602, -10.21990321164456006, -49.55383906828567575 ) ) ;
#49048 = CARTESIAN_POINT ( 'NONE',  ( 72.82769086651219936, 1.383811055320669947, -62.77287342953649585 ) ) ;
#49049 = CARTESIAN_POINT ( 'NONE',  ( 56.58402530372350014, 19.32354596816890080, -53.00599679597699776 ) ) ;
#49050 = CARTESIAN_POINT ( 'NONE',  ( 71.35346284499661351, 1.390806392144110060, -61.03748192468230371 ) ) ;
#49051 = FACE_BOUND ( 'NONE', #47006, .T. ) ;
#49052 = CARTESIAN_POINT ( 'NONE',  ( 72.23784989528050460, 1.054781932184780002, -61.27250974618609547 ) ) ;
#49053 = CARTESIAN_POINT ( 'NONE',  ( 17.16939886808665960, -23.52720133053026075, -71.96594023329781464 ) ) ;
#49054 = CARTESIAN_POINT ( 'NONE',  ( 65.04142308672740569, 1.102581332775290024, -70.73820378408520071 ) ) ;
#49055 = ORIENTED_EDGE ( 'NONE', *, *, #7860, .T. ) ;
#49056 = EDGE_LOOP ( 'NONE', ( #8818, #12198, #7164, #33211 ) ) ;
#49057 = CARTESIAN_POINT ( 'NONE',  ( 8.958479335714679692, -63.16393755107500851, -46.63341780269549730 ) ) ;
#49058 = AXIS2_PLACEMENT_3D ( 'NONE', #43405, #19030, #28166 ) ;
#49059 = DIRECTION ( 'NONE',  ( 1.000000000000000000, 2.460964292799963328E-14, 0.000000000000000000 ) ) ;
#49060 = ORIENTED_EDGE ( 'NONE', *, *, #29699, .F. ) ;
#49061 = FACE_OUTER_BOUND ( 'NONE', #9551, .T. ) ;
#49062 = FACE_OUTER_BOUND ( 'NONE', #15892, .T. ) ;
#49063 = CYLINDRICAL_SURFACE ( 'NONE', #9442, 0.4999999999999967248 ) ;
#49064 = CARTESIAN_POINT ( 'NONE',  ( 51.83314622386949821, 18.96308757159359715, -76.51145678373148939 ) ) ;
#49065 = ORIENTED_EDGE ( 'NONE', *, *, #18092, .F. ) ;
#49066 = FACE_OUTER_BOUND ( 'NONE', #43163, .T. ) ;
#49068 = CARTESIAN_POINT ( 'NONE',  ( 41.69553807872770079, 6.341659931880261780, -81.84199659484330880 ) ) ;
#49067 = AXIS2_PLACEMENT_3D ( 'NONE', #36737, #44613, #41455 ) ;
#49069 = CARTESIAN_POINT ( 'NONE',  ( 8.222598545279129922, -15.61602001634830117, -66.50766849176299900 ) ) ;
#49070 = ADVANCED_FACE ( 'NONE', ( #7091 ), #42044, .T. ) ;
#49071 = CARTESIAN_POINT ( 'NONE',  ( 18.34740929417809951, -23.55868617284500033, -56.20581778389630045 ) ) ;
#49072 = AXIS2_PLACEMENT_3D ( 'NONE', #7382, #35921, #4211 ) ;
#49073 = CARTESIAN_POINT ( 'NONE',  ( 19.73841138675414442, -9.822567584297365428, -56.13025822577677815 ) ) ;
#49074 = CARTESIAN_POINT ( 'NONE',  ( 43.17225766068933979, -37.80304688360283194, -74.45836467289994687 ) ) ;
#49075 = ADVANCED_FACE ( 'NONE', ( #37626 ), #49699, .T. ) ;
#49076 = EDGE_LOOP ( 'NONE', ( #3862, #32689, #28855, #19458 ) ) ;
#49077 = CARTESIAN_POINT ( 'NONE',  ( 10.87442115971020051, -64.65679685997820059, -23.33560984931219906 ) ) ;
#49078 = CARTESIAN_POINT ( 'NONE',  ( 9.522216423340641001, -19.05011374909959798, -45.08017965390989445 ) ) ;
#49079 = VECTOR ( 'NONE', #6741, 1000.000000000000000 ) ;
#49080 = CARTESIAN_POINT ( 'NONE',  ( 9.807704732040047446, -10.75459748142696270, -32.71600059186270215 ) ) ;
#49081 = B_SPLINE_CURVE_WITH_KNOTS ( 'NONE', 3,
 ( #3818, #27899, #4064, #7997, #27135, #23184, #15612, #48092, #27391, #31567, #39714, #43393, #43142, #38950, #137, #20031, #32074, #43903, #3295, #7488, #23950, #19277, #19014, #22930, #34989, #36028, #3561, #23700 ),
 .UNSPECIFIED., .F., .F.,
 ( 4, 2, 2, 2, 2, 2, 2, 2, 2, 2, 1, 1, 1, 1, 2, 4 ),
 ( 0.000000000000000000, 0.06250045418902985817, 0.1250009083780597163, 0.1875013625670895467, 0.2500018167561194327, 0.3125022709451493186, 0.3750027251341790935, 0.4375031793232089794, 0.4687534064177240056, 0.4843785199649814355, 0.4921910767386101782, 0.4960973551254245217, 0.4980504943188317490, 0.4990270639155353072, 0.4995153487138871418, 0.5000036335122389763 ),
 .UNSPECIFIED. ) ;
#49082 = CARTESIAN_POINT ( 'NONE',  ( 14.58630607399789980, 20.67960354982550086, -75.75221093576881515 ) ) ;
#49083 = DIRECTION ( 'NONE',  ( 1.000000000000000000, 0.000000000000000000, 0.000000000000000000 ) ) ;
#49084 = LINE ( 'NONE', #9249, #51588 ) ;
#49085 = CARTESIAN_POINT ( 'NONE',  ( 10.78136697721919823, -21.88776853859420157, -56.23255504334029098 ) ) ;
#49086 = ORIENTED_EDGE ( 'NONE', *, *, #9506, .T. ) ;
#49087 = AXIS2_PLACEMENT_3D ( 'NONE', #46511, #7436, #19477 ) ;
#49088 = CARTESIAN_POINT ( 'NONE',  ( 52.77132806972499424, -49.69320935574780407, -28.15000000000000213 ) ) ;
#49089 =( GEOMETRIC_REPRESENTATION_CONTEXT ( 3 ) GLOBAL_UNCERTAINTY_ASSIGNED_CONTEXT ( ( #12203 ) ) GLOBAL_UNIT_ASSIGNED_CONTEXT ( ( #16920, #32603, #44431 ) ) REPRESENTATION_CONTEXT ( 'NONE', 'WORKASPACE' ) );
#49090 = CARTESIAN_POINT ( 'NONE',  ( 16.06830620277110100, -51.06210401962729861, -20.66285861647710220 ) ) ;
#49091 = CARTESIAN_POINT ( 'NONE',  ( 85.38000601716228743, -48.61618894467930119, -60.34000486924599471 ) ) ;
#49092 = CARTESIAN_POINT ( 'NONE',  ( 68.13393739823159478, -1.166188945610419969, -65.65000000186969942 ) ) ;
#49093 = CARTESIAN_POINT ( 'NONE',  ( 46.19337157655569825, 14.89803173164150074, -9.780203716366939304 ) ) ;
#49094 = ORIENTED_EDGE ( 'NONE', *, *, #38309, .F. ) ;
#49095 =( BOUNDED_CURVE ( )  B_SPLINE_CURVE ( 3, ( #51680, #35696, #31728, #43816 ),
 .UNSPECIFIED., .F., .T. ) 
 B_SPLINE_CURVE_WITH_KNOTS ( ( 4, 4 ),
 ( 3.744786642406928934, 4.166152881452140022 ),
 .UNSPECIFIED. ) 
 CURVE ( )  GEOMETRIC_REPRESENTATION_ITEM ( )  RATIONAL_B_SPLINE_CURVE ( ( 1.000000000000000000, 0.9852588556718586688, 0.9852588556718586688, 1.000000000000000000 ) ) 
 REPRESENTATION_ITEM ( '' )  );
#49096 = CARTESIAN_POINT ( 'NONE',  ( -9.094368388026579098, -44.04680377273619740, -5.580026499916369787 ) ) ;
#49097 = CARTESIAN_POINT ( 'NONE',  ( 47.23303514576589635, 23.53638779022370286, -54.67236707882319990 ) ) ;
#49098 = VECTOR ( 'NONE', #27346, 1000.000000000000000 ) ;
#49099 = LINE ( 'NONE', #21541, #37074 ) ;
#49100 = CARTESIAN_POINT ( 'NONE',  ( 63.47152504824990160, 1.384378348444510243, -62.56683295884919715 ) ) ;
#49101 = DIRECTION ( 'NONE',  ( -0.3863301728269311619, 0.9223605572461961444, 1.110223024625156171E-16 ) ) ;
#49102 = CARTESIAN_POINT ( 'NONE',  ( 11.51051956401449949, 34.11712030960200082, -17.72953785340450139 ) ) ;
#49103 = PLANE ( 'NONE',  #5186 ) ;
#49104 = CARTESIAN_POINT ( 'NONE',  ( 53.36496928958640495, 18.14812949222240235, -48.76946463831480116 ) ) ;
#49105 = CARTESIAN_POINT ( 'NONE',  ( 8.222937397696199469, -15.61618894467929941, -32.14999999999999858 ) ) ;
#49106 = CARTESIAN_POINT ( 'NONE',  ( 53.59153692563230464, -49.40734274623049771, -49.22791863457509720 ) ) ;
#49107 = AXIS2_PLACEMENT_3D ( 'NONE', #1847, #14672, #14156 ) ;
#49108 = CARTESIAN_POINT ( 'NONE',  ( 22.74532932033418930, -17.09449615818190082, -66.52281770332464816 ) ) ;
#49109 = ADVANCED_FACE ( 'NONE', ( #1732 ), #45243, .T. ) ;
#49110 = CARTESIAN_POINT ( 'NONE',  ( 53.27977303602300196, 20.78456751779900102, -53.62768324064160197 ) ) ;
#49111 = CARTESIAN_POINT ( 'NONE',  ( 20.29256129770259776, -21.02754544282699456, -60.74449963404457264 ) ) ;
#49112 = CARTESIAN_POINT ( 'NONE',  ( 10.72263364360945737, -11.45749769863363809, -47.66115396588360653 ) ) ;
#49113 = VERTEX_POINT ( 'NONE', #49954 ) ;
#49114 = DIRECTION ( 'NONE',  ( 0.000000000000000000, 0.000000000000000000, -1.000000000000000000 ) ) ;
#49115 = CARTESIAN_POINT ( 'NONE',  ( 9.297729852059489986, 32.05137213967839926, -46.53031076905089947 ) ) ;
#49116 = FACE_OUTER_BOUND ( 'NONE', #16087, .T. ) ;
#49117 = AXIS2_PLACEMENT_3D ( 'NONE', #38383, #41337, #45278 ) ;
#49118 = CARTESIAN_POINT ( 'NONE',  ( 66.54986627545559941, -30.20275677880469800, -16.95609989249500060 ) ) ;
#49119 = ORIENTED_EDGE ( 'NONE', *, *, #2722, .F. ) ;
#49120 = CARTESIAN_POINT ( 'NONE',  ( 18.33252661170309850, 20.80550406818660036, -75.55956264724760274 ) ) ;
#49121 = AXIS2_PLACEMENT_3D ( 'NONE', #31188, #7886, #3446 ) ;
#49122 = ORIENTED_EDGE ( 'NONE', *, *, #14901, .F. ) ;
#49123 = ORIENTED_EDGE ( 'NONE', *, *, #30938, .T. ) ;
#49124 = CARTESIAN_POINT ( 'NONE',  ( 47.66548848826279539, 23.29226298427809638, -55.16185052358790131 ) ) ;
#49125 = EDGE_LOOP ( 'NONE', ( #34500, #17534, #4240 ) ) ;
#49126 = CARTESIAN_POINT ( 'NONE',  ( 11.20501727608539788, -64.66700489968309284, -46.03640593563060435 ) ) ;
#49127 = CARTESIAN_POINT ( 'NONE',  ( 56.78593216331930194, -45.94738399931370054, -26.22487339609619994 ) ) ;
#49128 = CARTESIAN_POINT ( 'NONE',  ( 19.62200085763610247, -21.54020370181870092, -81.23899999999999011 ) ) ;
#49129 = CARTESIAN_POINT ( 'NONE',  ( 61.46960199815709558, 14.08860104859740048, -47.25189778830119991 ) ) ;
#49130 = DIRECTION ( 'NONE',  ( 0.000000000000000000, 1.000000000000000000, 0.000000000000000000 ) ) ;
#49131 = VERTEX_POINT ( 'NONE', #1472 ) ;
#49132 = DIRECTION ( 'NONE',  ( 0.000000000000000000, 0.000000000000000000, 1.000000000000000000 ) ) ;
#49133 = CARTESIAN_POINT ( 'NONE',  ( 12.04669066983540660, 34.10719178353053849, -17.12210551403972403 ) ) ;
#49134 = ORIENTED_EDGE ( 'NONE', *, *, #47918, .T. ) ;
#49135 = CARTESIAN_POINT ( 'NONE',  ( 50.27336491350419578, -45.97712286795240288, -12.51542028137719953 ) ) ;
#49136 = CIRCLE ( 'NONE', #36559, 36.00000000000000000 ) ;
#49137 = CARTESIAN_POINT ( 'NONE',  ( 23.86187795847609650, -17.34972413055976403, -33.86254089651572485 ) ) ;
#49138 = ADVANCED_FACE ( 'NONE', ( #21888 ), #1990, .T. ) ;
#49139 = CARTESIAN_POINT ( 'NONE',  ( 15.12242003932687062, -22.59611672426211015, -49.39298971242588721 ) ) ;
#49140 = ORIENTED_EDGE ( 'NONE', *, *, #46084, .F. ) ;
#49141 = CARTESIAN_POINT ( 'NONE',  ( 72.76779797359338886, 1.388189907116970101, -62.58632377286669879 ) ) ;
#49142 = CARTESIAN_POINT ( 'NONE',  ( 46.97440434136990461, -54.33447984715540002, -75.47461153638509757 ) ) ;
#49143 = CARTESIAN_POINT ( 'NONE',  ( 16.13393739769620083, -15.61618894467929941, 6.072546842075589701 ) ) ;
#49144 = CARTESIAN_POINT ( 'NONE',  ( 11.51160566532390028, -51.12796951774690513, -21.14999999999999858 ) ) ;
#49145 = EDGE_CURVE ( 'NONE', #31736, #29987, #32666, .T. ) ;
#49146 = CARTESIAN_POINT ( 'NONE',  ( 24.04493737374410145, -16.65173368866850367, -67.83399587179394530 ) ) ;
#49147 = CARTESIAN_POINT ( 'NONE',  ( -3.785122221975860235, 16.81208508831930004, -4.794476613499900175 ) ) ;
#49148 = CARTESIAN_POINT ( 'NONE',  ( 16.13393739769620083, -15.61618894467929941, -643.2998782751060389 ) ) ;
#49149 = VECTOR ( 'NONE', #34246, 1000.000000000000000 ) ;
#49150 = CARTESIAN_POINT ( 'NONE',  ( 58.73226909804809281, 13.89440744020959961, -25.79432472329149917 ) ) ;
#49151 = CARTESIAN_POINT ( 'NONE',  ( 15.91255700721379895, -23.46078829110179953, -69.79648614575910415 ) ) ;
#49152 = VERTEX_POINT ( 'NONE', #17460 ) ;
#49153 = CARTESIAN_POINT ( 'NONE',  ( 56.68070624494579590, 16.55316904772309883, -48.38861384420910383 ) ) ;
#49154 = CARTESIAN_POINT ( 'NONE',  ( 74.17629866868290378, 4.883811055320659733, -65.34607522167520699 ) ) ;
#49155 = CARTESIAN_POINT ( 'NONE',  ( 76.82820232143379258, -43.20601130791419564, -14.64016038542719933 ) ) ;
#49156 = FACE_OUTER_BOUND ( 'NONE', #41745, .T. ) ;
#49157 = CARTESIAN_POINT ( 'NONE',  ( 17.16950173226367582, -23.52718653585607100, -36.25066335673832185 ) ) ;
#49158 = CARTESIAN_POINT ( 'NONE',  ( 82.24889277099100582, -45.11618894467940066, -46.39515210564750447 ) ) ;
#49159 = CARTESIAN_POINT ( 'NONE',  ( 21.54527565159127533, -19.77483657756496171, -78.66115106571606930 ) ) ;
#49160 = CARTESIAN_POINT ( 'NONE',  ( 49.47752793838059659, -53.68558960755940035, -54.66603854467830104 ) ) ;
#49161 = LINE ( 'NONE', #41535, #41506 ) ;
#49162 = EDGE_CURVE ( 'NONE', #1409, #25812, #5159, .T. ) ;
#49163 = B_SPLINE_CURVE_WITH_KNOTS ( 'NONE', 3,
 ( #36271, #40218, #12438, #5108, #32066, #31814, #20537, #21063 ),
 .UNSPECIFIED., .F., .F.,
 ( 4, 2, 2, 4 ),
 ( 0.000000000000000000, 0.1059767115674661170, 0.3294825338126947112, 0.3562431257904284942 ),
 .UNSPECIFIED. ) ;
#49164 = CARTESIAN_POINT ( 'NONE',  ( 12.48460695861928649, -22.65913801891631607, -34.15979310000165015 ) ) ;
#49165 = CARTESIAN_POINT ( 'NONE',  ( 17.92366493563939756, -51.11618894649849665, -74.14993593045390696 ) ) ;
#49166 = DIRECTION ( 'NONE',  ( 0.000000000000000000, 0.000000000000000000, -1.000000000000000000 ) ) ;
#49167 = ORIENTED_EDGE ( 'NONE', *, *, #46440, .T. ) ;
#49168 = ADVANCED_FACE ( 'NONE', ( #33162 ), #36024, .T. ) ;
#49169 = CARTESIAN_POINT ( 'NONE',  ( 16.96290023960060367, -8.212168756627189481, -46.60283323465849747 ) ) ;
#49170 = EDGE_CURVE ( 'NONE', #40777, #33786, #10119, .T. ) ;
#49171 = CARTESIAN_POINT ( 'NONE',  ( 64.21673630462969129, 0.9952277120692980539, -61.10412195540050107 ) ) ;
#49172 = ORIENTED_EDGE ( 'NONE', *, *, #28559, .F. ) ;
#49173 = CARTESIAN_POINT ( 'NONE',  ( -0.02466850413057549915, -50.78713108147470479, -34.78792709637806979 ) ) ;
#49174 = CARTESIAN_POINT ( 'NONE',  ( 60.79136938041280303, -45.68357609118859841, -47.68552353186040449 ) ) ;
#49175 = DIRECTION ( 'NONE',  ( 0.000000000000000000, 0.000000000000000000, -1.000000000000000000 ) ) ;
#49176 = CARTESIAN_POINT ( 'NONE',  ( 50.08385623533860098, 18.00127108905680018, -76.14999999999999147 ) ) ;
#49178 = DIRECTION ( 'NONE',  ( 0.000000000000000000, 0.000000000000000000, 1.000000000000000000 ) ) ;
#49177 = CARTESIAN_POINT ( 'NONE',  ( 45.15723187293362884, 8.809242139076280509, -61.04885190864924027 ) ) ;
#49179 = ADVANCED_FACE ( 'NONE', ( #26594 ), #1733, .F. ) ;
#49180 = CARTESIAN_POINT ( 'NONE',  ( 53.09962450323771321, -51.41544088504546295, -75.69942452463016025 ) ) ;
#49181 = CARTESIAN_POINT ( 'NONE',  ( 18.13393739769619728, -45.61618894467940066, -62.64999999999999858 ) ) ;
#49182 = EDGE_LOOP ( 'NONE', ( #4698, #35821, #4896, #11529 ) ) ;
#49183 = VERTEX_POINT ( 'NONE', #34191 ) ;
#49184 = ORIENTED_EDGE ( 'NONE', *, *, #39577, .T. ) ;
#49185 = CARTESIAN_POINT ( 'NONE',  ( 61.52464553311489937, -45.32266663462549872, -47.25836995145800046 ) ) ;
#49186 = CARTESIAN_POINT ( 'NONE',  ( 16.13393739769620083, -15.61618894467929941, -18.58999999999999986 ) ) ;
#49187 = PRESENTATION_LAYER_ASSIGNMENT (  '', '', ( #32375 ) ) ;
#49188 = ORIENTED_EDGE ( 'NONE', *, *, #7281, .F. ) ;
#49189 = ORIENTED_EDGE ( 'NONE', *, *, #4848, .T. ) ;
#49190 = DIRECTION ( 'NONE',  ( 0.000000000000000000, 0.000000000000000000, 1.000000000000000000 ) ) ;
#49191 = ORIENTED_EDGE ( 'NONE', *, *, #13135, .T. ) ;
#49192 = CARTESIAN_POINT ( 'NONE',  ( 56.77563393123009661, 19.41451721634069827, -53.45922468568930697 ) ) ;
#49193 = CARTESIAN_POINT ( 'NONE',  ( 30.13393739769619728, 7.383811055320659733, -84.65000000000000568 ) ) ;
#49194 = CARTESIAN_POINT ( 'NONE',  ( 9.412768094977693067, -14.16268697616711059, -65.91555746443309260 ) ) ;
#49195 = CARTESIAN_POINT ( 'NONE',  ( 15.24821961686016714, -8.849179223346602896, -35.91115229312517698 ) ) ;
#49196 = EDGE_CURVE ( 'NONE', #33088, #29183, #3028, .T. ) ;
#49197 = ORIENTED_EDGE ( 'NONE', *, *, #51572, .F. ) ;
#49198 = CARTESIAN_POINT ( 'NONE',  ( 33.38393739769599478, 10.88381105532080007, -35.14999999999999858 ) ) ;
#49199 = CARTESIAN_POINT ( 'NONE',  ( 52.47790443081309775, -50.33621177253660051, -76.75890347598199526 ) ) ;
#49200 = CARTESIAN_POINT ( 'NONE',  ( 18.66534361887244486, -21.90748510045777664, -46.83103359700395174 ) ) ;
#49201 = CARTESIAN_POINT ( 'NONE',  ( 60.74510967839550091, 14.28146716509339953, -47.06535153140909244 ) ) ;
#49202 = CARTESIAN_POINT ( 'NONE',  ( 8.318366073613649547, -14.90654645034790171, -67.04131744907229518 ) ) ;
#49203 = DIRECTION ( 'NONE',  ( 0.000000000000000000, 0.000000000000000000, -1.000000000000000000 ) ) ;
#49204 = CARTESIAN_POINT ( 'NONE',  ( 42.30721679385599998, 13.79944185400150047, -6.083977230941699510 ) ) ;
#49205 = CARTESIAN_POINT ( 'NONE',  ( 42.53968774367980643, -44.23115725350800176, -5.088323970340629998 ) ) ;
#49206 = CARTESIAN_POINT ( 'NONE',  ( 72.79984470539690733, 0.9644290104360989657, -61.87674839326469822 ) ) ;
#49207 = LINE ( 'NONE', #28220, #27372 ) ;
#49208 = EDGE_CURVE ( 'NONE', #14040, #14545, #39405, .T. ) ;
#49209 = CARTESIAN_POINT ( 'NONE',  ( 63.87903507333619757, 1.407740274733980002, -69.63435796713869763 ) ) ;
#49210 = CARTESIAN_POINT ( 'NONE',  ( 20.99566151349429077, -9.290060484552283171, -41.50066443384773862 ) ) ;
#49211 = CARTESIAN_POINT ( 'NONE',  ( 65.04837026172849335, 1.029399159225240057, -17.85459962871380313 ) ) ;
#49212 = ORIENTED_EDGE ( 'NONE', *, *, #49275, .F. ) ;
#49213 = CARTESIAN_POINT ( 'NONE',  ( 14.21603903184900020, -51.93578155835659516, -75.67800190747080080 ) ) ;
#49214 = CARTESIAN_POINT ( 'NONE',  ( 57.35719032655089933, 19.00113118003429591, -52.73978338582610803 ) ) ;
#49215 = DIRECTION ( 'NONE',  ( -0.5720614028176831400, 0.4156269377774557960, -0.7071067811865470176 ) ) ;
#49216 = CARTESIAN_POINT ( 'NONE',  ( 83.84453607997100733, 13.09586255422381562, -46.66650892571503562 ) ) ;
#49217 = DIRECTION ( 'NONE',  ( 0.8090169943749475623, 0.5877852522924730261, 0.000000000000000000 ) ) ;
#49218 =( GEOMETRIC_REPRESENTATION_CONTEXT ( 3 ) GLOBAL_UNCERTAINTY_ASSIGNED_CONTEXT ( ( #23193 ) ) GLOBAL_UNIT_ASSIGNED_CONTEXT ( ( #24024, #47914, #27970 ) ) REPRESENTATION_CONTEXT ( 'NONE', 'WORKASPACE' ) );
#49219 = CARTESIAN_POINT ( 'NONE',  ( 22.39105762524350141, -12.40667166394900178, -32.14999999999999858 ) ) ;
#49220 = DIRECTION ( 'NONE',  ( 1.000000000000000000, 0.000000000000000000, 0.000000000000000000 ) ) ;
#49221 = CARTESIAN_POINT ( 'NONE',  ( 47.75515754607209828, -54.46163821482410583, -54.87660553739389968 ) ) ;
#49223 = CARTESIAN_POINT ( 'NONE',  ( 8.320255473221708442, -14.14592437889882071, -44.56677848951485998 ) ) ;
#49222 = CARTESIAN_POINT ( 'NONE',  ( 20.30127474080329719, 10.88381105532070059, -34.64999999999999858 ) ) ;
#49224 = VECTOR ( 'NONE', #5529, 1000.000000000000114 ) ;
#49225 = CARTESIAN_POINT ( 'NONE',  ( 56.43116028100519799, 19.50260086978540031, -53.39630102202139739 ) ) ;
#49226 = CARTESIAN_POINT ( 'NONE',  ( 48.63696446388820505, 22.87845126040230070, -55.31022682284879721 ) ) ;
#49227 = ORIENTED_EDGE ( 'NONE', *, *, #49298, .T. ) ;
#49228 = CARTESIAN_POINT ( 'NONE',  ( 18.53141933435519917, -22.24903445304479987, -65.23677592514899004 ) ) ;
#49229 = EDGE_LOOP ( 'NONE', ( #32734, #7322, #2398, #36454, #44471, #37309 ) ) ;
#49230 = CYLINDRICAL_SURFACE ( 'NONE', #42959, 1.999999999999997780 ) ;
#49231 = CARTESIAN_POINT ( 'NONE',  ( 69.89373504110861290, -33.11618894431183691, -20.65000000000000213 ) ) ;
#49232 = CARTESIAN_POINT ( 'NONE',  ( 57.24507234304070380, -50.61619228913700397, -53.91419826543189942 ) ) ;
#49234 = CARTESIAN_POINT ( 'NONE',  ( 53.28513676268730137, 17.88318008810170312, -27.00290219004990178 ) ) ;
#49233 = CARTESIAN_POINT ( 'NONE',  ( 82.96870692852729690, 14.04770048173509878, -47.29707907477579454 ) ) ;
#49235 = CARTESIAN_POINT ( 'NONE',  ( 14.11179025357979988, -22.37292481521379983, -63.04538311481158530 ) ) ;
#49237 = EDGE_CURVE ( 'NONE', #1956, #35078, #27646, .T. ) ;
#49236 = CARTESIAN_POINT ( 'NONE',  ( 11.88460916116891575, 33.59273172673112384, -16.16716782997541202 ) ) ;
#49238 = CARTESIAN_POINT ( 'NONE',  ( 55.55440406777280060, -45.13279848311309905, -14.71482509943139938 ) ) ;
#49239 = DIRECTION ( 'NONE',  ( -1.000000000000000000, 0.000000000000000000, 0.000000000000000000 ) ) ;
#49240 = ORIENTED_EDGE ( 'NONE', *, *, #39326, .F. ) ;
#49241 = ORIENTED_EDGE ( 'NONE', *, *, #14775, .T. ) ;
#49242 = CARTESIAN_POINT ( 'NONE',  ( 11.93287529298650007, -65.09933430725659775, -16.56789608242559808 ) ) ;
#49243 = CARTESIAN_POINT ( 'NONE',  ( 11.10070370541949991, 32.46195726624170419, -44.39283574477070005 ) ) ;
#49244 = CARTESIAN_POINT ( 'NONE',  ( 21.93112139786197190, -10.15704698707457254, -39.26711392836666192 ) ) ;
#49245 =( BOUNDED_CURVE ( )  B_SPLINE_CURVE ( 3, ( #22242, #42186, #38250, #5761 ),
 .UNSPECIFIED., .F., .T. ) 
 B_SPLINE_CURVE_WITH_KNOTS ( ( 4, 4 ),
 ( 0.08942664019426993516, 0.6257761648869514248 ),
 .UNSPECIFIED. ) 
 CURVE ( )  GEOMETRIC_REPRESENTATION_ITEM ( )  RATIONAL_B_SPLINE_CURVE ( ( 1.000000000000000000, 0.9761707593066137889, 0.9761707593066137889, 1.000000000000000000 ) ) 
 REPRESENTATION_ITEM ( '' )  );
#49246 = CARTESIAN_POINT ( 'NONE',  ( 50.05726953842039961, -52.36002610383659572, -51.66910864135500248 ) ) ;
#49247 = CARTESIAN_POINT ( 'NONE',  ( 46.35275103504449845, -52.90993241930539881, -76.14999999999999147 ) ) ;
#49248 = EDGE_LOOP ( 'NONE', ( #45392, #11344, #47136, #23986 ) ) ;
#49249 = CARTESIAN_POINT ( 'NONE',  ( -10.06940692381879821, -44.95898322470259956, -43.89473864311649720 ) ) ;
#49250 = CARTESIAN_POINT ( 'NONE',  ( 57.32810207127130298, 14.58245081771279850, -26.26943966852299894 ) ) ;
#49251 = DIRECTION ( 'NONE',  ( 0.000000000000000000, 0.000000000000000000, 1.000000000000000000 ) ) ;
#49252 = CARTESIAN_POINT ( 'NONE',  ( 72.62341919120400746, 1.419970371292329947, -69.11014492780159912 ) ) ;
#49253 = ADVANCED_FACE ( 'NONE', ( #2250 ), #3286, .T. ) ;
#49254 = CARTESIAN_POINT ( 'NONE',  ( 26.93010376912529935, -27.85143120648099924, -35.14999999999999858 ) ) ;
#49255 = CARTESIAN_POINT ( 'NONE',  ( 17.16948286040633320, -23.52718923084113101, -43.96602994729640557 ) ) ;
#49256 = ORIENTED_EDGE ( 'NONE', *, *, #9104, .F. ) ;
#49257 = DIRECTION ( 'NONE',  ( 0.000000000000000000, -1.000000000000000000, 0.000000000000000000 ) ) ;
#49258 = FACE_OUTER_BOUND ( 'NONE', #23271, .T. ) ;
#49259 = ORIENTED_EDGE ( 'NONE', *, *, #50754, .F. ) ;
#49260 = CARTESIAN_POINT ( 'NONE',  ( 8.428826428148642691, -13.54554915206019672, -52.87566510375268791 ) ) ;
#49261 = AXIS2_PLACEMENT_3D ( 'NONE', #15922, #31878, #43955 ) ;
#49262 = CARTESIAN_POINT ( 'NONE',  ( 48.60192926749129327, -46.16789356278570011, -11.45750196660969955 ) ) ;
#49263 = CARTESIAN_POINT ( 'NONE',  ( 12.38031658575100025, -8.724376527540918858, -35.35374502362449789 ) ) ;
#49264 = CARTESIAN_POINT ( 'NONE',  ( 13.95361866583219879, -51.19462969149069664, -22.78638230707139911 ) ) ;
#49265 = CARTESIAN_POINT ( 'NONE',  ( 54.86522692285650038, 19.64335628441130055, -75.60900715747830247 ) ) ;
#49266 = CARTESIAN_POINT ( 'NONE',  ( 47.37714334366550162, -54.54225709709379544, -74.80639350504939955 ) ) ;
#49267 = ORIENTED_EDGE ( 'NONE', *, *, #47847, .T. ) ;
#49268 = CARTESIAN_POINT ( 'NONE',  ( 55.16747951314059861, 14.77612155303600083, -16.22375705186960104 ) ) ;
#49269 = CARTESIAN_POINT ( 'NONE',  ( 57.35590717504809533, -50.13655087669759780, -52.61987026566970371 ) ) ;
#49270 = CARTESIAN_POINT ( 'NONE',  ( 52.67086496592249745, -49.78228103073629995, -48.75851410805960029 ) ) ;
#49271 = EDGE_CURVE ( 'NONE', #40950, #41828, #12625, .T. ) ;
#49272 = CARTESIAN_POINT ( 'NONE',  ( 19.41271919554129965, -21.86055833610469890, -37.19327432862769456 ) ) ;
#49273 = FACE_OUTER_BOUND ( 'NONE', #1985, .T. ) ;
#49274 = ORIENTED_EDGE ( 'NONE', *, *, #23679, .T. ) ;
#49275 = EDGE_CURVE ( 'NONE', #31649, #49183, #7220, .T. ) ;
#49276 = CARTESIAN_POINT ( 'NONE',  ( 47.14077604958600176, 22.83395626750060003, -75.60950524211389734 ) ) ;
#49277 = CARTESIAN_POINT ( 'NONE',  ( 65.19851456808879675, 1.374300485541529948, -60.86138005882520474 ) ) ;
#49278 = CARTESIAN_POINT ( 'NONE',  ( 75.24176788607847755, -33.88749087479735067, -12.24369074004802016 ) ) ;
#49279 = CARTESIAN_POINT ( 'NONE',  ( 12.26282170032090058, 33.38295891277739713, -15.83707920940340053 ) ) ;
#49280 = FACE_OUTER_BOUND ( 'NONE', #29540, .T. ) ;
#49281 = LINE ( 'NONE', #45340, #18329 ) ;
#49282 = CARTESIAN_POINT ( 'NONE',  ( 57.17871029158580143, -50.61618894532200130, -74.69286753486250063 ) ) ;
#49284 = CARTESIAN_POINT ( 'NONE',  ( 46.36052476518712240, -40.25801055237913317, -54.62947754013732293 ) ) ;
#49283 = CARTESIAN_POINT ( 'NONE',  ( 64.97290478796060142, 0.8840451408750739093, -60.55014093144429665 ) ) ;
#49285 = CARTESIAN_POINT ( 'NONE',  ( 61.75019796695539753, 14.88381105532069881, -46.37203261889099792 ) ) ;
#49286 = CARTESIAN_POINT ( 'NONE',  ( -12.78066350546869856, -57.03146538805550136, -53.01233286176620396 ) ) ;
#49287 = ORIENTED_EDGE ( 'NONE', *, *, #10278, .F. ) ;
#49288 = EDGE_CURVE ( 'NONE', #41228, #49949, #31001, .T. ) ;
#49289 = CARTESIAN_POINT ( 'NONE',  ( 53.19189387552519577, -49.47595491150869407, -48.89717368174490275 ) ) ;
#49290 = VECTOR ( 'NONE', #16899, 1000.000000000000000 ) ;
#49291 = CARTESIAN_POINT ( 'NONE',  ( 61.55075694485340421, -45.11618134123870050, -27.39088103713649858 ) ) ;
#49292 = CARTESIAN_POINT ( 'NONE',  ( 47.75291977277740330, -54.48739848013089926, -55.20309039576500254 ) ) ;
#49293 = CARTESIAN_POINT ( 'NONE',  ( 57.57552615852310396, 13.96395657264059942, -25.75103562460460083 ) ) ;
#49294 = CARTESIAN_POINT ( 'NONE',  ( 17.44202617202429906, -8.685715479244029424, -38.01220089870779617 ) ) ;
#49296 = CARTESIAN_POINT ( 'NONE',  ( 50.29495134167750336, 18.68575087643539945, -76.14999999999999147 ) ) ;
#49295 = AXIS2_PLACEMENT_3D ( 'NONE', #13854, #50534, #10702 ) ;
#49298 = EDGE_CURVE ( 'NONE', #6528, #5619, #4877, .T. ) ;
#49297 = CARTESIAN_POINT ( 'NONE',  ( 53.38247603630389904, 18.20190482432069956, -49.11032166583889591 ) ) ;
#49299 = CARTESIAN_POINT ( 'NONE',  ( 71.23034918703520191, 1.369664981662519931, -70.37861443921559612 ) ) ;
#49300 = DIRECTION ( 'NONE',  ( 0.000000000000000000, 0.000000000000000000, 1.000000000000000000 ) ) ;
#49301 = CARTESIAN_POINT ( 'NONE',  ( 67.49343310951690000, -43.71773202259419833, -11.18492891670890010 ) ) ;
#49302 = ORIENTED_EDGE ( 'NONE', *, *, #33887, .T. ) ;
#49303 = VECTOR ( 'NONE', #5843, 1000.000000000000000 ) ;
#49304 = CARTESIAN_POINT ( 'NONE',  ( 11.77695353238810050, -9.572730833979290921, -70.36851255374429570 ) ) ;
#49305 = CARTESIAN_POINT ( 'NONE',  ( 73.10458614724748827, 1.096044978595170027, -68.93830798183888930 ) ) ;
#49306 = CARTESIAN_POINT ( 'NONE',  ( 47.47143074607309643, -54.61084340594300102, -54.78606453627770634 ) ) ;
#49307 = DIRECTION ( 'NONE',  ( 0.000000000000000000, -1.000000000000000000, 0.000000000000000000 ) ) ;
#49308 = CARTESIAN_POINT ( 'NONE',  ( 73.25400818986750551, 0.9960089569207349891, -62.53811752243721145 ) ) ;
#49309 = CARTESIAN_POINT ( 'NONE',  ( 58.29681012269350049, 17.45128343075899835, -50.95499530789079756 ) ) ;
#49310 = CARTESIAN_POINT ( 'NONE',  ( 71.31398829338289147, 1.388313565858570131, -61.02265534841509975 ) ) ;
#49311 = CARTESIAN_POINT ( 'NONE',  ( 46.67317881810770075, 7.891852522694349226, -34.65023821785899116 ) ) ;
#49312 = CARTESIAN_POINT ( 'NONE',  ( 72.08523627823790036, 1.342503070345590022, -61.28987608900740014 ) ) ;
#49313 = CARTESIAN_POINT ( 'NONE',  ( 23.64088795765827200, -18.16524924148145814, -71.61181469969464786 ) ) ;
#49314 = VERTEX_POINT ( 'NONE', #18225 ) ;
#49315 = CARTESIAN_POINT ( 'NONE',  ( 64.78158399514489929, 0.9281439705311369526, -70.62613840402418930 ) ) ;
#49316 = VERTEX_POINT ( 'NONE', #23172 ) ;
#49317 = CARTESIAN_POINT ( 'NONE',  ( 8.803322232233091071, -63.21315167929310519, -46.67017412665830278 ) ) ;
#49318 = LINE ( 'NONE', #41181, #11847 ) ;
#49319 = ORIENTED_EDGE ( 'NONE', *, *, #9279, .F. ) ;
#49320 = CYLINDRICAL_SURFACE ( 'NONE', #46798, 7.910999999999997812 ) ;
#49321 = CARTESIAN_POINT ( 'NONE',  ( 83.95017420394412966, 13.51629706050414370, -47.46180916972096497 ) ) ;
#49322 = CARTESIAN_POINT ( 'NONE',  ( 21.96868942811769898, -19.57828787301799878, -53.03706054135149373 ) ) ;
#49323 = CARTESIAN_POINT ( 'NONE',  ( 52.76002509195300405, 19.59599347919969858, -76.29651901294879224 ) ) ;
#49324 = ORIENTED_EDGE ( 'NONE', *, *, #26587, .T. ) ;
#49325 = DIRECTION ( 'NONE',  ( 0.000000000000000000, 0.000000000000000000, 1.000000000000000000 ) ) ;
#49326 = DIRECTION ( 'NONE',  ( -0.2138226895232112068, -0.2149704985134071045, -0.9529257800133007494 ) ) ;
#49327 = CARTESIAN_POINT ( 'NONE',  ( 45.63393739769620083, 19.38381105532069881, 14.21249999999999858 ) ) ;
#49328 = CARTESIAN_POINT ( 'NONE',  ( 17.71973881293279973, -7.524961971755559809, -53.35393626560600211 ) ) ;
#49329 = CARTESIAN_POINT ( 'NONE',  ( 22.70316795904539120, -13.93762338909561826, -56.37318659548496669 ) ) ;
#49330 = CARTESIAN_POINT ( 'NONE',  ( 42.72898525104111656, -37.73742736476912540, -76.67469147134403329 ) ) ;
#49331 = ORIENTED_EDGE ( 'NONE', *, *, #1937, .F. ) ;
#49332 = CARTESIAN_POINT ( 'NONE',  ( 18.42160731955080522, 20.91301623499861151, -75.51793353187491675 ) ) ;
#49333 = CARTESIAN_POINT ( 'NONE',  ( 13.44640934693589962, -8.667528154172808641, -47.61518544794569863 ) ) ;
#49334 = CIRCLE ( 'NONE', #21683, 6.100000000000001421 ) ;
#49335 = AXIS2_PLACEMENT_3D ( 'NONE', #30762, #22381, #26049 ) ;
#49336 = CARTESIAN_POINT ( 'NONE',  ( 10.81129653165480065, -11.20976454154149948, -32.14999999999999858 ) ) ;
#49337 = CIRCLE ( 'NONE', #45167, 33.00000000000000000 ) ;
#49338 = ADVANCED_FACE ( 'NONE', ( #39189 ), #33516, .T. ) ;
#49339 = CONICAL_SURFACE ( 'NONE', #26708, 3.567506086244481622, 0.04995839572194331335 ) ;
#49340 = CARTESIAN_POINT ( 'NONE',  ( 13.69873651028019879, 20.72643819036770196, -75.26885115310530239 ) ) ;
#49341 = EDGE_CURVE ( 'NONE', #3841, #46513, #34279, .T. ) ;
#49342 = CARTESIAN_POINT ( 'NONE',  ( 82.13853704237929776, -47.11618894467930119, -46.37203261889099792 ) ) ;
#49343 = CARTESIAN_POINT ( 'NONE',  ( 82.62217614637160068, -45.06710035710920437, -46.37143498965749444 ) ) ;
#49344 = CARTESIAN_POINT ( 'NONE',  ( 12.04442768316860146, -22.77570226639050333, -54.17286283568609662 ) ) ;
#49345 = ORIENTED_EDGE ( 'NONE', *, *, #11704, .F. ) ;
#49346 = CARTESIAN_POINT ( 'NONE',  ( 52.97741287737559901, -49.44182383634679923, -27.32735893619970113 ) ) ;
#49347 = CARTESIAN_POINT ( 'NONE',  ( 15.59055465918129890, -51.07878210359169913, -21.35214379961709952 ) ) ;
#49348 = CARTESIAN_POINT ( 'NONE',  ( 5.837997345208469469, 28.59614577856129713, -13.72651855969540158 ) ) ;
#49349 = CARTESIAN_POINT ( 'NONE',  ( 22.90068744318051586, -15.61618870719606278, -70.84718393407784731 ) ) ;
#49350 = DIRECTION ( 'NONE',  ( 1.000000000000000000, 0.000000000000000000, 0.000000000000000000 ) ) ;
#49351 = ORIENTED_EDGE ( 'NONE', *, *, #36763, .T. ) ;
#49352 = CARTESIAN_POINT ( 'NONE',  ( -10.87682430560830049, -42.35274797428079552, -6.258335782129580416 ) ) ;
#49353 = CARTESIAN_POINT ( 'NONE',  ( 47.38355736121539508, 23.43506509291880135, -54.85967685610170008 ) ) ;
#49354 = DIRECTION ( 'NONE',  ( 1.000000000000000000, 0.000000000000000000, 0.000000000000000000 ) ) ;
#49355 = CARTESIAN_POINT ( 'NONE',  ( 63.22191407479270708, 1.186701509386340003, -62.36552507365149722 ) ) ;
#49356 = DIRECTION ( 'NONE',  ( 0.000000000000000000, 0.000000000000000000, 1.000000000000000000 ) ) ;
#49357 = CARTESIAN_POINT ( 'NONE',  ( 11.24176296214520043, 33.99927896084999901, -17.63707693806219723 ) ) ;
#49358 = FACE_OUTER_BOUND ( 'NONE', #26857, .T. ) ;
#49360 = ADVANCED_FACE ( 'NONE', ( #34978 ), #15077, .F. ) ;
#49359 = CARTESIAN_POINT ( 'NONE',  ( 16.13393739769620083, -15.61618894467929941, -14.88746750000000141 ) ) ;
#49361 = DIRECTION ( 'NONE',  ( -0.5110015285683598973, 0.4887508954475665024, -0.7071067811865485719 ) ) ;
#49362 = CARTESIAN_POINT ( 'NONE',  ( 54.36726455973389704, -49.00028188061180856, -48.99340372004090227 ) ) ;
#49363 = CARTESIAN_POINT ( 'NONE',  ( 53.71520252225610648, 17.65497178273479761, -27.13662481516249869 ) ) ;
#49364 = CARTESIAN_POINT ( 'NONE',  ( 56.06025071900570111, 19.69505054709740222, -53.55197912626789503 ) ) ;
#49365 = AXIS2_PLACEMENT_3D ( 'NONE', #40310, #15692, #20122 ) ;
#49366 = CARTESIAN_POINT ( 'NONE',  ( 63.46802213033249274, 0.9644268476137619617, -69.42324179401759920 ) ) ;
#49367 = AXIS2_PLACEMENT_3D ( 'NONE', #17090, #49325, #25437 ) ;
#49368 = CARTESIAN_POINT ( 'NONE',  ( 34.41893739769619742, -15.61618894467929941, -14.68999999999999950 ) ) ;
#49369 = CARTESIAN_POINT ( 'NONE',  ( 46.59920180852409288, 13.88381105532070059, -7.957592738636480867 ) ) ;
#49370 = ORIENTED_EDGE ( 'NONE', *, *, #29343, .F. ) ;
#49371 = CARTESIAN_POINT ( 'NONE',  ( 19.04602951442133474, 21.06500373477386034, -15.95264016292855658 ) ) ;
#49372 = CARTESIAN_POINT ( 'NONE',  ( 9.735422304259749637, 31.96558444038419822, -46.29845817061509905 ) ) ;
#49373 = DIRECTION ( 'NONE',  ( -0.8660254037844384856, 0.5000000000000003331, 0.000000000000000000 ) ) ;
#49374 = AXIS2_PLACEMENT_3D ( 'NONE', #20174, #19917, #24347 ) ;
#49375 = DIRECTION ( 'NONE',  ( -0.7288689868556610385, 0.6846531968814593139, 0.000000000000000000 ) ) ;
#49376 = CARTESIAN_POINT ( 'NONE',  ( 17.91483615131959795, 20.08140804309819671, -75.03330975078259257 ) ) ;
#49377 = ORIENTED_EDGE ( 'NONE', *, *, #22925, .T. ) ;
#49378 = VERTEX_POINT ( 'NONE', #44144 ) ;
#49379 = DIRECTION ( 'NONE',  ( 0.000000000000000000, 1.000000000000000000, 0.000000000000000000 ) ) ;
#49380 = CIRCLE ( 'NONE', #35094, 1.000000000000000444 ) ;
#49381 = ORIENTED_EDGE ( 'NONE', *, *, #2060, .T. ) ;
#49382 = CARTESIAN_POINT ( 'NONE',  ( 12.84259407419289900, -65.50421454171720370, -47.60240834020890333 ) ) ;
#49383 = CARTESIAN_POINT ( 'NONE',  ( 57.29351084095430480, -45.75340000471780399, -26.24431632910020085 ) ) ;
#49384 = CARTESIAN_POINT ( 'NONE',  ( 16.13393739769620083, -15.61618894467929941, -11.65000000000000036 ) ) ;
#49385 = FACE_OUTER_BOUND ( 'NONE', #1697, .T. ) ;
#49386 = CARTESIAN_POINT ( 'NONE',  ( 61.68720307896570176, 13.88748677907970119, -46.48647000020920217 ) ) ;
#49387 = CARTESIAN_POINT ( 'NONE',  ( 64.71095929546520154, 1.416242794300709873, -61.14503753232310146 ) ) ;
#49388 = VERTEX_POINT ( 'NONE', #24451 ) ;
#49389 = CARTESIAN_POINT ( 'NONE',  ( 75.23597853791552836, 2.430820170349590192, -12.22130859511000622 ) ) ;
#49390 = ORIENTED_EDGE ( 'NONE', *, *, #15013, .T. ) ;
#49391 = CARTESIAN_POINT ( 'NONE',  ( 46.27378782115770406, -45.92656169234390262, -9.695123937814390302 ) ) ;
#49392 = LINE ( 'NONE', #37322, #37991 ) ;
#49393 = CARTESIAN_POINT ( 'NONE',  ( -19.37574330875981587, -50.98649365362385311, 11.97999999999999865 ) ) ;
#49394 = ORIENTED_EDGE ( 'NONE', *, *, #35831, .T. ) ;
#49395 = DIRECTION ( 'NONE',  ( 0.000000000000000000, 0.000000000000000000, 1.000000000000000000 ) ) ;
#49396 = CARTESIAN_POINT ( 'NONE',  ( 47.11354740527600171, -54.64978104499210332, -74.95188530402140259 ) ) ;
#49397 = CARTESIAN_POINT ( 'NONE',  ( 46.63393739769619373, 4.883811055320659733, -35.14999999999999858 ) ) ;
#49398 = CARTESIAN_POINT ( 'NONE',  ( 50.44903216339780272, 14.35615507604409835, -12.26919617389220107 ) ) ;
#49399 = ADVANCED_FACE ( 'NONE', ( #40464 ), #8434, .T. ) ;
#49400 = VECTOR ( 'NONE', #29529, 1000.000000000000000 ) ;
#49401 = CARTESIAN_POINT ( 'NONE',  ( 60.70500520956166923, 28.95487886718607484, 11.84999999999999964 ) ) ;
#49402 = CARTESIAN_POINT ( 'NONE',  ( -7.043336953760312547, -0.4477742326702461861, -84.65000000000000568 ) ) ;
#49403 = VECTOR ( 'NONE', #25241, 1000.000000000000000 ) ;
#49404 = VECTOR ( 'NONE', #15526, 1000.000000000000000 ) ;
#49405 = CARTESIAN_POINT ( 'NONE',  ( 12.36324357420019915, -64.54680782163349306, -15.76420532458509882 ) ) ;
#49406 = CARTESIAN_POINT ( 'NONE',  ( 58.68274678269510503, 13.94184647788599918, -25.96024197693940039 ) ) ;
#49407 = VECTOR ( 'NONE', #17602, 1000.000000000000000 ) ;
#49408 = CARTESIAN_POINT ( 'NONE',  ( 12.81178300798239889, -8.506333925476139868, -72.64836766404940249 ) ) ;
#49409 = B_SPLINE_SURFACE_WITH_KNOTS ( 'NONE', 3, 3, ( 
 ( #35342, #3649, #43985, #19101, #43734, #51082, #15180, #51344, #35610, #19620, #39545 ),
 ( #27983, #31907, #10996, #39038, #47422, #31138, #7068, #19870, #27216, #4147, #8091 ),
 ( #43228, #46910, #34822, #26961, #15954, #15442, #51598, #24035, #7320, #11776, #31395 ),
 ( #43475, #23267, #39286, #3395, #7835, #15693, #11515, #35861, #47670, #7582, #31648 ),
 ( #23784, #42973, #27474, #27735, #3905, #51850, #47928, #50826, #14918, #23018, #12804 ),
 ( #37160, #45023, #48436, #40566, #28503, #25073, #41090, #29279, #44238, #5201, #17244 ),
 ( #44501, #1257, #48969, #12536, #48702, #21152, #24818, #16458, #41340, #33208, #28760 ),
 ( #49226, #217, #44762, #29026, #13320, #45282, #32160, #9391, #48176, #25338, #8865 ),
 ( #20635, #20123, #36622, #995, #40311, #16202, #4407, #36116, #32413, #40827, #12278 ),
 ( #28240, #4926, #8342, #13073, #24296, #9122, #8603, #16993, #20374, #36363, #471 ),
 ( #20897, #36895, #32942, #24553, #4662, #724, #16717, #32675, #18007, #37663, #29535 ),
 ( #1769, #41857, #6480, #13823, #17750, #14594, #26629, #45540, #21921, #33719, #17498 ),
 ( #22179, #26110, #42121, #30564, #9635, #14079, #49734, #37411, #5962, #46585, #10414 ),
 ( #1513, #25591, #22438, #29781, #38445, #18258, #10673, #21410, #41597, #14337, #5457 ),
 ( #10153, #2027, #25845, #38189, #6222, #13572, #45800, #21659, #33972, #30040, #33466 ),
 ( #2284, #49486, #34499, #18526, #46064, #37931, #5704, #26367, #9889, #49986, #34227 ),
 ( #50247, #30306, #46323, #42383, #2545, #50504, #38716, #19554, #18780, #30818, #43162 ),
 ( #7002, #39486, #47606, #15633, #51536, #43414, #46846, #11453, #3584, #35546, #22953 ),
 ( #43672, #31585, #51279, #10932, #26899, #35801, #11706, #47864, #7772, #42646, #15376 ),
 ( #31075, #3322, #11967, #38975, #22700, #27411, #3067, #42906, #6743, #23722, #7515 ) ),
 .UNSPECIFIED., .F., .F., .F.,
 ( 4, 2, 2, 2, 2, 2, 2, 2, 2, 4 ),
 ( 4, 1, 1, 1, 1, 1, 1, 1, 4 ),
 ( -3.516439999999999908E-13, 0.4027787201731649613, 0.8630972575143259773, 1.150796343352550100, 1.294645886271670099, 1.524805154942250107, 1.789982511918259966, 2.002124397499069897, 2.214266283079879827, 2.301592686705460356 ),
 ( 0.000000000000000000, 0.1250000000000000000, 0.2500000000000000000, 0.3750000000000000000, 0.5000000000000000000, 0.6250000000000000000, 0.7500000000000000000, 0.8750000000000000000, 1.000000000000000000 ),
 .UNSPECIFIED. ) ;
#49410 = ORIENTED_EDGE ( 'NONE', *, *, #3242, .F. ) ;
#49411 = CARTESIAN_POINT ( 'NONE',  ( -0.007164427059776000244, -27.04615419348650107, -34.77269723891829756 ) ) ;
#49412 = CARTESIAN_POINT ( 'NONE',  ( -10.74377218051129823, -41.32309662373379666, -4.375840798615800331 ) ) ;
#49413 = CARTESIAN_POINT ( 'NONE',  ( 68.13393739769618662, -29.16618894467940137, -65.65000000000000568 ) ) ;
#49414 = CARTESIAN_POINT ( 'NONE',  ( 72.60355388137550392, 1.390572245144360064, -69.33358376010779978 ) ) ;
#49415 = EDGE_CURVE ( 'NONE', #17858, #31052, #1168, .T. ) ;
#49416 = DIRECTION ( 'NONE',  ( 0.5720614028176879140, 0.7071067811865481278, -0.4156269377774475249 ) ) ;
#49418 = EDGE_CURVE ( 'NONE', #4493, #16548, #51748, .T. ) ;
#49417 = CARTESIAN_POINT ( 'NONE',  ( 47.48063017294606425, -54.33024059656849403, -75.12266286251488623 ) ) ;
#49419 = CARTESIAN_POINT ( 'NONE',  ( 49.13578581667089651, -53.89835027320589944, -55.25235944000669974 ) ) ;
#49420 = CARTESIAN_POINT ( 'NONE',  ( 23.04644654094820311, -19.60034674646418296, -55.95901133476449019 ) ) ;
#49421 = CARTESIAN_POINT ( 'NONE',  ( 76.87859684847769870, -43.11619168008749625, -14.85884840380859906 ) ) ;
#49422 = EDGE_CURVE ( 'NONE', #23002, #25882, #18760, .T. ) ;
#49423 = DIRECTION ( 'NONE',  ( 0.000000000000000000, 0.000000000000000000, -1.000000000000000000 ) ) ;
#49424 = ORIENTED_EDGE ( 'NONE', *, *, #39185, .T. ) ;
#49425 = CARTESIAN_POINT ( 'NONE',  ( 11.35448481870250070, -9.900987514852682025, -48.34564971805809819 ) ) ;
#49426 = CARTESIAN_POINT ( 'NONE',  ( 64.21689986822309493, 1.266076987107070062, -61.19485232126449858 ) ) ;
#49427 = ORIENTED_EDGE ( 'NONE', *, *, #50427, .F. ) ;
#49428 = CARTESIAN_POINT ( 'NONE',  ( -0.03888451113519723890, -50.92360554050903687, -34.84227938466554519 ) ) ;
#49429 = CARTESIAN_POINT ( 'NONE',  ( 60.46305695989290285, -45.79448408183320396, -47.68939924749230386 ) ) ;
#49430 = DIRECTION ( 'NONE',  ( 0.000000000000000000, -1.000000000000000000, 0.000000000000000000 ) ) ;
#49431 = CARTESIAN_POINT ( 'NONE',  ( 12.44373460634760065, 18.75032478515380063, -21.13286269215250002 ) ) ;
#49433 = DIRECTION ( 'NONE',  ( 0.000000000000000000, 0.000000000000000000, 1.000000000000000000 ) ) ;
#49432 = CARTESIAN_POINT ( 'NONE',  ( 43.28072419627158496, 8.659894295519814378, -70.14142403610232179 ) ) ;
#49434 = CARTESIAN_POINT ( 'NONE',  ( 50.95182575631829991, -50.95090194773979420, -76.14999999999999147 ) ) ;
#49435 = CARTESIAN_POINT ( 'NONE',  ( 10.13393739769619906, -54.15188668067469990, -35.14999999999999858 ) ) ;
#49436 = VERTEX_POINT ( 'NONE', #4052 ) ;
#49437 = ORIENTED_EDGE ( 'NONE', *, *, #13021, .F. ) ;
#49438 = ORIENTED_EDGE ( 'NONE', *, *, #28835, .T. ) ;
#49439 = CARTESIAN_POINT ( 'NONE',  ( 61.44117429376609607, -45.34731734014510351, -47.30190162006350363 ) ) ;
#49440 = CIRCLE ( 'NONE', #1730, 0.5000000000000004441 ) ;
#49441 = CARTESIAN_POINT ( 'NONE',  ( 60.93032024860885798, 14.20921469949021976, -47.21540920729788127 ) ) ;
#49442 = TOROIDAL_SURFACE ( 'NONE', #27641, 18.49999999936520112, 4.999999999969890752 ) ;
#49443 = VECTOR ( 'NONE', #1213, 1000.000000000000000 ) ;
#49444 = VERTEX_POINT ( 'NONE', #48081 ) ;
#49445 = ORIENTED_EDGE ( 'NONE', *, *, #7249, .T. ) ;
#49446 = CIRCLE ( 'NONE', #7573, 5.499999999999998224 ) ;
#49447 = AXIS2_PLACEMENT_3D ( 'NONE', #44275, #12068, #3945 ) ;
#49448 = ORIENTED_EDGE ( 'NONE', *, *, #32309, .T. ) ;
#49449 = CARTESIAN_POINT ( 'NONE',  ( 10.22095815093987881, -19.02406446778493176, -73.28612399903180119 ) ) ;
#49450 = CARTESIAN_POINT ( 'NONE',  ( 9.367379825797401693, -15.61607429561870042, -45.84717978380999881 ) ) ;
#49451 = CARTESIAN_POINT ( 'NONE',  ( 13.61748873513634095, 18.38375039377714515, -83.08753104980289095 ) ) ;
#49452 = CARTESIAN_POINT ( 'NONE',  ( 19.54194020638888318, -21.52909355783877032, -52.78615182703926223 ) ) ;
#49453 = FACE_OUTER_BOUND ( 'NONE', #51555, .T. ) ;
#49454 = ORIENTED_EDGE ( 'NONE', *, *, #39280, .T. ) ;
#49455 = LINE ( 'NONE', #9361, #45890 ) ;
#49456 = CARTESIAN_POINT ( 'NONE',  ( 51.83314574864460411, -50.19546514301369911, -76.51145668752809570 ) ) ;
#49457 = CARTESIAN_POINT ( 'NONE',  ( 7.517033938252880354, -61.58399597082019739, -19.14999999999999858 ) ) ;
#49458 = CARTESIAN_POINT ( 'NONE',  ( 21.91117268576520161, -20.92752587786970153, -66.24912813843610593 ) ) ;
#49459 = B_SPLINE_CURVE_WITH_KNOTS ( 'NONE', 3,
 ( #21070, #40743, #37072, #36800, #910, #4573, #48352, #16905, #12445, #9312, #48879, #8521, #24468, #28934, #1170, #17166, #49146, #13243 ),
 .UNSPECIFIED., .F., .F.,
 ( 4, 2, 2, 2, 2, 2, 2, 2, 4 ),
 ( 0.000000000000000000, 0.06250015020281043943, 0.1250003004056208789, 0.1875004506084313183, 0.2500006008112417577, 0.3125007510140521694, 0.3750009012168626366, 0.4375010514196731037, 0.5000012016224835154 ),
 .UNSPECIFIED. ) ;
#49460 = CARTESIAN_POINT ( 'NONE',  ( 11.51160566532330165, 19.89559162839070083, -23.15000000000000213 ) ) ;
#49461 = CARTESIAN_POINT ( 'NONE',  ( 42.61258517392390388, 13.83109901667380015, -6.251412676332040341 ) ) ;
#49462 = EDGE_CURVE ( 'NONE', #1665, #22570, #19907, .T. ) ;
#49463 = B_SPLINE_CURVE_WITH_KNOTS ( 'NONE', 3,
 ( #14943, #46937, #26991, #47192, #35370, #7093 ),
 .UNSPECIFIED., .F., .F.,
 ( 4, 2, 4 ),
 ( 0.000000000000000000, 0.5400851465932335893, 1.000000000000000000 ),
 .UNSPECIFIED. ) ;
#49464 = CARTESIAN_POINT ( 'NONE',  ( 42.74124888519239818, -44.04278178416409872, -5.015693368613340475 ) ) ;
#49465 = CARTESIAN_POINT ( 'NONE',  ( 26.52624224310950396, -9.616188944679349149, -22.14999999999999858 ) ) ;
#49466 = DIRECTION ( 'NONE',  ( -0.9200120562340469155, 0.3918900565005459247, -8.326672684688669123E-17 ) ) ;
#49467 = CARTESIAN_POINT ( 'NONE',  ( 63.65233837787889826, 1.010052234904240009, -69.64061050479490689 ) ) ;
#49468 = CARTESIAN_POINT ( 'NONE',  ( 46.93104535293870327, 8.311849618651319105, -54.22205626569730441 ) ) ;
#49469 = CARTESIAN_POINT ( 'NONE',  ( 66.14676216358580518, -0.1907523817752760087, -17.02976572029630020 ) ) ;
#49470 = ORIENTED_EDGE ( 'NONE', *, *, #1221, .F. ) ;
#49471 = CARTESIAN_POINT ( 'NONE',  ( 14.10861501657639927, -52.01891576978010079, -75.67066142420200947 ) ) ;
#49472 = CARTESIAN_POINT ( 'NONE',  ( 57.35780230080800379, 18.93711611908999970, -52.65865528046390409 ) ) ;
#49473 = PRODUCT_DEFINITION_FORMATION_WITH_SPECIFIED_SOURCE ( 'ANY', '', #46688, .NOT_KNOWN. ) ;
#49474 = CARTESIAN_POINT ( 'NONE',  ( 53.63393739769619373, 31.59091783650714547, 17.05710678118654755 ) ) ;
#49475 = LINE ( 'NONE', #14587, #33463 ) ;
#49476 = AXIS2_PLACEMENT_3D ( 'NONE', #17687, #5895, #29469 ) ;
#49477 = AXIS2_PLACEMENT_3D ( 'NONE', #123, #40726, #20526 ) ;
#49478 = ADVANCED_FACE ( 'NONE', ( #32060 ), #22797, .T. ) ;
#49479 = CARTESIAN_POINT ( 'NONE',  ( 22.81054832899980056, -19.17189294434900049, -32.14999999999999858 ) ) ;
#49480 = CARTESIAN_POINT ( 'NONE',  ( 24.04472027134544021, -15.61619704117925522, -43.79232540400376905 ) ) ;
#49481 = CARTESIAN_POINT ( 'NONE',  ( 47.71207051903009955, -54.49607191801889883, -54.98518041347480079 ) ) ;
#49482 = CARTESIAN_POINT ( 'NONE',  ( 23.62413055734869971, -48.75525398023999912, -35.14999999999999858 ) ) ;
#49483 = DIRECTION ( 'NONE',  ( 1.000000000000000000, 0.000000000000000000, 0.000000000000000000 ) ) ;
#49484 = CARTESIAN_POINT ( 'NONE',  ( 41.66707738213217738, 13.41595190789255554, -5.278831647791760062 ) ) ;
#49485 = ADVANCED_FACE ( 'NONE', ( #1832 ), #5518, .T. ) ;
#49486 = CARTESIAN_POINT ( 'NONE',  ( 47.84365481784320195, 23.21637092124190360, -55.21126586928509994 ) ) ;
#49487 = CARTESIAN_POINT ( 'NONE',  ( 22.46358420153250179, -12.50521955988370060, -62.70177013111300113 ) ) ;
#49488 = ORIENTED_EDGE ( 'NONE', *, *, #17164, .F. ) ;
#49489 = CARTESIAN_POINT ( 'NONE',  ( 18.84360118837656017, -51.80630187018725508, -74.54430098193516585 ) ) ;
#49490 = CARTESIAN_POINT ( 'NONE',  ( 65.27736602627911111, 1.383811055320669947, -60.94999999999999574 ) ) ;
#49491 = DIRECTION ( 'NONE',  ( -0.8660254037844390407, -0.4999999999999995004, -5.551115123125774074E-17 ) ) ;
#49493 = CARTESIAN_POINT ( 'NONE',  ( 52.56521993400819781, 18.62941884317319818, -28.15003746460830314 ) ) ;
#49492 = CARTESIAN_POINT ( 'NONE',  ( 84.44784216359251161, 11.88381105532070059, -47.47585302082339354 ) ) ;
#49494 = CARTESIAN_POINT ( 'NONE',  ( 15.35791178160290116, -22.62620627274549889, -76.98791498200870365 ) ) ;
#49495 = DIRECTION ( 'NONE',  ( 0.000000000000000000, 0.000000000000000000, 1.000000000000000000 ) ) ;
#49496 = CARTESIAN_POINT ( 'NONE',  ( 72.73458218292580568, 1.393731187554809958, -68.81053500035210391 ) ) ;
#49497 = CARTESIAN_POINT ( 'NONE',  ( 8.222961568625748896, -16.65191337441482489, -80.75066493857167416 ) ) ;
#49498 = ORIENTED_EDGE ( 'NONE', *, *, #7411, .T. ) ;
#49499 = VERTEX_POINT ( 'NONE', #17810 ) ;
#49500 = CARTESIAN_POINT ( 'NONE',  ( 11.86574223144489970, -65.07138037345019654, -16.54426240394709779 ) ) ;
#49501 = CARTESIAN_POINT ( 'NONE',  ( 12.58777455595629924, 34.22037323676799758, -47.11705430144780138 ) ) ;
#49502 = DIRECTION ( 'NONE',  ( 0.000000000000000000, 0.000000000000000000, -1.000000000000000000 ) ) ;
#49503 = CARTESIAN_POINT ( 'NONE',  ( 12.18715281636350056, 34.05328359738290089, -46.13824078902359815 ) ) ;
#49504 = DIRECTION ( 'NONE',  ( 0.000000000000000000, -1.000000000000000000, 0.000000000000000000 ) ) ;
#49505 = ORIENTED_EDGE ( 'NONE', *, *, #6082, .T. ) ;
#49506 = CARTESIAN_POINT ( 'NONE',  ( -22.72492714007710291, -11.78847082558010051, -54.75782564465809088 ) ) ;
#49507 = DIRECTION ( 'NONE',  ( 1.000000000000000000, 0.000000000000000000, 0.000000000000000000 ) ) ;
#49508 = CARTESIAN_POINT ( 'NONE',  ( 47.54344196522969668, 23.41772573375219935, -55.12343871991259903 ) ) ;
#49509 = CARTESIAN_POINT ( 'NONE',  ( 64.42654594965659953, -1.187628165131600078, -16.42224863846029947 ) ) ;
#49510 = CARTESIAN_POINT ( 'NONE',  ( 50.92009741000290290, -50.43920147318139868, -76.16477593974259719 ) ) ;
#49511 = DIRECTION ( 'NONE',  ( 0.000000000000000000, -1.000000000000000000, 0.000000000000000000 ) ) ;
#49512 = VECTOR ( 'NONE', #4154, 1000.000000000000000 ) ;
#49513 = ORIENTED_EDGE ( 'NONE', *, *, #44287, .F. ) ;
#49514 = DIRECTION ( 'NONE',  ( 1.000000000000000000, 0.000000000000000000, 0.000000000000000000 ) ) ;
#49516 = DIRECTION ( 'NONE',  ( 0.000000000000000000, 0.000000000000000000, -1.000000000000000000 ) ) ;
#49515 = CIRCLE ( 'NONE', #49552, 5.251829701412240148 ) ;
#49517 = VERTEX_POINT ( 'NONE', #41400 ) ;
#49518 = LINE ( 'NONE', #13609, #8435 ) ;
#49519 = CARTESIAN_POINT ( 'NONE',  ( 50.59865606475919719, -46.19775965174260079, -12.88937197673160107 ) ) ;
#49520 = CARTESIAN_POINT ( 'NONE',  ( 8.865981372670939109, -12.65585574203520025, -33.13561495384320210 ) ) ;
#49521 = CARTESIAN_POINT ( 'NONE',  ( 22.90049624866714950, -16.13163838386897453, -64.87141853339200281 ) ) ;
#49522 = CARTESIAN_POINT ( 'NONE',  ( 54.50221993657880404, 19.67977562750719756, -75.72703011672629714 ) ) ;
#49523 = EDGE_CURVE ( 'NONE', #50974, #621, #18445, .T. ) ;
#49524 = CARTESIAN_POINT ( 'NONE',  ( 47.38033551737640181, -54.20286183426010496, -75.36291177546809195 ) ) ;
#49525 = VERTEX_POINT ( 'NONE', #37995 ) ;
#49526 = CARTESIAN_POINT ( 'NONE',  ( 55.76738788914159528, 14.35627483231789903, -16.42583790588760095 ) ) ;
#49527 = EDGE_CURVE ( 'NONE', #19003, #40749, #2092, .T. ) ;
#49528 = CARTESIAN_POINT ( 'NONE',  ( 57.26283657379369885, -50.61618895537380070, -53.75815476539319349 ) ) ;
#49529 = CARTESIAN_POINT ( 'NONE',  ( 52.70598057219940102, -49.76175563869689711, -48.81476139346880672 ) ) ;
#49530 = CARTESIAN_POINT ( 'NONE',  ( 15.17121401173930018, -22.60301372889670191, -33.39076563757389948 ) ) ;
#49531 = CARTESIAN_POINT ( 'NONE',  ( 53.70552627772385534, -51.31509389902640095, -75.56421117895261830 ) ) ;
#49532 = EDGE_CURVE ( 'NONE', #14446, #48131, #40226, .T. ) ;
#49533 = CARTESIAN_POINT ( 'NONE',  ( 47.16864635708899556, 22.97736630563930049, -75.46775895608919882 ) ) ;
#49534 = CARTESIAN_POINT ( 'NONE',  ( 65.11099717020638877, 1.370937308141420230, -60.89332811547459556 ) ) ;
#49535 = CARTESIAN_POINT ( 'NONE',  ( 41.43967002271349287, -45.63915426718229895, -6.362515298815959675 ) ) ;
#49536 = DIRECTION ( 'NONE',  ( 0.000000000000000000, 1.000000000000000000, 0.000000000000000000 ) ) ;
#49537 = CARTESIAN_POINT ( 'NONE',  ( 29.00424600244190287, -4.540411172299108955, -34.81403640487199880 ) ) ;
#49538 = ADVANCED_FACE ( 'NONE', ( #4994 ), #1055, .T. ) ;
#49539 = CARTESIAN_POINT ( 'NONE',  ( 23.55887781140449633, -12.03108354813719849, -79.36448291391718612 ) ) ;
#49540 = CARTESIAN_POINT ( 'NONE',  ( 60.83133136721959744, 14.23629320661039976, -47.01992809069390233 ) ) ;
#49541 = CARTESIAN_POINT ( 'NONE',  ( 57.24955896891499663, -50.61618894527399704, -74.42081638965770196 ) ) ;
#49543 = CARTESIAN_POINT ( 'NONE',  ( 41.64150979412020348, -37.55586782839380788, -82.11206661960329711 ) ) ;
#49542 = CARTESIAN_POINT ( 'NONE',  ( 64.89987712417470789, 0.8859637708054509675, -60.59611492242100184 ) ) ;
#49544 = CARTESIAN_POINT ( 'NONE',  ( 61.34010611512319855, 13.97110158644820110, -46.37202112184679947 ) ) ;
#49545 = CARTESIAN_POINT ( 'NONE',  ( 17.16947147975978183, -7.705187032170163874, -69.04933684442744379 ) ) ;
#49546 = EDGE_CURVE ( 'NONE', #44209, #47941, #33269, .T. ) ;
#49547 = CARTESIAN_POINT ( 'NONE',  ( -26.15868020285170203, 9.963078067300591201, -54.51850539491499603 ) ) ;
#49548 = ORIENTED_EDGE ( 'NONE', *, *, #7702, .T. ) ;
#49549 = CONICAL_SURFACE ( 'NONE', #13556, 19.50000000000000000, 0.2449786631268651149 ) ;
#49550 = SHAPE_REPRESENTATION ( 'Caster Wheel Tread', ( #20940 ), #20155 ) ;
#49551 = CARTESIAN_POINT ( 'NONE',  ( 52.83031072168890319, -49.66267504922139864, -48.71029889621100040 ) ) ;
#49552 = AXIS2_PLACEMENT_3D ( 'NONE', #38688, #11674, #11159 ) ;
#49553 = ORIENTED_EDGE ( 'NONE', *, *, #20785, .F. ) ;
#49554 = CARTESIAN_POINT ( 'NONE',  ( 59.16460309383230509, -45.16598951315400257, -26.08201338363890187 ) ) ;
#49555 = CARTESIAN_POINT ( 'NONE',  ( 23.86302254292488101, -17.34441396915490685, -65.86232905850448560 ) ) ;
#49556 = CARTESIAN_POINT ( 'NONE',  ( 13.38185851215770050, 19.61017703320019834, -21.60458205337010185 ) ) ;
#49557 = CARTESIAN_POINT ( 'NONE',  ( 56.57085133330490123, 14.20563404004749941, -25.70412341356980335 ) ) ;
#49558 = CARTESIAN_POINT ( 'NONE',  ( 19.30482607911089943, -21.91603209087760007, -38.80439020934399252 ) ) ;
#49559 = CARTESIAN_POINT ( 'NONE',  ( 28.98356459125599827, -26.68429298316319986, -34.79124076679859456 ) ) ;
#49560 = CARTESIAN_POINT ( 'NONE',  ( 52.91120708058170408, 18.40136555541419838, -48.91474115954339652 ) ) ;
#49561 = CARTESIAN_POINT ( 'NONE',  ( 9.221477657806792294, -19.60042875044780786, -58.34100165946446737 ) ) ;
#49562 = CARTESIAN_POINT ( 'NONE',  ( 73.88940586792639920, -43.69535901349680529, -12.99103297813889846 ) ) ;
#49563 = B_SPLINE_CURVE_WITH_KNOTS ( 'NONE', 3,
 ( #10385, #33945, #38160, #26341, #46035, #41829, #41569, #5683, #26602, #33692, #6196, #37904, #6454, #1998, #17978, #10127, #26085, #50219, #14309, #30278, #38417, #2515, #50478, #18498, #27895, #23696, #31818, #3036, #11424, #15086, #39711, #19529, #43138, #15859 ),
 .UNSPECIFIED., .F., .F.,
 ( 4, 2, 1, 1, 1, 1, 1, 1, 2, 2, 2, 2, 2, 2, 2, 2, 2, 2, 2, 4 ),
 ( 0.4999954466933561603, 0.5001175181175031570, 0.5002395895416501537, 0.5004837323899442580, 0.5009720180865326888, 0.5019485894797097725, 0.5039017322660637177, 0.5078080178387720522, 0.5156205889841884993, 0.5312457312750212823, 0.5624960158566866264, 0.6249965850200170925, 0.6874971541833474475, 0.7499977233466779136, 0.8124982925100083797, 0.8749988616733388458, 0.9062491462550041899, 0.9374994308366694229, 0.9687497154183346559, 1.000000000000000000 ),
 .UNSPECIFIED. ) ;
#49564 = VERTEX_POINT ( 'NONE', #5258 ) ;
#49565 = CARTESIAN_POINT ( 'NONE',  ( 10.90317266407199881, -20.92144997887719882, -77.81509207372450021 ) ) ;
#49566 = CARTESIAN_POINT ( 'NONE',  ( 72.94510729672219895, 1.263823323415670163, -68.97683676677020514 ) ) ;
#49567 = CARTESIAN_POINT ( 'NONE',  ( 47.47394861760930240, -54.61301726039770443, -54.85049212571620103 ) ) ;
#49568 = CARTESIAN_POINT ( 'NONE',  ( 23.97848197093998834, -14.55973312613292592, -49.74973267396308074 ) ) ;
#49569 = CARTESIAN_POINT ( 'NONE',  ( 73.15787026839889506, 0.9945465939392541532, -62.38364600848370145 ) ) ;
#49570 = B_SPLINE_CURVE_WITH_KNOTS ( 'NONE', 3,
 ( #35842, #12518, #15933, #11756, #28485, #11499, #27714, #47907, #31888, #3630, #7560, #8324, #32141, #24276, #39529, #43715, #19602, #43966 ),
 .UNSPECIFIED., .F., .F.,
 ( 4, 2, 2, 2, 2, 2, 2, 2, 4 ),
 ( 0.5000015647840699851, 0.5625013691860611953, 0.6250011735880525165, 0.6875009779900437268, 0.7500007823920349370, 0.8125005867940262583, 0.8750003911960174685, 0.9375001955980086787, 1.000000000000000000 ),
 .UNSPECIFIED. ) ;
#49571 = CARTESIAN_POINT ( 'NONE',  ( 11.00562562889980001, -65.16137108100819830, -18.07900588240499928 ) ) ;
#49572 = CARTESIAN_POINT ( 'NONE',  ( 52.82975622904289992, 18.42854261028849905, -48.47378032971769812 ) ) ;
#49573 = PLANE ( 'NONE',  #34298 ) ;
#49574 = CARTESIAN_POINT ( 'NONE',  ( 23.04646553001205334, -11.63206671227860944, -45.62564837832152875 ) ) ;
#49575 = ADVANCED_FACE ( 'NONE', ( #21210 ), #29329, .T. ) ;
#49576 = CARTESIAN_POINT ( 'NONE',  ( 8.426478244294473896, -17.64473173899449066, -46.42595012760061479 ) ) ;
#49577 = CARTESIAN_POINT ( 'NONE',  ( 65.03937945068039994, 1.384708701328909886, -70.30837376962780638 ) ) ;
#49578 = ORIENTED_EDGE ( 'NONE', *, *, #29395, .T. ) ;
#49579 = CARTESIAN_POINT ( 'NONE',  ( 9.285734567762460756, -63.19748911377190126, -46.53048861919899792 ) ) ;
#49580 = EDGE_LOOP ( 'NONE', ( #11692, #36458, #11208, #42741 ) ) ;
#49581 = DIRECTION ( 'NONE',  ( -1.000000000000000000, 0.000000000000000000, 0.000000000000000000 ) ) ;
#49582 = CARTESIAN_POINT ( 'NONE',  ( 84.44784216359251161, 11.88381105532070059, -47.47585302082339354 ) ) ;
#49583 = CARTESIAN_POINT ( 'NONE',  ( 22.90128585160542585, -15.83904648336577381, -52.85765549546293585 ) ) ;
#49584 = CARTESIAN_POINT ( 'NONE',  ( 51.40458829710209443, 19.31600304772210208, -76.23573209377541104 ) ) ;
#49585 = ORIENTED_EDGE ( 'NONE', *, *, #5103, .T. ) ;
#49586 = DIRECTION ( 'NONE',  ( 1.000000000000000000, 0.000000000000000000, 0.000000000000000000 ) ) ;
#49587 = CARTESIAN_POINT ( 'NONE',  ( -0.1295185695942999982, 0.6472670226113349523, -84.65000000000000568 ) ) ;
#49588 = CARTESIAN_POINT ( 'NONE',  ( 24.04215783492454150, -15.38969022549373022, -43.78321255858008243 ) ) ;
#49589 = CARTESIAN_POINT ( 'NONE',  ( 23.64151217820790052, -19.02486038249190159, -51.92799550646089557 ) ) ;
#49590 = DIRECTION ( 'NONE',  ( 1.000000000000000000, 0.000000000000000000, 0.000000000000000000 ) ) ;
#49591 = CARTESIAN_POINT ( 'NONE',  ( 45.05991202527755490, -38.04955529247586554, -65.02012688996633472 ) ) ;
#49592 = ORIENTED_EDGE ( 'NONE', *, *, #19521, .F. ) ;
#49593 = ADVANCED_FACE ( 'NONE', ( #2346 ), #35075, .T. ) ;
#49594 = CIRCLE ( 'NONE', #21082, 16.00000000000000000 ) ;
#49595 = CARTESIAN_POINT ( 'NONE',  ( 57.55751162087899786, 19.24776070067099099, -53.20292136905285929 ) ) ;
#49596 = CARTESIAN_POINT ( 'NONE',  ( 14.04776077600850037, -22.76843061483210207, -46.82299613730950227 ) ) ;
#49597 = AXIS2_PLACEMENT_3D ( 'NONE', #13533, #21881, #26070 ) ;
#49598 = AXIS2_PLACEMENT_3D ( 'NONE', #7700, #19977, #12389 ) ;
#49599 = DIRECTION ( 'NONE',  ( 0.000000000000000000, -1.000000000000000000, 0.000000000000000000 ) ) ;
#49600 = ADVANCED_FACE ( 'NONE', ( #46392 ), #30111, .T. ) ;
#49601 = CARTESIAN_POINT ( 'NONE',  ( 13.58362953646680005, 20.62786770048269958, -75.03330975078259257 ) ) ;
#49602 = LINE ( 'NONE', #25970, #3097 ) ;
#49603 = CARTESIAN_POINT ( 'NONE',  ( 41.22889096848290080, -44.82821486788269993, -5.431173202240829667 ) ) ;
#49604 = CARTESIAN_POINT ( 'NONE',  ( 20.83574943972819682, -9.224047739598423945, -61.20962266139596863 ) ) ;
#49605 = CARTESIAN_POINT ( 'NONE',  ( 7.959636065010880834, -14.53752382916180075, -56.54943076759479936 ) ) ;
#49606 = VERTEX_POINT ( 'NONE', #2614 ) ;
#49607 = CARTESIAN_POINT ( 'NONE',  ( 54.88272693801879853, -47.33106691389519938, -26.10537818549139999 ) ) ;
#49608 = CARTESIAN_POINT ( 'NONE',  ( 56.15371975346319999, -50.83714413667020438, -74.67436945125109560 ) ) ;
#49609 = CARTESIAN_POINT ( 'NONE',  ( -0.04430710383532700247, 22.44604592029679679, -9.692299893202831029 ) ) ;
#49610 = LINE ( 'NONE', #13448, #11268 ) ;
#49611 = CARTESIAN_POINT ( 'NONE',  ( 68.13393739769618662, -0.5161889446793590519, -65.65000000000000568 ) ) ;
#49612 = VERTEX_POINT ( 'NONE', #14141 ) ;
#49613 = CARTESIAN_POINT ( 'NONE',  ( -9.541283486264569902, -43.63710254895489982, -5.656394099422319854 ) ) ;
#49614 = CARTESIAN_POINT ( 'NONE',  ( 47.40067335528860326, 23.42405946800979777, -54.81948824301620249 ) ) ;
#49615 = DIRECTION ( 'NONE',  ( 0.000000000000000000, 0.000000000000000000, -1.000000000000000000 ) ) ;
#49616 = CARTESIAN_POINT ( 'NONE',  ( 63.21507766202849865, 1.186856010528209993, -62.37714938719420132 ) ) ;
#49617 = CARTESIAN_POINT ( 'NONE',  ( 61.02217321269120731, 14.13630581668499886, -46.91830674221320407 ) ) ;
#49618 = CARTESIAN_POINT ( 'NONE',  ( 11.88236604821910092, 34.20274920972010335, -17.91369388827870068 ) ) ;
#49619 = CARTESIAN_POINT ( 'NONE',  ( 52.08783726412929838, 18.38123683491329885, -77.13961689194590576 ) ) ;
#49620 = CARTESIAN_POINT ( 'NONE',  ( 52.85589143289899994, 18.41484964472980224, -48.63420543068679791 ) ) ;
#49621 = CYLINDRICAL_SURFACE ( 'NONE', #41725, 1.500000000000001332 ) ;
#49622 = CARTESIAN_POINT ( 'NONE',  ( 59.94065709827619770, -46.08170771231470297, -47.78792003745029859 ) ) ;
#49623 = DIRECTION ( 'NONE',  ( 0.000000000000000000, 0.000000000000000000, -1.000000000000000000 ) ) ;
#49624 = CARTESIAN_POINT ( 'NONE',  ( 55.53286969579190213, 19.65994446189469969, -52.96077464504600130 ) ) ;
#49625 = CARTESIAN_POINT ( 'NONE',  ( 63.28787718588009881, 0.9170817191178719519, -69.18823203240749820 ) ) ;
#49626 = CARTESIAN_POINT ( 'NONE',  ( 11.93174526809839975, -65.43929183185349530, -17.93019253464870033 ) ) ;
#49627 = CARTESIAN_POINT ( 'NONE',  ( 9.543085168726568313, -13.84486511917021367, -47.53615371606744588 ) ) ;
#49628 = ORIENTED_EDGE ( 'NONE', *, *, #6555, .F. ) ;
#49629 = CARTESIAN_POINT ( 'NONE',  ( 16.79927617522759675, -22.63757652019199895, -73.31710689363809763 ) ) ;
#49630 = CARTESIAN_POINT ( 'NONE',  ( 10.97882797226870188, 32.03231419732679797, -44.74228707380109427 ) ) ;
#49631 = AXIS2_PLACEMENT_3D ( 'NONE', #3170, #27253, #19401 ) ;
#49632 = DIRECTION ( 'NONE',  ( 1.000000000000000000, 0.000000000000000000, 0.000000000000000000 ) ) ;
#49633 = ADVANCED_FACE ( 'NONE', ( #46130 ), #36057, .T. ) ;
#49634 = CARTESIAN_POINT ( 'NONE',  ( 68.16820022677380564, -30.11594836049780355, -18.00617522382760072 ) ) ;
#49635 = CARTESIAN_POINT ( 'NONE',  ( 19.64758755231450849, -22.86272695187545168, -34.79644660940672907 ) ) ;
#49636 = EDGE_LOOP ( 'NONE', ( #1405, #26079 ) ) ;
#49637 = EDGE_CURVE ( 'NONE', #41326, #1162, #27967, .T. ) ;
#49638 = ORIENTED_EDGE ( 'NONE', *, *, #25127, .T. ) ;
#49639 = CARTESIAN_POINT ( 'NONE',  ( 49.72648160330989953, 22.41435850158119791, -55.11972614036179863 ) ) ;
#49640 = ORIENTED_EDGE ( 'NONE', *, *, #7315, .T. ) ;
#49641 = CARTESIAN_POINT ( 'NONE',  ( 10.57222913045199952, -64.13241197350170353, -46.01869289140690000 ) ) ;
#49642 = CARTESIAN_POINT ( 'NONE',  ( 57.36243933490059987, -45.44515605360940214, -26.07079599989479846 ) ) ;
#49643 = DIRECTION ( 'NONE',  ( 0.000000000000000000, 1.000000000000000000, 0.000000000000000000 ) ) ;
#49644 = EDGE_CURVE ( 'NONE', #31407, #25645, #21108, .T. ) ;
#49645 = CARTESIAN_POINT ( 'NONE',  ( 17.16954007596327969, -7.705196829635915456, -63.04933605003357400 ) ) ;
#49646 = DIRECTION ( 'NONE',  ( 0.000000000000000000, 1.000000000000000000, 0.000000000000000000 ) ) ;
#49647 = ORIENTED_EDGE ( 'NONE', *, *, #31979, .T. ) ;
#49648 = CARTESIAN_POINT ( 'NONE',  ( 45.48191705218061998, 6.865434676292834659, -62.91004931326258998 ) ) ;
#49649 = ORIENTED_EDGE ( 'NONE', *, *, #50994, .F. ) ;
#49650 = CARTESIAN_POINT ( 'NONE',  ( 49.79071638101620323, -45.11618894460959694, -10.43288004981720007 ) ) ;
#49651 = AXIS2_PLACEMENT_3D ( 'NONE', #20202, #32754, #16281 ) ;
#49652 = CARTESIAN_POINT ( 'NONE',  ( 9.973725646770976283, -20.62007079165992707, -34.57520601010690342 ) ) ;
#49653 = CARTESIAN_POINT ( 'NONE',  ( 16.22100018022290158, 19.83813723611639901, -20.14984494908090085 ) ) ;
#49654 = CARTESIAN_POINT ( 'NONE',  ( 47.64143405400680109, -54.53488714545009941, -74.14999999999999147 ) ) ;
#49655 = VERTEX_POINT ( 'NONE', #39544 ) ;
#49656 = LINE ( 'NONE', #33894, #20794 ) ;
#49657 = CARTESIAN_POINT ( 'NONE',  ( 47.02180052276420241, -54.30164223407509638, -75.47109442055590023 ) ) ;
#49658 = CARTESIAN_POINT ( 'NONE',  ( 60.46644818218479855, 14.58403685241730230, -47.72755095986849483 ) ) ;
#49659 = ADVANCED_FACE ( 'NONE', ( #7834 ), #27570, .F. ) ;
#49660 = CARTESIAN_POINT ( 'NONE',  ( 51.92534425568300094, 13.88381105524860004, -11.95547866172319829 ) ) ;
#49661 = DIRECTION ( 'NONE',  ( -0.7071067811865475727, 0.000000000000000000, 0.7071067811865475727 ) ) ;
#49662 = AXIS2_PLACEMENT_3D ( 'NONE', #7958, #11904, #28110 ) ;
#49663 = CIRCLE ( 'NONE', #30358, 0.5000000000000004441 ) ;
#49664 = CARTESIAN_POINT ( 'NONE',  ( 51.08534821908229873, 19.80328544295599968, -76.14824059617301089 ) ) ;
#49665 = CARTESIAN_POINT ( 'NONE',  ( 58.39402530481319786, 14.02893895274939950, -26.06414309828389975 ) ) ;
#49666 = CARTESIAN_POINT ( 'NONE',  ( 23.93780514016240346, -16.44467940405539608, -69.32117255937750144 ) ) ;
#49667 = ORIENTED_EDGE ( 'NONE', *, *, #36989, .T. ) ;
#49668 = DIRECTION ( 'NONE',  ( 0.000000000000000000, -1.000000000000000000, 0.000000000000000000 ) ) ;
#49669 = CARTESIAN_POINT ( 'NONE',  ( 73.13041444294920268, 0.8910129994591539093, -62.32805707658469885 ) ) ;
#49670 = CARTESIAN_POINT ( 'NONE',  ( 76.07020619028889996, -41.07279695184679724, -13.36374665373399928 ) ) ;
#49671 = CARTESIAN_POINT ( 'NONE',  ( 73.01685589897030582, 0.9479899806831150189, -69.13670813078400101 ) ) ;
#49672 = DIRECTION ( 'NONE',  ( 1.000000000000000000, 0.000000000000000000, 0.000000000000000000 ) ) ;
#49673 = CARTESIAN_POINT ( 'NONE',  ( 8.428805360677591452, -13.54562575312001727, -42.59098949349206009 ) ) ;
#49674 = CARTESIAN_POINT ( 'NONE',  ( 8.428796441877244305, -13.54565802726606272, -58.87567998479666187 ) ) ;
#49675 = CARTESIAN_POINT ( 'NONE',  ( 49.42992454522379830, -53.75819112648869691, -54.94336248455510230 ) ) ;
#49676 = CARTESIAN_POINT ( 'NONE',  ( 22.46007819155687812, -20.47790044386577790, -56.00067946053424350 ) ) ;
#49677 = CARTESIAN_POINT ( 'NONE',  ( 22.90093739854874144, -15.61802774535847504, -62.45291482988292842 ) ) ;
#49678 = CARTESIAN_POINT ( 'NONE',  ( 18.76043506954900053, -51.62277378238609771, -74.57010117178208475 ) ) ;
#49679 = CARTESIAN_POINT ( 'NONE',  ( 16.13393739769620083, -1.337601509563455471, -34.64999999999999858 ) ) ;
#49680 = ORIENTED_EDGE ( 'NONE', *, *, #34132, .T. ) ;
#49681 = CARTESIAN_POINT ( 'NONE',  ( 16.88857569320390084, -23.02815328493989711, -57.53504572143789630 ) ) ;
#49682 = CARTESIAN_POINT ( 'NONE',  ( 64.65045080987439974, 1.231980527807049919, -60.89105423166650866 ) ) ;
#49683 = ORIENTED_EDGE ( 'NONE', *, *, #45715, .T. ) ;
#49684 = CARTESIAN_POINT ( 'NONE',  ( 60.48124862545850533, -45.81154431168629770, -47.72914257570420205 ) ) ;
#49685 = FACE_OUTER_BOUND ( 'NONE', #33676, .T. ) ;
#49686 = CARTESIAN_POINT ( 'NONE',  ( 20.76113993473645891, -22.05978133672951458, -61.80939319232501816 ) ) ;
#49688 = CARTESIAN_POINT ( 'NONE',  ( 20.11811741000025577, -8.703694875967890709, -35.45899634741810047 ) ) ;
#49687 = CARTESIAN_POINT ( 'NONE',  ( 43.90603104686010738, 8.714656956882279815, -67.11423799122562173 ) ) ;
#49689 = CARTESIAN_POINT ( 'NONE',  ( 18.11497263573659922, 5.664030231104960400, -35.14999999999999858 ) ) ;
#49690 = CARTESIAN_POINT ( 'NONE',  ( 40.92586417822920453, -45.44479669594549875, -5.903607078647769235 ) ) ;
#49691 = ORIENTED_EDGE ( 'NONE', *, *, #15741, .F. ) ;
#49692 = EDGE_CURVE ( 'NONE', #38543, #11477, #30485, .T. ) ;
#49693 = ORIENTED_EDGE ( 'NONE', *, *, #28660, .T. ) ;
#49694 = VERTEX_POINT ( 'NONE', #12276 ) ;
#49695 = CARTESIAN_POINT ( 'NONE',  ( -22.84744350781432587, -16.08730834640482854, -54.74874053947917929 ) ) ;
#49696 = EDGE_CURVE ( 'NONE', #30733, #25873, #39878, .T. ) ;
#49697 = CARTESIAN_POINT ( 'NONE',  ( 16.13393739769620083, -15.61618894467929941, -35.14999999999999858 ) ) ;
#49698 = AXIS2_PLACEMENT_3D ( 'NONE', #22184, #1773, #14601 ) ;
#49699 = CYLINDRICAL_SURFACE ( 'NONE', #51121, 0.5000000000000006661 ) ;
#49700 = AXIS2_PLACEMENT_3D ( 'NONE', #12056, #40083, #20150 ) ;
#49701 = CONICAL_SURFACE ( 'NONE', #14562, 0.6299999999999977840, 0.7853981633974476129 ) ;
#49702 = EDGE_LOOP ( 'NONE', ( #22248, #16571, #4759, #45868, #36312 ) ) ;
#49703 = EDGE_LOOP ( 'NONE', ( #45098, #12392, #22664, #15976 ) ) ;
#49704 = CARTESIAN_POINT ( 'NONE',  ( 22.04683771704192452, -19.02420141048479962, -72.61946099805257404 ) ) ;
#49705 = CARTESIAN_POINT ( 'NONE',  ( 20.29258548203541679, -21.02752613792475245, -52.74448505271735144 ) ) ;
#49706 = CARTESIAN_POINT ( 'NONE',  ( 17.90516683090147865, -9.025310613233809676, -54.03615538479979818 ) ) ;
#49707 = ORIENTED_EDGE ( 'NONE', *, *, #50464, .F. ) ;
#49708 = CARTESIAN_POINT ( 'NONE',  ( 0.2602139982833864273, -46.15174389846320224, -34.65037388166341259 ) ) ;
#49709 = CARTESIAN_POINT ( 'NONE',  ( 52.68970890597619672, -50.62244288377420531, -76.51771729656020682 ) ) ;
#49710 = CARTESIAN_POINT ( 'NONE',  ( 47.47987492626153738, -54.61017751298710010, -54.97289024313108285 ) ) ;
#49711 = CARTESIAN_POINT ( 'NONE',  ( 17.19549608311789868, -7.840596314597150673, -63.55568448227298717 ) ) ;
#49712 = ADVANCED_FACE ( 'NONE', ( #3646 ), #19618, .T. ) ;
#49713 = DIRECTION ( 'NONE',  ( 6.891865000000000139E-13, 0.000000000000000000, 1.000000000000000000 ) ) ;
#49714 = TOROIDAL_SURFACE ( 'NONE', #32083, 16.60961179679779676, 0.5000000000000000000 ) ;
#49715 = CARTESIAN_POINT ( 'NONE',  ( 43.46649277351350094, 13.81022299180570023, -6.433241829987640159 ) ) ;
#49716 = ADVANCED_FACE ( 'NONE', ( #39797 ), #8089, .F. ) ;
#49717 = CARTESIAN_POINT ( 'NONE',  ( 42.78269187991680411, -42.70656023264469781, -3.305184689553219979 ) ) ;
#49718 = CARTESIAN_POINT ( 'NONE',  ( 68.13393739769840352, -50.61618894467879670, -73.25000000000220268 ) ) ;
#49719 = DIRECTION ( 'NONE',  ( 1.000000000000000000, 0.000000000000000000, 0.000000000000000000 ) ) ;
#49720 = CARTESIAN_POINT ( 'NONE',  ( 63.92533662763849378, 1.117797273082159926, -69.91988402493059596 ) ) ;
#49721 = CARTESIAN_POINT ( 'NONE',  ( 9.367400418259169470, -16.60470970061016516, -33.80066697648281604 ) ) ;
#49722 = CARTESIAN_POINT ( 'NONE',  ( 68.03809923644278967, 0.7701806829035969804, -18.68243761347000031 ) ) ;
#49723 = ORIENTED_EDGE ( 'NONE', *, *, #26436, .F. ) ;
#49724 = CARTESIAN_POINT ( 'NONE',  ( 14.14308403988269980, -52.38392585211880714, -75.82251062550821530 ) ) ;
#49725 = CARTESIAN_POINT ( 'NONE',  ( 47.18324198357289845, -54.80726809202429450, -54.61058319554170026 ) ) ;
#49726 = FACE_OUTER_BOUND ( 'NONE', #40251, .T. ) ;
#49727 = DIRECTION ( 'NONE',  ( 0.000000000000000000, 0.000000000000000000, -1.000000000000000000 ) ) ;
#49728 = CARTESIAN_POINT ( 'NONE',  ( 20.40033783584950200, -10.32204753240149842, -32.14999999999999858 ) ) ;
#49729 = CARTESIAN_POINT ( 'NONE',  ( 63.40811083734029552, 1.369613126987639928, -68.75357062980060618 ) ) ;
#49730 = CARTESIAN_POINT ( 'NONE',  ( 47.64143405403320486, -54.53488714543879468, -55.14905519569939685 ) ) ;
#49731 = CARTESIAN_POINT ( 'NONE',  ( 22.40487833862019684, -10.75395050048665446, -45.29781307381240651 ) ) ;
#49732 = DIRECTION ( 'NONE',  ( -0.7071067811865441310, 0.000000000000000000, 0.7071067811865510144 ) ) ;
#49733 = CARTESIAN_POINT ( 'NONE',  ( 42.05805489752406601, 13.23020005006048905, -5.167112208590642020 ) ) ;
#49734 = CARTESIAN_POINT ( 'NONE',  ( 48.19553001536780101, 23.02471837077230177, -54.91104515267559805 ) ) ;
#49735 = ORIENTED_EDGE ( 'NONE', *, *, #3562, .F. ) ;
#49736 = CARTESIAN_POINT ( 'NONE',  ( 11.34022645397350004, -10.44290231406579927, -74.10929620427420161 ) ) ;
#49737 = ORIENTED_EDGE ( 'NONE', *, *, #41821, .F. ) ;
#49738 = DIRECTION ( 'NONE',  ( 0.000000000000000000, 1.000000000000000000, 0.000000000000000000 ) ) ;
#49739 = CARTESIAN_POINT ( 'NONE',  ( 83.91174613973400653, 13.57252892771816732, -47.46626505588888989 ) ) ;
#49740 = DIRECTION ( 'NONE',  ( -1.000000000000000000, 0.000000000000000000, 0.000000000000000000 ) ) ;
#49742 = CARTESIAN_POINT ( 'NONE',  ( 54.18967173931659431, 16.81490735217020216, -26.03594187494229928 ) ) ;
#49741 = CARTESIAN_POINT ( 'NONE',  ( 82.66152712818241355, 14.12170720462269990, -47.35223793503389800 ) ) ;
#49743 = CARTESIAN_POINT ( 'NONE',  ( 22.33004736977609994, -18.98528079716979988, -74.61134705009999379 ) ) ;
#49744 = DIRECTION ( 'NONE',  ( 3.302498000000000159E-18, -1.533299999999999999E-17, -1.000000000000000000 ) ) ;
#49745 = CARTESIAN_POINT ( 'NONE',  ( 72.83393739769620367, 1.383811055320669947, -68.50657137141709541 ) ) ;
#49746 = DIRECTION ( 'NONE',  ( 0.000000000000000000, 0.000000000000000000, -1.000000000000000000 ) ) ;
#49747 = CARTESIAN_POINT ( 'NONE',  ( 88.13393739769620083, 1.883811055320649963, -65.65000000000000568 ) ) ;
#49748 = AXIS2_PLACEMENT_3D ( 'NONE', #12643, #40158, #48030 ) ;
#49749 = VERTEX_POINT ( 'NONE', #27733 ) ;
#49750 = EDGE_CURVE ( 'NONE', #10341, #44765, #20034, .T. ) ;
#49751 = ORIENTED_EDGE ( 'NONE', *, *, #33034, .F. ) ;
#49752 = CARTESIAN_POINT ( 'NONE',  ( 12.36320305068320025, -64.54682834576858852, -15.76422791927960176 ) ) ;
#49753 = CARTESIAN_POINT ( 'NONE',  ( 11.77948378290679976, 33.84506898935639185, -46.26038317283799728 ) ) ;
#49754 = CARTESIAN_POINT ( 'NONE',  ( 8.222524523195870572, -15.61634168869099959, -38.50766849176289952 ) ) ;
#49755 = CARTESIAN_POINT ( 'NONE',  ( 15.24818679882209693, -22.38319469959796848, -54.99448832485959571 ) ) ;
#49756 = CARTESIAN_POINT ( 'NONE',  ( 17.71568204744891517, -51.70197554413384466, -75.56421372420066973 ) ) ;
#49757 = ORIENTED_EDGE ( 'NONE', *, *, #5665, .F. ) ;
#49758 = CARTESIAN_POINT ( 'NONE',  ( -22.79226920359159791, -18.53556694150880091, -54.60327039117859727 ) ) ;
#49759 = DIRECTION ( 'NONE',  ( 0.000000000000000000, 0.000000000000000000, 1.000000000000000000 ) ) ;
#49760 = CIRCLE ( 'NONE', #16262, 3.569999999987189199 ) ;
#49761 = CARTESIAN_POINT ( 'NONE',  ( 53.29257619825270353, 18.13512485574420197, -48.87373464042530458 ) ) ;
#49762 = CARTESIAN_POINT ( 'NONE',  ( 61.22205614462959744, -2.031833448078650406, -15.94823484607219655 ) ) ;
#49763 = CARTESIAN_POINT ( 'NONE',  ( 51.21390658375870686, -49.87096767598450953, -76.33091596763159714 ) ) ;
#49764 = CARTESIAN_POINT ( 'NONE',  ( 59.80201330047449915, -46.57845792207670144, -48.51050247853770259 ) ) ;
#49765 = ORIENTED_EDGE ( 'NONE', *, *, #5257, .T. ) ;
#49766 = DIRECTION ( 'NONE',  ( 0.000000000000000000, 0.000000000000000000, -1.000000000000000000 ) ) ;
#49767 = CARTESIAN_POINT ( 'NONE',  ( 67.04038824939809160, 19.47158195952189885, -72.59354914830210248 ) ) ;
#49768 = ORIENTED_EDGE ( 'NONE', *, *, #44655, .F. ) ;
#49769 = DIRECTION ( 'NONE',  ( 0.000000000000000000, 0.000000000000000000, 1.000000000000000000 ) ) ;
#49770 = DIRECTION ( 'NONE',  ( 0.000000000000000000, -1.000000000000000000, 0.000000000000000000 ) ) ;
#49771 = CARTESIAN_POINT ( 'NONE',  ( 20.16036405916679897, -22.81136437679689877, -80.12993496510939906 ) ) ;
#49772 = CARTESIAN_POINT ( 'NONE',  ( 13.61938558558030010, -51.42721352468510077, -23.15000001641110217 ) ) ;
#49773 = CARTESIAN_POINT ( 'NONE',  ( 57.13444748808839790, 19.38601733984990005, -74.39740555932930022 ) ) ;
#49774 = ADVANCED_FACE ( 'NONE', ( #31647 ), #13370, .T. ) ;
#49775 = CARTESIAN_POINT ( 'NONE',  ( 47.56768146174049861, -54.56043035528880125, -74.36236381585459299 ) ) ;
#49776 = ORIENTED_EDGE ( 'NONE', *, *, #31306, .T. ) ;
#49777 = CARTESIAN_POINT ( 'NONE',  ( 54.97172322994220650, 14.66436157010849861, -15.90382766587370256 ) ) ;
#49778 = CARTESIAN_POINT ( 'NONE',  ( 22.41342994594504390, -12.46412855248205531, -78.69890846647390958 ) ) ;
#49779 = CARTESIAN_POINT ( 'NONE',  ( 56.87954272222179952, -50.36565961963330551, -52.82794281175259954 ) ) ;
#49780 = CARTESIAN_POINT ( 'NONE',  ( 53.59080506097220109, -49.40678926383840519, -49.22648751775089693 ) ) ;
#49781 = CARTESIAN_POINT ( 'NONE',  ( 22.61356707982760028, -12.83105728587160144, -36.71796074224590001 ) ) ;
#49782 = AXIS2_PLACEMENT_3D ( 'NONE', #14700, #7111, #47461 ) ;
#49783 = CARTESIAN_POINT ( 'NONE',  ( 47.18687257106159905, 22.80862807082690225, -75.61154398021749046 ) ) ;
#49784 = CARTESIAN_POINT ( 'NONE',  ( 65.27736602627911111, 1.383811055320669947, -60.94999999999999574 ) ) ;
#49785 = CARTESIAN_POINT ( 'NONE',  ( 60.97391253512203235, -45.68106840025293280, -47.73524043326641220 ) ) ;
#49786 = CARTESIAN_POINT ( 'NONE',  ( 68.13393739769625768, -15.41618894467850076, -103.0993275156848910 ) ) ;
#49787 = CARTESIAN_POINT ( 'NONE',  ( 28.88047141014009966, -4.586426805731299794, -34.71367995918279092 ) ) ;
#49788 = B_SPLINE_CURVE_WITH_KNOTS ( 'NONE', 3,
 ( #23009, #43218, #19292, #47096, #23453, #23841, #11576, #31969, #19679, #7381 ),
 .UNSPECIFIED., .F., .F.,
 ( 4, 2, 2, 2, 4 ),
 ( 0.1272047750342873151, 0.1420319546165290103, 0.1570382458071080123, 0.1723372614072689879, 0.1727139781532890106 ),
 .UNSPECIFIED. ) ;
#49789 = FACE_OUTER_BOUND ( 'NONE', #41728, .T. ) ;
#49790 = CARTESIAN_POINT ( 'NONE',  ( -5.194501806656489862, 17.26952857224580384, -39.31824944736199967 ) ) ;
#49792 = CARTESIAN_POINT ( 'NONE',  ( 43.93040869676359961, -39.07135447434988862, -70.79477508826258259 ) ) ;
#49791 = CYLINDRICAL_SURFACE ( 'NONE', #5700, 20.00000000000000355 ) ;
#49793 = AXIS2_PLACEMENT_3D ( 'NONE', #6988, #3573, #22941 ) ;
#49794 = CARTESIAN_POINT ( 'NONE',  ( 61.28421865660900636, 13.99901274604590107, -46.52379755071130063 ) ) ;
#49795 = CARTESIAN_POINT ( 'NONE',  ( 47.13393739769619373, -15.61618894467929941, -54.64999999999999858 ) ) ;
#49796 = CARTESIAN_POINT ( 'NONE',  ( -33.86606230032689524, -10.73522994510449990, -57.75543702565100546 ) ) ;
#49797 = ORIENTED_EDGE ( 'NONE', *, *, #12481, .T. ) ;
#49798 = CARTESIAN_POINT ( 'NONE',  ( 53.06503247311130167, -49.53825076443170161, -48.83676475835459740 ) ) ;
#49799 = VERTEX_POINT ( 'NONE', #51849 ) ;
#49800 = CARTESIAN_POINT ( 'NONE',  ( 44.28490121901400300, 8.836964955981793324, -64.90668349608083076 ) ) ;
#49801 = CARTESIAN_POINT ( 'NONE',  ( 0.3209249304026220440, -50.71887597443840434, -34.64999999999999858 ) ) ;
#49802 = CARTESIAN_POINT ( 'NONE',  ( 56.12571583893210203, 14.42962552814590005, -25.37490595678350402 ) ) ;
#49803 = CARTESIAN_POINT ( 'NONE',  ( 19.66377316389889529, -21.72215472907910083, -48.78597552336009358 ) ) ;
#49804 = CARTESIAN_POINT ( 'NONE',  ( 29.11900864776890074, -26.73446727828369873, -35.02873218748179340 ) ) ;
#49805 = CARTESIAN_POINT ( 'NONE',  ( 53.51329535014789940, 18.12655912379110035, -49.05665458396899936 ) ) ;
#49806 = CARTESIAN_POINT ( 'NONE',  ( 64.68608103367580497, 0.9036513197889520788, -60.73950228677190211 ) ) ;
#49807 = CARTESIAN_POINT ( 'NONE',  ( 85.84022851002180232, -48.61618894467930119, -53.47585302082339354 ) ) ;
#49808 = CARTESIAN_POINT ( 'NONE',  ( 53.29384558423090112, -50.54670888882439783, -28.15000000000000213 ) ) ;
#49809 = ORIENTED_EDGE ( 'NONE', *, *, #39829, .T. ) ;
#49810 = ADVANCED_FACE ( 'NONE', ( #12028 ), #37635, .T. ) ;
#49811 = CARTESIAN_POINT ( 'NONE',  ( 9.643579408486090188, -11.95805451436680045, -76.23071345245209329 ) ) ;
#49812 = EDGE_CURVE ( 'NONE', #42606, #11477, #4405, .T. ) ;
#49813 = CARTESIAN_POINT ( 'NONE',  ( 72.79231116732400153, 1.384708701328909886, -68.74455794701600553 ) ) ;
#49814 = CARTESIAN_POINT ( 'NONE',  ( 47.44876575161689658, -54.61831544581649922, -54.69911453683820213 ) ) ;
#49815 = CARTESIAN_POINT ( 'NONE',  ( 68.13393739769620083, 1.530257664727400879, -61.30355339059330078 ) ) ;
#49816 = CARTESIAN_POINT ( 'NONE',  ( 72.98500336837570046, 1.331842543267529821, -62.59469824041600816 ) ) ;
#49817 = CARTESIAN_POINT ( 'NONE',  ( 11.73422653529650006, -65.42249382734249252, -18.16216258087879964 ) ) ;
#49819 = ADVANCED_FACE ( 'NONE', ( #16457, #32412 ), #21658, .T. ) ;
#49818 = CARTESIAN_POINT ( 'NONE',  ( 52.83011278983949666, 18.42835579809699809, -48.49876830664469907 ) ) ;
#49820 = FACE_OUTER_BOUND ( 'NONE', #28533, .T. ) ;
#49821 = CARTESIAN_POINT ( 'NONE',  ( 19.83705332263880194, -9.918041006030941631, -62.13619471124365390 ) ) ;
#49822 = CARTESIAN_POINT ( 'NONE',  ( 10.22109417245393637, -12.20808089752747527, -57.61948683568049745 ) ) ;
#49823 = EDGE_CURVE ( 'NONE', #13981, #1527, #22549, .T. ) ;
#49824 = CARTESIAN_POINT ( 'NONE',  ( 64.81199447428100768, 0.8910129994591459157, -70.64647704525299332 ) ) ;
#49825 = ORIENTED_EDGE ( 'NONE', *, *, #22032, .T. ) ;
#49826 = VECTOR ( 'NONE', #45778, 1000.000000000000000 ) ;
#49827 = CARTESIAN_POINT ( 'NONE',  ( 13.99027006115310101, -51.18075678835780451, -22.90513383071120401 ) ) ;
#49828 = DIRECTION ( 'NONE',  ( 0.000000000000000000, 0.000000000000000000, -1.000000000000000000 ) ) ;
#49829 = ORIENTED_EDGE ( 'NONE', *, *, #3562, .T. ) ;
#49830 = DIRECTION ( 'NONE',  ( 0.8090169943749515591, 0.000000000000000000, -0.5877852522924675860 ) ) ;
#49831 = CYLINDRICAL_SURFACE ( 'NONE', #26862, 2.999999999999998668 ) ;
#49832 = CARTESIAN_POINT ( 'NONE',  ( 20.11810349957197985, -22.52869132921505724, -69.84100390017049165 ) ) ;
#49833 = CARTESIAN_POINT ( 'NONE',  ( 53.10748494364860051, 19.23566068709549981, -76.94545507200430734 ) ) ;
#49834 = VERTEX_POINT ( 'NONE', #48967 ) ;
#49835 = CYLINDRICAL_SURFACE ( 'NONE', #50995, 2.000000000000070610 ) ;
#49836 = CARTESIAN_POINT ( 'NONE',  ( -3.839728563314090071, -24.83858928721370063, -54.64999999999999858 ) ) ;
#49837 = CARTESIAN_POINT ( 'NONE',  ( 22.90115736359569354, -15.61618877121331295, -78.84717825834033533 ) ) ;
#49838 = CARTESIAN_POINT ( 'NONE',  ( 13.66418357337590095, -7.749611791737230249, -53.19549840347870173 ) ) ;
#49839 = CARTESIAN_POINT ( 'NONE',  ( 0.1457840918194806823, -20.72567761198500591, -34.68167776469320529 ) ) ;
#49840 = CIRCLE ( 'NONE', #45644, 5.499999999999998224 ) ;
#49841 = CARTESIAN_POINT ( 'NONE',  ( 45.73379805818350974, -38.12522060878801256, -61.65069626971402528 ) ) ;
#49842 = EDGE_CURVE ( 'NONE', #46792, #9610, #41704, .T. ) ;
#49843 = ORIENTED_EDGE ( 'NONE', *, *, #45012, .F. ) ;
#49844 = CARTESIAN_POINT ( 'NONE',  ( 57.79488012710090317, -49.04752211200187872, -51.23200826419654419 ) ) ;
#49845 = CARTESIAN_POINT ( 'NONE',  ( 13.00183092915110095, -8.856262696942298618, -41.59454668711060066 ) ) ;
#49846 = CARTESIAN_POINT ( 'NONE',  ( 52.82359347161860086, -49.70062430464940206, -48.95125679539609820 ) ) ;
#49847 = CARTESIAN_POINT ( 'NONE',  ( 8.842772715000620565, -15.57939790529679946, -32.14999999999999858 ) ) ;
#49848 = CARTESIAN_POINT ( 'NONE',  ( 13.81167868887400019, 20.68589454807339933, -75.38352342698830455 ) ) ;
#49849 = CARTESIAN_POINT ( 'NONE',  ( 17.69924730496158816, -51.74825541295913922, -75.61049359302290895 ) ) ;
#49850 =( BOUNDED_CURVE ( )  B_SPLINE_CURVE ( 3, ( #25724, #1385, #17372, #37808 ),
 .UNSPECIFIED., .F., .F. ) 
 B_SPLINE_CURVE_WITH_KNOTS ( ( 4, 4 ),
 ( 6.016222070146150180, 6.100653022355360555 ),
 .UNSPECIFIED. ) 
 CURVE ( )  GEOMETRIC_REPRESENTATION_ITEM ( )  RATIONAL_B_SPLINE_CURVE ( ( 1.000000000000000000, 0.9994060394106761835, 0.9994060394106761835, 1.000000000000000000 ) ) 
 REPRESENTATION_ITEM ( '' )  );
#49851 = CARTESIAN_POINT ( 'NONE',  ( 45.63983941734740313, -45.14183948007230640, -7.778235319476010545 ) ) ;
#49852 = CARTESIAN_POINT ( 'NONE',  ( 23.31002121937839178, -12.21984004604830076, -61.36704460802273786 ) ) ;
#49853 = ADVANCED_FACE ( 'NONE', ( #723 ), #4925, .T. ) ;
#49854 = AXIS2_PLACEMENT_3D ( 'NONE', #20426, #40105, #36413 ) ;
#49855 = CARTESIAN_POINT ( 'NONE',  ( 23.00121520682850118, -11.05294270968670034, -51.32098131739589775 ) ) ;
#49856 = EDGE_LOOP ( 'NONE', ( #36065, #65, #46236, #13212 ) ) ;
#49857 = CARTESIAN_POINT ( 'NONE',  ( 52.66674514831180431, -49.75608620355440337, -27.77093084507739817 ) ) ;
#49858 = AXIS2_PLACEMENT_3D ( 'NONE', #7445, #6936, #27092 ) ;
#49859 = CARTESIAN_POINT ( 'NONE',  ( 16.29169529782430104, -51.11619123902680428, -21.10106358378050118 ) ) ;
#49861 = CARTESIAN_POINT ( 'NONE',  ( 41.50874094001223114, -39.70998512007497538, -78.70214816491434817 ) ) ;
#49860 = CARTESIAN_POINT ( 'NONE',  ( 11.66464388782040196, 33.90635028133640105, -16.69887918881750011 ) ) ;
#49862 = CYLINDRICAL_SURFACE ( 'NONE', #40546, 5.999999999999998224 ) ;
#49863 = CARTESIAN_POINT ( 'NONE',  ( 68.88393739769620083, 6.883811055320649963, -71.50000000000000000 ) ) ;
#49864 = ORIENTED_EDGE ( 'NONE', *, *, #11648, .T. ) ;
#49865 = CARTESIAN_POINT ( 'NONE',  ( -5.660060735539860666, -46.84109022912470266, -5.074035175912159801 ) ) ;
#49866 = CARTESIAN_POINT ( 'NONE',  ( 47.55021976886940394, 23.31604569652889936, -54.67535596069880199 ) ) ;
#49867 = CARTESIAN_POINT ( 'NONE',  ( 56.04842253387821671, -45.73510956901836977, -25.30965062165876844 ) ) ;
#49868 = CARTESIAN_POINT ( 'NONE',  ( 63.13973003289760300, 0.9958340104639651358, -62.33798249239750078 ) ) ;
#49869 = DIRECTION ( 'NONE',  ( 0.000000000000000000, 0.000000000000000000, -1.000000000000000000 ) ) ;
#49870 = CARTESIAN_POINT ( 'NONE',  ( 11.62518889158750035, 33.82940804628189824, -16.65848135030810084 ) ) ;
#49871 = CARTESIAN_POINT ( 'NONE',  ( 52.25096257474319827, 18.53891021417129892, -77.19024871130291388 ) ) ;
#49872 = DIRECTION ( 'NONE',  ( 1.000000000000000000, 0.000000000000000000, 0.000000000000000000 ) ) ;
#49873 = CYLINDRICAL_SURFACE ( 'NONE', #34188, 10.00000000000000355 ) ;
#49874 = CARTESIAN_POINT ( 'NONE',  ( 22.90092024398637349, -15.63379323775387242, -66.45364811189233478 ) ) ;
#49875 = CARTESIAN_POINT ( 'NONE',  ( 54.79203463286849995, 20.14039653249960082, -53.38038282636030374 ) ) ;
#49876 = CARTESIAN_POINT ( 'NONE',  ( 63.28485546126960770, 1.028860417577979858, -69.16957158642991033 ) ) ;
#49877 = DIRECTION ( 'NONE',  ( 1.000000000000000000, 0.000000000000000000, 0.000000000000000000 ) ) ;
#49878 = EDGE_LOOP ( 'NONE', ( #39501, #24241, #28392, #20665 ) ) ;
#49879 = CARTESIAN_POINT ( 'NONE',  ( 20.04766857768572308, 23.93603348987157631, -19.07533074137708695 ) ) ;
#49880 = CARTESIAN_POINT ( 'NONE',  ( 11.10565272881359888, 32.16441030637599852, -44.25626093647380088 ) ) ;
#49881 = CARTESIAN_POINT ( 'NONE',  ( 72.84761368145599647, 1.149538111077639924, -62.00072402692669726 ) ) ;
#49882 = CARTESIAN_POINT ( 'NONE',  ( 66.28212128162849126, -33.07507224467300233, -19.91085132854729878 ) ) ;
#49883 = EDGE_CURVE ( 'NONE', #14340, #40830, #15500, .T. ) ;
#49884 = ORIENTED_EDGE ( 'NONE', *, *, #9818, .F. ) ;
#49885 = AXIS2_PLACEMENT_3D ( 'NONE', #1899, #34364, #26762 ) ;
#49886 = CARTESIAN_POINT ( 'NONE',  ( 18.78671181058629713, 20.36471648394369893, -74.34810712130391153 ) ) ;
#49887 = ORIENTED_EDGE ( 'NONE', *, *, #4071, .T. ) ;
#49888 = ORIENTED_EDGE ( 'NONE', *, *, #265, .F. ) ;
#49889 = CARTESIAN_POINT ( 'NONE',  ( 16.65211278259335614, -15.23971249058597088, -12.13039854958090125 ) ) ;
#49890 = CARTESIAN_POINT ( 'NONE',  ( 76.73335235168207191, 7.326484823470851282, -14.23296824953687256 ) ) ;
#49891 = ORIENTED_EDGE ( 'NONE', *, *, #13669, .T. ) ;
#49892 = CARTESIAN_POINT ( 'NONE',  ( 11.09888617399270139, -63.65665293880989850, -44.37975584975329468 ) ) ;
#49893 = CARTESIAN_POINT ( 'NONE',  ( 57.09481130578469532, -45.80449631822029488, -26.22977073655889768 ) ) ;
#49894 = CARTESIAN_POINT ( 'NONE',  ( 24.04493739695976018, -15.61630955180015334, -77.50768068703865765 ) ) ;
#49895 = CARTESIAN_POINT ( 'NONE',  ( 63.99198253403570646, 1.457833794292699992, -61.64494777836840456 ) ) ;
#49896 = EDGE_LOOP ( 'NONE', ( #13076, #33764, #11983, #3291 ) ) ;
#49897 = CARTESIAN_POINT ( 'NONE',  ( 45.80601968430718074, 6.900823852999605990, -61.28958453903135251 ) ) ;
#49898 = ORIENTED_EDGE ( 'NONE', *, *, #46017, .F. ) ;
#49899 = CARTESIAN_POINT ( 'NONE',  ( 51.49217680742329861, -45.11618894460779927, -11.64292740565939965 ) ) ;
#49900 = CIRCLE ( 'NONE', #23124, 17.09468304687049667 ) ;
#49901 = CARTESIAN_POINT ( 'NONE',  ( 20.23496625000258220, -22.44645670734013621, -34.12034017523288298 ) ) ;
#49902 = CARTESIAN_POINT ( 'NONE',  ( 16.36414204282080220, 19.86444509156779858, -20.27640028196680078 ) ) ;
#49903 = EDGE_CURVE ( 'NONE', #16762, #6409, #21713, .T. ) ;
#49904 = ORIENTED_EDGE ( 'NONE', *, *, #27404, .T. ) ;
#49905 = CARTESIAN_POINT ( 'NONE',  ( 73.15108049797990475, 0.8888742037077599356, -68.94068779328439689 ) ) ;
#49906 = CARTESIAN_POINT ( 'NONE',  ( 47.16774318698460178, -54.71371846786210114, -74.72677413543641478 ) ) ;
#49907 = CARTESIAN_POINT ( 'NONE',  ( 43.38948054135340016, 13.16722536039579872, -5.306502943738020228 ) ) ;
#49908 = CARTESIAN_POINT ( 'NONE',  ( 24.04504587474531263, -15.61618895646369687, -51.50767080737492165 ) ) ;
#49909 = AXIS2_PLACEMENT_3D ( 'NONE', #8267, #24218, #11699 ) ;
#49910 = CARTESIAN_POINT ( 'NONE',  ( 51.13393739769659874, -50.61618894467899565, 11.97999999999999865 ) ) ;
#49911 = CARTESIAN_POINT ( 'NONE',  ( 50.97250237377529913, 19.73188199481569782, -76.14992204905399831 ) ) ;
#49912 = CARTESIAN_POINT ( 'NONE',  ( 57.61853615479979851, 14.19444255287990053, -26.09622215295719982 ) ) ;
#49913 = EDGE_CURVE ( 'NONE', #40580, #44712, #43596, .T. ) ;
#49914 = CARTESIAN_POINT ( 'NONE',  ( 9.181218999323579766, -19.25575692125479677, -76.13400063084870339 ) ) ;
#49915 = VERTEX_POINT ( 'NONE', #12803 ) ;
#49916 = AXIS2_PLACEMENT_3D ( 'NONE', #12291, #31406, #28252 ) ;
#49918 = EDGE_CURVE ( 'NONE', #11156, #14039, #40148, .T. ) ;
#49917 = FACE_OUTER_BOUND ( 'NONE', #5405, .T. ) ;
#49919 = CARTESIAN_POINT ( 'NONE',  ( -10.77672099032110076, -41.59961327471660297, -4.617929491435150524 ) ) ;
#49920 = CARTESIAN_POINT ( 'NONE',  ( 47.13393739769619373, -36.11618894467930119, -54.64999999999999858 ) ) ;
#49921 = B_SPLINE_CURVE_WITH_KNOTS ( 'NONE', 3,
 ( #4845, #41007, #1435, #17421, #28417, #20812 ),
 .UNSPECIFIED., .F., .F.,
 ( 4, 2, 4 ),
 ( 0.4974519944936803828, 0.7487259972468401914, 1.000000000000000000 ),
 .UNSPECIFIED. ) ;
#49922 = CARTESIAN_POINT ( 'NONE',  ( 72.75077066479440191, 1.389801772588449946, -68.87277968851719834 ) ) ;
#49923 = EDGE_CURVE ( 'NONE', #42477, #25606, #21151, .T. ) ;
#49924 = LINE ( 'NONE', #38653, #7254 ) ;
#49925 = AXIS2_PLACEMENT_3D ( 'NONE', #40822, #31904, #40563 ) ;
#49926 = CARTESIAN_POINT ( 'NONE',  ( 71.33393739770056641, 11.38381105531911075, -69.84999999999840270 ) ) ;
#49927 = CARTESIAN_POINT ( 'NONE',  ( 41.46604563068979843, 12.80054222763110161, -4.103344234634350052 ) ) ;
#49928 = CARTESIAN_POINT ( 'NONE',  ( 65.09597585808549525, 1.387131204727280132, -70.29242575817399086 ) ) ;
#49929 = CARTESIAN_POINT ( 'NONE',  ( 19.69385247111841153, 24.22507436623365606, -75.39120620925201877 ) ) ;
#49930 = AXIS2_PLACEMENT_3D ( 'NONE', #30684, #46707, #11567 ) ;
#49931 = CARTESIAN_POINT ( 'NONE',  ( 8.222903922732800908, -15.61639209420869889, -32.79233150823699816 ) ) ;
#49932 = CARTESIAN_POINT ( 'NONE',  ( 75.97210306049274209, -43.32603839517573618, -13.61663700222281115 ) ) ;
#49933 = CARTESIAN_POINT ( 'NONE',  ( 57.39341912848639993, 13.88381105532070059, -16.95659913784360029 ) ) ;
#49934 = ORIENTED_EDGE ( 'NONE', *, *, #18249, .F. ) ;
#49935 = ADVANCED_FACE ( 'NONE', ( #45799 ), #31876, .T. ) ;
#49936 = CARTESIAN_POINT ( 'NONE',  ( 14.58992756899499987, -22.90472295277830028, -55.63379137591109469 ) ) ;
#49937 = CARTESIAN_POINT ( 'NONE',  ( 63.60379491233669569, 1.091560265417989894, -61.72337259268859810 ) ) ;
#49938 = VERTEX_POINT ( 'NONE', #49985 ) ;
#49939 = DIRECTION ( 'NONE',  ( 0.000000000000000000, -1.000000000000000000, 0.000000000000000000 ) ) ;
#49940 = CARTESIAN_POINT ( 'NONE',  ( 17.98749078828957337, 10.53025766472752522, -34.79644660940672907 ) ) ;
#49941 = CARTESIAN_POINT ( 'NONE',  ( 18.91091419587250044, -22.09931774463699838, -75.21836123916489214 ) ) ;
#49942 = DIRECTION ( 'NONE',  ( 2.806155971274087206E-29, 5.103645611290830066E-11, -1.000000000000000000 ) ) ;
#49944 = CARTESIAN_POINT ( 'NONE',  ( 9.221486982277522060, -11.63193319550961036, -34.95899771803228617 ) ) ;
#49943 = CARTESIAN_POINT ( 'NONE',  ( 43.60551842263911482, 8.688893774213322985, -68.56980346353216760 ) ) ;
#49945 = CARTESIAN_POINT ( 'NONE',  ( 9.618998415436749383, -18.02038534747480014, -81.23899999999999011 ) ) ;
#49946 = LINE ( 'NONE', #1982, #23580 ) ;
#49947 = ADVANCED_FACE ( 'NONE', ( #46062 ), #5961, .T. ) ;
#49948 = ORIENTED_EDGE ( 'NONE', *, *, #22165, .T. ) ;
#49949 = VERTEX_POINT ( 'NONE', #34498 ) ;
#49950 = ORIENTED_EDGE ( 'NONE', *, *, #28704, .T. ) ;
#49951 = VERTEX_POINT ( 'NONE', #6478 ) ;
#49952 = CARTESIAN_POINT ( 'NONE',  ( 61.23124000452309446, -45.25914701332289525, -46.66814466197200062 ) ) ;
#49953 = DIRECTION ( 'NONE',  ( 0.000000000000000000, 0.000000000000000000, -1.000000000000000000 ) ) ;
#49954 = CARTESIAN_POINT ( 'NONE',  ( 18.11900864776890074, -32.59522544870679894, -35.02873218748179340 ) ) ;
#49955 = AXIS2_PLACEMENT_3D ( 'NONE', #49611, #8992, #13700 ) ;
#49956 = VERTEX_POINT ( 'NONE', #46583 ) ;
#49957 = EDGE_LOOP ( 'NONE', ( #6899, #32366 ) ) ;
#49958 = CARTESIAN_POINT ( 'NONE',  ( 15.24805423083535594, -22.38317868667326493, -72.99443523961514302 ) ) ;
#49959 = CARTESIAN_POINT ( 'NONE',  ( 72.83393739769620367, 1.383811055320669947, -62.79342862858290886 ) ) ;
#49960 = CARTESIAN_POINT ( 'NONE',  ( 17.92370450339669929, -51.11618894467930119, -74.14999999999999147 ) ) ;
#49961 = ORIENTED_EDGE ( 'NONE', *, *, #16301, .T. ) ;
#49962 = DIRECTION ( 'NONE',  ( 0.05886216378194202015, 0.000000000000000000, 0.9982661196669493364 ) ) ;
#49963 = CARTESIAN_POINT ( 'NONE',  ( 52.19766841848610284, -50.16895301260710482, -76.74438382457309160 ) ) ;
#49964 = CARTESIAN_POINT ( 'NONE',  ( 60.62574835426579511, 14.40422389669799941, -47.47763332278800164 ) ) ;
#49965 = CONICAL_SURFACE ( 'NONE', #18158, 1.079032500000002059, 0.7853981633974469467 ) ;
#49966 = CARTESIAN_POINT ( 'NONE',  ( 10.53189742092200021, -10.12038184378820027, -69.25944751885370465 ) ) ;
#49967 = CARTESIAN_POINT ( 'NONE',  ( 2.422700639432810110, -5.409992334431690253, -35.02127583263639821 ) ) ;
#49968 = CARTESIAN_POINT ( 'NONE',  ( 41.12781764322979683, 13.68286643970050065, -5.505755319031189643 ) ) ;
#49969 = CARTESIAN_POINT ( 'NONE',  ( 41.35854777540759386, -44.05358766536809867, -3.852418435177789924 ) ) ;
#49970 = CARTESIAN_POINT ( 'NONE',  ( 29.99034385824719706, -15.61618894467929941, -24.14999999999999858 ) ) ;
#49971 = CARTESIAN_POINT ( 'NONE',  ( -4.967261132674519963, 16.44508974743529706, -5.583919853821729617 ) ) ;
#49972 = CARTESIAN_POINT ( 'NONE',  ( 64.76690267173279381, 1.308988796301270074, -70.38513104616750127 ) ) ;
#49973 = CARTESIAN_POINT ( 'NONE',  ( 15.17121401173929485, -22.60301372889673388, -33.39076563757389948 ) ) ;
#49974 = EDGE_LOOP ( 'NONE', ( #21042, #855, #4836, #24911 ) ) ;
#49976 = EDGE_CURVE ( 'NONE', #41163, #41111, #46321, .T. ) ;
#49975 = CARTESIAN_POINT ( 'NONE',  ( 14.80537258320890004, -52.82751997460400162, -76.12812327221449493 ) ) ;
#49977 = CARTESIAN_POINT ( 'NONE',  ( 57.33486091049710609, 19.16628497504979833, -53.00729108527669808 ) ) ;
#49978 = EDGE_CURVE ( 'NONE', #9812, #30733, #6135, .T. ) ;
#49979 = CARTESIAN_POINT ( 'NONE',  ( 9.188454688893768818, 32.78433166890278727, -46.76666145959791265 ) ) ;
#49980 = CARTESIAN_POINT ( 'NONE',  ( 53.63393739769619373, 21.88381105532059934, 11.84999999999999964 ) ) ;
#49981 = CARTESIAN_POINT ( 'NONE',  ( 47.14844574785740150, -54.72867718618289956, -74.72768729699521373 ) ) ;
#49982 = CARTESIAN_POINT ( 'NONE',  ( 63.41989057163110743, 1.369544300367010026, -68.78354504031220529 ) ) ;
#49983 = CARTESIAN_POINT ( 'NONE',  ( 48.21897519948650057, -54.20455510793630083, -54.75400547047010491 ) ) ;
#49984 = DIRECTION ( 'NONE',  ( 0.9741140340359945027, 0.000000000000000000, 0.2260571801428156169 ) ) ;
#49985 = CARTESIAN_POINT ( 'NONE',  ( 2.458146360389370511, -25.65221394861527671, -34.79644291222910368 ) ) ;
#49986 = CARTESIAN_POINT ( 'NONE',  ( 47.94507101407240413, 23.10143656816769919, -54.74296229181740614 ) ) ;
#49987 = ORIENTED_EDGE ( 'NONE', *, *, #13250, .F. ) ;
#49988 = CARTESIAN_POINT ( 'NONE',  ( 17.65356943138449708, -22.50337107214560106, -77.27805344681910071 ) ) ;
#49989 = ORIENTED_EDGE ( 'NONE', *, *, #50060, .T. ) ;
#49990 = B_SPLINE_SURFACE_WITH_KNOTS ( 'NONE', 3, 3, ( 
 ( #16832, #40932, #12915, #19968, #12646, #48287, #325, #40163, #44348, #8455 ),
 ( #24402, #4776, #44095, #39911, #8195, #28871, #20228, #28605, #21006, #1100 ),
 ( #40416, #5047, #36730, #17099, #48808, #12382, #24138, #44872, #33051, #35965 ),
 ( #4509, #838, #48035, #36216, #20479, #49077, #32514, #16310, #28342, #29131 ) ),
 .UNSPECIFIED., .F., .F., .F.,
 ( 4, 4 ),
 ( 4, 1, 1, 1, 1, 1, 1, 4 ),
 ( -1.508899358212140163, -1.485879941667409998 ),
 ( -1.180912899999999983E-08, 0.1428571428571430157, 0.2857142857142860315, 0.4285714285714289917, 0.5714285714285709528, 0.7142857142857139685, 0.8571428571428569843, 1.000000000000000000 ),
 .UNSPECIFIED. ) ;
#49991 = CARTESIAN_POINT ( 'NONE',  ( 16.13393739769620083, -15.61618894467929941, -20.58999999999999986 ) ) ;
#49992 = AXIS2_PLACEMENT_3D ( 'NONE', #20179, #8657, #40113 ) ;
#49993 = FACE_OUTER_BOUND ( 'NONE', #27563, .T. ) ;
#49994 = CARTESIAN_POINT ( 'NONE',  ( 64.43393739769619799, 11.38381105532070059, -62.44999999999999574 ) ) ;
#49996 = CARTESIAN_POINT ( 'NONE',  ( 52.92421614290409337, 18.24372338732509746, -27.16729016564240240 ) ) ;
#49995 = CARTESIAN_POINT ( 'NONE',  ( 83.01976156432699838, 14.15119948029169983, -47.45812318453789658 ) ) ;
#49997 = CARTESIAN_POINT ( 'NONE',  ( 11.09655785439759867, -20.55252016947139992, -79.20604505178991417 ) ) ;
#49998 = CARTESIAN_POINT ( 'NONE',  ( 9.366633833501754935, -15.85814187007113851, -79.83580626949178338 ) ) ;
#49999 = CARTESIAN_POINT ( 'NONE',  ( 55.68773921495960622, -45.11618894467940066, -14.55197505337829966 ) ) ;
#50000 = EDGE_CURVE ( 'NONE', #49749, #38938, #14335, .T. ) ;
#50001 = ORIENTED_EDGE ( 'NONE', *, *, #12422, .F. ) ;
#50002 = CARTESIAN_POINT ( 'NONE',  ( 62.63393739769619373, -53.11618894467930119, 10.84999999999999964 ) ) ;
#50003 = EDGE_LOOP ( 'NONE', ( #25848, #25549, #8446, #41311, #37161 ) ) ;
#50004 = EDGE_CURVE ( 'NONE', #37063, #3350, #11150, .T. ) ;
#50005 = VERTEX_POINT ( 'NONE', #47355 ) ;
#50006 = CARTESIAN_POINT ( 'NONE',  ( 12.28024544113980099, -64.62291823860830675, -15.84304030210369874 ) ) ;
#50007 = LINE ( 'NONE', #30324, #49149 ) ;
#50008 = DIRECTION ( 'NONE',  ( 1.000000000000000000, 0.000000000000000000, 0.000000000000000000 ) ) ;
#50009 = CARTESIAN_POINT ( 'NONE',  ( 9.758904647714020442, -64.50914077245040801, -46.91371261844790297 ) ) ;
#50010 = ORIENTED_EDGE ( 'NONE', *, *, #16319, .T. ) ;
#50011 = ORIENTED_EDGE ( 'NONE', *, *, #24110, .T. ) ;
#50012 = CARTESIAN_POINT ( 'NONE',  ( -10.12945549441239912, -44.87173451821930570, -43.73795196952299591 ) ) ;
#50013 = CARTESIAN_POINT ( 'NONE',  ( 63.93393739769613404, 11.38381105532129922, -68.84999999999941167 ) ) ;
#50014 = CARTESIAN_POINT ( 'NONE',  ( 53.57971248429669942, 18.11494520363680039, -49.11439736689410296 ) ) ;
#50015 = CARTESIAN_POINT ( 'NONE',  ( 64.37314994972929583, -0.8120157797042090175, -16.48846350816869943 ) ) ;
#50016 = CARTESIAN_POINT ( 'NONE',  ( 51.81521015446659817, -50.18342081774120089, -76.50775191966720001 ) ) ;
#50017 = CARTESIAN_POINT ( 'NONE',  ( 57.10526040051080088, -50.46725872370470256, -52.98753066802770206 ) ) ;
#50018 = ORIENTED_EDGE ( 'NONE', *, *, #27493, .T. ) ;
#50019 = CARTESIAN_POINT ( 'NONE',  ( 24.04315726994194335, -15.44410872182987582, -33.78540739674929938 ) ) ;
#50020 = DIRECTION ( 'NONE',  ( 1.000000000000000000, 0.000000000000000000, 0.000000000000000000 ) ) ;
#50021 = ORIENTED_EDGE ( 'NONE', *, *, #17254, .T. ) ;
#50022 = CARTESIAN_POINT ( 'NONE',  ( 15.09849901009799211, -7.705175762525661831, -56.96600136960869776 ) ) ;
#50023 = CARTESIAN_POINT ( 'NONE',  ( 11.63393739769619906, -41.61618894467930119, -54.64999999999999858 ) ) ;
#50024 = CARTESIAN_POINT ( 'NONE',  ( 23.08008446722849882, -19.26828265651219851, -42.16657309509579932 ) ) ;
#50025 = CARTESIAN_POINT ( 'NONE',  ( 13.77851400210420074, -50.96568734215840379, -21.81884038058960229 ) ) ;
#50026 = CARTESIAN_POINT ( 'NONE',  ( 56.90585954735670526, 19.41242710917140002, -74.35847077477819767 ) ) ;
#50027 = CARTESIAN_POINT ( 'NONE',  ( 47.42016093597910498, -54.35903067314299619, -75.11917674890220553 ) ) ;
#50028 = VERTEX_POINT ( 'NONE', #39734 ) ;
#50029 = CARTESIAN_POINT ( 'NONE',  ( 55.70104770110099679, 14.66019162433090095, -16.90779946243160126 ) ) ;
#50030 = FACE_OUTER_BOUND ( 'NONE', #14683, .T. ) ;
#50031 = CARTESIAN_POINT ( 'NONE',  ( 22.90118952179220813, -15.61618876469732875, -46.84717865327674247 ) ) ;
#50032 = VECTOR ( 'NONE', #12970, 1000.000000000000000 ) ;
#50033 = CARTESIAN_POINT ( 'NONE',  ( 10.40182605014470063, -11.50699697134410115, -40.04515584691789343 ) ) ;
#50034 = CARTESIAN_POINT ( 'NONE',  ( 22.41796512503769989, 0.7774003680457489684, -74.14999999999999147 ) ) ;
#50035 = VERTEX_POINT ( 'NONE', #19552 ) ;
#50037 = EDGE_CURVE ( 'NONE', #33088, #4775, #51851, .T. ) ;
#50036 = CARTESIAN_POINT ( 'NONE',  ( 46.40063036093010140, 21.74762169565689973, -76.14870948285189911 ) ) ;
#50038 = CARTESIAN_POINT ( 'NONE',  ( 65.05161336175049769, 1.196343736543249880, -60.62426770491639871 ) ) ;
#50039 = CARTESIAN_POINT ( 'NONE',  ( 61.22429803220455824, -45.61587231938426612, -47.69140452323649271 ) ) ;
#50040 = CARTESIAN_POINT ( 'NONE',  ( 68.13393739769658453, -28.80002732851820468, -102.2016796975550079 ) ) ;
#50041 = CARTESIAN_POINT ( 'NONE',  ( 50.95182575631829991, -50.95090194773979420, -78.14999999999999147 ) ) ;
#50042 = DIRECTION ( 'NONE',  ( 0.000000000000000000, 0.000000000000000000, -1.000000000000000000 ) ) ;
#50043 = CARTESIAN_POINT ( 'NONE',  ( 82.75628319263068988, 14.36882076953894050, -47.67910150642000389 ) ) ;
#50044 = CARTESIAN_POINT ( 'NONE',  ( -5.166791919687259593, 17.14663772333980063, -39.25848487190110347 ) ) ;
#50046 = CARTESIAN_POINT ( 'NONE',  ( 47.72980687449361881, -39.38200829285558058, -51.96765182151883522 ) ) ;
#50045 = CARTESIAN_POINT ( 'NONE',  ( 64.99525386628140211, 0.8838110553206740549, -60.53635606803790381 ) ) ;
#50047 = CARTESIAN_POINT ( 'NONE',  ( 8.486156673604268619, -13.29521644607133801, -70.60117058448025773 ) ) ;
#50048 = CARTESIAN_POINT ( 'NONE',  ( -29.90810223010410240, 4.891254745981789220, -56.68161292995529976 ) ) ;
#50049 = ORIENTED_EDGE ( 'NONE', *, *, #3071, .F. ) ;
#50050 = CARTESIAN_POINT ( 'NONE',  ( 52.97367367441350439, -49.59674172301600237, -48.91755411389170405 ) ) ;
#50051 = B_SPLINE_CURVE_WITH_KNOTS ( 'NONE', 3,
 ( #39719, #27652, #22682, #35265, #34735, #19796, #30800, #26879, #23188, #11437 ),
 .UNSPECIFIED., .F., .F.,
 ( 4, 1, 1, 1, 1, 1, 1, 4 ),
 ( 0.5000014761122578699, 0.5444555141086205863, 0.6236744451722389115, 0.7028933762358566817, 0.7821123072994755621, 0.8613312383630933322, 0.9405501694267122126, 1.000000000000000000 ),
 .UNSPECIFIED. ) ;
#50052 = VERTEX_POINT ( 'NONE', #31583 ) ;
#50053 = CARTESIAN_POINT ( 'NONE',  ( 41.96502951575018159, 8.570278285162954646, -76.32785687310233413 ) ) ;
#50054 = CARTESIAN_POINT ( 'NONE',  ( 53.70552627772385534, -51.31509389902640095, -75.56421117895261830 ) ) ;
#50055 = CARTESIAN_POINT ( 'NONE',  ( 57.44728655615209334, 13.96276471381350071, -25.73862226050399826 ) ) ;
#50056 = CARTESIAN_POINT ( 'NONE',  ( 11.16602909665550136, -20.62242963097040160, -47.20159690208769376 ) ) ;
#50057 = CARTESIAN_POINT ( 'NONE',  ( 50.61163702139570120, 19.09625748281729685, -76.14999999999999147 ) ) ;
#50058 = CARTESIAN_POINT ( 'NONE',  ( 53.34806562330150115, 18.23528164705630061, -49.15545160539839742 ) ) ;
#50059 = CARTESIAN_POINT ( 'NONE',  ( 64.68925548900161004, 0.9369374701296400154, -60.73727483855509490 ) ) ;
#50060 = EDGE_CURVE ( 'NONE', #19900, #49606, #27675, .T. ) ;
#50061 = FACE_OUTER_BOUND ( 'NONE', #41178, .T. ) ;
#50062 = ORIENTED_EDGE ( 'NONE', *, *, #35261, .T. ) ;
#50063 = CARTESIAN_POINT ( 'NONE',  ( 22.61907617509890045, -11.94880985653349903, -72.90351834778009277 ) ) ;
#50064 = ADVANCED_FACE ( 'NONE', ( #39485 ), #43412, .T. ) ;
#50065 = CARTESIAN_POINT ( 'NONE',  ( 53.29384558423090112, -50.54670888882439783, -48.47378032971909789 ) ) ;
#50066 = CARTESIAN_POINT ( 'NONE',  ( 24.04460491192063998, -15.61619351124008404, -49.79233069347445451 ) ) ;
#50067 = CARTESIAN_POINT ( 'NONE',  ( 72.93868606741401095, 1.327097482837290121, -62.49054404195729973 ) ) ;
#50068 = CARTESIAN_POINT ( 'NONE',  ( 11.73319001777059967, -65.42240559785089715, -18.17421237902190256 ) ) ;
#50069 = CARTESIAN_POINT ( 'NONE',  ( 52.86023839377149613, 18.41257215013510162, -48.64479331233690829 ) ) ;
#50070 = CARTESIAN_POINT ( 'NONE',  ( 8.222342146248220018, -15.61610160653870061, -76.79233150823698395 ) ) ;
#50071 = CARTESIAN_POINT ( 'NONE',  ( 71.34267188602959209, 0.8850831926798620186, -60.57999765399169689 ) ) ;
#50072 = CIRCLE ( 'NONE', #28303, 24.00000000000000000 ) ;
#50073 = FACE_OUTER_BOUND ( 'NONE', #35654, .T. ) ;
#50074 = CARTESIAN_POINT ( 'NONE',  ( 64.95255690645950608, 1.266538207494809942, -70.53881316596870477 ) ) ;
#50075 = VERTEX_POINT ( 'NONE', #40247 ) ;
#50076 = CARTESIAN_POINT ( 'NONE',  ( 9.735166606402680500, -63.19548571361389833, -46.29854363928350125 ) ) ;
#50077 = CARTESIAN_POINT ( 'NONE',  ( 24.04518460902906085, -15.61618869790763675, -47.79232989768991757 ) ) ;
#50078 = ORIENTED_EDGE ( 'NONE', *, *, #518, .F. ) ;
#50079 = CARTESIAN_POINT ( 'NONE',  ( 3.768317948728551858, -8.476895227121387322, -34.64999999999999858 ) ) ;
#50080 = CARTESIAN_POINT ( 'NONE',  ( 57.25486274975099832, 19.18878419988909911, -53.00955584377039287 ) ) ;
#50081 = CARTESIAN_POINT ( 'NONE',  ( 8.222431652840050731, -15.61631456792169992, -70.50766849176299900 ) ) ;
#50082 = CARTESIAN_POINT ( 'NONE',  ( 53.44459215460110357, 19.29420487410069995, -77.05819720518759652 ) ) ;
#50083 = VERTEX_POINT ( 'NONE', #36296 ) ;
#50084 = LINE ( 'NONE', #34335, #15729 ) ;
#50085 = DIRECTION ( 'NONE',  ( -0.7071067811865475727, 0.7071067811865475727, 0.000000000000000000 ) ) ;
#50086 = LINE ( 'NONE', #33823, #50261 ) ;
#50087 = CARTESIAN_POINT ( 'NONE',  ( 24.04424255568759961, -15.50293698162811040, -43.78776901094543206 ) ) ;
#50088 = CARTESIAN_POINT ( 'NONE',  ( 22.87440586111459950, -20.36474714160580035, -53.98768771411489098 ) ) ;
#50089 = CARTESIAN_POINT ( 'NONE',  ( 20.99566323537737134, -21.94231603232962513, -47.79933614068776393 ) ) ;
#50090 = CARTESIAN_POINT ( 'NONE',  ( 45.26653699117287033, -38.07366123800876068, -63.98696205713867613 ) ) ;
#50091 = EDGE_LOOP ( 'NONE', ( #35862, #15181, #46712, #15562, #27422, #7025, #12563, #37175, #2236 ) ) ;
#50092 = CARTESIAN_POINT ( 'NONE',  ( 56.90686501081929549, -45.95685669975489418, -26.24565630313109921 ) ) ;
#50093 = CARTESIAN_POINT ( 'NONE',  ( 23.57447716569279805, -15.99705869407809899, -48.24893689645459460 ) ) ;
#50094 = CARTESIAN_POINT ( 'NONE',  ( 53.41295794315580281, -49.45825314767390068, -49.19565172947730503 ) ) ;
#50095 = CARTESIAN_POINT ( 'NONE',  ( 9.970633004574349201, -12.25822725531089930, -32.14999999999999858 ) ) ;
#50096 = EDGE_CURVE ( 'NONE', #19315, #21614, #36818, .T. ) ;
#50097 = CARTESIAN_POINT ( 'NONE',  ( 13.48116775261750000, 20.36472114263469990, -74.14993923597720027 ) ) ;
#50098 = B_SPLINE_CURVE_WITH_KNOTS ( 'NONE', 3,
 ( #27501, #7606, #23554, #8115, #20400, #24061, #36142, #16745, #32698, #4432, #9148, #16481, #40082, #40588, #48725, #12827, #243, #1 ),
 .UNSPECIFIED., .F., .F.,
 ( 4, 2, 2, 2, 2, 2, 2, 2, 4 ),
 ( 0.000000000000000000, 0.06250000040564351877, 0.1250000008112870375, 0.1875000012169305563, 0.2500000016225740751, 0.3125000020282175939, 0.3750000024338611126, 0.4375000028395046314, 0.5000000032451481502 ),
 .UNSPECIFIED. ) ;
#50099 = EDGE_CURVE ( 'NONE', #50028, #44136, #33434, .T. ) ;
#50100 = CARTESIAN_POINT ( 'NONE',  ( 9.807862442681825499, -10.75439508610775974, -51.00066430329498957 ) ) ;
#50101 = ADVANCED_FACE ( 'NONE', ( #28172 ), #9307, .F. ) ;
#50102 = CARTESIAN_POINT ( 'NONE',  ( 45.96729298043059941, -45.11618877348409740, -7.679810998475620210 ) ) ;
#50103 = CARTESIAN_POINT ( 'NONE',  ( 24.04360322966152452, -15.45924965371268556, -61.50136194718664484 ) ) ;
#50104 = AXIS2_PLACEMENT_3D ( 'NONE', #29957, #46244, #45975 ) ;
#50105 = EDGE_CURVE ( 'NONE', #7343, #49436, #24204, .T. ) ;
#50107 = CIRCLE ( 'NONE', #45922, 20.00000000000000355 ) ;
#50106 = CARTESIAN_POINT ( 'NONE',  ( 14.89443207003930070, -23.76765183496380018, -66.05570249522899928 ) ) ;
#50108 = ORIENTED_EDGE ( 'NONE', *, *, #36196, .F. ) ;
#50109 = CARTESIAN_POINT ( 'NONE',  ( 52.66238559624279958, -49.77034287296790183, -28.15000000000000213 ) ) ;
#50110 = CARTESIAN_POINT ( 'NONE',  ( 54.51194644580689896, -51.02658531394220631, -75.53932869989588994 ) ) ;
#50112 = DIRECTION ( 'NONE',  ( -0.7071067811865476838, -0.7071067811865473507, 0.000000000000000000 ) ) ;
#50111 = CARTESIAN_POINT ( 'NONE',  ( 2.523152121134959902, 24.51152417802100203, -9.568711433707859371 ) ) ;
#50113 = CARTESIAN_POINT ( 'NONE',  ( 14.13958958332026583, -32.60348064536626111, -35.06583844469490430 ) ) ;
#50114 = FACE_OUTER_BOUND ( 'NONE', #8277, .T. ) ;
#50115 = ORIENTED_EDGE ( 'NONE', *, *, #10663, .F. ) ;
#50116 = CARTESIAN_POINT ( 'NONE',  ( 29.13393739769619728, -33.99486860111965569, -83.77132034355965118 ) ) ;
#50117 = CARTESIAN_POINT ( 'NONE',  ( 47.45089865496730397, 23.39580635657319974, -54.92520380177580108 ) ) ;
#50118 = DIRECTION ( 'NONE',  ( 0.000000000000000000, 1.000000000000000000, 0.000000000000000000 ) ) ;
#50119 = CARTESIAN_POINT ( 'NONE',  ( 84.44784216359251161, -43.11618894467930119, -47.47585302082339354 ) ) ;
#50120 = CARTESIAN_POINT ( 'NONE',  ( 16.13393739769620083, -15.61618894467929941, 7.849999999999999645 ) ) ;
#50121 = CARTESIAN_POINT ( 'NONE',  ( 11.51020347527180121, 33.95873866478400060, -17.03655015074090073 ) ) ;
#50122 = CARTESIAN_POINT ( 'NONE',  ( 51.63018455917120519, 17.53790506105039881, -76.93968096218729613 ) ) ;
#50123 = DIRECTION ( 'NONE',  ( 0.000000000000000000, -1.000000000000000000, 0.000000000000000000 ) ) ;
#50124 = FACE_OUTER_BOUND ( 'NONE', #50718, .T. ) ;
#50125 = CARTESIAN_POINT ( 'NONE',  ( 57.24929578232330130, -50.61618894764249887, -53.91492796143979405 ) ) ;
#50126 = CARTESIAN_POINT ( 'NONE',  ( 54.58029846603599822, 16.81705030249620236, -26.70560246487150025 ) ) ;
#50127 = CARTESIAN_POINT ( 'NONE',  ( 53.69314142483850105, 20.72471266374249765, -54.13035041278149606 ) ) ;
#50128 = EDGE_CURVE ( 'NONE', #8243, #38406, #15887, .T. ) ;
#50129 = CARTESIAN_POINT ( 'NONE',  ( 63.40807272917960091, 0.9828896327562162138, -69.34788335338460286 ) ) ;
#50130 = CARTESIAN_POINT ( 'NONE',  ( 12.16177399482889854, -65.11171494345551025, -16.53048058985559976 ) ) ;
#50131 = FACE_OUTER_BOUND ( 'NONE', #12836, .T. ) ;
#50132 = DIRECTION ( 'NONE',  ( -0.3535533905932731202, -0.6123724356957964687, 0.7071067811865462405 ) ) ;
#50133 = CARTESIAN_POINT ( 'NONE',  ( 10.98008937475129976, 32.20858435228970507, -44.74889856825390666 ) ) ;
#50134 = DIRECTION ( 'NONE',  ( 0.000000000000000000, -1.000000000000000000, 0.000000000000000000 ) ) ;
#50135 = CARTESIAN_POINT ( 'NONE',  ( 66.86287292282169403, -33.02813482287280067, -19.74633365862219847 ) ) ;
#50136 = CARTESIAN_POINT ( 'NONE',  ( 9.903862192720572111, -10.68226006460541555, -80.72097351600584147 ) ) ;
#50137 = ORIENTED_EDGE ( 'NONE', *, *, #7315, .F. ) ;
#50138 = ORIENTED_EDGE ( 'NONE', *, *, #30748, .T. ) ;
#50139 = DIRECTION ( 'NONE',  ( 0.8857883891771971552, 0.4640893551880569956, 0.000000000000000000 ) ) ;
#50140 = CARTESIAN_POINT ( 'NONE',  ( 76.52646094036225577, -1.396720341220584194, -13.34144236586088184 ) ) ;
#50141 = ORIENTED_EDGE ( 'NONE', *, *, #35145, .F. ) ;
#50142 = CARTESIAN_POINT ( 'NONE',  ( 11.45649489523620090, -64.61824938533239049, -44.81425297044399514 ) ) ;
#50143 = CARTESIAN_POINT ( 'NONE',  ( 57.45125141795639934, -45.60879174519349988, -26.20535967303949931 ) ) ;
#50144 = CARTESIAN_POINT ( 'NONE',  ( 4.133937397696209715, -8.687985714403829718, -35.14999999999999858 ) ) ;
#50145 = CARTESIAN_POINT ( 'NONE',  ( 63.54027722212589424, 1.395196698723379924, -62.46966344801359838 ) ) ;
#50146 = VERTEX_POINT ( 'NONE', #8018 ) ;
#50147 = CARTESIAN_POINT ( 'NONE',  ( 9.367442997458502063, -15.61610373232760018, -47.45282021618999835 ) ) ;
#50148 = AXIS2_PLACEMENT_3D ( 'NONE', #22293, #17860, #13435 ) ;
#50149 = EDGE_CURVE ( 'NONE', #39508, #44049, #48634, .T. ) ;
#50150 = CARTESIAN_POINT ( 'NONE',  ( 47.13393739769619373, 7.029298498933709283, -54.64999999999999858 ) ) ;
#50151 = VECTOR ( 'NONE', #46444, 1000.000000000000000 ) ;
#50152 = AXIS2_PLACEMENT_3D ( 'NONE', #20467, #36455, #16549 ) ;
#50153 = ORIENTED_EDGE ( 'NONE', *, *, #28621, .T. ) ;
#50154 = CARTESIAN_POINT ( 'NONE',  ( 47.86554978023400508, -45.20111752495729718, -9.670171237329979519 ) ) ;
#50155 = DIRECTION ( 'NONE',  ( 0.000000000000000000, 1.000000000000000000, 0.000000000000000000 ) ) ;
#50156 = CARTESIAN_POINT ( 'NONE',  ( 16.29169529782900128, 19.88381334967050051, -21.10106358377919733 ) ) ;
#50157 = LINE ( 'NONE', #5873, #12581 ) ;
#50158 = CARTESIAN_POINT ( 'NONE',  ( 22.68269334052732944, -17.37751627684776068, -46.53645479080106639 ) ) ;
#50159 =( BOUNDED_SURFACE ( )  B_SPLINE_SURFACE ( 2, 2, ( 
 ( #21947, #2311, #26925 ),
 ( #37957, #18034, #50013 ),
 ( #46354, #6507, #26140 ) ),
 .UNSPECIFIED., .F., .F., .T. ) 
 B_SPLINE_SURFACE_WITH_KNOTS ( ( 3, 3 ),
 ( 3, 3 ),
 ( -7.280321556379879384E-13, 1.570796326795560027 ),
 ( -3.141592653588870299, -1.570796326795379949 ),
 .UNSPECIFIED. ) 
 GEOMETRIC_REPRESENTATION_ITEM ( )  RATIONAL_B_SPLINE_SURFACE ( (
 ( 1.000000000000000000, 0.7071067811870440645, 1.000000000000000000),
 ( 0.7071067811860539676, 0.5000000000000000000, 0.7071067811860539676),
 ( 1.000000000000000000, 0.7071067811870440645, 1.000000000000000000) ) ) 
 REPRESENTATION_ITEM ( '' )  SURFACE ( )  );
#50160 = CARTESIAN_POINT ( 'NONE',  ( 73.13041444294910320, 0.8910129994591539093, -68.97194292341539779 ) ) ;
#50161 = CARTESIAN_POINT ( 'NONE',  ( 46.54186286179869825, -53.33175941191459657, -76.10201724918678678 ) ) ;
#50162 = CARTESIAN_POINT ( 'NONE',  ( 43.10178961967590539, 13.88381303978850134, -6.597083906273729426 ) ) ;
#50163 = CARTESIAN_POINT ( 'NONE',  ( 52.88720174400599916, 13.88381105532070059, -12.35033059861759952 ) ) ;
#50164 = EDGE_CURVE ( 'NONE', #19246, #20846, #34369, .T. ) ;
#50165 = CYLINDRICAL_SURFACE ( 'NONE', #20007, 0.4999999999999982236 ) ;
#50166 = EDGE_CURVE ( 'NONE', #12686, #35762, #46145, .T. ) ;
#50167 = CARTESIAN_POINT ( 'NONE',  ( 53.09964054308650105, 20.18306253101129855, -75.69942035651190793 ) ) ;
#50168 = CARTESIAN_POINT ( 'NONE',  ( 58.00476136467050026, 13.88377196530409918, -25.49213187376239986 ) ) ;
#50169 = ADVANCED_FACE ( 'NONE', ( #1709 ), #18489, .F. ) ;
#50170 = CARTESIAN_POINT ( 'NONE',  ( 8.138816769778330240, -13.60105449406839995, -36.58626013956259726 ) ) ;
#50171 = ORIENTED_EDGE ( 'NONE', *, *, #40471, .F. ) ;
#50172 = LINE ( 'NONE', #10081, #41399 ) ;
#50173 = CARTESIAN_POINT ( 'NONE',  ( -0.2744351088561370333, -53.43781633194900138, -9.661156741874108889 ) ) ;
#50174 = CARTESIAN_POINT ( 'NONE',  ( 8.222937397696199469, -15.61618894467929941, -32.14999999999999858 ) ) ;
#50175 = CARTESIAN_POINT ( 'NONE',  ( 72.97035904602149969, 1.134292167764390014, -69.12140099273041471 ) ) ;
#50176 = FACE_OUTER_BOUND ( 'NONE', #30834, .T. ) ;
#50177 = AXIS2_PLACEMENT_3D ( 'NONE', #24034, #43731, #20373 ) ;
#50178 = AXIS2_PLACEMENT_3D ( 'NONE', #26552, #22620, #13751 ) ;
#50179 = CARTESIAN_POINT ( 'NONE',  ( 16.81199894099719927, -16.95676073769629610, -35.14999999999999858 ) ) ;
#50180 = AXIS2_PLACEMENT_3D ( 'NONE', #46730, #22582, #34114 ) ;
#50181 = CARTESIAN_POINT ( 'NONE',  ( 23.17687047303220638, -11.91936411872809920, -65.35394111064542244 ) ) ;
#50182 = CARTESIAN_POINT ( 'NONE',  ( 13.52985239415419905, 18.98897015258729937, -21.01296976105329861 ) ) ;
#50183 = CARTESIAN_POINT ( 'NONE',  ( 11.51160566532330165, 19.89559162839070083, -23.15000000000000213 ) ) ;
#50184 = AXIS2_PLACEMENT_3D ( 'NONE', #21861, #29470, #1446 ) ;
#50185 = CARTESIAN_POINT ( 'NONE',  ( 43.12694253603230266, 11.52171575524780067, -4.223455518406679765 ) ) ;
#50186 = CARTESIAN_POINT ( 'NONE',  ( 47.26610112325450075, -54.05804861832230301, -75.56421356201970241 ) ) ;
#50187 = DIRECTION ( 'NONE',  ( 0.000000000000000000, 0.000000000000000000, -1.000000000000000000 ) ) ;
#50188 = CARTESIAN_POINT ( 'NONE',  ( 19.97369125467840334, -22.99931529436689814, -35.14999999999999858 ) ) ;
#50189 = CARTESIAN_POINT ( 'NONE',  ( 75.82340458658627824, -43.34274047612557013, -13.53568841794259825 ) ) ;
#50191 = ADVANCED_FACE ( 'NONE', ( #44434 ), #45479, .F. ) ;
#50190 = DIRECTION ( 'NONE',  ( 0.6339889056055382222, 0.000000000000000000, -0.7733421413379021336 ) ) ;
#50192 = ORIENTED_EDGE ( 'NONE', *, *, #2134, .T. ) ;
#50193 = CARTESIAN_POINT ( 'NONE',  ( 16.05054682600030347, -8.166374158331009880, -50.56377978783940108 ) ) ;
#50194 = CARTESIAN_POINT ( 'NONE',  ( 63.54511136546258854, 1.080095028449789885, -61.79280233996579597 ) ) ;
#50195 = EDGE_LOOP ( 'NONE', ( #13136, #7475 ) ) ;
#50196 = CARTESIAN_POINT ( 'NONE',  ( 5.772828151193539981, 28.52800643874740061, -13.89629191288699950 ) ) ;
#50197 = DIRECTION ( 'NONE',  ( 1.000000000000000000, 0.000000000000000000, 0.000000000000000000 ) ) ;
#50198 = CARTESIAN_POINT ( 'NONE',  ( 16.13393739769620083, -15.61618894467929941, 8.349999999999999645 ) ) ;
#50199 = CARTESIAN_POINT ( 'NONE',  ( 65.01767771978660448, 0.8838110553206759423, -70.77727272727270247 ) ) ;
#50200 = CARTESIAN_POINT ( 'NONE',  ( 45.68005094484422557, 8.842359151983487209, -58.51315632734830530 ) ) ;
#50201 = CARTESIAN_POINT ( 'NONE',  ( 9.402037793986869119, -17.49569968449790025, -81.23899999999999011 ) ) ;
#50202 = CARTESIAN_POINT ( 'NONE',  ( 45.07859124156069441, -46.11251916928470251, -9.026881350141310989 ) ) ;
#50203 = VERTEX_POINT ( 'NONE', #33662 ) ;
#50204 = ORIENTED_EDGE ( 'NONE', *, *, #7176, .F. ) ;
#50205 = B_SPLINE_CURVE_WITH_KNOTS ( 'NONE', 3,
 ( #41630, #30079, #33755, #37966, #41898, #46103, #7551, #30598, #6779, #19073, #3106, #39010, #35046, #47393, #47638, #42683, #51055, #27446 ),
 .UNSPECIFIED., .F., .F.,
 ( 4, 2, 2, 2, 2, 2, 2, 2, 4 ),
 ( 0.000000000000000000, 0.06249987509224218946, 0.1249997501844843789, 0.1874996252767265614, 0.2499995003689687578, 0.3124993754612109265, 0.3749992505534531229, 0.4374991256456953193, 0.4999990007379375156 ),
 .UNSPECIFIED. ) ;
#50206 = EDGE_LOOP ( 'NONE', ( #37665, #11351, #11214, #7003 ) ) ;
#50207 = CARTESIAN_POINT ( 'NONE',  ( 61.26666816648369718, -45.24236673898500527, -46.69299359672859850 ) ) ;
#50208 = CARTESIAN_POINT ( 'NONE',  ( 82.74184831039019627, -45.55978498551615274, -47.63392295364009499 ) ) ;
#50209 = EDGE_CURVE ( 'NONE', #44209, #7516, #25444, .T. ) ;
#50210 = ORIENTED_EDGE ( 'NONE', *, *, #38640, .T. ) ;
#50211 = EDGE_LOOP ( 'NONE', ( #22722, #4244, #7080, #28098 ) ) ;
#50212 = CYLINDRICAL_SURFACE ( 'NONE', #39451, 2.999999999999999112 ) ;
#50213 = EDGE_CURVE ( 'NONE', #20534, #30077, #6785, .T. ) ;
#50214 = CARTESIAN_POINT ( 'NONE',  ( 12.72597450771867145, -21.52911656548743480, -53.11948602161462674 ) ) ;
#50215 = CARTESIAN_POINT ( 'NONE',  ( 51.13393739769659874, -50.61618894467899565, 10.84999999999999964 ) ) ;
#50216 = CIRCLE ( 'NONE', #10033, 5.251829701412240148 ) ;
#50217 = AXIS2_PLACEMENT_3D ( 'NONE', #36797, #36023, #16110 ) ;
#50218 = ORIENTED_EDGE ( 'NONE', *, *, #11186, .F. ) ;
#50219 = CARTESIAN_POINT ( 'NONE',  ( 22.02211878048609961, -20.97478655844351891, -49.74279633225222597 ) ) ;
#50220 = CARTESIAN_POINT ( 'NONE',  ( 53.10073094383309211, -50.72614047099949630, -76.45474612258288971 ) ) ;
#50221 = CIRCLE ( 'NONE', #3384, 0.5000000000000004441 ) ;
#50222 = CARTESIAN_POINT ( 'NONE',  ( 60.52368085848160462, 14.45009813934579945, -47.49050240135510137 ) ) ;
#50223 = CIRCLE ( 'NONE', #25907, 2.000000000000001776 ) ;
#50224 = CARTESIAN_POINT ( 'NONE',  ( 18.18784219828660298, -23.19037026424729930, -72.42820476139849006 ) ) ;
#50225 = CARTESIAN_POINT ( 'NONE',  ( 85.66799001034409855, 17.38381105532069881, -61.58097075742929860 ) ) ;
#50226 = CARTESIAN_POINT ( 'NONE',  ( 41.35841886795890332, 13.63164803163950012, -5.517442860631740054 ) ) ;
#50227 = AXIS2_PLACEMENT_3D ( 'NONE', #33229, #18280, #21682 ) ;
#50228 = CARTESIAN_POINT ( 'NONE',  ( 41.57451192618589886, -43.86192582434640030, -3.761783080649049982 ) ) ;
#50229 = CARTESIAN_POINT ( 'NONE',  ( 65.30823784209736971, -0.2426529040835342932, -16.78605341132611883 ) ) ;
#50230 = CARTESIAN_POINT ( 'NONE',  ( 65.03603135454920903, 1.015437840524759938, -17.83403478221330118 ) ) ;
#50231 = ADVANCED_FACE ( 'NONE', ( #14798 ), #30764, .T. ) ;
#50232 = CARTESIAN_POINT ( 'NONE',  ( 64.86559958573539575, 1.367045641526589916, -70.32522074196269557 ) ) ;
#50233 = DIRECTION ( 'NONE',  ( -0.7071067811865470176, 0.000000000000000000, 0.7071067811865480168 ) ) ;
#50234 = DIRECTION ( 'NONE',  ( 0.000000000000000000, -1.000000000000000000, 0.000000000000000000 ) ) ;
#50235 = ADVANCED_FACE ( 'NONE', ( #14538 ), #1969, .T. ) ;
#50236 = ORIENTED_EDGE ( 'NONE', *, *, #917, .F. ) ;
#50237 = SURFACE_SIDE_STYLE ('',( #38179 ) ) ;
#50238 = CARTESIAN_POINT ( 'NONE',  ( 57.36367400179620546, 19.00004687350629951, -52.73881526266769271 ) ) ;
#50239 = CARTESIAN_POINT ( 'NONE',  ( 45.41582150454148348, -40.05831117691089815, -59.79522137358304690 ) ) ;
#50240 = DIRECTION ( 'NONE',  ( 0.000000000000000000, 0.7071067811865457964, 0.7071067811865492381 ) ) ;
#50241 = CARTESIAN_POINT ( 'NONE',  ( 22.08340413664989654, -11.95206882129740045, -32.14999999999999858 ) ) ;
#50242 = CARTESIAN_POINT ( 'NONE',  ( 63.43166809737898859, 1.369719003397489976, -68.81308079741751271 ) ) ;
#50243 = CARTESIAN_POINT ( 'NONE',  ( 48.31044912363459787, -54.24991223489359982, -55.31379430672990338 ) ) ;
#50244 = CARTESIAN_POINT ( 'NONE',  ( 19.43172305940224831, -9.381835016295289265, -50.50205474733376576 ) ) ;
#50245 = CARTESIAN_POINT ( 'NONE',  ( -11.32734370190460105, -41.88171845330919751, -6.430192534648670133 ) ) ;
#50246 = CARTESIAN_POINT ( 'NONE',  ( 17.16943926069780701, -23.52719545942989754, -46.25071487151191008 ) ) ;
#50247 = CARTESIAN_POINT ( 'NONE',  ( 47.77526208095149940, 23.24550361938769782, -55.21131733320120105 ) ) ;
#50248 =( GEOMETRIC_REPRESENTATION_CONTEXT ( 3 ) GLOBAL_UNCERTAINTY_ASSIGNED_CONTEXT ( ( #42636 ) ) GLOBAL_UNIT_ASSIGNED_CONTEXT ( ( #11360, #11618, #27071 ) ) REPRESENTATION_CONTEXT ( 'NONE', 'WORKASPACE' ) );
#50249 = VERTEX_POINT ( 'NONE', #5900 ) ;
#50250 = AXIS2_PLACEMENT_3D ( 'NONE', #43820, #7669, #7918 ) ;
#50251 = CARTESIAN_POINT ( 'NONE',  ( 10.74314122376619984, -11.06845590621349906, -78.07024275745519049 ) ) ;
#50252 = EDGE_LOOP ( 'NONE', ( #2534, #36578, #45823, #13519, #3480 ) ) ;
#50253 = CARTESIAN_POINT ( 'NONE',  ( 71.19138260135351004, 1.383767307422960169, -70.32144070214289400 ) ) ;
#50254 = FACE_OUTER_BOUND ( 'NONE', #11920, .T. ) ;
#50255 = DIRECTION ( 'NONE',  ( 1.000000000000000000, 0.000000000000000000, 0.000000000000000000 ) ) ;
#50256 = CARTESIAN_POINT ( 'NONE',  ( 14.27688361489088464, 19.15751927551417211, -20.83437801695187019 ) ) ;
#50258 = CARTESIAN_POINT ( 'NONE',  ( 52.84013465215829797, 18.33475784595760061, -27.28929192048029861 ) ) ;
#50257 = CARTESIAN_POINT ( 'NONE',  ( 84.05638291250180316, 13.23271651793530168, -47.35165316785450074 ) ) ;
#50259 = AXIS2_PLACEMENT_3D ( 'NONE', #14501, #26802, #42031 ) ;
#50260 = CARTESIAN_POINT ( 'NONE',  ( 17.13677513945059872, -8.635009040899712218, -79.99823436242620289 ) ) ;
#50261 = VECTOR ( 'NONE', #26218, 1000.000000000000000 ) ;
#50262 = LINE ( 'NONE', #42656, #6144 ) ;
#50263 = CARTESIAN_POINT ( 'NONE',  ( 24.04523903120960782, -15.61618918343368101, -41.50766953063602926 ) ) ;
#50264 = DIRECTION ( 'NONE',  ( 0.000000000000000000, 0.000000000000000000, -1.000000000000000000 ) ) ;
#50265 = B_SPLINE_SURFACE_WITH_KNOTS ( 'NONE', 3, 3, ( 
 ( #28377, #8486, #48581, #12682, #45425, #9272 ),
 ( #38075, #42010, #49364, #6109, #17891, #17383 ),
 ( #45943, #45681, #37296, #10297, #22065, #49624 ),
 ( #2172, #21034, #13718, #49875, #18151, #10032 ),
 ( #25999, #17128, #34117, #17644, #25477, #41481 ),
 ( #5596, #50127, #13465, #21551, #33081, #14223 ),
 ( #29672, #30196, #46213, #49110, #40961, #33348 ),
 ( #5079, #29925, #29420, #21812, #37035, #1132 ),
 ( #37547, #33610, #25220, #13209, #29159, #9529 ),
 ( #5339, #9782, #45157, #41224, #21291, #1394 ),
 ( #1652, #25734, #41741, #5847, #37819, #1912 ),
 ( #33864, #13970, #38332, #7397, #43048, #46992 ),
 ( #35420, #30450, #34903, #47242, #23345, #3469 ),
 ( #31215, #18664, #22326, #50393, #30710, #46473 ),
 ( #7145, #15516, #42267, #10559, #35159, #39367 ),
 ( #22838, #19180, #46732, #23097, #11077, #34381 ) ),
 .UNSPECIFIED., .F., .F., .F.,
 ( 4, 2, 2, 2, 2, 2, 2, 4 ),
 ( 4, 1, 1, 4 ),
 ( 0.1345845834583700162, 1.324410793755629978, 2.838023129476340056, 3.784030839301789850, 4.257034694214520520, 5.013840862074870230, 6.224730730651439892, 7.568061678603579701 ),
 ( 0.000000000000000000, 0.3333333333333329818, 0.6666666666666670737, 1.000000000000000000 ),
 .UNSPECIFIED. ) ;
#50266 = VERTEX_POINT ( 'NONE', #34699 ) ;
#50267 = DIRECTION ( 'NONE',  ( -1.000000000000000000, 0.000000000000000000, 0.000000000000000000 ) ) ;
#50268 = ORIENTED_EDGE ( 'NONE', *, *, #5449, .T. ) ;
#50269 = ORIENTED_EDGE ( 'NONE', *, *, #25134, .F. ) ;
#50270 = CYLINDRICAL_SURFACE ( 'NONE', #48720, 7.910999999999997812 ) ;
#50271 = CARTESIAN_POINT ( 'NONE',  ( 10.50324867407785767, -10.02729031740725674, -38.75656930020886648 ) ) ;
#50272 = CARTESIAN_POINT ( 'NONE',  ( 9.543085836910789155, -17.38751520322140820, -55.36948714503900959 ) ) ;
#50273 = CARTESIAN_POINT ( 'NONE',  ( 50.96089686506987704, 4.058150859599502169, -76.37981214989946466 ) ) ;
#50274 = ORIENTED_EDGE ( 'NONE', *, *, #15850, .F. ) ;
#50275 = EDGE_CURVE ( 'NONE', #26913, #13640, #9834, .T. ) ;
#50276 = ORIENTED_EDGE ( 'NONE', *, *, #47000, .T. ) ;
#50277 = CARTESIAN_POINT ( 'NONE',  ( -22.85259296468129975, -18.54880656488629853, -54.73566662495469615 ) ) ;
#50278 = CARTESIAN_POINT ( 'NONE',  ( 57.00663126403959780, 14.67647015083939976, -26.24686370817770253 ) ) ;
#50279 = EDGE_CURVE ( 'NONE', #35817, #16605, #39916, .T. ) ;
#50280 = CARTESIAN_POINT ( 'NONE',  ( 9.404870085045700989, -14.72357982206546900, -45.49475439789830489 ) ) ;
#50281 = CARTESIAN_POINT ( 'NONE',  ( 63.56762109228700552, -1.686163729233590036, -16.28338591870409857 ) ) ;
#50282 = CARTESIAN_POINT ( 'NONE',  ( 51.59929363246539680, -50.34116866607159579, -76.34973346688259710 ) ) ;
#50283 = ADVANCED_FACE ( 'NONE', ( #24170 ), #17400, .F. ) ;
#50284 = CARTESIAN_POINT ( 'NONE',  ( 57.04794059879459667, -50.06337071255109805, -52.46643742010060407 ) ) ;
#50285 = ORIENTED_EDGE ( 'NONE', *, *, #17029, .F. ) ;
#50286 = CARTESIAN_POINT ( 'NONE',  ( 16.15665784884619782, -7.677406726810557913, -33.29332427056172605 ) ) ;
#50287 = CARTESIAN_POINT ( 'NONE',  ( 70.83393739769690001, 16.88381105531960458, -68.79999999999942872 ) ) ;
#50288 = VERTEX_POINT ( 'NONE', #27356 ) ;
#50289 = CARTESIAN_POINT ( 'NONE',  ( 68.13393739769618662, -30.31618894467939995, -65.65000000000000568 ) ) ;
#50290 = CARTESIAN_POINT ( 'NONE',  ( 20.11810762141488595, -22.52868886509989821, -53.84100386235245139 ) ) ;
#50291 = CARTESIAN_POINT ( 'NONE',  ( 13.03098752936530147, -22.82440992535179802, -42.64188668147749439 ) ) ;
#50292 = CARTESIAN_POINT ( 'NONE',  ( 13.45430947954159961, -50.82897305452650016, -21.59563960679350103 ) ) ;
#50293 = CARTESIAN_POINT ( 'NONE',  ( 56.61615004124559647, 19.47122561338359858, -74.49138732573949540 ) ) ;
#50294 = CARTESIAN_POINT ( 'NONE',  ( 47.55554092369170149, -54.54384586952379976, -74.50311761397450994 ) ) ;
#50295 = CARTESIAN_POINT ( 'NONE',  ( 56.96371428459909936, 13.94730734397229988, -17.49295389172720050 ) ) ;
#50296 = CARTESIAN_POINT ( 'NONE',  ( 22.72481174712088858, -13.84494720633589360, -78.36948400686931393 ) ) ;
#50297 = CARTESIAN_POINT ( 'NONE',  ( 56.41694091142689871, -50.57803607321029915, -52.96189704198110348 ) ) ;
#50298 = AXIS2_PLACEMENT_3D ( 'NONE', #7513, #43922, #47605 ) ;
#50299 = CARTESIAN_POINT ( 'NONE',  ( 17.74966129736979781, -22.48146355349690140, -45.27360529711679504 ) ) ;
#50300 = CYLINDRICAL_SURFACE ( 'NONE', #45720, 0.4999999999999991118 ) ;
#50301 = AXIS2_PLACEMENT_3D ( 'NONE', #8625, #21174, #8886 ) ;
#50302 = EDGE_CURVE ( 'NONE', #25155, #2299, #2596, .T. ) ;
#50303 = VERTEX_POINT ( 'NONE', #4037 ) ;
#50304 = CARTESIAN_POINT ( 'NONE',  ( 47.04893601651119894, 22.57350237217389832, -75.82551461053719777 ) ) ;
#50305 = CARTESIAN_POINT ( 'NONE',  ( 65.17314292416639887, 1.382830464309369844, -60.94559068149789738 ) ) ;
#50306 = CARTESIAN_POINT ( 'NONE',  ( 75.16029866046824282, -29.42847402270892232, -11.84778187433581387 ) ) ;
#50307 = CARTESIAN_POINT ( 'NONE',  ( 68.13393739769625768, -15.41618894467990764, -28.20067248431510976 ) ) ;
#50308 = CARTESIAN_POINT ( 'NONE',  ( 54.17308944977700236, 19.38381105532069881, -77.01198594365929750 ) ) ;
#50309 = DIRECTION ( 'NONE',  ( 0.000000000000000000, 0.000000000000000000, -1.000000000000000000 ) ) ;
#50310 = CARTESIAN_POINT ( 'NONE',  ( 22.90120720387987774, -15.61618909956830770, -56.84718059981966576 ) ) ;
#50311 = CARTESIAN_POINT ( 'NONE',  ( -18.33921323110770274, 3.183518156266269994, -50.99327864761959717 ) ) ;
#50313 = CARTESIAN_POINT ( 'NONE',  ( 45.78987214702719655, -39.24112996349171567, -61.59531111407024895 ) ) ;
#50312 = CARTESIAN_POINT ( 'NONE',  ( 64.81199447428090821, 0.8910129994591539093, -60.65352295474699673 ) ) ;
#50314 = CARTESIAN_POINT ( 'NONE',  ( 17.96991432777422304, -7.851816221580103949, -71.08187692902760091 ) ) ;
#50315 = CARTESIAN_POINT ( 'NONE',  ( -31.60239111126589862, -6.246724563331800262, -55.64697389277930029 ) ) ;
#50316 = ORIENTED_EDGE ( 'NONE', *, *, #24867, .T. ) ;
#50317 = CARTESIAN_POINT ( 'NONE',  ( 52.71274985523909606, -49.73402172576329860, -48.58383670079809491 ) ) ;
#50318 = ORIENTED_EDGE ( 'NONE', *, *, #23858, .T. ) ;
#50319 = CARTESIAN_POINT ( 'NONE',  ( 45.91115938045514611, 8.982369621444501462, -56.88730701422755942 ) ) ;
#50320 = CARTESIAN_POINT ( 'NONE',  ( 22.90121965235462653, -15.61618904849089340, -42.45282069170939110 ) ) ;
#50321 = CARTESIAN_POINT ( 'NONE',  ( 13.76823759339399977, 19.89277676745740209, -22.18388608259699879 ) ) ;
#50322 = CARTESIAN_POINT ( 'NONE',  ( 56.12094024660369485, 14.43398220991280034, -25.30520633357740223 ) ) ;
#50323 = CARTESIAN_POINT ( 'NONE',  ( 19.88990749180780071, -9.646662384828470493, -42.13158531401599305 ) ) ;
#50324 = CARTESIAN_POINT ( 'NONE',  ( 28.63710131890649890, -26.55489129076070043, -34.65001001049759566 ) ) ;
#50325 = CARTESIAN_POINT ( 'NONE',  ( 52.98400444558360078, 18.37466557939660206, -48.99793963464180280 ) ) ;
#50326 = CARTESIAN_POINT ( 'NONE',  ( 55.79023370591369968, -45.75302572798440082, -16.82963326627560363 ) ) ;
#50327 = DIRECTION ( 'NONE',  ( -0.3294064756442134922, -0.9441882088882800339, 8.551492847173810438E-14 ) ) ;
#50328 = ORIENTED_EDGE ( 'NONE', *, *, #40875, .F. ) ;
#50329 = CARTESIAN_POINT ( 'NONE',  ( 13.60282763607719936, -8.187849186844388782, -36.68297296116619322 ) ) ;
#50330 = CARTESIAN_POINT ( 'NONE',  ( 62.63393739769619373, 21.88381105532059934, 17.35000000000000142 ) ) ;
#50331 = DIRECTION ( 'NONE',  ( 0.000000000000000000, 1.000000000000000000, 0.000000000000000000 ) ) ;
#50332 = CARTESIAN_POINT ( 'NONE',  ( 72.80537809983910336, 1.383767307422969939, -62.59255479634269648 ) ) ;
#50333 = CARTESIAN_POINT ( 'NONE',  ( 11.89321892218999999, -65.43602743108449715, -18.16392793341869805 ) ) ;
#50334 = CARTESIAN_POINT ( 'NONE',  ( 52.77399506770057513, -49.72485891806022096, -48.90117834109282313 ) ) ;
#50335 = CARTESIAN_POINT ( 'NONE',  ( 22.46789922215001312, -18.61594777151466218, -66.98826990121492031 ) ) ;
#50336 = CARTESIAN_POINT ( 'NONE',  ( 19.30814099325047906, -9.610988906536928056, -62.10768522194346986 ) ) ;
#50337 = CIRCLE ( 'NONE', #13525, 38.49999999999999289 ) ;
#50338 = VECTOR ( 'NONE', #23750, 1000.000000000000000 ) ;
#50339 = CARTESIAN_POINT ( 'NONE',  ( 22.72481324571542061, -13.84495462270172261, -58.36948662338765104 ) ) ;
#50340 = ORIENTED_EDGE ( 'NONE', *, *, #6498, .F. ) ;
#50341 = CARTESIAN_POINT ( 'NONE',  ( 64.82636581786128716, 1.096153228089730147, -70.60852099187108877 ) ) ;
#50342 = EDGE_LOOP ( 'NONE', ( #48655, #18497, #36829, #25983 ) ) ;
#50343 = CARTESIAN_POINT ( 'NONE',  ( 10.77427761093600012, -63.38637133307939564, -45.20767421870360181 ) ) ;
#50344 = ADVANCED_FACE ( 'NONE', ( #43107 ), #46248, .T. ) ;
#50345 = DIRECTION ( 'NONE',  ( 0.1414213562373085320, 0.000000000000000000, 0.9899494936611666907 ) ) ;
#50346 = ORIENTED_EDGE ( 'NONE', *, *, #45381, .T. ) ;
#50347 = DIRECTION ( 'NONE',  ( 1.000000000000000000, 0.000000000000000000, 0.000000000000000000 ) ) ;
#50348 = CARTESIAN_POINT ( 'NONE',  ( 57.26071802442650238, 19.38379676217989811, -53.75790974344070605 ) ) ;
#50349 = CARTESIAN_POINT ( 'NONE',  ( 52.69947341743939973, 19.21175676992940140, -76.74590226668858861 ) ) ;
#50350 = ORIENTED_EDGE ( 'NONE', *, *, #38935, .T. ) ;
#50351 = DIRECTION ( 'NONE',  ( 0.000000000000000000, 0.000000000000000000, 1.000000000000000000 ) ) ;
#50352 = DIRECTION ( 'NONE',  ( 0.000000000000000000, 0.000000000000000000, 1.000000000000000000 ) ) ;
#50353 = DIRECTION ( 'NONE',  ( 0.000000000000000000, 1.000000000000000000, 0.000000000000000000 ) ) ;
#50354 = CARTESIAN_POINT ( 'NONE',  ( 17.98749448546710994, -32.47778390180250341, -34.79644291222910368 ) ) ;
#50355 = CARTESIAN_POINT ( 'NONE',  ( 8.349645199064468670, -12.89819059621470210, -58.89926144005930553 ) ) ;
#50356 = CARTESIAN_POINT ( 'NONE',  ( 18.13393739769639978, 10.38381105532070059, -54.64999999999999858 ) ) ;
#50357 = CARTESIAN_POINT ( 'NONE',  ( 44.70043142015700965, -38.00651179226034060, -66.81746990982490786 ) ) ;
#50358 = ORIENTED_EDGE ( 'NONE', *, *, #35532, .T. ) ;
#50359 = CARTESIAN_POINT ( 'NONE',  ( 57.15880063199809769, -45.85422939174420520, -26.25419981771649702 ) ) ;
#50360 = CARTESIAN_POINT ( 'NONE',  ( 10.24628260800490054, -20.18151641185739820, -59.02271152110689911 ) ) ;
#50361 = CARTESIAN_POINT ( 'NONE',  ( 52.95065152567730138, -49.64318942350850250, -49.05053742289099716 ) ) ;
#50362 = CARTESIAN_POINT ( 'NONE',  ( 9.088130602754668885, -18.12643738272649685, -32.14999999999999858 ) ) ;
#50363 = EDGE_CURVE ( 'NONE', #5918, #51131, #37401, .T. ) ;
#50364 = FACE_OUTER_BOUND ( 'NONE', #9406, .T. ) ;
#50365 = ADVANCED_FACE ( 'NONE', ( #26099 ), #38957, .T. ) ;
#50366 = CARTESIAN_POINT ( 'NONE',  ( 14.32606013829879998, 20.01251569944690090, -74.87640169473949925 ) ) ;
#50367 = CARTESIAN_POINT ( 'NONE',  ( 17.34548134648386863, -52.74445246667860232, -76.12392058103051795 ) ) ;
#50368 = AXIS2_PLACEMENT_3D ( 'NONE', #37613, #13780, #9844 ) ;
#50369 = CARTESIAN_POINT ( 'NONE',  ( 40.99540311694470063, -44.99959555961480362, -5.546226915801610424 ) ) ;
#50370 = AXIS2_PLACEMENT_3D ( 'NONE', #19701, #4484, #31473 ) ;
#50371 = CARTESIAN_POINT ( 'NONE',  ( 8.222939282903173108, -14.98363466968944024, -60.53312594118477108 ) ) ;
#50372 = TOROIDAL_SURFACE ( 'NONE', #38675, 5.500000000000000000, 0.5000000000000000000 ) ;
#50373 = CARTESIAN_POINT ( 'NONE',  ( 8.620230944888110258, -19.01132311728650137, -66.37257821948348635 ) ) ;
#50374 = EDGE_LOOP ( 'NONE', ( #50622, #48385 ) ) ;
#50375 = CARTESIAN_POINT ( 'NONE',  ( 53.10609841537830533, -49.27737300328959691, -26.94345523169370082 ) ) ;
#50376 = CARTESIAN_POINT ( 'NONE',  ( 56.72469771552999873, -50.67197071006459907, -74.53479304648951143 ) ) ;
#50378 = CARTESIAN_POINT ( 'NONE',  ( 41.16162958179530307, -39.66950744282151931, -80.37574497360704129 ) ) ;
#50377 = CARTESIAN_POINT ( 'NONE',  ( 3.241158669444910156, 25.60760945040669867, -10.70730181694110072 ) ) ;
#50379 = DIRECTION ( 'NONE',  ( 0.000000000000000000, -3.399867999999999948E-10, 1.000000000000000000 ) ) ;
#50380 = CARTESIAN_POINT ( 'NONE',  ( 48.43113447640888580, 22.58636222950222816, -53.38348114488076845 ) ) ;
#50381 = EDGE_LOOP ( 'NONE', ( #43898, #31589, #36988, #41438 ) ) ;
#50382 = CARTESIAN_POINT ( 'NONE',  ( 16.13393739769620083, -15.61618894467929941, -28.45282021618999835 ) ) ;
#50383 = CARTESIAN_POINT ( 'NONE',  ( 47.49124202022650110, 23.36933501918910494, -54.82949043996080007 ) ) ;
#50384 = CARTESIAN_POINT ( 'NONE',  ( 9.019466863379530963, -12.08793898035315451, -64.93882274181090963 ) ) ;
#50385 = CARTESIAN_POINT ( 'NONE',  ( 11.63393739769619906, -41.61618894467930119, -54.64999999999999858 ) ) ;
#50386 = CARTESIAN_POINT ( 'NONE',  ( 56.70490786469932942, 14.04930731085842233, -25.29390771195738807 ) ) ;
#50387 = CARTESIAN_POINT ( 'NONE',  ( 11.37461205174560064, 33.83526575001669556, -16.88571183838750045 ) ) ;
#50388 = CARTESIAN_POINT ( 'NONE',  ( 51.70989473322139673, 17.69254021111469655, -77.02394377317959595 ) ) ;
#50389 = CARTESIAN_POINT ( 'NONE',  ( 53.36907892687840160, 18.14597633810089761, -48.78904877098699444 ) ) ;
#50390 = FACE_OUTER_BOUND ( 'NONE', #21512, .T. ) ;
#50391 = CARTESIAN_POINT ( 'NONE',  ( 8.731180243531472485, 17.69319178430564321, -34.79644561402098191 ) ) ;
#50392 = CARTESIAN_POINT ( 'NONE',  ( 52.77196772020159443, 18.44163949243500156, -27.80225394247760207 ) ) ;
#50393 = CARTESIAN_POINT ( 'NONE',  ( 50.34648245260830635, 22.03267857139280039, -54.24922544986609552 ) ) ;
#50394 = CARTESIAN_POINT ( 'NONE',  ( 63.59194260610701122, 1.176185264361309990, -69.52318026956261576 ) ) ;
#50395 = CARTESIAN_POINT ( 'NONE',  ( 52.62851231361270266, 18.57686390552120059, -48.67161502741990375 ) ) ;
#50396 = CARTESIAN_POINT ( 'NONE',  ( 58.33770897141780409, -45.11618894467940066, -10.68148127205489928 ) ) ;
#50397 = CARTESIAN_POINT ( 'NONE',  ( 71.10413293483961183, 1.338092079250050137, -60.76305085381149951 ) ) ;
#50398 = CARTESIAN_POINT ( 'NONE',  ( 10.97829214564769984, 31.96174209507660180, -44.74190632825920488 ) ) ;
#50399 = CARTESIAN_POINT ( 'NONE',  ( 72.94555459751978788, 0.9254890127240680275, -62.06507410682309711 ) ) ;
#50400 = CYLINDRICAL_SURFACE ( 'NONE', #16766, 1.999999999999997113 ) ;
#50401 = CARTESIAN_POINT ( 'NONE',  ( 18.50685669558849966, 20.06273926763419979, -74.14993629405250886 ) ) ;
#50402 = ORIENTED_EDGE ( 'NONE', *, *, #36828, .T. ) ;
#50403 = ORIENTED_EDGE ( 'NONE', *, *, #13135, .F. ) ;
#50404 = DIRECTION ( 'NONE',  ( 3.251616519950084978E-22, -1.000000000000000000, 1.784227544494129940E-11 ) ) ;
#50405 = EDGE_CURVE ( 'NONE', #814, #51345, #42508, .T. ) ;
#50406 = CARTESIAN_POINT ( 'NONE',  ( 50.31290364262088843, -0.9070165658829743016, -16.15042132747201364 ) ) ;
#50407 = ORIENTED_EDGE ( 'NONE', *, *, #44911, .T. ) ;
#50408 = CARTESIAN_POINT ( 'NONE',  ( 12.58828388404580068, -65.45077111865299457, -46.93561936501430409 ) ) ;
#50409 = CARTESIAN_POINT ( 'NONE',  ( 56.19278121266829373, -45.59700403742969144, -25.37063597392850056 ) ) ;
#50410 = CARTESIAN_POINT ( 'NONE',  ( 53.63393739769619373, 21.88381105532059934, 17.35000000000000142 ) ) ;
#50411 = CIRCLE ( 'NONE', #11095, 9.999999999999998224 ) ;
#50412 = B_SPLINE_CURVE_WITH_KNOTS ( 'NONE', 3,
 ( #8341, #4406, #4661, #994, #24552, #20633, #41089, #36621, #44761, #24817, #46063, #49733, #18006, #49484, #26365, #22437 ),
 .UNSPECIFIED., .F., .F.,
 ( 4, 2, 2, 2, 2, 2, 2, 4 ),
 ( 0.000000000000000000, 0.1750000000000000444, 0.3750000000000012768, 0.5000000000000000000, 0.5625000000000006661, 0.6600291104134125009, 0.8160756870748754332, 1.000000000000000000 ),
 .UNSPECIFIED. ) ;
#50413 = CARTESIAN_POINT ( 'NONE',  ( 13.51895031977020523, -51.88237913636656629, -74.91995119715397777 ) ) ;
#50414 = VERTEX_POINT ( 'NONE', #17992 ) ;
#50415 = AXIS2_PLACEMENT_3D ( 'NONE', #35711, #31493, #39137 ) ;
#50416 = CARTESIAN_POINT ( 'NONE',  ( 16.13393739769620083, -15.61618894467929941, -32.14999999999999858 ) ) ;
#50417 = CARTESIAN_POINT ( 'NONE',  ( 45.11614098616555424, 6.824003222330928153, -64.73897788473527726 ) ) ;
#50418 = CARTESIAN_POINT ( 'NONE',  ( 19.97369125467840334, -22.99931529436689814, -35.14999999999999858 ) ) ;
#50419 = VERTEX_POINT ( 'NONE', #6209 ) ;
#50420 = CARTESIAN_POINT ( 'NONE',  ( 10.16807496446329928, -9.924861728319630316, -37.03483646650040129 ) ) ;
#50421 = CARTESIAN_POINT ( 'NONE',  ( 14.59756433006669951, 19.88381105111769642, -22.39374700643550042 ) ) ;
#50422 = CARTESIAN_POINT ( 'NONE',  ( 9.366922816393266515, -16.24874389531281693, -51.42305503118727472 ) ) ;
#50423 = DIRECTION ( 'NONE',  ( 0.6339889056055382222, 0.000000000000000000, -0.7733421413379021336 ) ) ;
#50424 = CARTESIAN_POINT ( 'NONE',  ( 73.16133767175020353, 0.8879664753683469414, -68.92499589875210120 ) ) ;
#50425 = CARTESIAN_POINT ( 'NONE',  ( 47.31501038023650096, -54.57921746145999720, -74.80639350504939955 ) ) ;
#50426 = CARTESIAN_POINT ( 'NONE',  ( 41.58069270221000124, 12.33221690508110058, -4.585379893427648845 ) ) ;
#50427 = EDGE_CURVE ( 'NONE', #23870, #8412, #6386, .T. ) ;
#50428 = CARTESIAN_POINT ( 'NONE',  ( 53.17432493994039788, 20.66509266784749954, -53.32388713517680401 ) ) ;
#50429 = B_SPLINE_SURFACE_WITH_KNOTS ( 'NONE', 3, 3, ( 
 ( #35126, #15486, #15230, #31181, #47212, #27261, #41069, #49205, #33186, #17478, #37138, #13297, #1235, #45263, #29002, #28739 ),
 ( #45521, #33445, #29517, #40547, #9371, #49464, #5179, #25317, #37646, #13553, #41320, #25571, #9617, #24531, #21134, #36601 ),
 ( #16697, #12781, #5434, #20878, #44739, #20610, #21388, #37393, #41577, #1495, #5689, #21639, #36872, #17225, #12514, #16439 ),
 ( #4636, #24794, #705, #971, #32392, #48412, #8842, #28480, #32651, #48678, #16972, #44477, #40801, #8586, #4903, #32918 ),
 ( #29258, #48948, #13049, #45000, #9100, #25051, #29761, #30539, #45780, #26609, #10392, #22932, #13805, #30019, #50484, #42883 ),
 ( #14834, #42360, #34206, #46564, #41840, #46046, #14316, #30796, #26348, #21900, #42099, #10913, #18503, #17987, #6463, #2786 ),
 ( #18757, #10652, #34731, #22420, #2005, #50734, #37912, #38695, #26875, #10134, #6204, #42622, #22158, #6978, #6721, #46824 ),
 ( #9869, #38423, #38170, #26091, #33951, #2265, #18239, #1746, #50228, #34475, #49969, #33700, #14060, #22677, #30286, #2526 ),
 ( #17730, #49717, #46304, #25824, #5942, #14574, #27900, #27393, #39201, #43905, #12193, #15094, #47588, #4065, #43394, #3819 ),
 ( #31568, #19792, #7489, #7237, #3043, #16113, #36030, #138, #51514, #38952, #51765, #39974, #47336, #35262, #48094, #8254 ) ),
 .UNSPECIFIED., .F., .F., .F.,
 ( 4, 1, 1, 1, 1, 1, 1, 4 ),
 ( 4, 2, 2, 2, 2, 2, 2, 4 ),
 ( 0.000000000000000000, 0.1428571428571430157, 0.2857142857142860315, 0.4285714285714289917, 0.5714285714285709528, 0.7142857142857139685, 0.8571428571428569843, 1.000000000000000000 ),
 ( -3.863343447353519977, -3.187258344066659976, -2.414589654595949764, -1.931671723676759989, -1.690212758217169986, -1.313423695611309894, -0.7105611954419280840, 0.000000000000000000 ),
 .UNSPECIFIED. ) ;
#50430 = CARTESIAN_POINT ( 'NONE',  ( 53.19108282174769897, 19.98230769539780027, -75.83523926356809852 ) ) ;
#50431 = FACE_OUTER_BOUND ( 'NONE', #14599, .T. ) ;
#50432 = CARTESIAN_POINT ( 'NONE',  ( 7.903303049004190228, -15.12692539678219994, -34.52656793190860185 ) ) ;
#50433 = VERTEX_POINT ( 'NONE', #18244 ) ;
#50434 = CARTESIAN_POINT ( 'NONE',  ( 15.21636614235080032, 19.37178131641699963, -15.64999999240779971 ) ) ;
#50435 = CARTESIAN_POINT ( 'NONE',  ( 1.828123248987350014, -55.63609750716739910, -10.79459774355089863 ) ) ;
#50436 = CARTESIAN_POINT ( 'NONE',  ( 75.41210043417740394, 0.5916036937065950463, -12.07275756619249840 ) ) ;
#50437 = DIRECTION ( 'NONE',  ( 0.2260571801428161165, -2.775557561562891043E-17, -0.9741140340359943917 ) ) ;
#50438 = CARTESIAN_POINT ( 'NONE',  ( 19.75452741144124502, -55.45190691955212969, -75.31104072282781203 ) ) ;
#50439 = CARTESIAN_POINT ( 'NONE',  ( 12.84043731220637596, -55.48023558917851261, -75.66007724753696095 ) ) ;
#50440 = TOROIDAL_SURFACE ( 'NONE', #24438, 5.500000000000000000, 0.5000000000000000000 ) ;
#50441 = CARTESIAN_POINT ( 'NONE',  ( 7.571123728786862905, 29.74412437438943613, -20.43741446242724180 ) ) ;
#50442 = CARTESIAN_POINT ( 'NONE',  ( 63.02029346573409185, 0.8838110553206759423, -62.51131646858519275 ) ) ;
#50443 = CARTESIAN_POINT ( 'NONE',  ( 13.64046745046540110, 19.01922438765150147, -20.99582705430550078 ) ) ;
#50444 = PLANE ( 'NONE',  #8096 ) ;
#50445 = CARTESIAN_POINT ( 'NONE',  ( 40.95606765393399940, 13.15690657785849993, -3.881683722126650249 ) ) ;
#50446 = DIRECTION ( 'NONE',  ( 0.000000000000000000, 1.000000000000000000, 0.000000000000000000 ) ) ;
#50447 = CARTESIAN_POINT ( 'NONE',  ( 64.93393739769578588, 0.9098571636355720083, -61.17674615073129729 ) ) ;
#50448 = CARTESIAN_POINT ( 'NONE',  ( 68.13393739769745139, -49.21324915460503036, -70.54648330188275906 ) ) ;
#50449 = CARTESIAN_POINT ( 'NONE',  ( 75.92401563033300249, -43.33178766826745232, -13.58799118537118567 ) ) ;
#50450 = CARTESIAN_POINT ( 'NONE',  ( 18.15925977880919717, -52.01891576978010079, -75.67066142420200947 ) ) ;
#50451 = CARTESIAN_POINT ( 'NONE',  ( 53.10211901724390060, -45.11618894467940066, -9.306651317679861535 ) ) ;
#50452 = ORIENTED_EDGE ( 'NONE', *, *, #7745, .T. ) ;
#50453 = CARTESIAN_POINT ( 'NONE',  ( 20.33583072231489908, -21.76848825687689981, -57.37660785931080198 ) ) ;
#50454 = CARTESIAN_POINT ( 'NONE',  ( 63.87812827450808584, 1.200157260841299811, -61.45760966837089967 ) ) ;
#50455 = EDGE_LOOP ( 'NONE', ( #22125, #39823, #20834, #33940 ) ) ;
#50456 = DIRECTION ( 'NONE',  ( -0.4640893551880381218, 0.8857883891772070362, 0.000000000000000000 ) ) ;
#50457 = CARTESIAN_POINT ( 'NONE',  ( 44.13393739769620083, -36.11618894467930119, -44.64999999999999858 ) ) ;
#50458 = CARTESIAN_POINT ( 'NONE',  ( 74.93037295002240228, -43.11618894467930119, -15.31098073120859837 ) ) ;
#50459 = CARTESIAN_POINT ( 'NONE',  ( 45.65335366086122093, 8.840693443015325670, -58.64289655873446350 ) ) ;
#50460 = CARTESIAN_POINT ( 'NONE',  ( 9.151707502888131174, -16.64276093509979759, -81.23899999999999011 ) ) ;
#50461 = CARTESIAN_POINT ( 'NONE',  ( 63.63393739769619373, 21.88381105532059934, 11.84999999999999964 ) ) ;
#50462 = VERTEX_POINT ( 'NONE', #38702 ) ;
#50463 = ORIENTED_EDGE ( 'NONE', *, *, #20544, .T. ) ;
#50464 = EDGE_CURVE ( 'NONE', #51808, #16602, #42192, .T. ) ;
#50465 = ORIENTED_EDGE ( 'NONE', *, *, #10177, .F. ) ;
#50466 = DIRECTION ( 'NONE',  ( 0.000000000000000000, 0.000000000000000000, -1.000000000000000000 ) ) ;
#50467 = CARTESIAN_POINT ( 'NONE',  ( 61.29004561485690061, -45.22833724571190572, -46.51650915558359856 ) ) ;
#50468 =( BOUNDED_CURVE ( )  B_SPLINE_CURVE ( 3, ( #34338, #38036, #14439, #6326 ),
 .UNSPECIFIED., .F., .T. ) 
 B_SPLINE_CURVE_WITH_KNOTS ( ( 4, 4 ),
 ( 5.070260775219134430, 5.428132570053640471 ),
 .UNSPECIFIED. ) 
 CURVE ( )  GEOMETRIC_REPRESENTATION_ITEM ( )  RATIONAL_B_SPLINE_CURVE ( ( 1.000000000000000000, 0.9893557610490320009, 0.9893557610490320009, 1.000000000000000000 ) ) 
 REPRESENTATION_ITEM ( '' )  );
#50469 = DIRECTION ( 'NONE',  ( 1.000000000000000000, 0.000000000000000000, 0.000000000000000000 ) ) ;
#50470 = EDGE_CURVE ( 'NONE', #17717, #31931, #42630, .T. ) ;
#50471 = EDGE_LOOP ( 'NONE', ( #20912, #43829, #19814, #23540, #24339 ) ) ;
#50472 = EDGE_CURVE ( 'NONE', #38446, #13016, #46051, .T. ) ;
#50473 = ORIENTED_EDGE ( 'NONE', *, *, #28960, .F. ) ;
#50474 = CARTESIAN_POINT ( 'NONE',  ( 22.55531542943956680, -17.79663745630361049, -72.55697149734855600 ) ) ;
#50475 = LINE ( 'NONE', #25306, #37664 ) ;
#50476 = AXIS2_PLACEMENT_3D ( 'NONE', #2683, #27034, #30951 ) ;
#50477 = ORIENTED_EDGE ( 'NONE', *, *, #2977, .T. ) ;
#50478 = CARTESIAN_POINT ( 'NONE',  ( 15.70135240704478186, -23.59237159327061306, -50.02457256032881361 ) ) ;
#50480 = CARTESIAN_POINT ( 'NONE',  ( 52.61550136881809436, -51.35813298341240341, -75.86880934735940230 ) ) ;
#50479 = AXIS2_PLACEMENT_3D ( 'NONE', #9096, #16967, #25565 ) ;
#50481 = CARTESIAN_POINT ( 'NONE',  ( 60.23889825737590087, 14.54821815915980032, -47.30579064662340016 ) ) ;
#50482 = FACE_BOUND ( 'NONE', #10674, .T. ) ;
#50483 = EDGE_CURVE ( 'NONE', #9344, #12214, #10398, .T. ) ;
#50484 = CARTESIAN_POINT ( 'NONE',  ( 41.02582416393729403, -44.60212236685470089, -4.878402777628929599 ) ) ;
#50485 = CARTESIAN_POINT ( 'NONE',  ( 23.04647744410513255, -19.60028888980541240, -79.67433673434211983 ) ) ;
#50486 = CARTESIAN_POINT ( 'NONE',  ( 65.04225540962447383, 1.022507349525342502, -17.84440820854044674 ) ) ;
#50487 = CARTESIAN_POINT ( 'NONE',  ( 64.64302830678678902, 0.9098571636355680115, -70.52991329011140920 ) ) ;
#50488 = CARTESIAN_POINT ( 'NONE',  ( 82.13853704237929776, 13.88381105532070059, -46.37203261889099792 ) ) ;
#50489 = DIRECTION ( 'NONE',  ( 1.000000000000000000, 0.000000000000000000, 0.000000000000000000 ) ) ;
#50490 = CARTESIAN_POINT ( 'NONE',  ( 11.09952124908870097, -9.596105703907399587, -48.56581262070909588 ) ) ;
#50491 = ORIENTED_EDGE ( 'NONE', *, *, #36012, .T. ) ;
#50492 = CARTESIAN_POINT ( 'NONE',  ( 14.72298240475299913, -52.26337343415740122, -75.96669286083250938 ) ) ;
#50493 = CARTESIAN_POINT ( 'NONE',  ( 57.48794426520840517, 19.15268824649449897, -52.98983914114159433 ) ) ;
#50494 = CARTESIAN_POINT ( 'NONE',  ( 71.42967573711919727, 1.404650034021559968, -70.20402782815220633 ) ) ;
#50495 = CARTESIAN_POINT ( 'NONE',  ( 45.41861909476764225, -40.05849041370392172, -59.78164571485964984 ) ) ;
#50496 = DIRECTION ( 'NONE',  ( -0.7071067811865475727, 0.000000000000000000, -0.7071067811865475727 ) ) ;
#50498 = ADVANCED_FACE ( 'NONE', ( #26615 ), #38430, .T. ) ;
#50497 = DIRECTION ( 'NONE',  ( -0.3502816565540492477, 0.000000000000000000, 0.9366444154970182678 ) ) ;
#50499 = CARTESIAN_POINT ( 'NONE',  ( 63.25085271618998917, 1.186614556332910020, -68.98303591127670131 ) ) ;
#50500 = CARTESIAN_POINT ( 'NONE',  ( 47.98474431824940467, -54.38356013217800466, -55.12640935544759913 ) ) ;
#50501 = CARTESIAN_POINT ( 'NONE',  ( 22.57793705737757506, -13.54241025272627219, -80.74806968844832511 ) ) ;
#50502 = CIRCLE ( 'NONE', #1238, 2.000000000000001332 ) ;
#50503 = CARTESIAN_POINT ( 'NONE',  ( 56.48750710943370024, 19.52146772179129997, -53.61740591960349889 ) ) ;
#50504 = CARTESIAN_POINT ( 'NONE',  ( 47.84723601610939880, 23.19681007510559922, -54.96539816047189930 ) ) ;
#50505 = ORIENTED_EDGE ( 'NONE', *, *, #6862, .T. ) ;
#50506 = AXIS2_PLACEMENT_3D ( 'NONE', #30311, #6750, #25849 ) ;
#50507 = CARTESIAN_POINT ( 'NONE',  ( 9.532113884515599267, -18.09781854541880364, -71.73272827236579019 ) ) ;
#50508 = CIRCLE ( 'NONE', #48010, 3.400000000022780799 ) ;
#50509 = ORIENTED_EDGE ( 'NONE', *, *, #43555, .F. ) ;
#50510 = CARTESIAN_POINT ( 'NONE',  ( 71.31531788893299506, 1.266538207494809942, -70.53881316596870477 ) ) ;
#50511 = FACE_OUTER_BOUND ( 'NONE', #49182, .T. ) ;
#50512 = DIRECTION ( 'NONE',  ( 0.000000000000000000, 0.000000000000000000, -1.000000000000000000 ) ) ;
#50514 = CARTESIAN_POINT ( 'NONE',  ( 52.58854596461549846, 18.60460160505449778, -27.97794855353080123 ) ) ;
#50513 = DIRECTION ( 'NONE',  ( 0.3281607301299682700, -0.6263469766835021435, 0.7071067811865493491 ) ) ;
#50515 = CARTESIAN_POINT ( 'NONE',  ( 9.830109632710200884, -18.77914866715480358, -77.30479070626310545 ) ) ;
#50516 = DIRECTION ( 'NONE',  ( 0.000000000000000000, 0.000000000000000000, -1.000000000000000000 ) ) ;
#50517 = CARTESIAN_POINT ( 'NONE',  ( 0.5522155295079038684, -22.42457893558620796, -34.84133294386909796 ) ) ;
#50518 = CARTESIAN_POINT ( 'NONE',  ( 19.54188305415121008, -21.52912787978993947, -40.78610065424740583 ) ) ;
#50519 = ORIENTED_EDGE ( 'NONE', *, *, #8981, .T. ) ;
#50520 = CARTESIAN_POINT ( 'NONE',  ( 63.19893373200899589, -0.5161889446793590519, -62.06450996101597184 ) ) ;
#50521 = EDGE_LOOP ( 'NONE', ( #10250, #28711, #5748, #20076 ) ) ;
#50522 = VERTEX_POINT ( 'NONE', #14579 ) ;
#50523 = CARTESIAN_POINT ( 'NONE',  ( 12.16812838079169978, -64.68014690341630057, -15.91929859869470043 ) ) ;
#50524 = CARTESIAN_POINT ( 'NONE',  ( 57.50723796702219914, -46.11618894467930119, -25.33268370472680076 ) ) ;
#50525 = CARTESIAN_POINT ( 'NONE',  ( 11.83825639585159983, 33.81473130949329686, -45.42565952194429713 ) ) ;
#50526 = CARTESIAN_POINT ( 'NONE',  ( 9.511520510868781031, -63.71643849929780856, -46.52942082108589261 ) ) ;
#50527 = ORIENTED_EDGE ( 'NONE', *, *, #29192, .T. ) ;
#50528 = ORIENTED_EDGE ( 'NONE', *, *, #34515, .F. ) ;
#50529 = EDGE_CURVE ( 'NONE', #38543, #5918, #30545, .T. ) ;
#50530 = CARTESIAN_POINT ( 'NONE',  ( 54.91646384901320488, 20.20362395552419699, -54.04939823774940066 ) ) ;
#50531 = CARTESIAN_POINT ( 'NONE',  ( 56.57310015978940498, 14.96172080682539907, -26.26426129276709887 ) ) ;
#50532 = CARTESIAN_POINT ( 'NONE',  ( 53.11770077000060297, -49.55992874389239233, -49.09731761359610402 ) ) ;
#50533 = CARTESIAN_POINT ( 'NONE',  ( 48.79723671898879900, 22.41103229812440034, -53.89287427470050318 ) ) ;
#50534 = DIRECTION ( 'NONE',  ( -1.000000000000000000, 0.000000000000000000, 0.000000000000000000 ) ) ;
#50535 = CARTESIAN_POINT ( 'NONE',  ( 50.72974178121339150, -49.49305235525400093, -76.22250671080470852 ) ) ;
#50536 = CARTESIAN_POINT ( 'NONE',  ( 56.98397757690029408, -50.69327631065389994, -53.23409530833590253 ) ) ;
#50537 = ORIENTED_EDGE ( 'NONE', *, *, #8461, .T. ) ;
#50538 = DIRECTION ( 'NONE',  ( 0.000000000000000000, 1.000000000000000000, 0.000000000000000000 ) ) ;
#50539 = CARTESIAN_POINT ( 'NONE',  ( 69.22748654599826068, 19.47158195952208004, -70.40645085170191919 ) ) ;
#50540 = ORIENTED_EDGE ( 'NONE', *, *, #30360, .T. ) ;
#50541 = DIRECTION ( 'NONE',  ( 0.000000000000000000, 0.000000000000000000, -1.000000000000000000 ) ) ;
#50542 = CARTESIAN_POINT ( 'NONE',  ( 49.92842301023320317, -45.11618894467940066, -10.23644921203369940 ) ) ;
#50543 = CARTESIAN_POINT ( 'NONE',  ( 10.60612691485259873, -21.18665201854900104, -46.76127109678569838 ) ) ;
#50544 = CARTESIAN_POINT ( 'NONE',  ( 13.76822423289859998, -51.12516065014939670, -22.18389327967700098 ) ) ;
#50545 = CARTESIAN_POINT ( 'NONE',  ( 55.34187454801539729, 19.38381105532069881, -76.48031925771689998 ) ) ;
#50546 = CARTESIAN_POINT ( 'NONE',  ( 47.57128498443769615, -54.56535262155699684, -74.19815949659729881 ) ) ;
#50547 = CARTESIAN_POINT ( 'NONE',  ( 55.17360652619739625, 13.97791545909459998, -14.82785752668969792 ) ) ;
#50548 = CARTESIAN_POINT ( 'NONE',  ( 47.69785024206510116, 23.27647591315859898, -55.07623521634459962 ) ) ;
#50549 = CIRCLE ( 'NONE', #7867, 5.500000000000000000 ) ;
#50550 = CARTESIAN_POINT ( 'NONE',  ( 56.50450790981899729, -50.73896967485040221, -53.50133212754479928 ) ) ;
#50551 = CARTESIAN_POINT ( 'NONE',  ( 20.16990914961739989, -9.832289637797728687, -46.54110819413470068 ) ) ;
#50552 = CARTESIAN_POINT ( 'NONE',  ( 45.63393739769620083, 19.38381105532069881, 11.34999999999999964 ) ) ;
#50553 = VERTEX_POINT ( 'NONE', #46570 ) ;
#50554 = CARTESIAN_POINT ( 'NONE',  ( 47.62448412835980349, 23.28090870184360028, -74.50417146787160050 ) ) ;
#50555 = CARTESIAN_POINT ( 'NONE',  ( 64.95585434546930514, 1.326578174762039986, -60.85378544217730479 ) ) ;
#50556 = CARTESIAN_POINT ( 'NONE',  ( 43.63773095450489592, -46.04023181038529344, -8.037430359857850704 ) ) ;
#50557 = CARTESIAN_POINT ( 'NONE',  ( 22.46012548327199454, -10.75454236778581318, -57.58399795081778194 ) ) ;
#50558 = CARTESIAN_POINT ( 'NONE',  ( 57.55751162049570269, -48.61618894467930119, -53.92796738110899923 ) ) ;
#50559 = EDGE_CURVE ( 'NONE', #4500, #44239, #7534, .T. ) ;
#50560 = CARTESIAN_POINT ( 'NONE',  ( 4.133937397696199945, -15.61618894467930652, -22.14999999999999858 ) ) ;
#50562 = EDGE_CURVE ( 'NONE', #51441, #39898, #33628, .T. ) ;
#50561 = CARTESIAN_POINT ( 'NONE',  ( 82.13853704237929776, 13.98942268381949994, -47.02038781679129897 ) ) ;
#50563 = VECTOR ( 'NONE', #16632, 1000.000000000000000 ) ;
#50564 = CARTESIAN_POINT ( 'NONE',  ( -18.25696898823050063, 2.971788218260359660, -50.64156704142759935 ) ) ;
#50566 = CARTESIAN_POINT ( 'NONE',  ( 47.11822937922350718, -38.11590075025419111, -54.71074210669950588 ) ) ;
#50565 = CARTESIAN_POINT ( 'NONE',  ( 16.13393739954389972, -15.61618894518879941, 4.350000000321379900 ) ) ;
#50567 = CARTESIAN_POINT ( 'NONE',  ( 10.14686910709649936, -10.32892520170320338, -70.73769537184530520 ) ) ;
#50568 = CARTESIAN_POINT ( 'NONE',  ( -33.86606230032689524, -20.49714794425430142, -57.75543702565100546 ) ) ;
#50569 = EDGE_CURVE ( 'NONE', #32442, #35847, #35124, .T. ) ;
#50570 = VERTEX_POINT ( 'NONE', #29691 ) ;
#50571 = CARTESIAN_POINT ( 'NONE',  ( 52.86125339900270603, -49.65852478324119801, -48.87400161482390359 ) ) ;
#50572 = ORIENTED_EDGE ( 'NONE', *, *, #36261, .T. ) ;
#50573 = CARTESIAN_POINT ( 'NONE',  ( 17.64670642448523097, 20.66383147154662581, -75.74021525116319253 ) ) ;
#50574 = CARTESIAN_POINT ( 'NONE',  ( 22.04686314924591883, -12.20822412868739981, -42.28615306984772815 ) ) ;
#50575 = CARTESIAN_POINT ( 'NONE',  ( 13.64848238802169966, 20.16422653727189740, -23.00152640757379885 ) ) ;
#50576 = FACE_OUTER_BOUND ( 'NONE', #1726, .T. ) ;
#50577 = CARTESIAN_POINT ( 'NONE',  ( 22.82000994230530111, -13.37141888410519996, -44.34971538379739542 ) ) ;
#50578 = CARTESIAN_POINT ( 'NONE',  ( 64.81566772303590085, 1.395841836299290151, -61.06813208783949420 ) ) ;
#50579 = CARTESIAN_POINT ( 'NONE',  ( 53.56302256524990213, 18.15423094141489813, -49.17075139047800292 ) ) ;
#50580 = CARTESIAN_POINT ( 'NONE',  ( 55.52984664395540193, -45.92959713896109264, -16.63879282810290050 ) ) ;
#50581 = CARTESIAN_POINT ( 'NONE',  ( 68.13393739769618662, -30.66618894467940137, -90.65000000000000568 ) ) ;
#50582 = ORIENTED_EDGE ( 'NONE', *, *, #33421, .T. ) ;
#50583 = TOROIDAL_SURFACE ( 'NONE', #8716, 16.49999999812870044, 0.4999999999096970127 ) ;
#50584 = CARTESIAN_POINT ( 'NONE',  ( 8.300043692618718438, -15.15050933049450066, -34.30640502925760416 ) ) ;
#50585 = CARTESIAN_POINT ( 'NONE',  ( 11.93488811383480019, -65.43955691952199061, -17.90291648171000105 ) ) ;
#50586 = CARTESIAN_POINT ( 'NONE',  ( 9.742037140472790568, 33.13719944107199922, -46.80840188538130064 ) ) ;
#50587 = CARTESIAN_POINT ( 'NONE',  ( 73.12399047084761605, 1.191644800533229853, -62.50206874317210293 ) ) ;
#50588 = CARTESIAN_POINT ( 'NONE',  ( 10.66246720348149957, -64.86660773051299600, -18.01843150775420099 ) ) ;
#50589 = CARTESIAN_POINT ( 'NONE',  ( 64.93393739769619799, 1.883811055320669947, -69.84999999999999432 ) ) ;
#50590 = CARTESIAN_POINT ( 'NONE',  ( 24.01934093808031179, -16.26519669879829166, -75.81845923383386321 ) ) ;
#50591 = CARTESIAN_POINT ( 'NONE',  ( 13.18974571921978978, -9.507163701089766050, -61.80991948917802148 ) ) ;
#50592 = DIRECTION ( 'NONE',  ( 1.000000000000000000, 0.000000000000000000, 0.000000000000000000 ) ) ;
#50593 = ORIENTED_EDGE ( 'NONE', *, *, #44228, .T. ) ;
#50594 = ADVANCED_FACE ( 'NONE', ( #5865 ), #29948, .T. ) ;
#50595 = CARTESIAN_POINT ( 'NONE',  ( 0.3209249304026170480, -15.61618894467929941, -35.14999999999999858 ) ) ;
#50596 = ORIENTED_EDGE ( 'NONE', *, *, #22003, .T. ) ;
#50597 = CARTESIAN_POINT ( 'NONE',  ( 9.729212633477690275, -63.13885989062299586, -46.30111529514049806 ) ) ;
#50598 = DIRECTION ( 'NONE',  ( 0.000000000000000000, -1.000000000000000000, 0.000000000000000000 ) ) ;
#50599 = ORIENTED_EDGE ( 'NONE', *, *, #6924, .F. ) ;
#50600 = CARTESIAN_POINT ( 'NONE',  ( 0.2609591194317593676, -8.253214024663448001, -34.64999999999999858 ) ) ;
#50601 = CARTESIAN_POINT ( 'NONE',  ( 56.87125374609500028, 19.41964089708080010, -53.85479923334150243 ) ) ;
#50602 = CARTESIAN_POINT ( 'NONE',  ( 54.14345801728809704, 19.38380527828979893, -76.93443301949999125 ) ) ;
#50603 = ORIENTED_EDGE ( 'NONE', *, *, #389, .T. ) ;
#50604 = CARTESIAN_POINT ( 'NONE',  ( 44.11147024075970080, 1.884029797248020000, -54.64999999999999858 ) ) ;
#50605 = CARTESIAN_POINT ( 'NONE',  ( 16.13393739769620083, -15.61618894467929941, 1.600000000000000089 ) ) ;
#50606 = CARTESIAN_POINT ( 'NONE',  ( 15.09835210727568011, -7.705193513269825267, -69.25066627866567615 ) ) ;
#50607 = CARTESIAN_POINT ( 'NONE',  ( 24.36192440164969852, -15.08425857451129914, -67.77178171918468763 ) ) ;
#50608 = CIRCLE ( 'NONE', #33827, 2.999999999999960920 ) ;
#50609 = CARTESIAN_POINT ( 'NONE',  ( 22.90088705258820667, -15.61618575905976414, -62.45282818884277276 ) ) ;
#50610 = CARTESIAN_POINT ( 'NONE',  ( 44.71029624102973798, -38.00771234126634113, -66.76814554949260128 ) ) ;
#50611 = ORIENTED_EDGE ( 'NONE', *, *, #8021, .F. ) ;
#50612 = FACE_OUTER_BOUND ( 'NONE', #7156, .T. ) ;
#50613 = CARTESIAN_POINT ( 'NONE',  ( 23.58405125408460279, -15.56621563185109913, -58.23052221047069565 ) ) ;
#50614 = CARTESIAN_POINT ( 'NONE',  ( 10.18216224808260151, -11.95184640257830111, -32.14999999999999858 ) ) ;
#50615 = LINE ( 'NONE', #3183, #28307 ) ;
#50616 = MECHANICAL_DESIGN_GEOMETRIC_PRESENTATION_REPRESENTATION (  '', ( #7936 ), #36377 ) ;
#50617 = CARTESIAN_POINT ( 'NONE',  ( 26.52624224310950041, -21.61618894467929763, -22.14999999999999858 ) ) ;
#50618 = CARTESIAN_POINT ( 'NONE',  ( 52.68908936341578908, -49.75029824513269716, -48.47378032971909789 ) ) ;
#50619 = CARTESIAN_POINT ( 'NONE',  ( 45.38207380022019777, -45.37872504213810032, -8.365231906245979232 ) ) ;
#50620 = CARTESIAN_POINT ( 'NONE',  ( 8.674532686402148585, -12.88142895660771359, -60.61962948924526273 ) ) ;
#50621 = CARTESIAN_POINT ( 'NONE',  ( 13.90615343176800067, -23.55468372077690020, -62.09475594204819515 ) ) ;
#50622 = ORIENTED_EDGE ( 'NONE', *, *, #27475, .F. ) ;
#50623 = CARTESIAN_POINT ( 'NONE',  ( 52.73888932328210188, -49.67618315451370137, -27.47948615241350012 ) ) ;
#50624 = EDGE_CURVE ( 'NONE', #16095, #4073, #40987, .T. ) ;
#50625 = CARTESIAN_POINT ( 'NONE',  ( 56.50063657765719682, -50.76119911934350171, -74.14935534434708586 ) ) ;
#50627 = CARTESIAN_POINT ( 'NONE',  ( 41.15616284062399188, -39.66885904924578909, -80.40208926020751790 ) ) ;
#50626 = CARTESIAN_POINT ( 'NONE',  ( -2.574198652525490072, 19.80097958437369954, -8.360332649887961765 ) ) ;
#50628 = CARTESIAN_POINT ( 'NONE',  ( 47.32222669057270537, -54.70165496723960530, -54.63504270530570039 ) ) ;
#50629 = CYLINDRICAL_SURFACE ( 'NONE', #18065, 1.000000000000001110 ) ;
#50630 = EDGE_CURVE ( 'NONE', #23138, #50553, #2192, .T. ) ;
#50631 = ORIENTED_EDGE ( 'NONE', *, *, #45311, .F. ) ;
#50632 = CARTESIAN_POINT ( 'NONE',  ( 52.82975622904280755, -49.66092049964720445, -48.48626292588439668 ) ) ;
#50633 = CARTESIAN_POINT ( 'NONE',  ( 47.79460208473339833, 23.17020998024509737, -54.69564055610090492 ) ) ;
#50634 = FACE_OUTER_BOUND ( 'NONE', #47685, .T. ) ;
#50635 = CARTESIAN_POINT ( 'NONE',  ( 84.42051414649773733, -43.53095039421000223, -47.44928429663789160 ) ) ;
#50636 = DIRECTION ( 'NONE',  ( 0.000000000000000000, -1.000000000000000000, 0.000000000000000000 ) ) ;
#50637 = CARTESIAN_POINT ( 'NONE',  ( 12.05606148284509871, 33.93520160465880053, -16.66333073003769627 ) ) ;
#50638 = CARTESIAN_POINT ( 'NONE',  ( 9.367334447929739127, -15.61631861598680082, -57.84717978380999170 ) ) ;
#50639 = CARTESIAN_POINT ( 'NONE',  ( 53.30584942118750291, 18.17910404770230315, -48.80307101436750372 ) ) ;
#50640 = CARTESIAN_POINT ( 'NONE',  ( 18.38892583657722923, 24.32148015893219650, -76.14999999999999147 ) ) ;
#50641 = DIRECTION ( 'NONE',  ( 0.4145156864928219442, -0.9100421669633690369, 0.000000000000000000 ) ) ;
#50642 = CARTESIAN_POINT ( 'NONE',  ( 52.89288899001359567, 18.34731072048720080, -27.71426086418919965 ) ) ;
#50643 = AXIS2_PLACEMENT_3D ( 'NONE', #13551, #20607, #36600 ) ;
#50644 = CARTESIAN_POINT ( 'NONE',  ( 50.61900101762439874, 4.651609355440132987, -76.23853349069526075 ) ) ;
#50645 = CARTESIAN_POINT ( 'NONE',  ( 23.83903461665352097, -13.54549833210122856, -37.70900104367377281 ) ) ;
#50646 = CARTESIAN_POINT ( 'NONE',  ( 52.70698220066480388, 18.52838197885590077, -48.81385519956149466 ) ) ;
#50647 = CARTESIAN_POINT ( 'NONE',  ( 8.222281512103441159, -15.61614627842319969, -76.50766849176299900 ) ) ;
#50648 = CARTESIAN_POINT ( 'NONE',  ( 71.23719564129540061, 1.194703186106690129, -60.63553603340079690 ) ) ;
#50649 = CARTESIAN_POINT ( 'NONE',  ( 10.77427333304090062, 32.15375400438119868, -45.20766266540499601 ) ) ;
#50650 = DIRECTION ( 'NONE',  ( 0.000000000000000000, 1.000000000000000000, 0.000000000000000000 ) ) ;
#50651 = CARTESIAN_POINT ( 'NONE',  ( 13.20770907579910158, -46.26637462015160196, -23.15000000000000213 ) ) ;
#50652 = EDGE_CURVE ( 'NONE', #45496, #14025, #22995, .T. ) ;
#50653 = CARTESIAN_POINT ( 'NONE',  ( 53.63393739769619373, -62.11618894467930119, 16.35000000000000142 ) ) ;
#50654 = ORIENTED_EDGE ( 'NONE', *, *, #40911, .T. ) ;
#50655 = VERTEX_POINT ( 'NONE', #37838 ) ;
#50656 = CARTESIAN_POINT ( 'NONE',  ( 22.84151302485214075, -17.15290527753463934, -36.91946906410927198 ) ) ;
#50657 = AXIS2_PLACEMENT_3D ( 'NONE', #14270, #23647, #27087 ) ;
#50658 = EDGE_CURVE ( 'NONE', #33090, #25965, #41760, .T. ) ;
#50659 = CARTESIAN_POINT ( 'NONE',  ( 51.01907554470725614, 0.1776427667142097822, -16.88746765477635847 ) ) ;
#50660 = ORIENTED_EDGE ( 'NONE', *, *, #23318, .F. ) ;
#50661 = CARTESIAN_POINT ( 'NONE',  ( 11.30321776117639843, -64.33719732150139237, -44.46574515417460560 ) ) ;
#50662 = CARTESIAN_POINT ( 'NONE',  ( 55.86565860574650344, -45.97208290794810637, -25.40205046782289955 ) ) ;
#50663 = CARTESIAN_POINT ( 'NONE',  ( 21.61927372987474172, -21.31691565204681638, -77.76379145751687361 ) ) ;
#50664 = CARTESIAN_POINT ( 'NONE',  ( 63.53329261246669546, 1.393731187554809958, -68.81053500035210391 ) ) ;
#50665 = VERTEX_POINT ( 'NONE', #9294 ) ;
#50666 = CARTESIAN_POINT ( 'NONE',  ( 16.13393739769599833, 14.38381105532070059, -35.14999999999999858 ) ) ;
#50667 = CARTESIAN_POINT ( 'NONE',  ( 43.88591490443007359, 6.670162465103853577, -70.89007156030166357 ) ) ;
#50668 = CARTESIAN_POINT ( 'NONE',  ( 11.36486248725049997, 32.41286963914479458, -24.38092508955430304 ) ) ;
#50669 = ORIENTED_EDGE ( 'NONE', *, *, #34835, .T. ) ;
#50670 = CARTESIAN_POINT ( 'NONE',  ( 7.912936474371079498, -14.98542442814910025, -34.81670639671899892 ) ) ;
#50671 = DIRECTION ( 'NONE',  ( 0.000000000000000000, 0.000000000000000000, -1.000000000000000000 ) ) ;
#50672 = CARTESIAN_POINT ( 'NONE',  ( 14.34399776555499884, 19.88381105071939814, -22.49261467888849708 ) ) ;
#50673 = CARTESIAN_POINT ( 'NONE',  ( 16.16386221864532047, -22.38313233367915345, -46.95141631609453015 ) ) ;
#50674 = CARTESIAN_POINT ( 'NONE',  ( 63.19468704395289649, 0.8986939045430389905, -62.24348040161360274 ) ) ;
#50675 = CARTESIAN_POINT ( 'NONE',  ( 47.30599826317899215, -54.71628134471639981, -74.19801721955809626 ) ) ;
#50676 = CARTESIAN_POINT ( 'NONE',  ( 52.00606832011370528, 13.88381313913080106, -8.714322203361728469 ) ) ;
#50677 = VECTOR ( 'NONE', #41138, 1000.000000000000000 ) ;
#50678 = AXIS2_PLACEMENT_3D ( 'NONE', #4453, #40101, #770 ) ;
#50679 = PLANE ( 'NONE',  #3347 ) ;
#50680 = CARTESIAN_POINT ( 'NONE',  ( 61.65645849501900244, 13.88380407631539981, -27.60631482466889963 ) ) ;
#50681 = CARTESIAN_POINT ( 'NONE',  ( 19.93821446653229756, -8.301122528535961109, -35.16031938041749783 ) ) ;
#50682 = B_SPLINE_SURFACE_WITH_KNOTS ( 'NONE', 3, 3, ( 
 ( #42732, #35098, #23285, #35362, #39308, #6559, #2632, #46928, #27491, #6827, #11012, #19119, #22779, #22524, #18341, #31411, #51361, #11534, #3411, #34582, #38799, #2893 ),
 ( #2363, #26983, #18858, #34843, #14934, #7600, #50586, #34318, #23036, #23544, #46411, #51099, #43498, #39058, #50843, #3151, #14419, #38536, #27232, #18604, #14676, #19379 ),
 ( #30387, #30899, #42990, #15198, #7086, #30646, #10499, #47439, #15461, #42470, #10754, #26713, #31157, #47185, #43250, #35877, #48718, #8884, #27753, #4166, #15970, #40583 ),
 ( #12047, #741, #48452, #4681, #43750, #36132, #39816, #12557, #44257, #31924, #20653, #486, #12298, #20394, #39562, #32430, #24570, #44517, #8364, #16475, #237, #34365 ),
 ( #32177, #48193, #51616, #19638, #40073, #36638, #28520, #3668, #16739, #8623, #12822, #32693, #47689, #28257, #7852, #44779, #3926, #47946, #24313, #36381, #28780, #35630 ),
 ( #19886, #28000, #40331, #11793, #15709, #31666, #23802, #44006, #8109, #24055, #20143, #16222, #4424, #37431, #37688, #25609, #45819, #9655, #33487, #33738, #40843, #5474 ),
 ( #4942, #1786, #45557, #21428, #13092, #29044, #41880, #20917, #5217, #13589, #9907, #13843, #49753, #1529, #29298, #17011, #5723, #36911, #1013, #1274, #17515, #45040 ),
 ( #29801, #32959, #49243, #29554, #48988, #41614, #9139, #25095, #13338, #41107, #21172, #21677, #37177, #17767, #17265, #45299, #33225, #49501, #25865, #24836, #9408, #41359 ),
 ( #25356, #47849, #24740, #48360, #4330, #20299, #28943, #36289, #655, #39982, #51773, #4075, #40751, #16124, #8530, #32859, #12993, #16913, #399, #48889, #48626, #44948 ),
 ( #9048, #20046, #28681, #36038, #146, #4851, #12726, #32085, #24215, #24995, #43913, #32341, #28163, #16638, #16383, #919, #41014, #20818, #48104, #19801, #35790, #15878 ) ),
 .UNSPECIFIED., .F., .F., .F.,
 ( 4, 1, 1, 1, 1, 1, 1, 4 ),
 ( 4, 2, 2, 2, 2, 2, 2, 2, 2, 2, 4 ),
 ( -2.341432999999999973E-10, 0.1428571428571430157, 0.2857142857142860315, 0.4285714285714289917, 0.5714285714285709528, 0.7142857142857139685, 0.8571428571428569843, 1.000000000234150033 ),
 ( -8.594361155364929061, -7.576833180893860487, -6.384773949355639466, -5.367405169037740009, -4.291753173673400035, -3.753927175991219833, -2.893405579699740215, -2.204988302666559985, -1.516571025633369985, -0.4151033823802809941, 0.01085480778399900044 ),
 .UNSPECIFIED. ) ;
#50683 = ORIENTED_EDGE ( 'NONE', *, *, #913, .F. ) ;
#50684 = CARTESIAN_POINT ( 'NONE',  ( 54.05043764316730659, -48.58749351201610267, -26.96881999329520241 ) ) ;
#50685 = EDGE_CURVE ( 'NONE', #23063, #20497, #15083, .T. ) ;
#50686 = CARTESIAN_POINT ( 'NONE',  ( -5.040141449686119657, -47.05667976586999401, -4.957448605375669892 ) ) ;
#50687 = CARTESIAN_POINT ( 'NONE',  ( 76.35984344540050017, -21.83182212063609740, -12.62201988643909978 ) ) ;
#50688 = CARTESIAN_POINT ( 'NONE',  ( 75.16286580954648855, 13.70473030084525767, -14.50431359832863620 ) ) ;
#50689 = CARTESIAN_POINT ( 'NONE',  ( 61.09721242536592456, -45.48235634517234161, -47.46777540746526824 ) ) ;
#50690 = CARTESIAN_POINT ( 'NONE',  ( 14.15073023633500071, 1.361188710403610003, -35.02127583263639821 ) ) ;
#50691 = DIRECTION ( 'NONE',  ( 0.000000000000000000, 0.000000000000000000, 1.000000000000000000 ) ) ;
#50692 = AXIS2_PLACEMENT_3D ( 'NONE', #42399, #18793, #45552 ) ;
#50693 = FACE_OUTER_BOUND ( 'NONE', #11215, .T. ) ;
#50694 = CARTESIAN_POINT ( 'NONE',  ( 73.01385068780759013, 0.9098571636355720083, -62.15909090909049439 ) ) ;
#50695 = CARTESIAN_POINT ( 'NONE',  ( 41.39168664676449794, 12.97209261023169979, -4.419063984731860018 ) ) ;
#50696 = FACE_OUTER_BOUND ( 'NONE', #21314, .T. ) ;
#50697 = CARTESIAN_POINT ( 'NONE',  ( 49.42204313923179626, -53.51403126671309707, -54.19389682688790089 ) ) ;
#50698 = AXIS2_PLACEMENT_3D ( 'NONE', #36174, #43545, #7895 ) ;
#50699 = DIRECTION ( 'NONE',  ( 0.000000000000000000, 0.000000000000000000, 1.000000000000000000 ) ) ;
#50700 = CARTESIAN_POINT ( 'NONE',  ( 75.79443952681172902, -43.34572367340545185, -13.52171987147115750 ) ) ;
#50701 = CARTESIAN_POINT ( 'NONE',  ( 18.01252544226889896, -51.38128844478560353, -75.14498753491579919 ) ) ;
#50702 = CARTESIAN_POINT ( 'NONE',  ( 60.59355682701219337, -44.96618261540349692, -10.31481105180509950 ) ) ;
#50703 = VERTEX_POINT ( 'NONE', #33101 ) ;
#50704 = CARTESIAN_POINT ( 'NONE',  ( 15.97580875125819944, -23.06479214726149962, -53.57409916825699270 ) ) ;
#50705 = CARTESIAN_POINT ( 'NONE',  ( 63.74194282759800245, 1.270920007605170099, -61.65828220330239873 ) ) ;
#50706 = ORIENTED_EDGE ( 'NONE', *, *, #38110, .T. ) ;
#50707 = DIRECTION ( 'NONE',  ( 0.000000000000000000, 0.000000000000000000, 1.000000000000000000 ) ) ;
#50708 = CYLINDRICAL_SURFACE ( 'NONE', #44341, 2.999999999999999112 ) ;
#50709 = CARTESIAN_POINT ( 'NONE',  ( 72.83058059882510804, 1.382840740411490188, -68.63401718432778864 ) ) ;
#50710 = CARTESIAN_POINT ( 'NONE',  ( 45.32643724771776306, 8.820270950418585443, -60.22851707904983698 ) ) ;
#50711 = AXIS2_PLACEMENT_3D ( 'NONE', #24749, #406, #27666 ) ;
#50712 = CARTESIAN_POINT ( 'NONE',  ( 9.544598273871880423, -17.84714125077449864, -81.23899999999999011 ) ) ;
#50713 = CARTESIAN_POINT ( 'NONE',  ( 45.22526645711639759, -45.57792172170950806, -8.601017710285070450 ) ) ;
#50714 = ORIENTED_EDGE ( 'NONE', *, *, #39212, .T. ) ;
#50715 = AXIS2_PLACEMENT_3D ( 'NONE', #17806, #42707, #2866 ) ;
#50716 = ORIENTED_EDGE ( 'NONE', *, *, #8618, .T. ) ;
#50717 = EDGE_CURVE ( 'NONE', #49113, #22505, #3342, .T. ) ;
#50718 = EDGE_LOOP ( 'NONE', ( #3336, #39053, #45129, #17610 ) ) ;
#50719 = CARTESIAN_POINT ( 'NONE',  ( 74.13393739769620083, -42.11618894467930119, -65.65000000000000568 ) ) ;
#50720 = CARTESIAN_POINT ( 'NONE',  ( 61.09780586005280156, -45.32905657884899853, -46.84341276801610121 ) ) ;
#50721 = DIRECTION ( 'NONE',  ( 0.9244418645452657790, 4.067568864690730049E-12, 0.3813230114693739181 ) ) ;
#50722 = CARTESIAN_POINT ( 'NONE',  ( -15.32468133715470238, -15.61618894467930296, -81.65000000000000568 ) ) ;
#50723 = VERTEX_POINT ( 'NONE', #9802 ) ;
#50724 = LINE ( 'NONE', #31555, #7356 ) ;
#50725 = EDGE_LOOP ( 'NONE', ( #13721, #44138, #29598, #50777 ) ) ;
#50726 = DIRECTION ( 'NONE',  ( 1.000000000000000000, 0.000000000000000000, 0.000000000000000000 ) ) ;
#50727 = CARTESIAN_POINT ( 'NONE',  ( 83.89200044194980421, -50.61618894467930119, -53.92796738110899923 ) ) ;
#50728 = EDGE_LOOP ( 'NONE', ( #50527, #31920, #31732, #38267 ) ) ;
#50729 = CARTESIAN_POINT ( 'NONE',  ( 60.83133137330749918, -45.46867109277970087, -47.01992810568810199 ) ) ;
#50730 = CARTESIAN_POINT ( 'NONE',  ( 51.42345331545769227, -50.56011499177679980, -76.23764483251279955 ) ) ;
#50731 = CARTESIAN_POINT ( 'NONE',  ( 60.63179223956819897, 14.34380986286560145, -47.21451266482660714 ) ) ;
#50732 = CIRCLE ( 'NONE', #13929, 9.000000000000007105 ) ;
#50733 = DIRECTION ( 'NONE',  ( 0.000000000000000000, 0.000000000000000000, 1.000000000000000000 ) ) ;
#50734 = CARTESIAN_POINT ( 'NONE',  ( 41.98583910622449622, -43.58195263108250117, -3.946145645806039770 ) ) ;
#50735 = PRODUCT_RELATED_PRODUCT_CATEGORY ( 'part', '', ( #16002 ) ) ;
#50736 = CARTESIAN_POINT ( 'NONE',  ( 57.50723796702470025, 15.88381105532069704, -17.93019253464870033 ) ) ;
#50737 = CARTESIAN_POINT ( 'NONE',  ( -7.073749351297280441, 14.53014294518820115, -5.239700901386809662 ) ) ;
#50738 = CARTESIAN_POINT ( 'NONE',  ( 64.34681638194778941, 1.254582981797469854, -70.20495024723810218 ) ) ;
#50739 = VECTOR ( 'NONE', #20827, 1000.000000000000000 ) ;
#50740 = DIRECTION ( 'NONE',  ( 0.000000000000000000, 0.000000000000000000, -1.000000000000000000 ) ) ;
#50741 = DIRECTION ( 'NONE',  ( 0.000000000000000000, 0.000000000000000000, 1.000000000000000000 ) ) ;
#50742 = CARTESIAN_POINT ( 'NONE',  ( 8.343752523778771746, -16.56474986173779840, -48.24893689645469408 ) ) ;
#50743 = VERTEX_POINT ( 'NONE', #45701 ) ;
#50744 = AXIS2_PLACEMENT_3D ( 'NONE', #7782, #7525, #35556 ) ;
#50745 = B_SPLINE_CURVE_WITH_KNOTS ( 'NONE', 3,
 ( #15412, #31111, #3618, #19072, #43448, #35580, #32128, #7550, #51565, #15667, #27952, #35045, #23241, #51054, #40027, #51818 ),
 .UNSPECIFIED., .F., .F.,
 ( 4, 2, 2, 2, 2, 2, 2, 4 ),
 ( -8.881783999999999806E-15, 0.07319275283555599920, 0.1391693187718399949, 0.1804046724820169978, 0.2061767685508779924, 0.2577209606886000093, 0.3401916681089540151, 0.4123535371017650331 ),
 .UNSPECIFIED. ) ;
#50746 = CARTESIAN_POINT ( 'NONE',  ( 14.74661529360900047, -52.24941868644869913, -75.96018872839380265 ) ) ;
#50747 = EDGE_CURVE ( 'NONE', #50419, #45223, #9226, .T. ) ;
#50748 = LINE ( 'NONE', #6732, #34443 ) ;
#50749 = CARTESIAN_POINT ( 'NONE',  ( 72.03549263123640856, 1.087300712304640093, -70.20170571670161053 ) ) ;
#50750 = B_SPLINE_CURVE_WITH_KNOTS ( 'NONE', 3,
 ( #34237, #50774, #14864, #30828 ),
 .UNSPECIFIED., .F., .F.,
 ( 4, 4 ),
 ( 0.000000000000000000, 19.53260001885960051 ),
 .UNSPECIFIED. ) ;
#50751 = CARTESIAN_POINT ( 'NONE',  ( 45.73065097657321587, -40.07790899994112976, -58.26712722073379069 ) ) ;
#50752 = EDGE_CURVE ( 'NONE', #29814, #11667, #13587, .T. ) ;
#50753 = CARTESIAN_POINT ( 'NONE',  ( 15.53208191794040083, 19.63190946341060084, -20.56249370038050017 ) ) ;
#50754 = EDGE_CURVE ( 'NONE', #31343, #9229, #6722, .T. ) ;
#50755 = CARTESIAN_POINT ( 'NONE',  ( 22.10482594698319758, -11.98148934663060139, -32.14999999999999858 ) ) ;
#50756 = EDGE_CURVE ( 'NONE', #47619, #31811, #17662, .T. ) ;
#50757 = CARTESIAN_POINT ( 'NONE',  ( 63.24043675930629860, 1.099344084866040072, -69.05806188122140554 ) ) ;
#50758 = CARTESIAN_POINT ( 'NONE',  ( 48.02969574711249834, -54.30226728297670036, -54.78113594584849722 ) ) ;
#50759 = CARTESIAN_POINT ( 'NONE',  ( 24.04493739769670313, -15.61618198714410610, -45.50767582953553614 ) ) ;
#50760 = CARTESIAN_POINT ( 'NONE',  ( 71.33393739769628894, 1.883811055320669947, -61.44999999999999574 ) ) ;
#50761 = CARTESIAN_POINT ( 'NONE',  ( 22.46009103554561293, -10.75449509031862938, -71.58399138287670382 ) ) ;
#50762 = ORIENTED_EDGE ( 'NONE', *, *, #7474, .T. ) ;
#50763 = CARTESIAN_POINT ( 'NONE',  ( 9.778345137114559549, -12.55857448374969998, -69.98991178896608290 ) ) ;
#50764 =( BOUNDED_SURFACE ( )  B_SPLINE_SURFACE ( 2, 2, ( 
 ( #21594, #17939, #45472 ),
 ( #49926, #33399, #45732 ),
 ( #5648, #14277, #37593 ) ),
 .UNSPECIFIED., .F., .F., .T. ) 
 B_SPLINE_SURFACE_WITH_KNOTS ( ( 3, 3 ),
 ( 3, 3 ),
 ( -1.570796326792230024, -3.926887462493479784E-13 ),
 ( -8.405333417276831159E-12, 1.570796326803189924 ),
 .UNSPECIFIED. ) 
 GEOMETRIC_REPRESENTATION_ITEM ( )  RATIONAL_B_SPLINE_SURFACE ( (
 ( 1.000000000000000000, 0.7071067811806429626, 1.000000000000000000),
 ( 0.7071067811876210474, 0.4999999999965839548, 0.7071067811876210474),
 ( 1.000000000000000000, 0.7071067811806429626, 1.000000000000000000) ) ) 
 REPRESENTATION_ITEM ( '' )  SURFACE ( )  );
#50765 = ORIENTED_EDGE ( 'NONE', *, *, #44590, .F. ) ;
#50766 = CARTESIAN_POINT ( 'NONE',  ( 71.50903575780739629, 0.9989215084293960878, -70.60223669534680369 ) ) ;
#50767 = CYLINDRICAL_SURFACE ( 'NONE', #19202, 13.50000000000000178 ) ;
#50768 = AXIS2_PLACEMENT_3D ( 'NONE', #26305, #26563, #47038 ) ;
#50769 = CARTESIAN_POINT ( 'NONE',  ( 82.75389495153045516, 14.36254469553479574, -47.67225488023363766 ) ) ;
#50770 = CARTESIAN_POINT ( 'NONE',  ( 83.36355414428213351, 14.11443836545216968, -47.55048134665359783 ) ) ;
#50771 = EDGE_CURVE ( 'NONE', #43577, #41820, #20483, .T. ) ;
#50773 = CARTESIAN_POINT ( 'NONE',  ( 14.34415610061919821, -8.794221333858748935, -58.26550999155039534 ) ) ;
#50772 = CARTESIAN_POINT ( 'NONE',  ( 83.69028489729539899, 13.83794172252809851, -47.49660994411200221 ) ) ;
#50774 = CARTESIAN_POINT ( 'NONE',  ( 8.900684698865370947, 16.90943255658890010, -48.24693240561549601 ) ) ;
#50775 = CARTESIAN_POINT ( 'NONE',  ( 71.36799767121759430, 0.8859637708054480809, -70.70388507757908769 ) ) ;
#50776 = DIRECTION ( 'NONE',  ( 1.000000000000000000, 2.460964292799963328E-14, 0.000000000000000000 ) ) ;
#50777 = ORIENTED_EDGE ( 'NONE', *, *, #29155, .T. ) ;
#50778 = CYLINDRICAL_SURFACE ( 'NONE', #2210, 0.4999999999999967248 ) ;
#50779 = ORIENTED_EDGE ( 'NONE', *, *, #34759, .F. ) ;
#50780 = ADVANCED_FACE ( 'NONE', ( #44020 ), #32585, .F. ) ;
#50781 = ORIENTED_EDGE ( 'NONE', *, *, #28621, .F. ) ;
#50782 = CARTESIAN_POINT ( 'NONE',  ( 11.88460916115749910, -64.82510961609500555, -16.16716782998640056 ) ) ;
#50783 = CARTESIAN_POINT ( 'NONE',  ( 7.695097139525112873, -60.75237708241192536, -20.68192065308969418 ) ) ;
#50784 = CARTESIAN_POINT ( 'NONE',  ( 76.49394062354240020, -27.97249612882005465, -13.20130748058310388 ) ) ;
#50785 = CARTESIAN_POINT ( 'NONE',  ( 9.381135691567910939, -63.38818850907809832, -46.50683779583690125 ) ) ;
#50786 = AXIS2_PLACEMENT_3D ( 'NONE', #467, #12026, #27731 ) ;
#50787 = ORIENTED_EDGE ( 'NONE', *, *, #10867, .F. ) ;
#50788 = ORIENTED_EDGE ( 'NONE', *, *, #30266, .F. ) ;
#50789 = LINE ( 'NONE', #22723, #39340 ) ;
#50790 = AXIS2_PLACEMENT_3D ( 'NONE', #24927, #36476, #24408 ) ;
#50791 = LINE ( 'NONE', #39002, #31223 ) ;
#50792 = CARTESIAN_POINT ( 'NONE',  ( 16.13393739769599833, 14.38381105532070059, -62.64999999999999858 ) ) ;
#50793 = CARTESIAN_POINT ( 'NONE',  ( 64.61005101894130576, 0.6433700368313129969, -17.35087735437779699 ) ) ;
#50794 = CARTESIAN_POINT ( 'NONE',  ( 52.19990148684729547, -49.79086060043429995, -77.09681897153029695 ) ) ;
#50795 = CARTESIAN_POINT ( 'NONE',  ( 58.72540476535390042, -48.17849370114159768, -50.40155767129670039 ) ) ;
#50796 = VERTEX_POINT ( 'NONE', #15016 ) ;
#50797 = DIRECTION ( 'NONE',  ( 1.000000000000000000, 0.000000000000000000, 0.000000000000000000 ) ) ;
#50798 = DIRECTION ( 'NONE',  ( 0.6415444970810866288, 0.4854844151940982400, 0.5939070136550167467 ) ) ;
#50799 = ORIENTED_EDGE ( 'NONE', *, *, #21791, .T. ) ;
#50800 = CARTESIAN_POINT ( 'NONE',  ( 9.366908763506170743, -15.61636271700460021, -33.45282021618999835 ) ) ;
#50801 = DIRECTION ( 'NONE',  ( 1.000000000000000000, 0.000000000000000000, 0.000000000000000000 ) ) ;
#50802 = ADVANCED_FACE ( 'NONE', ( #10580 ), #25901, .T. ) ;
#50803 = CARTESIAN_POINT ( 'NONE',  ( 19.20059249649200339, -22.83992579596429806, -44.38470316487709511 ) ) ;
#50804 = CARTESIAN_POINT ( 'NONE',  ( 14.01755875199390111, -51.05430465436170806, -22.03916537273070020 ) ) ;
#50805 = LINE ( 'NONE', #31628, #39335 ) ;
#50806 = CARTESIAN_POINT ( 'NONE',  ( 57.06558336992600289, 13.88381105532070059, -16.29907433820719831 ) ) ;
#50807 = CARTESIAN_POINT ( 'NONE',  ( 60.66036723437029821, -45.55824399519830337, -47.11242429048819957 ) ) ;
#50808 = CARTESIAN_POINT ( 'NONE',  ( 71.19761362482960010, 1.388189907116970101, -70.28386057589720792 ) ) ;
#50809 = CARTESIAN_POINT ( 'NONE',  ( 9.081105072284950452, -15.60544817723029887, -43.84766453797169561 ) ) ;
#50810 = CARTESIAN_POINT ( 'NONE',  ( 75.47966807050509885, -43.37310274687460065, -13.40512917118210012 ) ) ;
#50811 = EDGE_LOOP ( 'NONE', ( #48999, #13993 ) ) ;
#50812 = CARTESIAN_POINT ( 'NONE',  ( 47.61774400735439627, 23.31213713685490418, -74.19770771130870912 ) ) ;
#50813 = CARTESIAN_POINT ( 'NONE',  ( 65.07026117056290104, 1.388189907116970101, -61.01613942410280345 ) ) ;
#50814 = CARTESIAN_POINT ( 'NONE',  ( 44.67725961099969822, -46.10245440686500018, -8.756022344162619930 ) ) ;
#50815 = EDGE_CURVE ( 'NONE', #6439, #29653, #17995, .T. ) ;
#50816 = DIRECTION ( 'NONE',  ( -1.000000000000000000, 0.000000000000000000, 0.000000000000000000 ) ) ;
#50817 = CARTESIAN_POINT ( 'NONE',  ( 14.06332624887442861, -7.911071329197555180, -46.92433573622849252 ) ) ;
#50818 = CIRCLE ( 'NONE', #27348, 1.999999999999996669 ) ;
#50819 = DIRECTION ( 'NONE',  ( 0.000000000000000000, -1.000000000000000000, 0.000000000000000000 ) ) ;
#50820 = ADVANCED_FACE ( 'NONE', ( #35892 ), #30984, .T. ) ;
#50821 = CARTESIAN_POINT ( 'NONE',  ( 82.51403489249999268, 13.88629484321260144, -46.70334943848269660 ) ) ;
#50822 = CARTESIAN_POINT ( 'NONE',  ( -18.35260750266889929, 3.120353346132920258, -50.84549189752459597 ) ) ;
#50824 = DIRECTION ( 'NONE',  ( 0.000000000000000000, 1.000000000000000000, 0.000000000000000000 ) ) ;
#50823 = CARTESIAN_POINT ( 'NONE',  ( 52.97776614862323896, 19.06888045206829574, -77.23905649707201349 ) ) ;
#50825 = CARTESIAN_POINT ( 'NONE',  ( 50.76363268875235235, -51.12586965113521131, 16.21999999999999886 ) ) ;
#50826 = CARTESIAN_POINT ( 'NONE',  ( 48.95529619442159941, 22.62706584891199668, -54.62080953740519362 ) ) ;
#50827 = VERTEX_POINT ( 'NONE', #10319 ) ;
#50828 = CARTESIAN_POINT ( 'NONE',  ( 52.89023673218689936, -49.63844819782259776, -48.86102656628040108 ) ) ;
#50829 = ORIENTED_EDGE ( 'NONE', *, *, #30464, .T. ) ;
#50830 = CARTESIAN_POINT ( 'NONE',  ( 41.02599897614819469, 8.452786747797132350, -80.89672324886578281 ) ) ;
#50831 = DIRECTION ( 'NONE',  ( 0.000000000000000000, 0.000000000000000000, -1.000000000000000000 ) ) ;
#50832 = CARTESIAN_POINT ( 'NONE',  ( 13.99025901751500101, 19.94838289472389903, -22.90514570209199974 ) ) ;
#50833 = CARTESIAN_POINT ( 'NONE',  ( 52.26504646883520167, -49.78354544620959388, -77.19463087837650050 ) ) ;
#50834 = CARTESIAN_POINT ( 'NONE',  ( 23.16873431782460102, -15.11201537419210084, -52.43004635228659538 ) ) ;
#50835 = CARTESIAN_POINT ( 'NONE',  ( 53.02886661541120361, 18.37360774895879700, -49.08317481420909445 ) ) ;
#50836 = CARTESIAN_POINT ( 'NONE',  ( 55.92660166244869657, -45.72950351173099648, -17.10190867576899976 ) ) ;
#50837 = CARTESIAN_POINT ( 'NONE',  ( 44.13393739769620083, 1.883811055320659955, -54.27132075603810080 ) ) ;
#50838 = ORIENTED_EDGE ( 'NONE', *, *, #37197, .T. ) ;
#50839 = CARTESIAN_POINT ( 'NONE',  ( 23.94572442901580089, -14.86603458648409948, -35.25703220202099430 ) ) ;
#50840 = EDGE_CURVE ( 'NONE', #34516, #42834, #32868, .T. ) ;
#50841 = VERTEX_POINT ( 'NONE', #42551 ) ;
#50842 = CARTESIAN_POINT ( 'NONE',  ( 73.03096648148358838, 1.005545696829380109, -69.10544663728329340 ) ) ;
#50843 = CARTESIAN_POINT ( 'NONE',  ( 11.46849097211869939, 34.01295885014749842, -47.29791990983230221 ) ) ;
#50844 = CARTESIAN_POINT ( 'NONE',  ( 72.72759757326660690, 1.395196698723390138, -62.46966344801350601 ) ) ;
#50845 = FACE_OUTER_BOUND ( 'NONE', #7211, .T. ) ;
#50846 = CARTESIAN_POINT ( 'NONE',  ( 53.41693480164780539, 18.12090330447910347, -48.75416851879779756 ) ) ;
#50847 = CARTESIAN_POINT ( 'NONE',  ( -2.927827710953269769, 17.96742650791509988, -5.740515240579870060 ) ) ;
#50848 = CARTESIAN_POINT ( 'NONE',  ( 51.07994173643560032, -52.78781467787970882, -53.74568964421160189 ) ) ;
#50849 = EDGE_LOOP ( 'NONE', ( #19579, #342, #44151, #29491, #41305, #39951, #17721 ) ) ;
#50850 = CARTESIAN_POINT ( 'NONE',  ( 64.66786723518761448, 0.9395704634982849912, -70.54765821028060202 ) ) ;
#50851 = ORIENTED_EDGE ( 'NONE', *, *, #24513, .T. ) ;
#50852 = CARTESIAN_POINT ( 'NONE',  ( 9.731586802489630372, -63.16114365233679706, -46.29992529111800081 ) ) ;
#50853 = CARTESIAN_POINT ( 'NONE',  ( 12.14986582965795670, -8.703631913686264099, -47.12566550774506169 ) ) ;
#50854 = ORIENTED_EDGE ( 'NONE', *, *, #23701, .F. ) ;
#50855 = CARTESIAN_POINT ( 'NONE',  ( 11.13393739769619906, -63.52234721269329754, -43.76018303787720498 ) ) ;
#50856 = CARTESIAN_POINT ( 'NONE',  ( 57.00264671592019994, 19.39868990108010038, -53.72993498978910054 ) ) ;
#50857 = CARTESIAN_POINT ( 'NONE',  ( 52.00136199551640459, 18.79993947043690028, -76.70561737979799943 ) ) ;
#50858 = VERTEX_POINT ( 'NONE', #23813 ) ;
#50859 = DIRECTION ( 'NONE',  ( 1.000000000000000000, 0.000000000000000000, 0.000000000000000000 ) ) ;
#50860 = PRODUCT_DEFINITION_SHAPE ( 'NONE', 'NONE',  #31487 ) ;
#50861 = CARTESIAN_POINT ( 'NONE',  ( 51.84413674030108155, 20.10506014047227197, -76.02231598272827284 ) ) ;
#50862 = DIRECTION ( 'NONE',  ( 0.6415444970810866288, 0.4854844151940982400, 0.5939070136550167467 ) ) ;
#50863 = CIRCLE ( 'NONE', #16503, 34.47562460986249278 ) ;
#50864 = CARTESIAN_POINT ( 'NONE',  ( 17.94297559678595988, -32.43785826095941616, -34.75586992539664521 ) ) ;
#50865 = ADVANCED_FACE ( 'NONE', ( #6907 ), #20078, .T. ) ;
#50866 = CARTESIAN_POINT ( 'NONE',  ( 10.99908320461310041, -9.165143101429379158, -65.07833806302170387 ) ) ;
#50867 = EDGE_CURVE ( 'NONE', #12484, #25175, #28455, .T. ) ;
#50868 = CARTESIAN_POINT ( 'NONE',  ( 22.46012711993053657, -20.47783328051634300, -47.71600292291422107 ) ) ;
#50869 = DIRECTION ( 'NONE',  ( -0.000000000000000000, 1.000000000000000000, 0.000000000000000000 ) ) ;
#50870 = AXIS2_PLACEMENT_3D ( 'NONE', #2952, #29674, #9785 ) ;
#50871 = ORIENTED_EDGE ( 'NONE', *, *, #6446, .T. ) ;
#50872 = ORIENTED_EDGE ( 'NONE', *, *, #21261, .T. ) ;
#50873 = CARTESIAN_POINT ( 'NONE',  ( 16.13393739769620083, -15.61618894467929941, -76.14999999999999147 ) ) ;
#50874 = CARTESIAN_POINT ( 'NONE',  ( 20.22938470947429934, -21.83985387152069890, -58.54739793472509746 ) ) ;
#50875 = CARTESIAN_POINT ( 'NONE',  ( 16.13393739769620083, -15.61618894467929941, -28.45282021618999835 ) ) ;
#50876 = CARTESIAN_POINT ( 'NONE',  ( 9.366937397696199596, -15.61618894467949836, -28.45282021618999835 ) ) ;
#50877 = CARTESIAN_POINT ( 'NONE',  ( 0.1416488651360941764, 14.72332773530568772, -34.68322412398370602 ) ) ;
#50878 = CARTESIAN_POINT ( 'NONE',  ( 51.13393739769620083, 19.38381105532069881, 16.21999999999999886 ) ) ;
#50879 = EDGE_CURVE ( 'NONE', #37502, #23561, #4179, .T. ) ;
#50880 = CARTESIAN_POINT ( 'NONE',  ( 12.21104395315670033, 33.65513056404519432, -16.16308188030659920 ) ) ;
#50881 = CARTESIAN_POINT ( 'NONE',  ( 13.08127967867459951, -7.956946060459409331, -62.88694525268430624 ) ) ;
#50882 = EDGE_CURVE ( 'NONE', #9229, #26724, #51658, .T. ) ;
#50883 = CARTESIAN_POINT ( 'NONE',  ( 21.65241842836849884, -21.01139045118939919, -32.14999999999999858 ) ) ;
#50884 = CARTESIAN_POINT ( 'NONE',  ( 53.82849609051940121, -50.85534700936450747, -76.11669736854409507 ) ) ;
#50886 = PLANE ( 'NONE',  #18863 ) ;
#50885 = CARTESIAN_POINT ( 'NONE',  ( -9.937296257482078232, 11.24462281463240032, -4.618840561276110535 ) ) ;
#50887 = CARTESIAN_POINT ( 'NONE',  ( 47.21829295900949575, -54.77949880278709571, -54.61684610847309784 ) ) ;
#50888 = DIRECTION ( 'NONE',  ( 0.000000000000000000, 1.000000000000000000, 0.000000000000000000 ) ) ;
#50889 = ORIENTED_EDGE ( 'NONE', *, *, #28034, .F. ) ;
#50890 = CARTESIAN_POINT ( 'NONE',  ( 28.13393739769619728, -22.54439217495490055, -35.14999999999999858 ) ) ;
#50891 = CARTESIAN_POINT ( 'NONE',  ( 47.75992848858749795, 23.21189837656569921, -54.79446835205050803 ) ) ;
#50892 = CIRCLE ( 'NONE', #25768, 5.499999999999998224 ) ;
#50893 = CARTESIAN_POINT ( 'NONE',  ( 41.99203386431830154, -44.88537213046480190, -5.712673480947970006 ) ) ;
#50894 = CARTESIAN_POINT ( 'NONE',  ( 63.54027722212589424, 1.395196698723379924, -62.46966344801359838 ) ) ;
#50895 = CARTESIAN_POINT ( 'NONE',  ( 61.41197480388229479, 14.20364326968670099, -47.45949227984320373 ) ) ;
#50896 = CARTESIAN_POINT ( 'NONE',  ( 11.65337899615939854, 33.98458825826539709, -16.97470857289490098 ) ) ;
#50897 = CARTESIAN_POINT ( 'NONE',  ( 51.51548137838339869, 17.54834764421520177, -76.79511588530829158 ) ) ;
#50898 = CARTESIAN_POINT ( 'NONE',  ( 52.79375783669770072, 18.44803353500160270, -48.48715717239780076 ) ) ;
#50899 = CARTESIAN_POINT ( 'NONE',  ( 20.11809198619220140, -22.52869821230809677, -70.12566693189073419 ) ) ;
#50900 = CARTESIAN_POINT ( 'NONE',  ( 53.02240710655760125, -49.55998530720779627, -48.78672999826209633 ) ) ;
#50901 = CARTESIAN_POINT ( 'NONE',  ( 56.36055665625740119, 14.84967702978789994, -26.17082522920440013 ) ) ;
#50902 = CARTESIAN_POINT ( 'NONE',  ( 16.13393739769620083, -15.61618894467929941, -28.45282021618999835 ) ) ;
#50903 = CARTESIAN_POINT ( 'NONE',  ( -31.36606260230380272, -53.11618894467930119, 11.84999999999999964 ) ) ;
#50904 = CARTESIAN_POINT ( 'NONE',  ( 12.24533245415720017, -64.90027884028160088, -16.17634614696339668 ) ) ;
#50905 = CARTESIAN_POINT ( 'NONE',  ( 62.63757649181060572, -31.25222801252620286, -16.75027474776850411 ) ) ;
#50906 = CARTESIAN_POINT ( 'NONE',  ( 71.19526263826620038, 1.274277262446069869, -60.70118609097839624 ) ) ;
#50907 = CARTESIAN_POINT ( 'NONE',  ( 11.13393739769619906, 32.16464604112239556, -43.91975316531460294 ) ) ;
#50908 = CARTESIAN_POINT ( 'NONE',  ( 72.78995442782039049, 1.368315088675930102, -62.33478283481320403 ) ) ;
#50909 = CARTESIAN_POINT ( 'NONE',  ( 66.13282620745420104, -31.02979715315369802, -17.01779704780440028 ) ) ;
#50910 = DIRECTION ( 'NONE',  ( 1.000000000000000000, 0.000000000000000000, 0.000000000000000000 ) ) ;
#50911 = ORIENTED_EDGE ( 'NONE', *, *, #7026, .F. ) ;
#50912 = EDGE_LOOP ( 'NONE', ( #13224, #33285, #49888, #48764, #51712 ) ) ;
#50913 = DIRECTION ( 'NONE',  ( -0.5481519472162221795, 0.4595820247375140832, -0.6987945372577201164 ) ) ;
#50914 = CARTESIAN_POINT ( 'NONE',  ( 49.69240448927909171, -1.840319678862813557, -15.81291498579800603 ) ) ;
#50915 = ORIENTED_EDGE ( 'NONE', *, *, #16903, .F. ) ;
#50916 = CARTESIAN_POINT ( 'NONE',  ( 12.69791550947999959, -65.47883885079799882, -47.19956182400449762 ) ) ;
#50917 = CARTESIAN_POINT ( 'NONE',  ( 56.67873295854410287, -45.30972226631099886, -25.50361698670420196 ) ) ;
#50918 = CARTESIAN_POINT ( 'NONE',  ( 46.25525774125583922, -33.99486860111965569, -35.14999999999999858 ) ) ;
#50919 = SHAPE_REPRESENTATION ( 'Wheel Axle Bolt', ( #20940 ), #854 ) ;
#50920 = CARTESIAN_POINT ( 'NONE',  ( 63.43393739769620510, 1.383811055320669947, -68.50657137141709541 ) ) ;
#50921 = ORIENTED_EDGE ( 'NONE', *, *, #41521, .T. ) ;
#50922 = CARTESIAN_POINT ( 'NONE',  ( 10.65677182350291297, 32.67421915925709186, -23.61757666224062291 ) ) ;
#50923 = CARTESIAN_POINT ( 'NONE',  ( 43.05104827289743952, 6.553104225060173427, -75.06444201244694625 ) ) ;
#50924 = CARTESIAN_POINT ( 'NONE',  ( 10.65234009212060151, 32.64172376425219824, -23.62431477846339689 ) ) ;
#50925 = ORIENTED_EDGE ( 'NONE', *, *, #33575, .F. ) ;
#50926 = CARTESIAN_POINT ( 'NONE',  ( 8.609312831402940347, -18.98705607306339971, -34.65826853459189749 ) ) ;
#50927 = ADVANCED_FACE ( 'NONE', ( #16487 ), #1284, .T. ) ;
#50928 = CARTESIAN_POINT ( 'NONE',  ( 51.19326779044995845, 0.4483973451604243987, -17.14369881442766541 ) ) ;
#50929 = CARTESIAN_POINT ( 'NONE',  ( 10.61754762155600140, 33.59328422689429772, -18.17417937929459981 ) ) ;
#50930 = CARTESIAN_POINT ( 'NONE',  ( 10.99043526536265958, -20.04924589561327153, -51.22642174526011871 ) ) ;
#50931 = ADVANCED_FACE ( 'NONE', ( #13349 ), #30745, .T. ) ;
#50932 = CARTESIAN_POINT ( 'NONE',  ( 60.03835289033210643, -29.28719532749419940, -15.81793802652529912 ) ) ;
#50933 = CARTESIAN_POINT ( 'NONE',  ( 63.18115153217100755, 0.8966068345641570181, -62.26318953425300862 ) ) ;
#50934 = CARTESIAN_POINT ( 'NONE',  ( 46.69862573999040478, -53.56655740942600374, -76.01558715013979395 ) ) ;
#50935 = CARTESIAN_POINT ( 'NONE',  ( 60.34784213368690331, 13.88381105527400017, -11.22423537798319870 ) ) ;
#50936 = CIRCLE ( 'NONE', #7433, 6.099999999999994316 ) ;
#50937 = DIRECTION ( 'NONE',  ( -0.7071067811865475727, 0.7071067811865475727, 0.000000000000000000 ) ) ;
#50938 = LINE ( 'NONE', #3510, #37365 ) ;
#50939 = CARTESIAN_POINT ( 'NONE',  ( 22.84203745199910074, -19.68904318595090075, -79.46119573552050497 ) ) ;
#50940 = ADVANCED_FACE ( 'NONE', ( #16685 ), #25039, .T. ) ;
#50941 = EDGE_LOOP ( 'NONE', ( #35708, #36002, #21615, #9516 ) ) ;
#50942 = CARTESIAN_POINT ( 'NONE',  ( 54.27327278922639664, -48.38567173727960125, -26.87344227122169826 ) ) ;
#50943 = B_SPLINE_CURVE_WITH_KNOTS ( 'NONE', 3,
 ( #16476, #4425, #44258, #48453, #12558, #21173, #28521, #44780, #32178, #44007, #12299, #32960, #8365 ),
 .UNSPECIFIED., .F., .F.,
 ( 4, 2, 2, 1, 2, 2, 4 ),
 ( 0.000000000000000000, 0.2499999999999940048, 0.3749999999999943379, 0.4374999999999973910, 0.4687499999999962808, 0.4999999999999952260, 1.000000000000000000 ),
 .UNSPECIFIED. ) ;
#50944 = CARTESIAN_POINT ( 'NONE',  ( 8.049435107523031263, -62.14063497384629642, -15.83799620030899824 ) ) ;
#50945 = CARTESIAN_POINT ( 'NONE',  ( 76.06651092694269778, 9.716726065570350457, -13.34696153651469963 ) ) ;
#50946 = DIRECTION ( 'NONE',  ( 0.6888026391158329487, -0.7071067811865494601, 0.1598465650148944150 ) ) ;
#50947 = CARTESIAN_POINT ( 'NONE',  ( 14.19855276898660001, 24.33696219936630101, -76.14999999999999147 ) ) ;
#50948 = DIRECTION ( 'NONE',  ( -0.7675009104025394269, -0.5576220516902739011, 0.3162277660168423266 ) ) ;
#50949 = CARTESIAN_POINT ( 'NONE',  ( 47.18324198357279897, 23.57489020266570279, -54.61058319554400242 ) ) ;
#50950 = CARTESIAN_POINT ( 'NONE',  ( 57.42460124420632894, 18.88910505960214437, -52.60814507333387979 ) ) ;
#50951 = CARTESIAN_POINT ( 'NONE',  ( 57.49235397115290169, -50.30295757539000334, -52.84913016542050457 ) ) ;
#50952 = CARTESIAN_POINT ( 'NONE',  ( 42.65512910241979938, 11.62675827516850013, -3.541891443476870016 ) ) ;
#50953 = CARTESIAN_POINT ( 'NONE',  ( 0.3209249304026170480, -23.01378514180129997, -34.64999999999999858 ) ) ;
#50954 = CARTESIAN_POINT ( 'NONE',  ( 66.97218591609239979, -45.11618894467940066, -13.04694144512030007 ) ) ;
#50955 = CARTESIAN_POINT ( 'NONE',  ( 59.41577471975829638, -46.21032088470760613, -47.36236646002819839 ) ) ;
#50956 = CARTESIAN_POINT ( 'NONE',  ( 16.13393739769620083, -15.61618894467929941, -22.64999999999999858 ) ) ;
#50957 = CARTESIAN_POINT ( 'NONE',  ( 31.58225770014188427, -28.80002732851970393, -65.65000000000000568 ) ) ;
#50958 = CARTESIAN_POINT ( 'NONE',  ( 18.50067234189449650, -52.01740915708810320, -75.38689171750549178 ) ) ;
#50959 = FACE_OUTER_BOUND ( 'NONE', #45403, .T. ) ;
#50960 = CARTESIAN_POINT ( 'NONE',  ( 17.49210479782680139, -8.290748640399698388, -68.62569607034470209 ) ) ;
#50961 = CARTESIAN_POINT ( 'NONE',  ( 63.86171360969409960, 1.406831506490820116, -61.68741386948379812 ) ) ;
#50962 = ORIENTED_EDGE ( 'NONE', *, *, #46923, .F. ) ;
#50963 = CARTESIAN_POINT ( 'NONE',  ( -3.470035664683920107, 18.86435654622399838, -8.135935225242089786 ) ) ;
#50964 = CARTESIAN_POINT ( 'NONE',  ( 22.90117443638819239, -15.61618876209028528, -62.84717844892357164 ) ) ;
#50965 = CARTESIAN_POINT ( 'NONE',  ( 72.85271889401160195, 1.383136297697689976, -68.56705292396610218 ) ) ;
#50966 = CIRCLE ( 'NONE', #2396, 15.29999999999999716 ) ;
#50967 = CARTESIAN_POINT ( 'NONE',  ( 9.366957987891332493, -14.73023998519778743, -73.49448688334868507 ) ) ;
#50968 = CIRCLE ( 'NONE', #45134, 12.50000000000000000 ) ;
#50969 = LINE ( 'NONE', #31034, #24249 ) ;
#50970 = CARTESIAN_POINT ( 'NONE',  ( 41.93137151579249888, -45.40097046374709322, -6.436558053594640505 ) ) ;
#50971 = EDGE_LOOP ( 'NONE', ( #28147, #27116, #10113, #10384 ) ) ;
#50972 = CARTESIAN_POINT ( 'NONE',  ( 17.21347160910339724, 21.88381105532300097, -76.14999999999999147 ) ) ;
#50973 = VERTEX_POINT ( 'NONE', #189 ) ;
#50974 = VERTEX_POINT ( 'NONE', #16168 ) ;
#50975 = CARTESIAN_POINT ( 'NONE',  ( 57.50723796702470025, -45.11618894467940066, -17.93019253464870033 ) ) ;
#50976 = CARTESIAN_POINT ( 'NONE',  ( 22.92703987217370099, -11.95345884179289975, -81.23899999999999011 ) ) ;
#50977 = CARTESIAN_POINT ( 'NONE',  ( 16.13393739769620083, -15.61618894467929941, -34.64999999999999858 ) ) ;
#50978 = CARTESIAN_POINT ( 'NONE',  ( -22.10349206065158612, -23.47247094433527792, -54.22342502566657174 ) ) ;
#50979 = ORIENTED_EDGE ( 'NONE', *, *, #30074, .F. ) ;
#50980 = DIRECTION ( 'NONE',  ( -8.592609827796581962E-15, 1.919972818367709724E-16, -1.000000000000000000 ) ) ;
#50981 = EDGE_LOOP ( 'NONE', ( #23923, #11299, #1176, #19189 ) ) ;
#50982 = CARTESIAN_POINT ( 'NONE',  ( 72.48038400710301232, 1.530257664727401545, -62.44999999999999574 ) ) ;
#50983 = ADVANCED_FACE ( 'NONE', ( #5170 ), #48937, .F. ) ;
#50984 = CARTESIAN_POINT ( 'NONE',  ( 45.30908585303109959, -33.79766069374939974, -34.65739582053399204 ) ) ;
#50985 = ORIENTED_EDGE ( 'NONE', *, *, #29390, .T. ) ;
#50986 = CARTESIAN_POINT ( 'NONE',  ( 44.79905630159557717, 1.958006841695987266, -42.17908975497248036 ) ) ;
#50987 = CARTESIAN_POINT ( 'NONE',  ( 52.69948128945090104, -51.21643021819709674, -75.94570035807549857 ) ) ;
#50988 = CIRCLE ( 'NONE', #35069, 22.00000000000000000 ) ;
#50989 = CARTESIAN_POINT ( 'NONE',  ( 60.99523858508910479, 14.17424510680999994, -47.17226579437169676 ) ) ;
#50990 = CARTESIAN_POINT ( 'NONE',  ( 19.61497263573680172, -40.47764751925419802, -35.14999999999999858 ) ) ;
#50991 = DIRECTION ( 'NONE',  ( 1.000000000000000000, 0.000000000000000000, 0.000000000000000000 ) ) ;
#50992 = CARTESIAN_POINT ( 'NONE',  ( 65.41765731850109944, -1.045745731241882526, -16.56748124947237244 ) ) ;
#50993 = CARTESIAN_POINT ( 'NONE',  ( -8.870889643038399441, 13.08137690754710114, -5.817308098515409753 ) ) ;
#50994 = EDGE_CURVE ( 'NONE', #23485, #6332, #1225, .T. ) ;
#50995 = AXIS2_PLACEMENT_3D ( 'NONE', #38555, #42225, #6325 ) ;
#50996 = CIRCLE ( 'NONE', #33397, 2.999999999999999112 ) ;
#50997 = CARTESIAN_POINT ( 'NONE',  ( 64.26031169644889474, 0.9860222121691910591, -70.23289684640710107 ) ) ;
#50998 = CARTESIAN_POINT ( 'NONE',  ( 16.13393739769620083, -15.61618894467929941, -12.65000000000000036 ) ) ;
#50999 = VECTOR ( 'NONE', #10730, 999.9999999999998863 ) ;
#51000 = AXIS2_PLACEMENT_3D ( 'NONE', #30761, #38912, #42847 ) ;
#51001 = CARTESIAN_POINT ( 'NONE',  ( 20.24515493355339757, -8.931531993418198923, -56.96301931345279712 ) ) ;
#51002 = ADVANCED_FACE ( 'NONE', ( #28208 ), #17214, .T. ) ;
#51003 = VERTEX_POINT ( 'NONE', #32643 ) ;
#51004 = CARTESIAN_POINT ( 'NONE',  ( 59.65718820948480783, 14.85145970413650041, -47.32570903220330649 ) ) ;
#51006 = CIRCLE ( 'NONE', #18374, 1.000000000000003109 ) ;
#51005 = CARTESIAN_POINT ( 'NONE',  ( 57.37145085794500687, 19.38381105532069881, -53.92454733977369585 ) ) ;
#51007 = UNCERTAINTY_MEASURE_WITH_UNIT (LENGTH_MEASURE( 1.000000000000000082E-05 ), #47775, 'distance_accuracy_value', 'NONE');
#51008 = EDGE_CURVE ( 'NONE', #34913, #6962, #41057, .T. ) ;
#51009 = CARTESIAN_POINT ( 'NONE',  ( 71.73794240842320846, 1.239065815390139935, -70.33274506191480668 ) ) ;
#51010 = CARTESIAN_POINT ( 'NONE',  ( 46.05101011062605920, -40.09655301607604372, -56.71146331062539758 ) ) ;
#51011 = FACE_OUTER_BOUND ( 'NONE', #22658, .T. ) ;
#51012 = CARTESIAN_POINT ( 'NONE',  ( 8.423931095146343750, -17.63235750399038082, -40.42643503837953745 ) ) ;
#51013 = CARTESIAN_POINT ( 'NONE',  ( 63.34508830662979761, 1.264689361399219836, -69.01667010504620237 ) ) ;
#51014 = CARTESIAN_POINT ( 'NONE',  ( 47.90035703882499973, -54.39486251246400172, -54.90987639013900434 ) ) ;
#51015 = CARTESIAN_POINT ( 'NONE',  ( 9.366376358913971245, -15.61615244833809868, -75.84717978381000592 ) ) ;
#51016 = DIRECTION ( 'NONE',  ( -0.5897727341282608116, 0.3900873262218075288, 0.7071067811865454633 ) ) ;
#51017 = CARTESIAN_POINT ( 'NONE',  ( 20.11804220191760351, -8.703649910996523076, -71.45898685654994154 ) ) ;
#51018 = ORIENTED_EDGE ( 'NONE', *, *, #3179, .F. ) ;
#51019 = CARTESIAN_POINT ( 'NONE',  ( 17.41854199065469899, -22.95488674316110078, -35.51218288575179827 ) ) ;
#51020 = ORIENTED_EDGE ( 'NONE', *, *, #15367, .T. ) ;
#51021 = CARTESIAN_POINT ( 'NONE',  ( 71.40428550048659417, 1.263903724274369811, -70.49199270151910923 ) ) ;
#51022 = CARTESIAN_POINT ( 'NONE',  ( 60.41625431243939914, -45.68614159457540325, -47.22708700711559970 ) ) ;
#51023 = CARTESIAN_POINT ( 'NONE',  ( 16.13393739769620083, -15.61618894467929941, -15.18999999999999950 ) ) ;
#51024 = CARTESIAN_POINT ( 'NONE',  ( 7.441840577107667443, 30.27300150430266967, -19.49871569355902423 ) ) ;
#51026 = DIRECTION ( 'NONE',  ( 0.000000000000000000, 0.000000000000000000, -1.000000000000000000 ) ) ;
#51025 = CARTESIAN_POINT ( 'NONE',  ( 84.44421879469800274, 12.09119879402660125, -47.46023938497990002 ) ) ;
#51027 = CARTESIAN_POINT ( 'NONE',  ( 9.366881967297588929, -15.61636073738300112, -79.84717978380999170 ) ) ;
#51028 = CARTESIAN_POINT ( 'NONE',  ( 8.428873746072833129, -17.68700077691279660, -42.42433505261755045 ) ) ;
#51029 = CARTESIAN_POINT ( 'NONE',  ( 0.1339373976962109913, -15.61618894467929941, -34.64999999999999858 ) ) ;
#51030 = ORIENTED_EDGE ( 'NONE', *, *, #40177, .F. ) ;
#51031 = DIRECTION ( 'NONE',  ( 0.000000000000000000, 0.000000000000000000, -1.000000000000000000 ) ) ;
#51032 = EDGE_LOOP ( 'NONE', ( #34102, #11798, #32353 ) ) ;
#51033 = VERTEX_POINT ( 'NONE', #16429 ) ;
#51034 = CARTESIAN_POINT ( 'NONE',  ( 0.3209249304026170480, -26.47788675693900018, -34.64999999999999858 ) ) ;
#51035 = VECTOR ( 'NONE', #22604, 1000.000000000000000 ) ;
#51036 = CARTESIAN_POINT ( 'NONE',  ( 18.20457692116078263, -7.911077539172547191, -39.37565924810114382 ) ) ;
#51037 = AXIS2_PLACEMENT_3D ( 'NONE', #44414, #48347, #8517 ) ;
#51038 = CARTESIAN_POINT ( 'NONE',  ( 76.43497123267530924, -23.65911996861112598, -12.94720032858890235 ) ) ;
#51039 = CARTESIAN_POINT ( 'NONE',  ( 8.815605888606221185, -63.28267529256429924, -46.67186389937329949 ) ) ;
#51040 = AXIS2_PLACEMENT_3D ( 'NONE', #33480, #29292, #17257 ) ;
#51041 = ORIENTED_EDGE ( 'NONE', *, *, #11247, .F. ) ;
#51042 = CIRCLE ( 'NONE', #35130, 49.07571608970690846 ) ;
#51043 = ORIENTED_EDGE ( 'NONE', *, *, #49422, .F. ) ;
#51044 = CARTESIAN_POINT ( 'NONE',  ( 51.65752907925210025, 21.59180590640109898, -54.64640228080400419 ) ) ;
#51045 = DIRECTION ( 'NONE',  ( -1.000000000000000000, 0.000000000000000000, 0.000000000000000000 ) ) ;
#51046 = CARTESIAN_POINT ( 'NONE',  ( 0.4047412638266219553, -8.844334399411719616, -35.14999999999999858 ) ) ;
#51047 = EDGE_CURVE ( 'NONE', #24198, #14157, #44469, .T. ) ;
#51048 = VECTOR ( 'NONE', #27496, 1000.000000000000000 ) ;
#51049 = CARTESIAN_POINT ( 'NONE',  ( 9.366956826296663152, -14.73024848268338438, -35.49448676863867291 ) ) ;
#51050 = CARTESIAN_POINT ( 'NONE',  ( 59.95447645319909924, -1.253371738758830123, -15.99147373105880021 ) ) ;
#51051 = CARTESIAN_POINT ( 'NONE',  ( 51.65858043925479848, -48.93466924497870707, -76.94737799441629988 ) ) ;
#51052 = LINE ( 'NONE', #35578, #10390 ) ;
#51053 = ORIENTED_EDGE ( 'NONE', *, *, #44488, .T. ) ;
#51054 = CARTESIAN_POINT ( 'NONE',  ( 63.03407832914049891, 0.8840451408750739093, -68.81103260973580404 ) ) ;
#51055 = CARTESIAN_POINT ( 'NONE',  ( 24.04493742333003325, -16.65172792896177967, -47.83400009015595344 ) ) ;
#51056 = CARTESIAN_POINT ( 'NONE',  ( 11.97538872468891391, -10.20477610388419265, -51.74448612926989455 ) ) ;
#51057 = DIRECTION ( 'NONE',  ( 0.000000000000000000, 0.000000000000000000, -1.000000000000000000 ) ) ;
#51058 = CARTESIAN_POINT ( 'NONE',  ( 23.63916941805720029, -17.90927418342020161, -40.10688088744169733 ) ) ;
#51059 = CARTESIAN_POINT ( 'NONE',  ( 13.64784227573900033, -51.18487036888380004, -22.24579103685289994 ) ) ;
#51060 = DIRECTION ( 'NONE',  ( 0.000000000000000000, -1.000000000000000000, 0.000000000000000000 ) ) ;
#51061 = CARTESIAN_POINT ( 'NONE',  ( 55.65694285038450317, 13.96926599109930045, -15.18560201429809986 ) ) ;
#51062 = CARTESIAN_POINT ( 'NONE',  ( 61.18408626113220805, -45.35865915913219482, -47.22189121640219867 ) ) ;
#51063 = CARTESIAN_POINT ( 'NONE',  ( 71.23851365796429036, 1.390208944942409985, -70.27002685503239832 ) ) ;
#51064 = EDGE_CURVE ( 'NONE', #12739, #18289, #24519, .T. ) ;
#51065 = CARTESIAN_POINT ( 'NONE',  ( 23.10043867740759893, -16.71637942556440137, -42.89703736520819888 ) ) ;
#51066 = CARTESIAN_POINT ( 'NONE',  ( 9.366918674202366901, -14.73052779765556686, -43.49448186140821093 ) ) ;
#51067 = ORIENTED_EDGE ( 'NONE', *, *, #37132, .F. ) ;
#51068 = FACE_OUTER_BOUND ( 'NONE', #2150, .T. ) ;
#51069 = CARTESIAN_POINT ( 'NONE',  ( 64.86043556304430524, 0.9234936569010840923, -60.62162712823549526 ) ) ;
#51070 = EDGE_CURVE ( 'NONE', #42105, #51177, #30961, .T. ) ;
#51071 = CARTESIAN_POINT ( 'NONE',  ( 42.67726216907190206, -45.92311385897509979, -7.341706899958339250 ) ) ;
#51072 = CARTESIAN_POINT ( 'NONE',  ( 54.74839138441483755, -47.94984410803592567, -26.69632610202470602 ) ) ;
#51073 = CONICAL_SURFACE ( 'NONE', #856, 1.587553672713209574, 1.249045772398249987 ) ;
#51074 = CARTESIAN_POINT ( 'NONE',  ( 66.37097987491060280, 13.88381105532070059, -12.87817958664409979 ) ) ;
#51075 = AXIS2_PLACEMENT_3D ( 'NONE', #27420, #27683, #12224 ) ;
#51076 = VECTOR ( 'NONE', #10259, 1000.000000000000000 ) ;
#51077 = CARTESIAN_POINT ( 'NONE',  ( 82.13853704237929776, 13.88381105532070059, -46.37203261889099792 ) ) ;
#51078 = CARTESIAN_POINT ( 'NONE',  ( 71.62484648860579739, 0.9098571636355720083, -70.52991329011129551 ) ) ;
#51080 = CARTESIAN_POINT ( 'NONE',  ( 47.13346488154629554, -38.11675101726400072, -54.63444359475949597 ) ) ;
#51079 = CARTESIAN_POINT ( 'NONE',  ( 47.51796364507180215, 23.14532756813578018, -75.00952367038003388 ) ) ;
#51081 = DIRECTION ( 'NONE',  ( 0.000000000000000000, 0.000000000000000000, 1.000000000000000000 ) ) ;
#51082 = CARTESIAN_POINT ( 'NONE',  ( 49.58793114173270311, 22.40222048251530040, -54.62161527680250117 ) ) ;
#51083 = ORIENTED_EDGE ( 'NONE', *, *, #20791, .F. ) ;
#51084 = CARTESIAN_POINT ( 'NONE',  ( 52.92152590114420718, -49.62269093325190283, -48.88490684695970145 ) ) ;
#51085 = VERTEX_POINT ( 'NONE', #4895 ) ;
#51086 = CARTESIAN_POINT ( 'NONE',  ( 47.12390138149789465, 6.751667908743102409, -54.63444595951939675 ) ) ;
#51087 = LINE ( 'NONE', #34830, #42823 ) ;
#51088 = CARTESIAN_POINT ( 'NONE',  ( 13.48683992790090080, 20.06883863126540035, -22.27491888996000213 ) ) ;
#51089 = DIRECTION ( 'NONE',  ( 0.000000000000000000, 0.000000000000000000, 1.000000000000000000 ) ) ;
#51090 = CARTESIAN_POINT ( 'NONE',  ( 22.55585100403209964, -18.53193658968969970, -52.58848421441379628 ) ) ;
#51091 = CARTESIAN_POINT ( 'NONE',  ( 53.05395538955789903, 18.35446051233180143, -49.07041595412979262 ) ) ;
#51092 = CARTESIAN_POINT ( 'NONE',  ( 55.97242077277940098, -45.56436908181329670, -16.74564425458379802 ) ) ;
#51093 = DIRECTION ( 'NONE',  ( 1.000000000000000000, 0.000000000000000000, 0.000000000000000000 ) ) ;
#51094 = EDGE_LOOP ( 'NONE', ( #48479, #474, #21907, #42219, #15398 ) ) ;
#51095 = CARTESIAN_POINT ( 'NONE',  ( 17.45659250951840136, -7.880729576396868552, -36.84141082329339412 ) ) ;
#51096 = ORIENTED_EDGE ( 'NONE', *, *, #51402, .T. ) ;
#51097 = CIRCLE ( 'NONE', #28483, 20.00000000000000355 ) ;
#51098 = FACE_OUTER_BOUND ( 'NONE', #25112, .T. ) ;
#51099 = CARTESIAN_POINT ( 'NONE',  ( 10.86442074884469911, 33.79593519927429668, -47.12165869429840370 ) ) ;
#51100 = CARTESIAN_POINT ( 'NONE',  ( 73.07509570698499601, 0.9325382164350239922, -62.24624853760359855 ) ) ;
#51101 = CARTESIAN_POINT ( 'NONE',  ( 20.11801055182510112, -22.52874690906305233, -40.12567795478347676 ) ) ;
#51102 = CARTESIAN_POINT ( 'NONE',  ( 52.70698372528335796, -49.76075902929102313, -48.81385732385554377 ) ) ;
#51103 = DIRECTION ( 'NONE',  ( -1.000000000000000000, 0.000000000000000000, 0.000000000000000000 ) ) ;
#51104 = CARTESIAN_POINT ( 'NONE',  ( 53.27996121806150143, -52.13308956689839846, -54.32024439625410395 ) ) ;
#51105 = ORIENTED_EDGE ( 'NONE', *, *, #2428, .F. ) ;
#51106 = CARTESIAN_POINT ( 'NONE',  ( 64.76726729265020310, 1.264689361399219836, -70.43884909106650127 ) ) ;
#51107 = CARTESIAN_POINT ( 'NONE',  ( 10.48585289546009847, -63.13039971493990521, -45.62882785086220139 ) ) ;
#51108 = EDGE_CURVE ( 'NONE', #14302, #48357, #30384, .T. ) ;
#51109 = CARTESIAN_POINT ( 'NONE',  ( 68.13393739769819035, 19.47158195952109594, -72.59354914830207406 ) ) ;
#51110 = VERTEX_POINT ( 'NONE', #26339 ) ;
#51111 = CARTESIAN_POINT ( 'NONE',  ( 22.83754687068412892, -19.96581757452138106, -43.97580730608837740 ) ) ;
#51112 = CARTESIAN_POINT ( 'NONE',  ( 57.24507234422829782, 19.38381439976799925, -53.91419826612269617 ) ) ;
#51113 = AXIS2_PLACEMENT_3D ( 'NONE', #13235, #13997, #29186 ) ;
#51114 = EDGE_CURVE ( 'NONE', #46452, #29692, #50216, .T. ) ;
#51115 = CARTESIAN_POINT ( 'NONE',  ( 23.94726892773138260, -14.25686971664534575, -49.45287839032192778 ) ) ;
#51116 = VECTOR ( 'NONE', #48767, 1000.000000000000000 ) ;
#51117 = ORIENTED_EDGE ( 'NONE', *, *, #34069, .F. ) ;
#51118 = ADVANCED_FACE ( 'NONE', ( #46031 ), #10904, .T. ) ;
#51119 = CARTESIAN_POINT ( 'NONE',  ( 12.14980481010722890, -22.52871145908785877, -36.17433415090009419 ) ) ;
#51120 = DIRECTION ( 'NONE',  ( 0.000000000000000000, 1.000000000000000000, 0.000000000000000000 ) ) ;
#51121 = AXIS2_PLACEMENT_3D ( 'NONE', #5925, #13027, #37372 ) ;
#51122 = CARTESIAN_POINT ( 'NONE',  ( 14.62116837088475485, 20.66383147155319122, -75.74021525116816633 ) ) ;
#51123 = LINE ( 'NONE', #38295, #11099 ) ;
#51124 = AXIS2_PLACEMENT_3D ( 'NONE', #2849, #18814, #34794 ) ;
#51125 = EDGE_CURVE ( 'NONE', #51719, #4886, #45559, .T. ) ;
#51126 = B_SPLINE_SURFACE_WITH_KNOTS ( 'NONE', 3, 3, ( 
 ( #1131, #37545, #44900, #5338, #9006, #37295, #1393, #17380, #1651, #49363, #13464, #17643, #33609, #14993, #46471, #30959, #26515, #31214, #46991, #23095, #11076, #18150, #46731, #10558 ),
 ( #22324, #2947, #11332, #39114, #6108, #14739, #42531, #6619, #18663, #27991, #38330, #38074, #26774, #22064, #50126, #38858, #15259, #42792, #22583, #6887, #47241, #42265, #27042, #26260 ),
 ( #3208, #38600, #22837, #2691, #50642, #18918, #34637, #6364, #2170, #35158, #19179, #43047, #2420, #30709, #34902, #7143, #14476, #18401, #34115, #14221, #46211, #10815, #30195, #50901 ),
 ( #10296, #51166, #34380, #50392, #30449, #17253, #1003, #9131, #48976, #4157, #32683, #32421, #36371, #24304, #28512, #44509, #1265, #8612, #24827, #12287, #24043, #28248, #13082, #40320 ),
 ( #12814, #13329, #36123, #40835, #33217, #28768, #24561, #44770, #49234, #44246, #17003, #8352, #4416, #12545, #40574, #45031, #40064, #43994, #16210, #4671, #16466, #4934, #20644, #25084 ),
 ( #20382, #36630, #8874, #41098, #48444, #732, #8100, #20131, #48183, #16728, #48710, #5209, #20906, #36903, #32950, #29035, #21162, #37168, #227, #9643, #9399, #13832, #34507, #34235 ),
 ( #2035, #10161, #50514, #22188, #14345, #50258, #49996, #6232, #41868, #41606, #30315, #21668, #14087, #6490, #41348, #25348, #29789, #46337, #38198, #29289, #26376, #2294, #38454, #42393 ),
 ( #49493, #45290, #29545, #25599, #18267, #33729, #5711, #33475, #10424, #22447, #2558, #5465, #21419, #37420, #49742, #30048, #1521, #17506, #13580, #45548, #37941, #37675, #1777, #17758 ) ),
 .UNSPECIFIED., .F., .F., .F.,
 ( 4, 1, 1, 1, 1, 4 ),
 ( 4, 2, 2, 2, 2, 2, 2, 2, 2, 2, 2, 4 ),
 ( -3.746466027699999873E-05, 0.2000000000000000111, 0.4000000000000000222, 0.5999999999999999778, 0.8000000000000000444, 1.000000000000000000 ),
 ( -3.746466027699999873E-05, 0.2627958365207210267, 0.8013173561513319276, 1.332723478065980016, 1.850236617094970004, 2.367749756123960214, 3.156999674831939995, 3.551624634185940099, 4.183024569152329342, 5.193264465098549998, 6.167115316339319975, 6.314004134380339472 ),
 .UNSPECIFIED. ) ;
#51127 = CARTESIAN_POINT ( 'NONE',  ( 20.21053605544689802, -22.78306158478949683, -64.12771089025820004 ) ) ;
#51128 = FACE_OUTER_BOUND ( 'NONE', #13755, .T. ) ;
#51129 = CARTESIAN_POINT ( 'NONE',  ( 61.28610861176739633, -45.23040055550220018, -46.37203261889099792 ) ) ;
#51130 = DIRECTION ( 'NONE',  ( 0.000000000000000000, 0.000000000000000000, 1.000000000000000000 ) ) ;
#51131 = VERTEX_POINT ( 'NONE', #49960 ) ;
#51132 = ORIENTED_EDGE ( 'NONE', *, *, #34990, .T. ) ;
#51133 = CARTESIAN_POINT ( 'NONE',  ( 14.63393739769630031, 0.9255523191757060175, -34.64999999999999858 ) ) ;
#51134 = CARTESIAN_POINT ( 'NONE',  ( 13.90228228614060058, -8.507995836145079593, -53.63582420878069001 ) ) ;
#51135 = CARTESIAN_POINT ( 'NONE',  ( 53.27382404857079479, -49.51603170232989726, -49.18478183594810105 ) ) ;
#51136 = CARTESIAN_POINT ( 'NONE',  ( 55.55365748065509734, 13.88381105532070059, -14.32025611302120005 ) ) ;
#51137 = CARTESIAN_POINT ( 'NONE',  ( 11.48393739769620048, -15.61618894467929941, -9.721247897589949005 ) ) ;
#51138 = FACE_OUTER_BOUND ( 'NONE', #4887, .T. ) ;
#51139 = CARTESIAN_POINT ( 'NONE',  ( 61.50409964636570237, 14.14168666559669951, -47.35437808293550432 ) ) ;
#51140 = EDGE_CURVE ( 'NONE', #45267, #23479, #50475, .T. ) ;
#51141 = CARTESIAN_POINT ( 'NONE',  ( 64.43393739769619799, 10.88381105532070059, -62.44999999999999574 ) ) ;
#51142 = CARTESIAN_POINT ( 'NONE',  ( 12.05049839503350029, 33.67281946323389263, -16.21910226667979771 ) ) ;
#51143 = CARTESIAN_POINT ( 'NONE',  ( 12.46522631496400102, -23.00017700672360021, -64.15444814970220477 ) ) ;
#51144 = CARTESIAN_POINT ( 'NONE',  ( 22.40560713194629727, -19.95407936107560332, -32.14999999999999858 ) ) ;
#51145 = CARTESIAN_POINT ( 'NONE',  ( 56.79309010641989630, -50.66781749968460247, -74.34195920670471480 ) ) ;
#51147 = CARTESIAN_POINT ( 'NONE',  ( 47.59368629830048292, 23.27965873589448620, -54.68140488027380997 ) ) ;
#51146 = CARTESIAN_POINT ( 'NONE',  ( -5.006796579080280196, 16.35122532122439765, -5.448334583328020564 ) ) ;
#51148 = DIRECTION ( 'NONE',  ( -0.000000000000000000, 1.000000000000000000, 0.000000000000000000 ) ) ;
#51149 = CARTESIAN_POINT ( 'NONE',  ( 20.13393739768839552, 24.18330853958629945, -74.14999999999999147 ) ) ;
#51150 = CARTESIAN_POINT ( 'NONE',  ( 11.01107138704560029, -65.03344997371249292, -17.34607880264680091 ) ) ;
#51151 = VERTEX_POINT ( 'NONE', #1484 ) ;
#51152 = CIRCLE ( 'NONE', #125, 134.7319120578750073 ) ;
#51153 = CARTESIAN_POINT ( 'NONE',  ( -2.623662900533460185, -48.66391853465049877, -4.296538300593259585 ) ) ;
#51154 = VECTOR ( 'NONE', #4557, 1000.000000000000000 ) ;
#51155 = CARTESIAN_POINT ( 'NONE',  ( 47.50821162171600065, 23.36490262398820050, -54.98790728447610121 ) ) ;
#51156 = EDGE_CURVE ( 'NONE', #43432, #42739, #17469, .T. ) ;
#51157 = CARTESIAN_POINT ( 'NONE',  ( 58.54073765571180132, -45.63607917995849306, -26.46024503793289995 ) ) ;
#51158 = CARTESIAN_POINT ( 'NONE',  ( 63.26785353957599511, 1.102139304147779830, -62.20100733290610151 ) ) ;
#51159 = CARTESIAN_POINT ( 'NONE',  ( 61.28260267805470107, 14.10897515434229987, -47.23932327355679917 ) ) ;
#51160 = CIRCLE ( 'NONE', #28538, 25.00000000000000355 ) ;
#51161 = CARTESIAN_POINT ( 'NONE',  ( 21.90359465038130082, -10.90261821839509970, -72.01461621554048520 ) ) ;
#51162 = CARTESIAN_POINT ( 'NONE',  ( 51.54546934566289451, 17.72378080735539996, -76.80150978094809489 ) ) ;
#51163 = CARTESIAN_POINT ( 'NONE',  ( 52.94089227972619938, 18.37031531951570074, -48.75998158604740240 ) ) ;
#51164 = CARTESIAN_POINT ( 'NONE',  ( 15.09843646001806761, -23.52719456774363138, -70.33399961199894790 ) ) ;
#51165 = DIRECTION ( 'NONE',  ( 0.000000000000000000, 0.000000000000000000, -1.000000000000000000 ) ) ;
#51166 = CARTESIAN_POINT ( 'NONE',  ( 52.71556636524050532, 18.49758259741449962, -28.08016480817499883 ) ) ;
#51167 = CARTESIAN_POINT ( 'NONE',  ( 13.05521822061487214, -49.46974233527257780, -34.79644660940672907 ) ) ;
#51168 = CARTESIAN_POINT ( 'NONE',  ( 57.24929578234380045, 19.38381105828390361, -53.91492796160409284 ) ) ;
#51169 = CYLINDRICAL_SURFACE ( 'NONE', #23681, 6.099999999999994316 ) ;
#51170 = DIRECTION ( 'NONE',  ( -0.3535533905932738974, 0.6123724356957941373, 0.7071067811865477948 ) ) ;
#51171 = CARTESIAN_POINT ( 'NONE',  ( 65.12655588804669549, -32.00338151092800132, -17.50916650718779977 ) ) ;
#51172 = CARTESIAN_POINT ( 'NONE',  ( 70.99050876911339003, 1.383811055320669947, -60.94999999999999574 ) ) ;
#51173 = CARTESIAN_POINT ( 'NONE',  ( 11.13393739769619906, 31.90680957093530168, -43.74348518090240390 ) ) ;
#51174 = CARTESIAN_POINT ( 'NONE',  ( 72.55639720057749287, 1.338417587229449923, -61.77627077996229588 ) ) ;
#51175 = DIRECTION ( 'NONE',  ( 1.430038757655089944E-15, 8.684364315601310195E-16, -1.000000000000000000 ) ) ;
#51176 = CARTESIAN_POINT ( 'NONE',  ( 60.29344216025802439, -45.37694481291970305, -27.03112392671941322 ) ) ;
#51177 = VERTEX_POINT ( 'NONE', #22149 ) ;
#51178 = VERTEX_POINT ( 'NONE', #6194 ) ;
#51179 = DIRECTION ( 'NONE',  ( 1.000000000000000000, 0.000000000000000000, 0.000000000000000000 ) ) ;
#51180 = CARTESIAN_POINT ( 'NONE',  ( 55.13393739769630031, -15.61618894467929941, -34.64999999999999858 ) ) ;
#51181 = ORIENTED_EDGE ( 'NONE', *, *, #19205, .F. ) ;
#51182 = CARTESIAN_POINT ( 'NONE',  ( 56.92872317984839725, -45.28411505133909998, -25.70904297234619662 ) ) ;
#51183 = CARTESIAN_POINT ( 'NONE',  ( 20.70919841900760261, -22.07818802934547264, -77.81157068189432380 ) ) ;
#51184 = EDGE_CURVE ( 'NONE', #30215, #14338, #17596, .T. ) ;
#51185 = VERTEX_POINT ( 'NONE', #25815 ) ;
#51186 = CARTESIAN_POINT ( 'NONE',  ( 10.83684432477319959, -19.82762902495380075, -81.23899999999999011 ) ) ;
#51187 = B_SPLINE_CURVE_WITH_KNOTS ( 'NONE', 3,
 ( #34376, #25993, #26255, #18397, #45938, #2687, #41736, #21545, #13965, #50638 ),
 .UNSPECIFIED., .F., .F.,
 ( 4, 1, 1, 1, 1, 1, 1, 4 ),
 ( 0.5000013100879009409, 0.5754136553612179128, 0.6546325864248377924, 0.7338515174884554515, 0.8130704485520910962, 0.8922893796157064239, 0.9715083106793263035, 1.000000000000000000 ),
 .UNSPECIFIED. ) ;
#51188 = CARTESIAN_POINT ( 'NONE',  ( 43.11472998706207704, 6.562511154101421162, -74.74601975373923324 ) ) ;
#51189 = CARTESIAN_POINT ( 'NONE',  ( 41.35567059317689598, -44.75886416236139809, -5.363894289339560473 ) ) ;
#51190 = ADVANCED_FACE ( 'NONE', ( #14307 ), #5933, .T. ) ;
#51191 = VERTEX_POINT ( 'NONE', #14050 ) ;
#51192 = CARTESIAN_POINT ( 'NONE',  ( 46.60731143751889505, -45.11618894467940066, -7.962942859665570694 ) ) ;
#51193 = CARTESIAN_POINT ( 'NONE',  ( 51.45118121745367290, 0.8518969343010126538, -17.60358367641750732 ) ) ;
#51194 = CARTESIAN_POINT ( 'NONE',  ( 24.04526736911255469, -15.61618908158827068, -41.79233198438217300 ) ) ;
#51195 = CARTESIAN_POINT ( 'NONE',  ( 64.73577143960351066, -30.09401345844290177, -16.46742189103860099 ) ) ;
#51196 = AXIS2_PLACEMENT_3D ( 'NONE', #27418, #36060, #47872 ) ;
#51197 = CARTESIAN_POINT ( 'NONE',  ( 22.90093737620393100, -14.73039356599736749, -64.41115567542702536 ) ) ;
#51198 = CARTESIAN_POINT ( 'NONE',  ( 47.24371072983239372, -54.76060195732999603, -74.14999999999999147 ) ) ;
#51199 = CARTESIAN_POINT ( 'NONE',  ( 8.290267814922380296, -15.86836957012680038, -71.00226400225328405 ) ) ;
#51200 = AXIS2_PLACEMENT_3D ( 'NONE', #28289, #44291, #40621 ) ;
#51201 = DIRECTION ( 'NONE',  ( 0.7071067811865475727, 0.000000000000000000, 0.7071067811865475727 ) ) ;
#51202 = VECTOR ( 'NONE', #28468, 1000.000000000000000 ) ;
#51203 = CARTESIAN_POINT ( 'NONE',  ( 44.26797775832170601, 14.17447024376930109, -7.721004194715090030 ) ) ;
#51204 = DIRECTION ( 'NONE',  ( -0.9987374001630935361, 0.000000000000000000, -0.05023550054956103100 ) ) ;
#51205 = CARTESIAN_POINT ( 'NONE',  ( 83.48374992014450413, -44.73979101690569848, -46.79909128427029685 ) ) ;
#51206 = CARTESIAN_POINT ( 'NONE',  ( 59.40674124460660721, 13.88381117262120057, -25.82779764205569961 ) ) ;
#51207 = CARTESIAN_POINT ( 'NONE',  ( 17.55559842845789831, -23.73786368710720041, -35.95250869105369418 ) ) ;
#51208 = ORIENTED_EDGE ( 'NONE', *, *, #6288, .F. ) ;
#51209 = CARTESIAN_POINT ( 'NONE',  ( 56.55524560877629625, -46.21195526465520231, -26.26695727885629950 ) ) ;
#51210 = CARTESIAN_POINT ( 'NONE',  ( 8.291970543062280541, -62.33611482735770437, -15.32312980843789951 ) ) ;
#51211 = CARTESIAN_POINT ( 'NONE',  ( 75.24914379931091446, -35.01601405374659493, -12.30266221336199983 ) ) ;
#51212 = B_SPLINE_CURVE_WITH_KNOTS ( 'NONE', 3,
 ( #19319, #35300, #27938, #15394, #27429, #11726, #8039, #7533, #19830, #23992 ),
 .UNSPECIFIED., .F., .F.,
 ( 4, 1, 1, 1, 1, 1, 1, 4 ),
 ( 0.4999964962326966522, 0.5260408281246501394, 0.6052597591882703520, 0.6844786902518882332, 0.7636976213155060034, 0.8429165523791239956, 0.9221354834427439862, 1.000000000000000000 ),
 .UNSPECIFIED. ) ;
#51213 = CARTESIAN_POINT ( 'NONE',  ( 75.11247970983615119, 13.77271509087269408, -14.67931599322431957 ) ) ;
#51214 = DIRECTION ( 'NONE',  ( 0.000000000000000000, -1.000000000000000000, 0.000000000000000000 ) ) ;
#51215 = CARTESIAN_POINT ( 'NONE',  ( -0.1295185695942999982, 0.6472670226113349523, 4.943674098299870145 ) ) ;
#51216 = CARTESIAN_POINT ( 'NONE',  ( 8.133937397696209715, -54.80802482921019703, -21.14999999999999858 ) ) ;
#51217 = ADVANCED_FACE ( 'NONE', ( #9359 ), #30011, .F. ) ;
#51218 = CARTESIAN_POINT ( 'NONE',  ( 82.48251884290169755, -45.34700424204849867, -47.31937152333360075 ) ) ;
#51219 = CARTESIAN_POINT ( 'NONE',  ( 57.55751162049190128, -50.61618894467939356, -53.92796738110899923 ) ) ;
#51220 = CARTESIAN_POINT ( 'NONE',  ( 41.41708261413649694, 13.08600793429160092, -4.679819212124120220 ) ) ;
#51221 = CARTESIAN_POINT ( 'NONE',  ( 0.5406133260286609676, 12.32747302715160131, -20.15000000000000213 ) ) ;
#51222 = CARTESIAN_POINT ( 'NONE',  ( 63.25402410758490390, 0.9098571636355720083, -62.15909090909049439 ) ) ;
#51223 = CARTESIAN_POINT ( 'NONE',  ( 55.55538329330519787, -48.25727492885060599, -48.41463972625499679 ) ) ;
#51224 = CARTESIAN_POINT ( 'NONE',  ( 14.55219295556159409, -51.70197612871098869, -75.56421430877743717 ) ) ;
#51225 = ADVANCED_FACE ( 'NONE', ( #49453 ), #822, .T. ) ;
#51226 = CARTESIAN_POINT ( 'NONE',  ( 66.66073096664889874, -1.315816564741499883, -17.00118905793410207 ) ) ;
#51227 = CARTESIAN_POINT ( 'NONE',  ( 17.74852555148360267, -51.60940715663139855, -75.47164421335219231 ) ) ;
#51228 = B_SPLINE_CURVE_WITH_KNOTS ( 'NONE', 3,
 ( #36484, #40427, #24675, #7706, #16324, #589, #40688, #32529, #3773, #28618, #19739, #36743, #4269, #12147, #28101, #850, #8208, #4521, #47792, #35732, #11898, #32796 ),
 .UNSPECIFIED., .F., .F.,
 ( 4, 2, 2, 2, 2, 2, 2, 1, 2, 2, 1, 4 ),
 ( 0.000000000000000000, 0.1311013905112042854, 0.1966520857668051792, 0.2294274333946048072, 0.2622027810224044075, 0.3933041715336068056, 0.4588548667892080601, 0.4916302144170072164, 0.4998240513239579075, 0.5039209697774372776, 0.5080178882309165367, 0.5244055620448262456 ),
 .UNSPECIFIED. ) ;
#51229 = CARTESIAN_POINT ( 'NONE',  ( 41.17242569490439763, -45.11618894467940066, -6.491241765574168987 ) ) ;
#51230 = EDGE_CURVE ( 'NONE', #38024, #13386, #20, .T. ) ;
#51231 = CARTESIAN_POINT ( 'NONE',  ( 17.01461248871479981, -8.218141518337640505, -62.60505730950960412 ) ) ;
#51232 = DIRECTION ( 'NONE',  ( 0.000000000000000000, 0.000000000000000000, 1.000000000000000000 ) ) ;
#51233 = DIRECTION ( 'NONE',  ( -1.000000000000000000, 0.000000000000000000, 0.000000000000000000 ) ) ;
#51234 = ORIENTED_EDGE ( 'NONE', *, *, #31496, .T. ) ;
#51235 = CARTESIAN_POINT ( 'NONE',  ( 22.20417850065088672, -53.99262654159362285, -34.79644414665607144 ) ) ;
#51236 = TOROIDAL_SURFACE ( 'NONE', #14403, 13.00000000000000000, 0.5000000000000000000 ) ;
#51237 = CARTESIAN_POINT ( 'NONE',  ( 22.87787853217752598, -16.19320691800228929, -34.47998061787313873 ) ) ;
#51238 = CARTESIAN_POINT ( 'NONE',  ( 73.06112045927889653, 1.270877794983130027, -68.75550371754310675 ) ) ;
#51239 = CARTESIAN_POINT ( 'NONE',  ( 45.27709827453856661, 8.817119440491692828, -60.46762888545257653 ) ) ;
#51240 = CARTESIAN_POINT ( 'NONE',  ( 9.157169031609750931, -13.44670018174929993, -81.23899999999999011 ) ) ;
#51241 = CARTESIAN_POINT ( 'NONE',  ( 40.85470386722510483, -45.35371597153389445, -5.792869590957399950 ) ) ;
#51242 = ORIENTED_EDGE ( 'NONE', *, *, #44975, .F. ) ;
#51243 = CARTESIAN_POINT ( 'NONE',  ( 17.77325585800819852, 21.34486587698399873, -76.03043890231919022 ) ) ;
#51244 = ORIENTED_EDGE ( 'NONE', *, *, #24047, .T. ) ;
#51245 = ORIENTED_EDGE ( 'NONE', *, *, #11648, .F. ) ;
#51246 = DIRECTION ( 'NONE',  ( 0.6975711590030510001, 0.7165155114351260401, 0.000000000000000000 ) ) ;
#51247 = LINE ( 'NONE', #31041, #3531 ) ;
#51248 = CARTESIAN_POINT ( 'NONE',  ( 17.41829529840355306, -14.68304830863572619, -11.23251175440650051 ) ) ;
#51249 = ORIENTED_EDGE ( 'NONE', *, *, #42050, .F. ) ;
#51250 = EDGE_CURVE ( 'NONE', #31048, #37975, #10458, .T. ) ;
#51251 = DIRECTION ( 'NONE',  ( -1.000000000000000000, -0.000000000000000000, -0.000000000000000000 ) ) ;
#51252 = EDGE_LOOP ( 'NONE', ( #1485, #23478, #10451, #44863, #28176 ) ) ;
#51253 = CARTESIAN_POINT ( 'NONE',  ( 23.83903661103793326, -13.54550828489940706, -63.70900020837209610 ) ) ;
#51254 = DIRECTION ( 'NONE',  ( 1.000000000000000000, 0.000000000000000000, 0.000000000000000000 ) ) ;
#51255 = VERTEX_POINT ( 'NONE', #35773 ) ;
#51256 = CARTESIAN_POINT ( 'NONE',  ( 72.83393739769620367, 1.383811055320669947, -62.79342862858290886 ) ) ;
#51257 = CARTESIAN_POINT ( 'NONE',  ( 52.75030668772299691, -51.36013153243110452, -75.83477191552309193 ) ) ;
#51258 = CARTESIAN_POINT ( 'NONE',  ( 60.38681717586829478, 14.58921176390859920, -47.68186590178469686 ) ) ;
#51259 = CARTESIAN_POINT ( 'NONE',  ( 72.18749078828946608, 11.23736444591397543, -68.84999999999999432 ) ) ;
#51260 = CARTESIAN_POINT ( 'NONE',  ( -10.87940544930430065, 11.11767143334649965, -6.276159589371210323 ) ) ;
#51261 = AXIS2_PLACEMENT_3D ( 'NONE', #43064, #39385, #15012 ) ;
#51262 = AXIS2_PLACEMENT_3D ( 'NONE', #13111, #29062, #13610 ) ;
#51263 = CARTESIAN_POINT ( 'NONE',  ( 46.80617081706476768, 22.71927041949727766, -75.82639806882809808 ) ) ;
#51264 = CARTESIAN_POINT ( 'NONE',  ( 22.90079931266048874, -15.61618915558698184, -42.84717230777439312 ) ) ;
#51265 = CARTESIAN_POINT ( 'NONE',  ( 14.58466807763749884, -7.922911830399110400, -48.72425048283629678 ) ) ;
#51266 = EDGE_LOOP ( 'NONE', ( #35028, #23179, #19197, #38678, #2918, #29168, #24722 ) ) ;
#51267 = CARTESIAN_POINT ( 'NONE',  ( 59.94414702407019746, 14.70111394113749981, -47.28272102067069937 ) ) ;
#51268 = CARTESIAN_POINT ( 'NONE',  ( 16.13393739769620083, -15.61618894467929941, -17.93019253464870033 ) ) ;
#51269 = CARTESIAN_POINT ( 'NONE',  ( 71.35671708621339349, 1.389801772588449946, -70.26683326709820676 ) ) ;
#51270 = CARTESIAN_POINT ( 'NONE',  ( 45.89732069378420931, -40.08804502263331671, -57.45677221337471252 ) ) ;
#51271 = CARTESIAN_POINT ( 'NONE',  ( 13.86889551668940079, 19.40587202548489998, -21.27403962367360180 ) ) ;
#51272 = DIRECTION ( 'NONE',  ( -0.7071067811865475727, 0.7071067811865475727, 0.000000000000000000 ) ) ;
#51273 = CARTESIAN_POINT ( 'NONE',  ( 8.327683877742938279, -17.09775678691067213, -32.44805707646908388 ) ) ;
#51274 = CARTESIAN_POINT ( 'NONE',  ( 61.44121465274793081, 14.11489996882993481, -47.30179314246718292 ) ) ;
#51275 = CARTESIAN_POINT ( 'NONE',  ( 48.76069114195910714, -54.05633143203520063, -55.20115406384710610 ) ) ;
#51276 = CARTESIAN_POINT ( 'NONE',  ( 24.01793456853353703, -14.94176252685236683, -45.48051509102815970 ) ) ;
#51277 = EDGE_CURVE ( 'NONE', #15326, #26727, #38518, .T. ) ;
#51278 = CARTESIAN_POINT ( 'NONE',  ( 9.205734167420699166, -27.61618894467930119, -24.14999999999999858 ) ) ;
#51279 = CARTESIAN_POINT ( 'NONE',  ( 47.68893187850459725, 23.28158913229470173, -55.10584722141680203 ) ) ;
#51280 = EDGE_CURVE ( 'NONE', #26468, #21433, #18405, .T. ) ;
#51281 = ORIENTED_EDGE ( 'NONE', *, *, #45663, .F. ) ;
#51282 = CARTESIAN_POINT ( 'NONE',  ( 23.41350660572370046, -17.20193020699759856, -33.13561495384320210 ) ) ;
#51283 = ORIENTED_EDGE ( 'NONE', *, *, #30360, .F. ) ;
#51284 = CARTESIAN_POINT ( 'NONE',  ( 71.61023385683570552, 1.007912009470880221, -70.53231455471861011 ) ) ;
#51285 = CARTESIAN_POINT ( 'NONE',  ( 23.83903775132751335, -17.68686396165632146, -57.59100091412105371 ) ) ;
#51286 = CARTESIAN_POINT ( 'NONE',  ( 60.52894022340500157, 14.10979985953984261, -27.14274995353532915 ) ) ;
#51287 = CARTESIAN_POINT ( 'NONE',  ( 82.78853260243879220, 13.78813726657122807, -46.36933949695569623 ) ) ;
#51289 = CARTESIAN_POINT ( 'NONE',  ( 46.25525774125583922, 2.762490711761015572, -44.64999999999999858 ) ) ;
#51288 = CARTESIAN_POINT ( 'NONE',  ( 83.76205119356160367, 13.76116822878180024, -47.48604701470450351 ) ) ;
#51290 = CARTESIAN_POINT ( 'NONE',  ( 47.13393739769619373, -39.28050807707779768, -53.76790129988369671 ) ) ;
#51291 = DIRECTION ( 'NONE',  ( 0.000000000000000000, 0.000000000000000000, 1.000000000000000000 ) ) ;
#51292 = LINE ( 'NONE', #43684, #26934 ) ;
#51293 = ORIENTED_EDGE ( 'NONE', *, *, #11247, .T. ) ;
#51294 = DIRECTION ( 'NONE',  ( 0.000000000000000000, 0.000000000000000000, 1.000000000000000000 ) ) ;
#51295 = ORIENTED_EDGE ( 'NONE', *, *, #35831, .F. ) ;
#51296 = VERTEX_POINT ( 'NONE', #14826 ) ;
#51297 = CARTESIAN_POINT ( 'NONE',  ( 73.38393739769610136, -15.61618894467929941, -84.94863984844540994 ) ) ;
#51298 = CARTESIAN_POINT ( 'NONE',  ( 37.88393739769619373, -41.76263555408612405, -34.79644660940672907 ) ) ;
#51299 = VECTOR ( 'NONE', #36204, 1000.000000000000000 ) ;
#51300 = CARTESIAN_POINT ( 'NONE',  ( 76.42687394393672662, -22.88878007474863452, -12.91230967307213007 ) ) ;
#51301 = CARTESIAN_POINT ( 'NONE',  ( 12.90826365979919998, -65.51213270651270193, -47.70124197908979369 ) ) ;
#51302 = AXIS2_PLACEMENT_3D ( 'NONE', #47082, #6723, #30797 ) ;
#51303 = ORIENTED_EDGE ( 'NONE', *, *, #1477, .F. ) ;
#51304 = VERTEX_POINT ( 'NONE', #15082 ) ;
#51305 = EDGE_CURVE ( 'NONE', #15377, #24229, #29280, .T. ) ;
#51306 = DIRECTION ( 'NONE',  ( -1.000000000000000000, 0.000000000000000000, 0.000000000000000000 ) ) ;
#51307 = CARTESIAN_POINT ( 'NONE',  ( 23.13393739769620083, -2.337132753317950229, -84.65000000000000568 ) ) ;
#51308 = CARTESIAN_POINT ( 'NONE',  ( 56.42320082141079496, -50.66862966398220181, -53.17468687661730797 ) ) ;
#51309 = CARTESIAN_POINT ( 'NONE',  ( 22.90059226164785500, -15.54233919852935664, -46.44935462124129799 ) ) ;
#51310 = EDGE_CURVE ( 'NONE', #42024, #48161, #15116, .T. ) ;
#51311 = CARTESIAN_POINT ( 'NONE',  ( 63.40479749674490506, -0.6709863343795420265, -16.43330761011030106 ) ) ;
#51312 = CARTESIAN_POINT ( 'NONE',  ( 52.22857431453279276, -49.81596975065740196, -77.10487740174859539 ) ) ;
#51313 = DIRECTION ( 'NONE',  ( 1.000000000000000000, 0.000000000000000000, 0.000000000000000000 ) ) ;
#51314 = VERTEX_POINT ( 'NONE', #47581 ) ;
#51315 = DIRECTION ( 'NONE',  ( 0.000000000000000000, 0.000000000000000000, 1.000000000000000000 ) ) ;
#51316 = CARTESIAN_POINT ( 'NONE',  ( 62.13393739769620083, -20.61618894467929763, -65.65000000000000568 ) ) ;
#51317 = CARTESIAN_POINT ( 'NONE',  ( 22.90066504558609850, -15.61618132107965984, -48.84717678326153845 ) ) ;
#51318 = FACE_OUTER_BOUND ( 'NONE', #4552, .T. ) ;
#51319 = CARTESIAN_POINT ( 'NONE',  ( 8.949779341734769744, -18.77445122298149727, -50.88065551209399473 ) ) ;
#51320 = CARTESIAN_POINT ( 'NONE',  ( 13.79563961991189913, -50.43795090918690249, -21.08562558917969909 ) ) ;
#51321 = VECTOR ( 'NONE', #41527, 1000.000000000000000 ) ;
#51322 = CARTESIAN_POINT ( 'NONE',  ( 57.21115044914409964, 19.38381105532069881, -74.41047019428449971 ) ) ;
#51323 = CARTESIAN_POINT ( 'NONE',  ( 22.66931125956381976, -13.27800589393286401, -64.73722150501926365 ) ) ;
#51324 = CARTESIAN_POINT ( 'NONE',  ( 56.95254701797419727, 13.89618346210419908, -16.49528551305159851 ) ) ;
#51325 = CARTESIAN_POINT ( 'NONE',  ( 22.37318698975099807, -53.60726374558549878, -34.64999999999999858 ) ) ;
#51326 = CARTESIAN_POINT ( 'NONE',  ( 56.70659705506859893, -50.55677919107559859, -53.10139024712660216 ) ) ;
#51327 = CARTESIAN_POINT ( 'NONE',  ( 23.15902141439090300, -14.99108596689769968, -50.81893047157019794 ) ) ;
#51328 = CARTESIAN_POINT ( 'NONE',  ( 22.90065123677362635, -15.61618748955864433, -66.45281999012681240 ) ) ;
#51329 = VERTEX_POINT ( 'NONE', #50727 ) ;
#51330 = CARTESIAN_POINT ( 'NONE',  ( 11.73319001777203674, -65.42240559785102505, -18.17421237900516573 ) ) ;
#51331 = CARTESIAN_POINT ( 'NONE',  ( 64.85305306408208992, 1.096036836948800053, -60.67470092284240479 ) ) ;
#51332 = CARTESIAN_POINT ( 'NONE',  ( 17.16955733179256782, -7.705199290335150053, -51.04933357283481143 ) ) ;
#51333 = CIRCLE ( 'NONE', #6971, 3.799999999999829736 ) ;
#51334 = FACE_OUTER_BOUND ( 'NONE', #44914, .T. ) ;
#51335 = AXIS2_PLACEMENT_3D ( 'NONE', #30591, #6772, #51045 ) ;
#51336 = CARTESIAN_POINT ( 'NONE',  ( 51.93064585340319894, 13.88381105532070059, -9.012777190992919074 ) ) ;
#51337 = CARTESIAN_POINT ( 'NONE',  ( 46.97184464991040187, -53.68621135916810516, -75.90842213619210099 ) ) ;
#51338 = CARTESIAN_POINT ( 'NONE',  ( 10.74148174184799842, 33.72025021587940330, -18.12706498523149889 ) ) ;
#51339 = CARTESIAN_POINT ( 'NONE',  ( 8.222930619450961487, -15.61639179890759976, -64.50766849176299900 ) ) ;
#51341 = CARTESIAN_POINT ( 'NONE',  ( 11.37984272568584565, 33.25260846225116751, -24.02068460187723531 ) ) ;
#51340 = DIRECTION ( 'NONE',  ( 0.3805321250008310008, 0.000000000000000000, -0.9247677015566404535 ) ) ;
#51342 = EDGE_CURVE ( 'NONE', #3035, #39880, #30532, .T. ) ;
#51343 = CARTESIAN_POINT ( 'NONE',  ( -9.957798083463760719, -43.31361333265569868, -6.454122150048999806 ) ) ;
#51344 = CARTESIAN_POINT ( 'NONE',  ( 49.50151222301030174, 22.34932762003050044, -54.38302206046260068 ) ) ;
#51345 = VERTEX_POINT ( 'NONE', #31051 ) ;
#51346 = CARTESIAN_POINT ( 'NONE',  ( 52.68730831268639747, -49.75855573695199752, -48.67468093701120324 ) ) ;
#51347 = ORIENTED_EDGE ( 'NONE', *, *, #46325, .T. ) ;
#51348 = CARTESIAN_POINT ( 'NONE',  ( 42.31734421635291454, 6.282516177144741754, -78.71114254000248422 ) ) ;
#51349 = DIRECTION ( 'NONE',  ( 0.000000000000000000, 0.000000000000000000, -1.000000000000000000 ) ) ;
#51350 = CARTESIAN_POINT ( 'NONE',  ( 13.79433266918769974, 20.04646218605449803, -22.92985858714899905 ) ) ;
#51351 = CARTESIAN_POINT ( 'NONE',  ( 52.25096198472439823, -49.77129323599559996, -77.19024164398209109 ) ) ;
#51352 = CARTESIAN_POINT ( 'NONE',  ( 19.93152537058130136, -9.673051365519301115, -58.13380938886719917 ) ) ;
#51353 = CARTESIAN_POINT ( 'NONE',  ( 52.57474326386780206, 18.61928770101469865, -48.47378032971769812 ) ) ;
#51354 = CARTESIAN_POINT ( 'NONE',  ( 55.91594474632509559, -45.90466738476499842, -17.78184253245080271 ) ) ;
#51355 = LINE ( 'NONE', #47434, #47416 ) ;
#51356 = AXIS2_PLACEMENT_3D ( 'NONE', #42391, #51232, #6488 ) ;
#51357 = ORIENTED_EDGE ( 'NONE', *, *, #30069, .T. ) ;
#51358 = CARTESIAN_POINT ( 'NONE',  ( 14.56124311489510070, -23.30471161656020129, -39.85173020371090047 ) ) ;
#51359 = VERTEX_POINT ( 'NONE', #42616 ) ;
#51360 = CARTESIAN_POINT ( 'NONE',  ( 11.55844482067919898, -65.17238045331160379, -16.94284742230230023 ) ) ;
#51361 = CARTESIAN_POINT ( 'NONE',  ( 11.86093866196219970, 34.13069104538590182, -47.45833196181009583 ) ) ;
#51362 = CARTESIAN_POINT ( 'NONE',  ( 73.08672326322148649, 0.8966068345641440285, -62.26318953425310099 ) ) ;
#51363 = CARTESIAN_POINT ( 'NONE',  ( 24.04465145034966156, -15.61618865458276595, -39.79233592887338489 ) ) ;
#51364 = DIRECTION ( 'NONE',  ( 0.000000000000000000, 1.000000000000000000, 0.000000000000000000 ) ) ;
#51365 = DIRECTION ( 'NONE',  ( 1.000000000000000000, 0.000000000000000000, 0.000000000000000000 ) ) ;
#51366 = EDGE_LOOP ( 'NONE', ( #25169, #35437, #17139, #17973, #24801 ) ) ;
#51367 = CARTESIAN_POINT ( 'NONE',  ( 64.93393739769599904, 1.396834109478120034, -70.23662692463440749 ) ) ;
#51368 = CARTESIAN_POINT ( 'NONE',  ( 11.13393739769619906, -63.30209769551670007, -43.74698219623469697 ) ) ;
#51369 = DIRECTION ( 'NONE',  ( 0.8732394366197182567, 0.4872913772396111343, 1.665334536937735304E-16 ) ) ;
#51370 = ORIENTED_EDGE ( 'NONE', *, *, #35822, .T. ) ;
#51371 = EDGE_CURVE ( 'NONE', #7528, #48439, #3290, .T. ) ;
#51372 = CARTESIAN_POINT ( 'NONE',  ( 9.031253978508082980, -19.22508473272204554, -44.64247938458763798 ) ) ;
#51373 = CARTESIAN_POINT ( 'NONE',  ( 15.85768616877558657, -7.688762805127981714, -76.99657294770088356 ) ) ;
#51374 = CARTESIAN_POINT ( 'NONE',  ( 31.25349618544100139, -15.61618894467929763, -6.721843382729280059 ) ) ;
#51375 = AXIS2_PLACEMENT_3D ( 'NONE', #2496, #46013, #38139 ) ;
#51376 = ORIENTED_EDGE ( 'NONE', *, *, #33157, .T. ) ;
#51377 = AXIS2_PLACEMENT_3D ( 'NONE', #36097, #40039, #4130 ) ;
#51378 = CARTESIAN_POINT ( 'NONE',  ( 8.222926353263792620, -16.65165556482179099, -62.75066471232383947 ) ) ;
#51379 = CYLINDRICAL_SURFACE ( 'NONE', #15015, 7.910999999999997812 ) ;
#51380 = CARTESIAN_POINT ( 'NONE',  ( 83.23750471064099088, -44.81947890601180262, -46.42261246043593559 ) ) ;
#51381 = DIRECTION ( 'NONE',  ( 1.000000000000000000, 0.000000000000000000, 0.000000000000000000 ) ) ;
#51382 = CARTESIAN_POINT ( 'NONE',  ( 8.992839782551710570, -11.49460612895030032, -60.95895364771349989 ) ) ;
#51383 = CARTESIAN_POINT ( 'NONE',  ( 53.53273701459760048, -33.11618894467940066, -56.74709961107230782 ) ) ;
#51384 = CARTESIAN_POINT ( 'NONE',  ( 22.90093739769620029, -15.61618894467913243, -28.45282021618999835 ) ) ;
#51385 = CARTESIAN_POINT ( 'NONE',  ( 0.000000000000000000, 0.000000000000000000, 0.000000000000000000 ) ) ;
#51386 = ORIENTED_EDGE ( 'NONE', *, *, #15557, .T. ) ;
#51387 = VERTEX_POINT ( 'NONE', #42875 ) ;
#51388 = CARTESIAN_POINT ( 'NONE',  ( 3.987490788289478783, -8.603434725040944642, -34.79644660940672907 ) ) ;
#51389 = CARTESIAN_POINT ( 'NONE',  ( 18.13401765809539867, -22.79298298917490229, -56.64614358919829584 ) ) ;
#51390 = CARTESIAN_POINT ( 'NONE',  ( 50.03007040746459921, -48.76509257287760590, -76.14999999999999147 ) ) ;
#51391 = DIRECTION ( 'NONE',  ( 0.000000000000000000, 0.000000000000000000, -1.000000000000000000 ) ) ;
#51392 = AXIS2_PLACEMENT_3D ( 'NONE', #11223, #12709, #19588 ) ;
#51393 = CARTESIAN_POINT ( 'NONE',  ( 46.35275103504439898, 21.67755452994670406, -76.14999999999999147 ) ) ;
#51394 = CARTESIAN_POINT ( 'NONE',  ( 41.64265090550279780, -46.42699119286230314, -4.296538310234280011 ) ) ;
#51395 = PLANE ( 'NONE',  #23846 ) ;
#51396 = CARTESIAN_POINT ( 'NONE',  ( 11.92234616937149916, 33.79182978746079868, -16.43998781664420150 ) ) ;
#51397 = CARTESIAN_POINT ( 'NONE',  ( 21.72942902755440286, -9.560349272993629910, -75.24509849860889688 ) ) ;
#51398 = CARTESIAN_POINT ( 'NONE',  ( 55.01074116390060453, -47.06068843752029807, -25.62222821926209804 ) ) ;
#51399 = CARTESIAN_POINT ( 'NONE',  ( 57.13447189169250606, -50.61839380715989734, -74.40093450475029613 ) ) ;
#51401 = CARTESIAN_POINT ( 'NONE',  ( 10.47385409520754784, -55.21366976880749888, -45.62050209441289894 ) ) ;
#51400 = CARTESIAN_POINT ( 'NONE',  ( -2.611054804631980364, 19.76244294662099676, -8.524286943195571453 ) ) ;
#51402 = EDGE_CURVE ( 'NONE', #36774, #46160, #49440, .T. ) ;
#51403 = AXIS2_PLACEMENT_3D ( 'NONE', #37300, #13722, #50132 ) ;
#51404 = CARTESIAN_POINT ( 'NONE',  ( 63.37726551317079782, 1.370937308141420230, -68.67294022748990301 ) ) ;
#51405 = CARTESIAN_POINT ( 'NONE',  ( -18.86606260230390220, 19.38381105532060289, 16.21999999999999886 ) ) ;
#51406 = B_SPLINE_CURVE_WITH_KNOTS ( 'NONE', 3,
 ( #26837, #43614, #34436, #2746, #7717, #18717 ),
 .UNSPECIFIED., .F., .F.,
 ( 4, 2, 4 ),
 ( 0.000000000000000000, 0.4606906889216966228, 1.000000000000000000 ),
 .UNSPECIFIED. ) ;
#51407 = DIRECTION ( 'NONE',  ( -8.660081000000000658E-17, -2.123755000000000144E-17, -1.000000000000000000 ) ) ;
#51408 = ADVANCED_FACE ( 'NONE', ( #19266 ), #7228, .T. ) ;
#51409 = ORIENTED_EDGE ( 'NONE', *, *, #38697, .T. ) ;
#51410 = CARTESIAN_POINT ( 'NONE',  ( 53.13650397927179370, -49.50020675881640386, -48.81774254784100009 ) ) ;
#51411 = EDGE_CURVE ( 'NONE', #45283, #35235, #43134, .T. ) ;
#51412 = CARTESIAN_POINT ( 'NONE',  ( 47.66026032047859928, 23.29152205301619816, -55.04550996317009748 ) ) ;
#51413 = CARTESIAN_POINT ( 'NONE',  ( 60.37605544241890243, -45.23483286569010176, -26.84318989901830221 ) ) ;
#51414 = CARTESIAN_POINT ( 'NONE',  ( 15.09829039507263992, -23.52717692012846129, -72.33402119296106036 ) ) ;
#51415 = CARTESIAN_POINT ( 'NONE',  ( 61.10200072402039240, 14.51600081101689987, -47.83148716568879877 ) ) ;
#51416 = CARTESIAN_POINT ( 'NONE',  ( 14.41409580431940185, -22.86524672475230346, -72.80680552617650392 ) ) ;
#51417 = EDGE_CURVE ( 'NONE', #12711, #33975, #28492, .T. ) ;
#51418 = CARTESIAN_POINT ( 'NONE',  ( 51.59666223323370104, 18.72863052202810152, -76.48753527057338886 ) ) ;
#51419 = CARTESIAN_POINT ( 'NONE',  ( 53.39565654316790244, 18.13205158027290054, -48.78219270784469330 ) ) ;
#51420 = CARTESIAN_POINT ( 'NONE',  ( 11.27230730455335461, -21.94239041139972457, -70.50066575608552455 ) ) ;
#51421 = CARTESIAN_POINT ( 'NONE',  ( -0.3118748401327328668, -45.36041153914962365, -35.03826966092410089 ) ) ;
#51422 = CARTESIAN_POINT ( 'NONE',  ( 50.84162296648852220, 4.268840990914108069, -76.32020521981469585 ) ) ;
#51423 = CARTESIAN_POINT ( 'NONE',  ( 16.15735268940072444, -23.52715647658576614, -62.00672901155839156 ) ) ;
#51424 = FACE_OUTER_BOUND ( 'NONE', #10897, .T. ) ;
#51425 = CARTESIAN_POINT ( 'NONE',  ( 8.222937397696199469, -15.61618894467929941, -32.14999999999999858 ) ) ;
#51426 = CARTESIAN_POINT ( 'NONE',  ( 59.04060495528540287, -28.42300215364210203, -15.65182665779249760 ) ) ;
#51427 = CARTESIAN_POINT ( 'NONE',  ( 71.20883305211729919, 1.369885150286779929, -60.91305399111080021 ) ) ;
#51428 = CARTESIAN_POINT ( 'NONE',  ( 11.13393739769619906, 31.92895765439750377, -43.91250086627189120 ) ) ;
#51429 = CARTESIAN_POINT ( 'NONE',  ( 72.31664968728070164, 1.060191324942699964, -61.34806069345289359 ) ) ;
#51430 = CARTESIAN_POINT ( 'NONE',  ( 41.61626771661330082, -36.11618894467930119, -82.23834840541459812 ) ) ;
#51431 = CARTESIAN_POINT ( 'NONE',  ( 22.90065123677362635, -15.61618748955864433, -66.45281999012681240 ) ) ;
#51432 = EDGE_LOOP ( 'NONE', ( #51852, #17765, #10632, #9109, #11518 ) ) ;
#51433 = VERTEX_POINT ( 'NONE', #15347 ) ;
#51434 = VECTOR ( 'NONE', #33047, 1000.000000000000000 ) ;
#51435 = DIRECTION ( 'NONE',  ( 0.000000000000000000, -1.784214116308896674E-11, -1.000000000000000000 ) ) ;
#51436 = CARTESIAN_POINT ( 'NONE',  ( 51.09505050758819777, 0.2955707463199704899, -16.99481687198596092 ) ) ;
#51437 = ORIENTED_EDGE ( 'NONE', *, *, #27186, .T. ) ;
#51438 = EDGE_CURVE ( 'NONE', #371, #47191, #21798, .T. ) ;
#51439 = CARTESIAN_POINT ( 'NONE',  ( 11.69948082737000128, -64.91643855301771282, -45.13443972449930186 ) ) ;
#51440 = CARTESIAN_POINT ( 'NONE',  ( 1.058369240368480124, -8.644356418428410294, -34.64999999999999858 ) ) ;
#51441 = VERTEX_POINT ( 'NONE', #43388 ) ;
#51442 = CARTESIAN_POINT ( 'NONE',  ( 22.88844470591842750, -16.50768533441256380, -80.49475390970813748 ) ) ;
#51443 = CARTESIAN_POINT ( 'NONE',  ( 42.66038805835393788, 6.494748731714828693, -77.01767951336998408 ) ) ;
#51444 = CARTESIAN_POINT ( 'NONE',  ( 11.46164187755220176, 33.11604602725170565, -24.23493799255319914 ) ) ;
#51445 = AXIS2_PLACEMENT_3D ( 'NONE', #31639, #30872, #39789 ) ;
#51446 = ORIENTED_EDGE ( 'NONE', *, *, #30870, .F. ) ;
#51447 = CARTESIAN_POINT ( 'NONE',  ( 16.12586798055579962, -7.371029459282210539, -35.29201998310079347 ) ) ;
#51448 = CARTESIAN_POINT ( 'NONE',  ( 17.16949817664738376, -23.52718704373073066, -67.96600030527693548 ) ) ;
#51449 = VECTOR ( 'NONE', #2465, 1000.000000000000000 ) ;
#51450 = CARTESIAN_POINT ( 'NONE',  ( 10.12088335912352477, -20.79866362218473341, -50.56593387224838665 ) ) ;
#51451 = CARTESIAN_POINT ( 'NONE',  ( 61.53134167473509564, -29.71365059239380102, -16.03273234134309888 ) ) ;
#51452 = CARTESIAN_POINT ( 'NONE',  ( 17.01976861749745140, -8.849193657844582006, -63.99448808445440307 ) ) ;
#51453 = CARTESIAN_POINT ( 'NONE',  ( 47.11382581093260313, -54.35277270616690259, -75.35700034530711378 ) ) ;
#51454 = CARTESIAN_POINT ( 'NONE',  ( 8.743127158028750401, -12.97750146928379955, -75.12164841756138856 ) ) ;
#51455 = CARTESIAN_POINT ( 'NONE',  ( 35.69765375167399668, -15.61618894467929941, 7.849999999999999645 ) ) ;
#51456 = ADVANCED_FACE ( 'NONE', ( #39458 ), #3555, .T. ) ;
#51457 = CARTESIAN_POINT ( 'NONE',  ( 45.32091059241599851, 14.34211425166129850, -8.659579894684350521 ) ) ;
#51458 = CARTESIAN_POINT ( 'NONE',  ( 15.05440318628110141, 21.88381105532300097, -76.14999999999999147 ) ) ;
#51459 = CARTESIAN_POINT ( 'NONE',  ( 83.75509190357360012, -44.57363762736590473, -46.98971415009500419 ) ) ;
#51460 = DIRECTION ( 'NONE',  ( 0.000000000000000000, 1.000000000000000000, 0.000000000000000000 ) ) ;
#51461 = CARTESIAN_POINT ( 'NONE',  ( 24.28204518499680020, -14.35481659857889980, -45.45878041868809305 ) ) ;
#51462 = VERTEX_POINT ( 'NONE', #24979 ) ;
#51463 = CARTESIAN_POINT ( 'NONE',  ( -2.623662905471100260, -48.66391853184789795, -4.296538310234220504 ) ) ;
#51464 = VECTOR ( 'NONE', #970, 1000.000000000000000 ) ;
#51465 = CARTESIAN_POINT ( 'NONE',  ( 15.45245043279190078, -50.80479114967339882, -20.50565891244549732 ) ) ;
#51466 = CARTESIAN_POINT ( 'NONE',  ( 75.89808373934218366, -34.96973134563179997, -12.58107089590020067 ) ) ;
#51467 = CARTESIAN_POINT ( 'NONE',  ( -18.86606260230360022, -50.61618894467959962, 11.34999999999999964 ) ) ;
#51468 = LINE ( 'NONE', #27598, #48264 ) ;
#51469 = CARTESIAN_POINT ( 'NONE',  ( 14.15276264669889983, 1.359379830875179884, -35.01387690002259490 ) ) ;
#51470 = CARTESIAN_POINT ( 'NONE',  ( 8.428868622292895907, -17.68698215233624893, -38.70899843570095555 ) ) ;
#51471 = CARTESIAN_POINT ( 'NONE',  ( 10.22109734872648978, -19.02430242310299136, -49.28615388261155772 ) ) ;
#51472 = CARTESIAN_POINT ( 'NONE',  ( 82.25187930537960312, -45.11682425727330070, -46.44925488524950197 ) ) ;
#51473 = CARTESIAN_POINT ( 'NONE',  ( 57.55751162049750036, -50.61618894467939356, -53.87300832422299379 ) ) ;
#51474 = CARTESIAN_POINT ( 'NONE',  ( 42.16594883133879534, 12.74031567877150017, -4.735301441621479590 ) ) ;
#51475 = ADVANCED_FACE ( 'NONE', ( #20279 ), #35200, .F. ) ;
#51476 = DIRECTION ( 'NONE',  ( 0.000000000000000000, -1.000000000000000000, 0.000000000000000000 ) ) ;
#51477 = DIRECTION ( 'NONE',  ( 0.000000000000000000, 0.000000000000000000, -1.000000000000000000 ) ) ;
#51478 = DIRECTION ( 'NONE',  ( 0.000000000000000000, 0.000000000000000000, 1.000000000000000000 ) ) ;
#51479 = CARTESIAN_POINT ( 'NONE',  ( 68.13393739769841773, -50.61618894467878960, -73.25000000000220268 ) ) ;
#51480 = CARTESIAN_POINT ( 'NONE',  ( 31.58225770014180256, -2.032350560840031406, -102.2016796975540274 ) ) ;
#51481 = CARTESIAN_POINT ( 'NONE',  ( 18.52893073613670083, -52.05919180694159820, -75.36996982820370761 ) ) ;
#51482 = CARTESIAN_POINT ( 'NONE',  ( 53.58981775341219844, -43.47668491205899954, -7.400685398707020468 ) ) ;
#51483 = CARTESIAN_POINT ( 'NONE',  ( 23.01915031812909973, -12.77004464428880048, -68.94257179459910390 ) ) ;
#51484 = CARTESIAN_POINT ( 'NONE',  ( 24.04490680206547992, -15.61618865440000192, -77.79233401716611240 ) ) ;
#51485 = FACE_OUTER_BOUND ( 'NONE', #12537, .T. ) ;
#51486 = ORIENTED_EDGE ( 'NONE', *, *, #26777, .F. ) ;
#51487 = CYLINDRICAL_SURFACE ( 'NONE', #20045, 1.999999999999997113 ) ;
#51488 = CARTESIAN_POINT ( 'NONE',  ( 22.89185590794151892, -15.97420724114682855, -34.46966105702839656 ) ) ;
#51489 = CARTESIAN_POINT ( 'NONE',  ( 73.16231026946078941, 0.9234936569010840923, -68.92350183465200075 ) ) ;
#51490 = CARTESIAN_POINT ( 'NONE',  ( 13.55743739769619971, -15.61618894467929941, -22.64999999999999858 ) ) ;
#51491 = CARTESIAN_POINT ( 'NONE',  ( 8.977138400209929259, -15.31030486894329989, -81.23899999999999011 ) ) ;
#51492 = EDGE_LOOP ( 'NONE', ( #12707, #20012, #8153, #18212 ) ) ;
#51493 = CARTESIAN_POINT ( 'NONE',  ( 18.27939235371979976, 20.97417580057950204, -75.67041253543310120 ) ) ;
#51494 = ORIENTED_EDGE ( 'NONE', *, *, #32990, .F. ) ;
#51495 = VERTEX_POINT ( 'NONE', #32576 ) ;
#51496 = EDGE_CURVE ( 'NONE', #29113, #7609, #49163, .T. ) ;
#51497 = CARTESIAN_POINT ( 'NONE',  ( -5.366062602303915519, -15.61618894467939889, -10.44999999999999929 ) ) ;
#51498 = CARTESIAN_POINT ( 'NONE',  ( 23.22105033138630148, -12.70121737134209994, -81.23899999999999011 ) ) ;
#51499 = CARTESIAN_POINT ( 'NONE',  ( 16.13393739769620083, -15.61618894467929941, -34.64999999999999858 ) ) ;
#51500 = CARTESIAN_POINT ( 'NONE',  ( 8.223251455316621161, -15.61600507739779786, -72.79233150823699816 ) ) ;
#51501 = ORIENTED_EDGE ( 'NONE', *, *, #34935, .F. ) ;
#51502 = CARTESIAN_POINT ( 'NONE',  ( 18.89412612953066883, -9.387266263190900517, -80.08542171964066370 ) ) ;
#51503 = VERTEX_POINT ( 'NONE', #32322 ) ;
#51504 = CARTESIAN_POINT ( 'NONE',  ( 82.13853704237929776, 14.40950277491920062, -47.72348187592560009 ) ) ;
#51505 = AXIS2_PLACEMENT_3D ( 'NONE', #39592, #3696, #28030 ) ;
#51506 = CARTESIAN_POINT ( 'NONE',  ( 17.92370450339669929, -52.11618894467930119, -76.14999999999999147 ) ) ;
#51507 = ORIENTED_EDGE ( 'NONE', *, *, #49923, .F. ) ;
#51508 = LINE ( 'NONE', #19010, #41762 ) ;
#51509 = CARTESIAN_POINT ( 'NONE',  ( 51.55044215929650164, -51.25128868776180013, -76.08578283986020097 ) ) ;
#51510 = CARTESIAN_POINT ( 'NONE',  ( 60.58512182557269909, 14.48389043468630000, -47.62866706370459724 ) ) ;
#51511 = EDGE_CURVE ( 'NONE', #34773, #16490, #381, .T. ) ;
#51512 = EDGE_CURVE ( 'NONE', #11148, #49525, #10073, .T. ) ;
#51513 = CARTESIAN_POINT ( 'NONE',  ( 0.3209249304026170480, -4.754491132419490285, -34.64999999999999858 ) ) ;
#51514 = CARTESIAN_POINT ( 'NONE',  ( 41.50224532540739375, -43.90848951166579894, -3.489448901339209819 ) ) ;
#51515 = EDGE_CURVE ( 'NONE', #14662, #8293, #12049, .T. ) ;
#51516 = CARTESIAN_POINT ( 'NONE',  ( -6.905748412548989634, 14.77189088641519987, -5.492407866796149563 ) ) ;
#51517 = FACE_OUTER_BOUND ( 'NONE', #29633, .T. ) ;
#51518 = CARTESIAN_POINT ( 'NONE',  ( 11.63393739769600010, 10.38381105532060111, -35.14999999999999858 ) ) ;
#51519 = CARTESIAN_POINT ( 'NONE',  ( 20.17788239820569984, -22.34175635687860151, -47.61518544794569863 ) ) ;
#51520 = VERTEX_POINT ( 'NONE', #44149 ) ;
#51521 = CARTESIAN_POINT ( 'NONE',  ( 55.00867404205050093, 17.28694651894000245, -48.28813249775050309 ) ) ;
#51522 = CARTESIAN_POINT ( 'NONE',  ( 43.61538151352439741, 14.80464860828879914, -8.020992654718998693 ) ) ;
#51523 = CARTESIAN_POINT ( 'NONE',  ( 71.44915456287860422, 1.368315088675810198, -70.30601703012600012 ) ) ;
#51524 = CARTESIAN_POINT ( 'NONE',  ( 43.92098005941133465, -39.94817122821439881, -67.04241095931078576 ) ) ;
#51525 = DIRECTION ( 'NONE',  ( 0.000000000000000000, 0.000000000000000000, 1.000000000000000000 ) ) ;
#51526 = EDGE_CURVE ( 'NONE', #50522, #22194, #24460, .T. ) ;
#51527 =( BOUNDED_CURVE ( )  B_SPLINE_CURVE ( 3, ( #11822, #24341, #7629, #23573 ),
 .UNSPECIFIED., .F., .T. ) 
 B_SPLINE_CURVE_WITH_KNOTS ( ( 4, 4 ),
 ( 1.570796326794885678, 2.356194490192327962 ),
 .UNSPECIFIED. ) 
 CURVE ( )  GEOMETRIC_REPRESENTATION_ITEM ( )  RATIONAL_B_SPLINE_CURVE ( ( 1.000000000000000000, 0.9492530216741918991, 0.9492530216741918991, 1.000000000000000000 ) ) 
 REPRESENTATION_ITEM ( '' )  );
#51528 = CARTESIAN_POINT ( 'NONE',  ( 68.13393739769620083, 19.38381105532069881, -67.99999999999998579 ) ) ;
#51529 = CARTESIAN_POINT ( 'NONE',  ( 22.90095859539430379, -15.61618916398383661, -38.45281773784812174 ) ) ;
#51530 = EDGE_CURVE ( 'NONE', #5719, #39196, #11744, .T. ) ;
#51531 = CARTESIAN_POINT ( 'NONE',  ( 63.54027722212589424, 1.395196698723390138, -68.83033655198650536 ) ) ;
#51532 = CARTESIAN_POINT ( 'NONE',  ( 48.51115049231150067, -54.01384098269380019, -54.58190071400479582 ) ) ;
#51533 = AXIS2_PLACEMENT_3D ( 'NONE', #12023, #39539, #3126 ) ;
#51534 = CARTESIAN_POINT ( 'NONE',  ( 23.93801254160047165, -14.27752776017385727, -45.45360011000054357 ) ) ;
#51535 = CARTESIAN_POINT ( 'NONE',  ( 64.26031169644889474, 0.9860222121691860631, -70.23289684640710107 ) ) ;
#51536 = CARTESIAN_POINT ( 'NONE',  ( 47.75491787206179595, 23.24500768174080179, -55.00204154977200233 ) ) ;
#51537 = ORIENTED_EDGE ( 'NONE', *, *, #32218, .T. ) ;
#51538 = CARTESIAN_POINT ( 'NONE',  ( 19.59748479214910333, -22.21244043963609727, -37.41343723127859278 ) ) ;
#51539 = FACE_OUTER_BOUND ( 'NONE', #25885, .T. ) ;
#51540 = EDGE_LOOP ( 'NONE', ( #99, #8259 ) ) ;
#51541 = CARTESIAN_POINT ( 'NONE',  ( 71.31398829338289147, 1.388313565858570131, -70.27734465158499688 ) ) ;
#51542 = CARTESIAN_POINT ( 'NONE',  ( 60.63631542821100595, -45.63186250400350019, -47.47615296169890087 ) ) ;
#51543 = CARTESIAN_POINT ( 'NONE',  ( 48.21566362429802410, -54.17964390236606675, -54.67775470772499347 ) ) ;
#51544 = CARTESIAN_POINT ( 'NONE',  ( 9.366428224829499882, -15.61611423639980067, -77.45282021618989177 ) ) ;
#51545 = CARTESIAN_POINT ( 'NONE',  ( 9.367832377137357724, -14.89726563169283935, -57.88099794497199468 ) ) ;
#51546 = CARTESIAN_POINT ( 'NONE',  ( 74.17629866868290378, -43.11618894467930119, -65.34607522167520699 ) ) ;
#51547 = DIRECTION ( 'NONE',  ( 0.000000000000000000, 1.000000000000000000, 0.000000000000000000 ) ) ;
#51548 = EDGE_LOOP ( 'NONE', ( #13665, #36929, #10264, #17486, #19374, #51437, #5994, #50669, #28272, #34042 ) ) ;
#51549 = CARTESIAN_POINT ( 'NONE',  ( 23.13393739769620083, -28.89524513604070322, -84.65000000000000568 ) ) ;
#51550 = VERTEX_POINT ( 'NONE', #27891 ) ;
#51551 = PLANE ( 'NONE',  #20258 ) ;
#51552 = CARTESIAN_POINT ( 'NONE',  ( 7.517033938252880354, -61.58399597082019739, -19.14999999999999858 ) ) ;
#51553 = CARTESIAN_POINT ( 'NONE',  ( 9.367167526866026606, -15.17380814805779821, -61.86798012936559132 ) ) ;
#51554 = CARTESIAN_POINT ( 'NONE',  ( 9.286360118224829208, -63.91023846612779380, -46.69215455456279784 ) ) ;
#51555 = EDGE_LOOP ( 'NONE', ( #50018, #17568, #10826, #18689, #22562, #8442, #19956 ) ) ;
#51556 = DIRECTION ( 'NONE',  ( 0.000000000000000000, 0.000000000000000000, -1.000000000000000000 ) ) ;
#51557 = CIRCLE ( 'NONE', #49885, 24.00000000000000000 ) ;
#51558 = CARTESIAN_POINT ( 'NONE',  ( 22.41898323842375262, -18.19086658339881524, -32.97087606503488644 ) ) ;
#51559 = CARTESIAN_POINT ( 'NONE',  ( 56.48879402914270287, -50.71168639969660319, -53.39119800914449598 ) ) ;
#51560 = CARTESIAN_POINT ( 'NONE',  ( 17.16857899493826523, -8.907709375196542823, -46.00150713458933183 ) ) ;
#51561 = CARTESIAN_POINT ( 'NONE',  ( 61.99554605869259660, -0.5193312204098330387, -16.39842119712499979 ) ) ;
#51562 = CARTESIAN_POINT ( 'NONE',  ( 51.63757889171279913, -49.63238467538800336, -76.65049610660180690 ) ) ;
#51563 = LINE ( 'NONE', #40734, #39681 ) ;
#51564 = ORIENTED_EDGE ( 'NONE', *, *, #29438, .F. ) ;
#51565 = CARTESIAN_POINT ( 'NONE',  ( 63.13228119804391270, 0.8904513541338869853, -68.96413986139360475 ) ) ;
#51566 = CYLINDRICAL_SURFACE ( 'NONE', #23393, 1.999999999999997113 ) ;
#51567 = CARTESIAN_POINT ( 'NONE',  ( 65.01767771978660448, 0.8838110553206759423, -70.77727272727270247 ) ) ;
#51568 = DIRECTION ( 'NONE',  ( 0.000000000000000000, 0.000000000000000000, 1.000000000000000000 ) ) ;
#51569 = CIRCLE ( 'NONE', #5525, 2.500000000000000444 ) ;
#51570 = CARTESIAN_POINT ( 'NONE',  ( 11.60978911814099845, -9.203792361795480659, -55.31691565165669289 ) ) ;
#51571 = VECTOR ( 'NONE', #44382, 1000.000000000000000 ) ;
#51572 = EDGE_CURVE ( 'NONE', #1811, #24006, #44665, .T. ) ;
#51573 = CARTESIAN_POINT ( 'NONE',  ( 13.18306315670809958, -50.33123850494190066, -21.16866690708240029 ) ) ;
#51574 = CARTESIAN_POINT ( 'NONE',  ( 55.84450736765219858, 19.38381105532069881, -76.10951658791620389 ) ) ;
#51575 = DIRECTION ( 'NONE',  ( -0.05023550054956202326, 0.000000000000000000, -0.9987374001630934250 ) ) ;
#51576 = EDGE_CURVE ( 'NONE', #483, #13261, #27881, .T. ) ;
#51577 = CARTESIAN_POINT ( 'NONE',  ( 65.43042069957887463, -49.21324915460706961, -70.54648330188271643 ) ) ;
#51578 = CARTESIAN_POINT ( 'NONE',  ( 61.00628429235199945, -45.37700835658660736, -46.89453324795130129 ) ) ;
#51579 = DIRECTION ( 'NONE',  ( 0.000000000000000000, -0.7071067811865492381, 0.7071067811865457964 ) ) ;
#51580 = CARTESIAN_POINT ( 'NONE',  ( 21.12773481075129922, -20.59660524975009821, -55.09675274900569519 ) ) ;
#51581 = CARTESIAN_POINT ( 'NONE',  ( -13.39236625349559873, -30.35380722911099838, -54.64999999999999858 ) ) ;
#51582 = VERTEX_POINT ( 'NONE', #8245 ) ;
#51583 = CARTESIAN_POINT ( 'NONE',  ( 11.89321892217540011, -65.43602743108330344, -18.17421237901570308 ) ) ;
#51584 = CARTESIAN_POINT ( 'NONE',  ( 64.88733809717980705, 1.187415670095769871, -60.71585052632950408 ) ) ;
#51585 = CARTESIAN_POINT ( 'NONE',  ( 8.222958075229072961, -14.58049008954063730, -50.54933503646082471 ) ) ;
#51586 = LINE ( 'NONE', #24026, #17135 ) ;
#51587 = CARTESIAN_POINT ( 'NONE',  ( 24.04523214473702097, -15.61618869705131729, -47.50766735973101618 ) ) ;
#51588 = VECTOR ( 'NONE', #25197, 1000.000000000000000 ) ;
#51589 = LINE ( 'NONE', #47662, #20536 ) ;
#51590 = EDGE_CURVE ( 'NONE', #47254, #8577, #11763, .T. ) ;
#51591 = CIRCLE ( 'NONE', #32293, 2.999999999999994227 ) ;
#51592 = CARTESIAN_POINT ( 'NONE',  ( 11.13393739770549828, 31.88334419040860013, -48.70288603379470516 ) ) ;
#51593 = CARTESIAN_POINT ( 'NONE',  ( 69.63393739769620083, -38.11618894467930119, -73.25000000000000000 ) ) ;
#51595 = CARTESIAN_POINT ( 'NONE',  ( 8.222960500461509170, -16.65190554600032158, -58.75066482977644000 ) ) ;
#51594 = CYLINDRICAL_SURFACE ( 'NONE', #492, 6.766999999999998572 ) ;
#51596 = EDGE_CURVE ( 'NONE', #40337, #45245, #4224, .T. ) ;
#51597 = DIRECTION ( 'NONE',  ( 0.000000000000000000, -0.7071067811865466846, -0.7071067811865483499 ) ) ;
#51598 = CARTESIAN_POINT ( 'NONE',  ( 49.33374094960719702, 22.48211379487710104, -54.59177036145960216 ) ) ;
#51599 = VERTEX_POINT ( 'NONE', #48605 ) ;
#51600 = CARTESIAN_POINT ( 'NONE',  ( 52.66298673388549645, -49.77964374310990081, -48.68532682492069341 ) ) ;
#51601 = EDGE_LOOP ( 'NONE', ( #23998, #21186, #22977, #20973, #43231, #24906, #8814, #11010, #20226, #46666 ) ) ;
#51602 = CARTESIAN_POINT ( 'NONE',  ( 46.88244175870809727, 6.730884966597995955, -55.84197583295708256 ) ) ;
#51603 = CIRCLE ( 'NONE', #42408, 0.4999999999999995559 ) ;
#51604 = CARTESIAN_POINT ( 'NONE',  ( 9.083937397696097094, -15.61618894467929941, -20.75000000000000711 ) ) ;
#51605 = DIRECTION ( 'NONE',  ( 0.000000000000000000, 0.000000000000000000, 1.000000000000000000 ) ) ;
#51606 = CARTESIAN_POINT ( 'NONE',  ( 84.37071767335301331, 12.21453624936390092, -47.23470317516540007 ) ) ;
#51607 = CARTESIAN_POINT ( 'NONE',  ( 22.35343623859719742, -18.94190583952410023, -58.60912297524879477 ) ) ;
#51608 = DIRECTION ( 'NONE',  ( 0.000000000000000000, 0.000000000000000000, 1.000000000000000000 ) ) ;
#51609 = CARTESIAN_POINT ( 'NONE',  ( 57.12685297953459695, -45.12805850059309876, -16.97874220678049895 ) ) ;
#51610 = CARTESIAN_POINT ( 'NONE',  ( 11.13393739769619906, -63.52234720672429802, -24.14942632405960055 ) ) ;
#51611 = VECTOR ( 'NONE', #43783, 1000.000000000000000 ) ;
#51612 = VERTEX_POINT ( 'NONE', #28662 ) ;
#51613 = CARTESIAN_POINT ( 'NONE',  ( 8.664468393074560737, -13.20916153058959885, -42.38673599774679701 ) ) ;
#51614 = ORIENTED_EDGE ( 'NONE', *, *, #29950, .F. ) ;
#51615 = CARTESIAN_POINT ( 'NONE',  ( 11.79333632018079925, -65.42240134614850433, -17.82631581233690099 ) ) ;
#51616 = CARTESIAN_POINT ( 'NONE',  ( 10.32625535581710174, 32.28964825586200504, -45.85549233471310515 ) ) ;
#51617 = CARTESIAN_POINT ( 'NONE',  ( 73.03096648148358838, 1.005545696829380109, -62.19455336271669665 ) ) ;
#51618 = CARTESIAN_POINT ( 'NONE',  ( 23.83903199042086740, -17.68689264766797464, -39.87567244413330769 ) ) ;
#51619 = CARTESIAN_POINT ( 'NONE',  ( 8.804713206766638933, 31.98843531701869836, -46.67024040703379484 ) ) ;
#51620 = CARTESIAN_POINT ( 'NONE',  ( -13.73674066540309902, -30.55263188852779876, -46.71145918530379504 ) ) ;
#51621 = VERTEX_POINT ( 'NONE', #16623 ) ;
#51622 = CARTESIAN_POINT ( 'NONE',  ( 64.93408011569840710, 1.389468113695450091, -70.26995969721839685 ) ) ;
#51623 = CARTESIAN_POINT ( 'NONE',  ( 11.13393739769619906, -63.38752784187269640, -43.91920917233640154 ) ) ;
#51624 = AXIS2_PLACEMENT_3D ( 'NONE', #11639, #43859, #42842 ) ;
#51625 = CARTESIAN_POINT ( 'NONE',  ( 68.13393739769819035, 19.47158195952109594, -72.59354914830207406 ) ) ;
#51626 = ORIENTED_EDGE ( 'NONE', *, *, #41038, .F. ) ;
#51627 = CARTESIAN_POINT ( 'NONE',  ( 68.23750916396743094, -31.42880183748190959, -18.38207368453976187 ) ) ;
#51628 = CARTESIAN_POINT ( 'NONE',  ( 56.76664444808910304, 19.44233945464709734, -53.84360320718689508 ) ) ;
#51629 = CARTESIAN_POINT ( 'NONE',  ( 52.27433152305400199, 18.55914638219779889, -77.19764549399749853 ) ) ;
#51630 = ORIENTED_EDGE ( 'NONE', *, *, #6630, .F. ) ;
#51631 = CARTESIAN_POINT ( 'NONE',  ( 24.04493740548085867, -16.65173988180983855, -61.83399520223390056 ) ) ;
#51632 = CARTESIAN_POINT ( 'NONE',  ( 51.55044211529342135, 20.01891078301827775, -76.08578284841361494 ) ) ;
#51634 = FACE_OUTER_BOUND ( 'NONE', #47195, .T. ) ;
#51633 = AXIS2_PLACEMENT_3D ( 'NONE', #34161, #10862, #46519 ) ;
#51635 = CARTESIAN_POINT ( 'NONE',  ( 57.88659593186079633, 17.67030499234060059, -51.07754743084770155 ) ) ;
#51636 = CARTESIAN_POINT ( 'NONE',  ( 7.987404321646320859, -16.88769155842430081, -74.74304765278330365 ) ) ;
#51637 = EDGE_CURVE ( 'NONE', #9653, #41755, #20023, .T. ) ;
#51638 = DIRECTION ( 'NONE',  ( 0.000000000000000000, 0.000000000000000000, 1.000000000000000000 ) ) ;
#51639 = CARTESIAN_POINT ( 'NONE',  ( -0.3016046179078940015, -10.91500322974829906, -35.02873218748179340 ) ) ;
#51640 = ITEM_DEFINED_TRANSFORMATION ( 'NONE', 'NONE', #41945,  #20940 ) ;
#51641 = VERTEX_POINT ( 'NONE', #12710 ) ;
#51642 = ORIENTED_EDGE ( 'NONE', *, *, #27500, .T. ) ;
#51643 = CARTESIAN_POINT ( 'NONE',  ( 8.983156071820218358, -17.70736570302589996, -63.14209593641499652 ) ) ;
#51644 = CARTESIAN_POINT ( 'NONE',  ( 53.02879415315700129, -49.61082998701090219, -49.09627670324169202 ) ) ;
#51645 = CIRCLE ( 'NONE', #34872, 6.999999999999999112 ) ;
#51646 = CARTESIAN_POINT ( 'NONE',  ( -0.007164427059776000244, -8.408015226406421405, -34.77269723891829756 ) ) ;
#51647 = CARTESIAN_POINT ( 'NONE',  ( 10.58587177825300074, -20.98084142191969903, -32.14999999999999858 ) ) ;
#51648 = CARTESIAN_POINT ( 'NONE',  ( 47.18785506009880493, 23.26044294672620083, -75.11690455987650239 ) ) ;
#51649 = DIRECTION ( 'NONE',  ( 0.3294064756441309472, 0.9441882088883087887, 3.053113317719179500E-16 ) ) ;
#51650 = CARTESIAN_POINT ( 'NONE',  ( 9.895190454275772041, 22.37603658786960281, -34.64999999999999858 ) ) ;
#51651 = CARTESIAN_POINT ( 'NONE',  ( 12.04145588158159974, 33.83966319556200375, -16.48289738545560112 ) ) ;
#51652 = CARTESIAN_POINT ( 'NONE',  ( 23.85596303094300197, -18.50635171318529970, -77.62166643051759252 ) ) ;
#51653 = EDGE_CURVE ( 'NONE', #39898, #26913, #44139, .T. ) ;
#51654 = CARTESIAN_POINT ( 'NONE',  ( 52.61990787174079998, -49.80354421666699949, -27.74322489265380298 ) ) ;
#51655 = CARTESIAN_POINT ( 'NONE',  ( 56.50763749952780302, -50.63556182365589819, -75.24339335911510318 ) ) ;
#51657 = DIRECTION ( 'NONE',  ( 0.000000000000000000, 0.000000000000000000, -1.000000000000000000 ) ) ;
#51656 = CARTESIAN_POINT ( 'NONE',  ( 1.322326434189930122, 22.25801372082519691, -7.691437081604280301 ) ) ;
#51658 = B_SPLINE_CURVE_WITH_KNOTS ( 'NONE', 3,
 ( #20154, #50145, #47010, #11096, #24846, #4437, #41369, #36391, #32440, #29055, #40593, #48466, #40343, #41116, #5230, #37188 ),
 .UNSPECIFIED., .F., .F.,
 ( 4, 2, 2, 2, 2, 2, 2, 4 ),
 ( -8.326672999999999728E-16, 0.07319275283556599121, 0.1391693187718509861, 0.1804046724820289882, 0.2061767685508900105, 0.2577209606886129989, 0.3401916681089700023, 0.4123535371017769680 ),
 .UNSPECIFIED. ) ;
#51660 = EDGE_CURVE ( 'NONE', #1081, #47211, #14158, .T. ) ;
#51659 = CARTESIAN_POINT ( 'NONE',  ( 63.10556452593170462, 0.9234936569010840923, -68.92350183465200075 ) ) ;
#51661 = CARTESIAN_POINT ( 'NONE',  ( 61.28671122457539866, 13.99937605583419931, -46.63577450329929519 ) ) ;
#51662 = FACE_OUTER_BOUND ( 'NONE', #38868, .T. ) ;
#51663 = VERTEX_POINT ( 'NONE', #14253 ) ;
#51664 = CARTESIAN_POINT ( 'NONE',  ( 53.20760851556250515, -49.46295310004039436, -48.79936141346989587 ) ) ;
#51665 = CARTESIAN_POINT ( 'NONE',  ( 59.87633579703659592, -45.40677854013640058, -26.81043307918650243 ) ) ;
#51666 = CARTESIAN_POINT ( 'NONE',  ( 11.34449012104014898, -21.94230794375442883, -66.49862320159839157 ) ) ;
#51667 = CARTESIAN_POINT ( 'NONE',  ( 61.30642482279199612, 14.15530932967999966, -47.35784862597040501 ) ) ;
#51668 = CARTESIAN_POINT ( 'NONE',  ( 20.92368333918920342, -9.909611369538689374, -69.95492400788640452 ) ) ;
#51669 = CARTESIAN_POINT ( 'NONE',  ( 52.11523513670289276, 18.63129512089459894, -76.92610540732999880 ) ) ;
#51670 = CARTESIAN_POINT ( 'NONE',  ( 52.98105868624149650, 18.35548441844140299, -48.88375723731650169 ) ) ;
#51671 = CARTESIAN_POINT ( 'NONE',  ( 38.67452568954060155, -36.11618894467930119, -81.65000000000000568 ) ) ;
#51672 = CARTESIAN_POINT ( 'NONE',  ( 53.41693480158270546, -49.35328119387190071, -48.75416851881869462 ) ) ;
#51673 = ORIENTED_EDGE ( 'NONE', *, *, #13678, .T. ) ;
#51674 = CARTESIAN_POINT ( 'NONE',  ( 22.89142746321374844, -16.00358779221829408, -40.47104892312902535 ) ) ;
#51675 = CARTESIAN_POINT ( 'NONE',  ( 47.65034348264629926, -54.52133088470490208, -54.93304805868889673 ) ) ;
#51676 = DIRECTION ( 'NONE',  ( 0.000000000000000000, -1.000000000000000000, 0.000000000000000000 ) ) ;
#51677 = CARTESIAN_POINT ( 'NONE',  ( 22.90090927591486292, -15.61618926791037687, -70.45281771081829447 ) ) ;
#51678 = CARTESIAN_POINT ( 'NONE',  ( 64.37958960603660330, -32.00321536173649406, -17.48880570145399815 ) ) ;
#51679 = CARTESIAN_POINT ( 'NONE',  ( 71.26748243800840044, 1.369544300367000034, -60.93595317393490518 ) ) ;
#51680 = CARTESIAN_POINT ( 'NONE',  ( -10.98165337464593350, -35.31681881277557977, -44.31573110638452562 ) ) ;
#51681 = CARTESIAN_POINT ( 'NONE',  ( 72.68322664906099817, 1.025918948571989953, -61.73674522937599818 ) ) ;
#51682 = CIRCLE ( 'NONE', #1474, 1.000000000000000888 ) ;
#51683 = DIRECTION ( 'NONE',  ( 0.5813178231270340612, 0.8136765871738268485, 0.000000000000000000 ) ) ;
#51684 = SPHERICAL_SURFACE ( 'NONE', #44368, 3.000000000000159872 ) ;
#51685 = ORIENTED_EDGE ( 'NONE', *, *, #9685, .F. ) ;
#51686 = ORIENTED_EDGE ( 'NONE', *, *, #41882, .T. ) ;
#51687 = CARTESIAN_POINT ( 'NONE',  ( 56.95883372640280129, 19.02269652816849899, -52.69722348556799574 ) ) ;
#51688 = DIRECTION ( 'NONE',  ( 0.3294064756440925335, -0.9441882088883221114, -3.330669073875470607E-16 ) ) ;
#51689 = EDGE_LOOP ( 'NONE', ( #38989, #11874, #10485, #19623, #42410, #72, #44646 ) ) ;
#51690 = CARTESIAN_POINT ( 'NONE',  ( 12.17133826609699909, -65.27733561067250889, -46.10644761563530380 ) ) ;
#51691 = CARTESIAN_POINT ( 'NONE',  ( 16.85486949525910205, -23.50587475634130641, -77.97868939198153271 ) ) ;
#51692 = ORIENTED_EDGE ( 'NONE', *, *, #49976, .F. ) ;
#51693 = CARTESIAN_POINT ( 'NONE',  ( 11.39514780622933721, 34.02490255884188741, -22.76376844004561306 ) ) ;
#51694 = CARTESIAN_POINT ( 'NONE',  ( 44.48818529294619850, 6.748246523411627784, -67.87874373785433590 ) ) ;
#51695 = CARTESIAN_POINT ( 'NONE',  ( 9.807844417311496699, -10.75441821519198804, -34.71600119539038332 ) ) ;
#51696 = CARTESIAN_POINT ( 'NONE',  ( 8.964216265994560118, -11.54460215946079948, -44.95672957286240035 ) ) ;
#51697 = EDGE_CURVE ( 'NONE', #23772, #17962, #37713, .T. ) ;
#51698 = DIRECTION ( 'NONE',  ( 0.000000000000000000, 0.000000000000000000, -1.000000000000000000 ) ) ;
#51699 = CARTESIAN_POINT ( 'NONE',  ( 24.04492332548655753, -15.63231832970819823, -49.79297929963119174 ) ) ;
#51700 = EDGE_CURVE ( 'NONE', #885, #6210, #44410, .T. ) ;
#51701 = CARTESIAN_POINT ( 'NONE',  ( 62.83001711768829267, -30.40726919850919785, -16.32748532433430100 ) ) ;
#51702 = EDGE_CURVE ( 'NONE', #7519, #13595, #45710, .T. ) ;
#51703 = CARTESIAN_POINT ( 'NONE',  ( 85.66799001034409855, -48.61618894467930119, -61.58097075742929860 ) ) ;
#51704 = CARTESIAN_POINT ( 'NONE',  ( 12.08163306161019968, -8.895654951072430094, -77.33977848734279803 ) ) ;
#51705 = CARTESIAN_POINT ( 'NONE',  ( 11.97531774029090812, -21.02754808119717822, -37.16115274999724249 ) ) ;
#51706 = CARTESIAN_POINT ( 'NONE',  ( 43.16103038202970055, 14.52412741791340167, -7.511464010228710464 ) ) ;
#51707 = CARTESIAN_POINT ( 'NONE',  ( 14.91722740704980055, 21.75175735174070013, -76.14999999999999147 ) ) ;
#51708 = CARTESIAN_POINT ( 'NONE',  ( 83.51014914612841267, -44.78785608086950276, -46.95038033932869581 ) ) ;
#51709 = CIRCLE ( 'NONE', #34106, 36.55167969755429880 ) ;
#51710 = CARTESIAN_POINT ( 'NONE',  ( 24.04493740378650557, -14.58064945420081848, -57.75066457030849421 ) ) ;
#51711 = CARTESIAN_POINT ( 'NONE',  ( 20.85221322589909931, -8.854488424989650497, -47.20159690208759429 ) ) ;
#51712 = ORIENTED_EDGE ( 'NONE', *, *, #26644, .T. ) ;
#51713 = DIRECTION ( 'NONE',  ( 0.000000000000000000, 0.000000000000000000, 1.000000000000000000 ) ) ;
#51714 = CARTESIAN_POINT ( 'NONE',  ( 14.17150143963580078, -50.41474702392260099, -20.90975112687990034 ) ) ;
#51715 = CARTESIAN_POINT ( 'NONE',  ( 23.06315139208389908, -19.45320742824282689, -39.66865486300337551 ) ) ;
#51717 = EDGE_CURVE ( 'NONE', #29806, #25078, #33637, .T. ) ;
#51716 = CARTESIAN_POINT ( 'NONE',  ( 61.75019796695539753, -45.11618894467940066, -46.37203261889099792 ) ) ;
#51718 = CARTESIAN_POINT ( 'NONE',  ( 2.422196078461530178, -5.407548561780520124, -35.02873218748179340 ) ) ;
#51719 = VERTEX_POINT ( 'NONE', #30222 ) ;
#51720 = CARTESIAN_POINT ( 'NONE',  ( -5.738263256628330033, -47.06162393351850426, -5.576567369078139436 ) ) ;
#51721 = CARTESIAN_POINT ( 'NONE',  ( 47.21574955295219667, 23.54913593804809935, -54.62186942783370114 ) ) ;
#51722 = CARTESIAN_POINT ( 'NONE',  ( 22.72481340201672850, -17.38742253237608182, -48.53615538150855002 ) ) ;
#51723 = CARTESIAN_POINT ( 'NONE',  ( 63.11679429741250402, 0.8888742037077609348, -62.35931220671560027 ) ) ;
#51724 = CARTESIAN_POINT ( 'NONE',  ( 57.55751162062720283, -50.12763441343680171, -52.61703142046619774 ) ) ;
#51725 = CARTESIAN_POINT ( 'NONE',  ( 42.60880854190150302, 12.70305552983409925, -4.906336349105670180 ) ) ;
#51726 = DIRECTION ( 'NONE',  ( -0.5193766129849320956, 0.000000000000000000, 0.8545454545454562734 ) ) ;
#51727 = CARTESIAN_POINT ( 'NONE',  ( 64.64302830678670375, 0.9098571636355720083, -60.77008670988870165 ) ) ;
#51728 = DIRECTION ( 'NONE',  ( 0.000000000000000000, 8.635067969306036542E-13, 1.000000000000000000 ) ) ;
#51729 = CARTESIAN_POINT ( 'NONE',  ( 16.13393739769620083, -15.61618894467929941, -32.14999999999999858 ) ) ;
#51730 = CARTESIAN_POINT ( 'NONE',  ( 14.36265068495626451, -22.20705206307993862, -63.03615020535895042 ) ) ;
#51731 = CARTESIAN_POINT ( 'NONE',  ( 17.21347160910390173, -53.11618894467930119, -76.14999999999999147 ) ) ;
#51732 = CARTESIAN_POINT ( 'NONE',  ( 23.57797937038209923, -15.92103882122889935, -63.08037089589128499 ) ) ;
#51733 = CARTESIAN_POINT ( 'NONE',  ( 15.67961730780073282, 19.63028885021686776, -20.20261264479897179 ) ) ;
#51734 = CARTESIAN_POINT ( 'NONE',  ( 54.21268375596449829, -52.70726339247860182, -55.25757456134129342 ) ) ;
#51735 = ORIENTED_EDGE ( 'NONE', *, *, #2738, .F. ) ;
#51736 = CARTESIAN_POINT ( 'NONE',  ( 22.19769533645168025, -54.00735027852237380, -34.80997524099233686 ) ) ;
#51737 = CARTESIAN_POINT ( 'NONE',  ( 14.32416091673447944, -22.20785798411766976, -35.03836990857198685 ) ) ;
#51738 = CARTESIAN_POINT ( 'NONE',  ( 72.83393739769620367, 1.383811055320669947, -68.50657137141709541 ) ) ;
#51739 = CARTESIAN_POINT ( 'NONE',  ( 72.83393739769620367, 1.383811055320669947, -62.79342862858290886 ) ) ;
#51740 = B_SPLINE_CURVE_WITH_KNOTS ( 'NONE', 3,
 ( #23001, #51066, #31892, #3632, #27965, #47909, #6793, #15427, #27199, #43212, #35329, #22746, #31124, #38764, #27458, #7303, #23255, #2859 ),
 .UNSPECIFIED., .F., .F.,
 ( 4, 2, 2, 2, 2, 2, 2, 2, 4 ),
 ( 0.000000000000000000, 0.06250000041077040380, 0.1250000008215408076, 0.1875000012323111975, 0.2500000016430816152, 0.3125000020538520329, 0.3750000024646223951, 0.4375000028753928127, 0.5000000032861632304 ),
 .UNSPECIFIED. ) ;
#51741 = CARTESIAN_POINT ( 'NONE',  ( 10.03800373361939968, -11.28597919796850135, -81.23899999999999011 ) ) ;
#51742 = ORIENTED_EDGE ( 'NONE', *, *, #30582, .T. ) ;
#51743 = CARTESIAN_POINT ( 'NONE',  ( 17.82930383619740056, 21.38897561371040013, -76.01805773991210913 ) ) ;
#51744 = ORIENTED_EDGE ( 'NONE', *, *, #11470, .T. ) ;
#51745 = VERTEX_POINT ( 'NONE', #10065 ) ;
#51746 = CARTESIAN_POINT ( 'NONE',  ( 56.99379046497180212, -45.91441743241509243, -26.24653381559409837 ) ) ;
#51747 = CARTESIAN_POINT ( 'NONE',  ( 22.47177368144460274, -11.09078156707060003, -81.23899999999999011 ) ) ;
#51748 = LINE ( 'NONE', #35766, #48611 ) ;
#51749 = AXIS2_PLACEMENT_3D ( 'NONE', #40345, #15987, #3942 ) ;
#51750 = EDGE_LOOP ( 'NONE', ( #27907, #46104, #15117, #48868 ) ) ;
#51751 = DIRECTION ( 'NONE',  ( -1.000000000000000000, 0.000000000000000000, 0.000000000000000000 ) ) ;
#51752 = VERTEX_POINT ( 'NONE', #26290 ) ;
#51753 = CARTESIAN_POINT ( 'NONE',  ( -11.36606260230380094, -15.61618894467929941, -54.64999999999999858 ) ) ;
#51754 = EDGE_CURVE ( 'NONE', #2432, #35705, #6744, .T. ) ;
#51755 = CARTESIAN_POINT ( 'NONE',  ( 18.13393739769639978, 6.292713355527299157, -54.64999999999999858 ) ) ;
#51756 = ORIENTED_EDGE ( 'NONE', *, *, #2197, .F. ) ;
#51757 = ORIENTED_EDGE ( 'NONE', *, *, #32784, .F. ) ;
#51758 = EDGE_CURVE ( 'NONE', #24567, #36534, #50157, .T. ) ;
#51759 = DIRECTION ( 'NONE',  ( 0.000000000000000000, -1.000000000000000000, 0.000000000000000000 ) ) ;
#51760 = CARTESIAN_POINT ( 'NONE',  ( 29.99034385824719706, -15.61618894467929941, -24.15000000000000213 ) ) ;
#51761 = CARTESIAN_POINT ( 'NONE',  ( 60.73162164295760590, 14.50084501932449932, -47.73368171119290082 ) ) ;
#51762 = EDGE_CURVE ( 'NONE', #1516, #18021, #3379, .T. ) ;
#51763 = B_SPLINE_CURVE_WITH_KNOTS ( 'NONE', 3,
 ( #44330, #27566, #44078, #32249, #4243, #7673 ),
 .UNSPECIFIED., .F., .F.,
 ( 4, 2, 4 ),
 ( -0.2608998691367954148, -0.2578313219245090271, -0.2220763490922390004 ),
 .UNSPECIFIED. ) ;
#51764 = CYLINDRICAL_SURFACE ( 'NONE', #5494, 0.4999999999999985012 ) ;
#51765 = CARTESIAN_POINT ( 'NONE',  ( 41.27829218924360077, -44.10783499397969365, -3.596739496640999789 ) ) ;
#51766 = CARTESIAN_POINT ( 'NONE',  ( -10.88316963630090051, 11.11373587982220101, -6.260756294843470293 ) ) ;
#51767 = CYLINDRICAL_SURFACE ( 'NONE', #35488, 2.999999999999994227 ) ;
#51768 = CARTESIAN_POINT ( 'NONE',  ( 60.53218407266430034, 14.08784413439149930, -27.12214479265229983 ) ) ;
#51769 = CARTESIAN_POINT ( 'NONE',  ( 17.87834122126339764, -23.26758120253060369, -61.71615517726989708 ) ) ;
#51770 = ORIENTED_EDGE ( 'NONE', *, *, #34876, .F. ) ;
#51771 = DIRECTION ( 'NONE',  ( 0.000000000000000000, 0.000000000000000000, -1.000000000000000000 ) ) ;
#51772 = CARTESIAN_POINT ( 'NONE',  ( 41.83246392257819934, 14.51853978555750224, -6.687642457104619353 ) ) ;
#51773 = CARTESIAN_POINT ( 'NONE',  ( 11.79571167639570106, 33.77864909481949951, -45.51356534913389851 ) ) ;
#51775 = ADVANCED_FACE ( 'NONE', ( #26026 ), #47747, .T. ) ;
#51774 = CARTESIAN_POINT ( 'NONE',  ( 72.50969334808389988, 1.026088617261680103, -69.75574693290759853 ) ) ;
#51776 = CARTESIAN_POINT ( 'NONE',  ( 43.30576519922845335, -39.89449908986776450, -70.02050220811160841 ) ) ;
#51777 = AXIS2_PLACEMENT_3D ( 'NONE', #37066, #384, #12441 ) ;
#51778 = CARTESIAN_POINT ( 'NONE',  ( 16.13393739769620083, -15.61618894467929941, -40.14999999999999858 ) ) ;
#51779 = CARTESIAN_POINT ( 'NONE',  ( 22.57344131301335466, -18.29224899765534929, -44.97302808468992907 ) ) ;
#51780 = AXIS2_PLACEMENT_3D ( 'NONE', #42736, #27758, #27236 ) ;
#51781 = CARTESIAN_POINT ( 'NONE',  ( 61.05617857231141699, 14.11849002744650861, -46.88538215577281676 ) ) ;
#51782 = CARTESIAN_POINT ( 'NONE',  ( 48.59175220363999870, -54.13008784871289691, -55.28206484397910003 ) ) ;
#51783 = FACE_OUTER_BOUND ( 'NONE', #739, .T. ) ;
#51784 = CARTESIAN_POINT ( 'NONE',  ( 58.92073384691924076, -2.788940267406039730, -15.64999999999991687 ) ) ;
#51785 = CARTESIAN_POINT ( 'NONE',  ( 23.83903376137553565, -13.54549413143066516, -71.70899800185173945 ) ) ;
#51786 = VERTEX_POINT ( 'NONE', #9300 ) ;
#51787 = CARTESIAN_POINT ( 'NONE',  ( 13.73101345958830066, -8.564050908167290643, -36.46281005851519552 ) ) ;
#51788 = CARTESIAN_POINT ( 'NONE',  ( 21.54527357617396532, -19.77483941921981980, -76.66116015834198549 ) ) ;
#51789 = ORIENTED_EDGE ( 'NONE', *, *, #41621, .T. ) ;
#51790 = CARTESIAN_POINT ( 'NONE',  ( 71.35301946752790059, 1.370853092582090094, -70.32939881202800336 ) ) ;
#51791 = CARTESIAN_POINT ( 'NONE',  ( 60.74032281998740501, -45.58551599716069802, -47.45715664104950093 ) ) ;
#51792 = DIRECTION ( 'NONE',  ( 0.000000000000000000, 0.000000000000000000, 1.000000000000000000 ) ) ;
#51793 = DIRECTION ( 'NONE',  ( 1.000000000000000000, 0.000000000000000000, 0.000000000000000000 ) ) ;
#51795 = CARTESIAN_POINT ( 'NONE',  ( 44.81444952522934955, -33.19054756649958904, -41.91622283249964909 ) ) ;
#51794 = CARTESIAN_POINT ( 'NONE',  ( 41.50605423569203367, 8.477321776405595699, -78.71501693997980453 ) ) ;
#51796 = ADVANCED_FACE ( 'NONE', ( #9554 ), #39368, .F. ) ;
#51797 = DIRECTION ( 'NONE',  ( 1.000000000000000000, 0.000000000000000000, 0.000000000000000000 ) ) ;
#51798 = CARTESIAN_POINT ( 'NONE',  ( 8.428880937703265630, -13.54535095895175623, -66.59100159127797269 ) ) ;
#51799 = ORIENTED_EDGE ( 'NONE', *, *, #39411, .F. ) ;
#51800 = DIRECTION ( 'NONE',  ( 0.000000000000000000, -1.000000000000000000, 0.000000000000000000 ) ) ;
#51801 = ORIENTED_EDGE ( 'NONE', *, *, #18180, .F. ) ;
#51802 = ORIENTED_EDGE ( 'NONE', *, *, #46237, .T. ) ;
#51803 = CARTESIAN_POINT ( 'NONE',  ( 36.13393739769620083, -15.61618894467929941, -18.58999999999999986 ) ) ;
#51804 = CARTESIAN_POINT ( 'NONE',  ( 12.13393739769600010, -55.41568642894409180, -23.15000000000000213 ) ) ;
#51805 = CARTESIAN_POINT ( 'NONE',  ( 76.39120699412700333, -16.72954576041491492, -12.75862843308438244 ) ) ;
#51806 = CIRCLE ( 'NONE', #9126, 2.999999999999997780 ) ;
#51807 = ORIENTED_EDGE ( 'NONE', *, *, #47182, .F. ) ;
#51808 = VERTEX_POINT ( 'NONE', #25250 ) ;
#51809 = CARTESIAN_POINT ( 'NONE',  ( 47.90440150906960071, 23.11714053132569902, -54.72371951289599679 ) ) ;
#51810 = CARTESIAN_POINT ( 'NONE',  ( 57.30561799036939874, -45.12637755034730702, -25.31757343247140213 ) ) ;
#51811 = CARTESIAN_POINT ( 'NONE',  ( 56.46551886492290606, -50.77617157417189730, -53.85226995702900155 ) ) ;
#51812 = CARTESIAN_POINT ( 'NONE',  ( 21.07716222532573624, -10.95738292575066808, -46.21233756114791191 ) ) ;
#51813 = CARTESIAN_POINT ( 'NONE',  ( 62.22754354791340603, -0.4274600148359939955, -16.45757208976800001 ) ) ;
#51814 = CARTESIAN_POINT ( 'NONE',  ( 51.50850416226440132, -48.61618662830229454, -76.79363219169609067 ) ) ;
#51815 = EDGE_CURVE ( 'NONE', #12214, #17870, #22095, .T. ) ;
#51816 = AXIS2_PLACEMENT_3D ( 'NONE', #43324, #47264, #15018 ) ;
#51817 = ORIENTED_EDGE ( 'NONE', *, *, #24921, .T. ) ;
#51818 = CARTESIAN_POINT ( 'NONE',  ( 63.00666467042349694, 0.8838110553206759423, -68.76625967790960203 ) ) ;
#51819 = CARTESIAN_POINT ( 'NONE',  ( 52.26507113493899936, -49.78346811056199783, -77.19475928984779500 ) ) ;
#51820 = CARTESIAN_POINT ( 'NONE',  ( 22.69443958732917821, -13.86771010790146086, -34.36998131010714985 ) ) ;
#51821 = AXIS2_PLACEMENT_3D ( 'NONE', #5371, #10597, #17928 ) ;
#51822 = CARTESIAN_POINT ( 'NONE',  ( 12.14988939796288214, -22.52875931012240684, -54.17433617705772519 ) ) ;
#51823 = CIRCLE ( 'NONE', #13375, 18.50000000000000000 ) ;
#51824 = VECTOR ( 'NONE', #30659, 1000.000000000000114 ) ;
#51825 = ADVANCED_FACE ( 'NONE', ( #41253 ), #5364, .T. ) ;
#51826 = CARTESIAN_POINT ( 'NONE',  ( 14.87499325793340077, -23.36227229334909694, -50.56377978783950056 ) ) ;
#51827 = DIRECTION ( 'NONE',  ( 0.000000000000000000, 0.000000000000000000, 1.000000000000000000 ) ) ;
#51828 = CARTESIAN_POINT ( 'NONE',  ( 29.13393739769619728, -33.11618894467940066, -81.65000000000000568 ) ) ;
#51829 = AXIS2_PLACEMENT_3D ( 'NONE', #7657, #11330, #39618 ) ;
#51830 = LINE ( 'NONE', #35054, #45200 ) ;
#51831 = CARTESIAN_POINT ( 'NONE',  ( 57.39590324383170383, 13.88381105532070059, -17.43811253406409989 ) ) ;
#51832 = CARTESIAN_POINT ( 'NONE',  ( 8.731180243531472485, 17.69319178430564321, -34.79644561402098191 ) ) ;
#51833 =( BOUNDED_SURFACE ( )  B_SPLINE_SURFACE ( 2, 3, ( 
 ( #21734, #6545, #18846, #42458, #34306, #38521, #30886, #6033, #30632, #41933, #21991, #50319, #2620, #18592, #10486, #34568, #46914, #34828, #49800, #25919, #14405, #18074, #9956, #26441, #46135, #14663, #46657, #37741, #50053, #17817, #1839, #33791, #50830, #10740, #26696, #11000, #30116 ),
 ( #42718, #42977, #38001, #22767, #38786, #13891, #29850, #10226, #26184, #42195, #3138, #31145, #11519, #27220, #3653, #39803, #48180, #23022, #43232, #15959, #40060, #36120, #19624, #51857, #27480, #3910, #43738, #15184, #35348, #7839, #15446, #4153, #19874, #31399, #11780, #39550, #32164 ),
 ( #23272, #35615, #31911, #39043, #51086, #43482, #47426, #7586, #23532, #7325, #51602, #23788, #35865, #47677, #47933, #223, #20127, #35083, #11258, #15697, #39293, #47170, #27739, #31652, #12034, #27987, #7072, #3399, #19106, #19366, #51348, #16206, #43990, #8095, #12282, #24039, #28244 ) ),
 .UNSPECIFIED., .F., .F., .T. ) 
 B_SPLINE_SURFACE_WITH_KNOTS ( ( 3, 3 ),
 ( 4, 3, 3, 3, 3, 3, 3, 3, 3, 3, 3, 3, 4 ),
 ( -0.3886185405137270177, 0.4281390595564339985 ),
 ( -1.401241294368219981, -1.393251294075019908, -1.393221429621980034, -1.392992571260399881, -1.384912848423149878, -1.376592006214460095, -1.368290935607660019, -1.360011799518540121, -1.351756755142390132, -1.343527953381050022, -1.335327538272319980, -1.327157646422050030, -1.318834645256290017 ),
 .UNSPECIFIED. ) 
 GEOMETRIC_REPRESENTATION_ITEM ( )  RATIONAL_B_SPLINE_SURFACE ( (
 ( 1.001164415209670144, 1.001164415209680136, 1.001164415209680136, 1.001164415209680136, 1.001164415209680136, 1.001164415209680136, 1.001164415209680136, 1.001164415209680136, 1.001164415209680136, 1.001164415209680136, 1.001164415209680136, 1.001164415209680136, 1.001164415209680136, 1.001164415209680136, 1.001164415209680136, 1.001164415209680136, 1.001164415209680136, 1.001164415209680136, 1.001164415209680136, 1.001164415209680136, 1.001164415209680136, 1.001164415209680136, 1.001164415209680136, 1.001164415209680136, 1.001164415209680136, 1.001164415209680136, 1.001164415209680136, 1.001164415209680136, 1.001164415209680136, 1.001164415209680136, 1.001164415209680136, 1.001164415209680136, 1.001164415209680136, 1.001164415209680136, 1.001164415209680136, 1.001164415209680136, 1.001164415209680136),
 ( 0.9227754158175089927, 0.9227754158167740250, 0.9227754158169680920, 0.9227754158169680920, 0.9227754158169680920, 0.9227754158169539922, 0.9227754158169539922, 0.9227754158169539922, 0.9227754158169710896, 0.9227754158169710896, 0.9227754158169710896, 0.9227754158169660936, 0.9227754158169660936, 0.9227754158169660936, 0.9227754158169569898, 0.9227754158169569898, 0.9227754158169569898, 0.9227754158169509946, 0.9227754158169509946, 0.9227754158169509946, 0.9227754158169620968, 0.9227754158169620968, 0.9227754158169620968, 0.9227754158169710896, 0.9227754158169710896, 0.9227754158169710896, 0.9227754158169569898, 0.9227754158169569898, 0.9227754158169569898, 0.9227754158169600984, 0.9227754158169600984, 0.9227754158169600984, 0.9227754158169760856, 0.9227754158169760856, 0.9227754158169750864, 0.9227754158143870455, 0.9227754159543060108),
 ( 1.009136175741510044, 1.009136175741579988, 1.009136175741560004, 1.009136175741560004, 1.009136175741560004, 1.009136175741560004, 1.009136175741560004, 1.009136175741560004, 1.009136175741560004, 1.009136175741560004, 1.009136175741560004, 1.009136175741560004, 1.009136175741560004, 1.009136175741560004, 1.009136175741560004, 1.009136175741560004, 1.009136175741560004, 1.009136175741560004, 1.009136175741560004, 1.009136175741560004, 1.009136175741560004, 1.009136175741560004, 1.009136175741560004, 1.009136175741560004, 1.009136175741560004, 1.009136175741560004, 1.009136175741560004, 1.009136175741560004, 1.009136175741560004, 1.009136175741560004, 1.009136175741560004, 1.009136175741560004, 1.009136175741560004, 1.009136175741560004, 1.009136175741560004, 1.009136175741900177, 1.009136175723519990) ) ) 
 REPRESENTATION_ITEM ( '' )  SURFACE ( )  );
#51834 = DIRECTION ( 'NONE',  ( 1.000000000000000000, 0.000000000000000000, 0.000000000000000000 ) ) ;
#51835 = CARTESIAN_POINT ( 'NONE',  ( 21.17745084236759823, -10.68612491792770136, -48.60080040178890215 ) ) ;
#51836 = CARTESIAN_POINT ( 'NONE',  ( 46.75606609761160115, -39.76767805705360104, -54.48523547516549570 ) ) ;
#51837 = ORIENTED_EDGE ( 'NONE', *, *, #46100, .F. ) ;
#51838 = CARTESIAN_POINT ( 'NONE',  ( 11.49562787866076619, -65.37291902649519670, -18.17421237899758779 ) ) ;
#51839 = CARTESIAN_POINT ( 'NONE',  ( 47.23516258507500254, -54.76715534530099916, -54.66979262849320520 ) ) ;
#51840 = DIRECTION ( 'NONE',  ( 0.000000000000000000, 0.000000000000000000, 1.000000000000000000 ) ) ;
#51841 = CARTESIAN_POINT ( 'NONE',  ( 12.14981042511106146, -8.703663254087580015, -36.84100281579361535 ) ) ;
#51842 = CYLINDRICAL_SURFACE ( 'NONE', #51445, 7.910999999999997812 ) ;
#51843 = CARTESIAN_POINT ( 'NONE',  ( 8.919738259460670449, -49.28809633162239834, -34.65024031912469837 ) ) ;
#51844 = CARTESIAN_POINT ( 'NONE',  ( 0.05120484486776299277, 19.58911166448121932, -34.72736369164719861 ) ) ;
#51845 = CARTESIAN_POINT ( 'NONE',  ( 11.06596496317180112, 33.95392516474009881, -17.90443099699100316 ) ) ;
#51846 = CARTESIAN_POINT ( 'NONE',  ( 15.08314606030777760, -7.746415292052812873, -64.96536708472149257 ) ) ;
#51848 = CARTESIAN_POINT ( 'NONE',  ( 14.06334253594054573, -23.32131077769746597, -74.09100152957813634 ) ) ;
#51847 = CARTESIAN_POINT ( 'NONE',  ( 26.52624224310950041, -9.616188944679349149, -22.14999999999999858 ) ) ;
#51849 = CARTESIAN_POINT ( 'NONE',  ( 9.367163129351689932, -15.61602587752549809, -57.45282021618999835 ) ) ;
#51850 = CARTESIAN_POINT ( 'NONE',  ( 49.00738943425649552, 22.66954927679429943, -54.83009724927129724 ) ) ;
#51851 = CIRCLE ( 'NONE', #31740, 1.000000000000001554 ) ;
#51852 = ORIENTED_EDGE ( 'NONE', *, *, #46970, .T. ) ;
#51853 = AXIS2_PLACEMENT_3D ( 'NONE', #17600, #50352, #49586 ) ;
#51854 = CARTESIAN_POINT ( 'NONE',  ( 53.11419549839710186, -49.54851579802859618, -49.05615260309770065 ) ) ;
#51855 = VERTEX_POINT ( 'NONE', #33378 ) ;
#51856 = AXIS2_PLACEMENT_3D ( 'NONE', #22362, #3762, #15296 ) ;
#51857 = CARTESIAN_POINT ( 'NONE',  ( 43.98278727443419456, 7.770898977125641593, -70.80343447450441374 ) ) ;
#51858 = CARTESIAN_POINT ( 'NONE',  ( 15.24822463963293373, -22.38319927160165790, -74.99448688826869613 ) ) ;
#51859 = CARTESIAN_POINT ( 'NONE',  ( 14.12259462364040097, 19.90775691718999951, -22.75706045377140185 ) ) ;
#51860 = CARTESIAN_POINT ( 'NONE',  ( 82.81259997840240317, 13.80159592993990003, -46.56543266184489482 ) ) ;
#51861 = EDGE_CURVE ( 'NONE', #27489, #42283, #21577, .T. ) ;
#51862 = CARTESIAN_POINT ( 'NONE',  ( 9.105706864571400772, -15.02751733004349965, -51.47941917952310575 ) ) ;
#51863 = CARTESIAN_POINT ( 'NONE',  ( 52.95214313111540605, 18.40625499070019799, -49.03964310582890107 ) ) ;
#51864 = CARTESIAN_POINT ( 'NONE',  ( 55.00335051654970187, -45.49428894239379417, -15.38805630266439906 ) ) ;
#51865 = CARTESIAN_POINT ( 'NONE',  ( 54.85035616863599728, 16.02459751768909868, -25.69268928997570001 ) ) ;
#51866 = B_SPLINE_CURVE_WITH_KNOTS ( 'NONE', 3,
 ( #8310, #44732, #47639, #35835, #4121, #28212, #195, #443, #16433, #48407, #48149 ),
 .UNSPECIFIED., .F., .F.,
 ( 4, 1, 1, 1, 1, 1, 1, 1, 4 ),
 ( 0.000000000000000000, 0.1250000000000000000, 0.2500000000000000000, 0.3750000000000000000, 0.5000000000000000000, 0.6250000000000000000, 0.7500000000000000000, 0.8750000000000000000, 1.000000000000000000 ),
 .UNSPECIFIED. ) ;
#51867 = EDGE_CURVE ( 'NONE', #14876, #630, #5444, .T. ) ;
#51868 = ORIENTED_EDGE ( 'NONE', *, *, #51411, .T. ) ;
#51869 = CARTESIAN_POINT ( 'NONE',  ( 14.06638412633730084, -23.18665601437029977, -45.87236896454599844 ) ) ;
#51870 = EDGE_LOOP ( 'NONE', ( #9165, #28517, #30777, #39067, #20109 ) ) ;
#51871 = EDGE_CURVE ( 'NONE', #425, #19145, #43585, .T. ) ;
#51872 = ORIENTED_EDGE ( 'NONE', *, *, #28733, .F. ) ;
#51873 = NEXT_ASSEMBLY_USAGE_OCCURRENCE ( 'NAUO1', ' ', ' ', #21256, #46257, $ ) ;
#51874 = NEXT_ASSEMBLY_USAGE_OCCURRENCE ( 'NAUO2', ' ', ' ', #21256, #48485, $ ) ;
#51875 = NEXT_ASSEMBLY_USAGE_OCCURRENCE ( 'NAUO3', ' ', ' ', #21256, #15826, $ ) ;
#51876 = NEXT_ASSEMBLY_USAGE_OCCURRENCE ( 'NAUO4', ' ', ' ', #21256, #45296, $ ) ;
#51877 = NEXT_ASSEMBLY_USAGE_OCCURRENCE ( 'NAUO5', ' ', ' ', #21256, #31487, $ ) ;
#51878 = NEXT_ASSEMBLY_USAGE_OCCURRENCE ( 'NAUO6', ' ', ' ', #21256, #38253, $ ) ;
ENDSEC;
END-ISO-10303-21;
